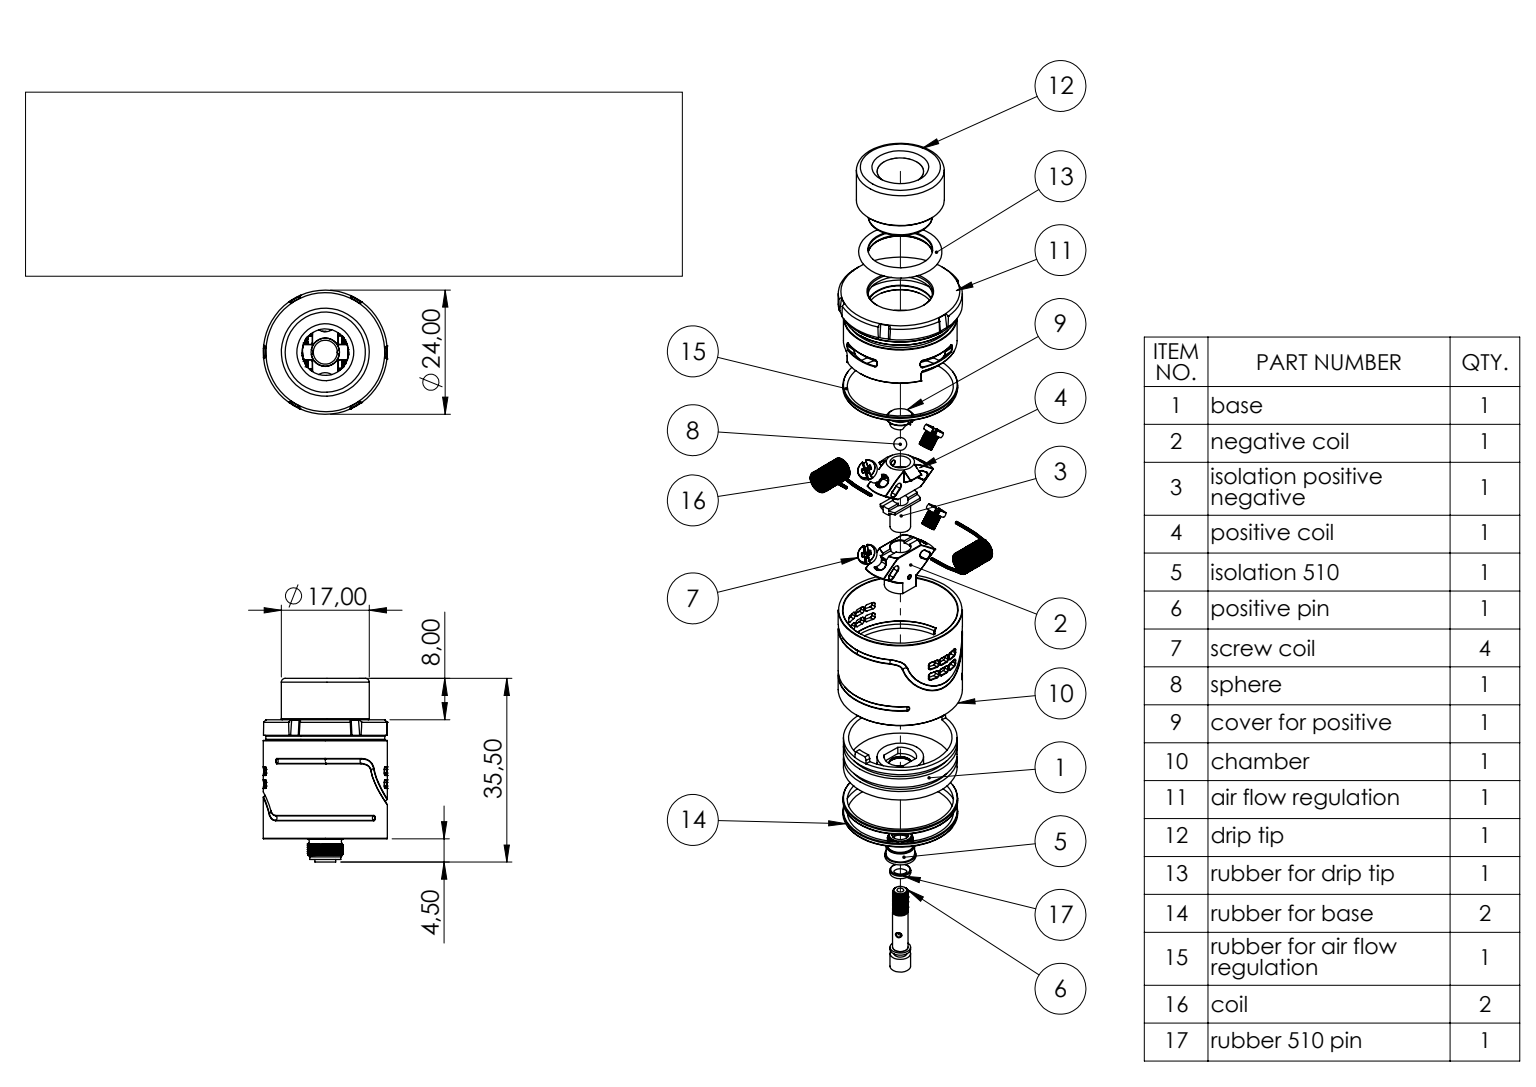
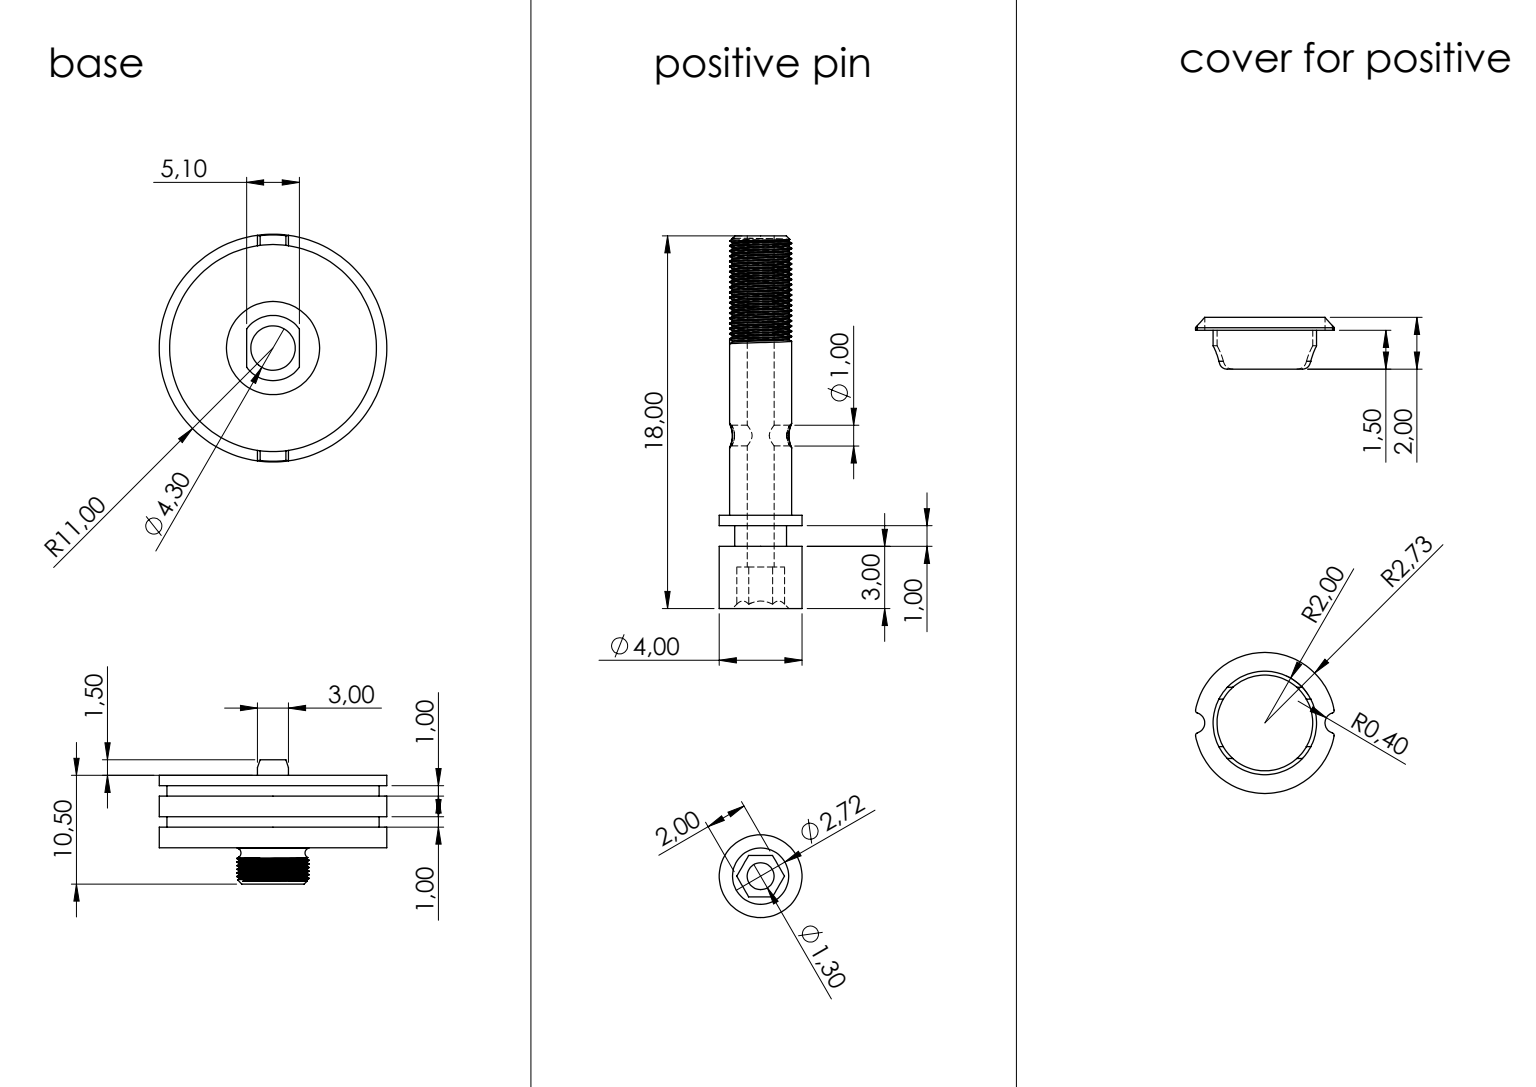
ISO-10303-21;
HEADER;
FILE_DESCRIPTION (('STEP AP214'),
    '1' );
FILE_NAME ('MAS-692',
    '2026-10-05T20:10:51',
    ( '' ),
    ( '' ),
    'SwSTEP 2.0',
    'SolidWorks 2020',
    '' );
FILE_SCHEMA (( 'AUTOMOTIVE_DESIGN' ));
ENDSEC;

DATA;
#1 = ORIENTED_EDGE ( 'NONE', *, *, #97562, .T. ) ;
#2 =( NAMED_UNIT ( * ) PLANE_ANGLE_UNIT ( ) SI_UNIT ( $, .RADIAN. ) );
#3 = ORIENTED_EDGE ( 'NONE', *, *, #96141, .T. ) ;
#4 = CARTESIAN_POINT ( 'NONE',  ( 5.963713532047742127, -0.4821895448718095945, 1.909345749545824367 ) ) ;
#5 = CARTESIAN_POINT ( 'NONE',  ( 1.311946287462633309, 1.302956792059128066, -1.440285294924074311 ) ) ;
#6 = CARTESIAN_POINT ( 'NONE',  ( 0.2454708137151571101, -1.954895187565863779, -0.4925657318226167591 ) ) ;
#8 = CARTESIAN_POINT ( 'NONE',  ( 4.311269015108330827, -1.545260327404588852, -1.036625270625696205 ) ) ;
#7 = CARTESIAN_POINT ( 'NONE',  ( -7.144220599758281054, 7.299621885998258897, 0.7998128361456341429 ) ) ;
#9 = CARTESIAN_POINT ( 'NONE',  ( 6.873057527484919937, 6.983264968346048818, 0.7998128361456352531 ) ) ;
#11 = ADVANCED_FACE ( 'NONE', ( #143939 ), #115364, .T. ) ;
#10 = CARTESIAN_POINT ( 'NONE',  ( 8.996750068618124985, 1.000000000000000888, 7.838941051145326355 ) ) ;
#12 = CYLINDRICAL_SURFACE ( 'NONE', #60912, 0.5000000000000000000 ) ;
#13 = CARTESIAN_POINT ( 'NONE',  ( -4.869349725602420520, 8.832658446511480577, 1.040834085586084257E-14 ) ) ;
#14 = CARTESIAN_POINT ( 'NONE',  ( -4.828112100242303306, 4.805421336470338645, -0.7216878364870338292 ) ) ;
#15 = CARTESIAN_POINT ( 'NONE',  ( 0.04676574305502099321, -1.756316032869180921, 1.310637071781264984 ) ) ;
#16 = CARTESIAN_POINT ( 'NONE',  ( 5.233084105194869551, 6.167981546557892436, -1.082531754730548412 ) ) ;
#17 = CARTESIAN_POINT ( 'NONE',  ( 11.89942855770814312, 9.799999999999998934, 0.6999999999999992895 ) ) ;
#18 = CARTESIAN_POINT ( 'NONE',  ( 1.833030277982334422, 2.531131934864056632, -2.500000000000000444 ) ) ;
#19 = CARTESIAN_POINT ( 'NONE',  ( 1.260069262837599791, 0.7379878962356714034, 1.670071910705408946 ) ) ;
#20 = CARTESIAN_POINT ( 'NONE',  ( -4.460796234096120472, 5.163016013655583158, 1.199719254218462483 ) ) ;
#21 = MECHANICAL_DESIGN_GEOMETRIC_PRESENTATION_REPRESENTATION (  '', ( #3437 ), #103815 ) ;
#22 = CARTESIAN_POINT ( 'NONE',  ( 3.515997504735939305, -1.600726479906929844, 0.6675610986628178756 ) ) ;
#23 = CARTESIAN_POINT ( 'NONE',  ( -0.4770184558378520734, 2.994739774722604331, -1.942553401570029203 ) ) ;
#24 = CARTESIAN_POINT ( 'NONE',  ( 6.609000000000019526, 4.695354556932705314, 2.562644781943986150 ) ) ;
#25 = CARTESIAN_POINT ( 'NONE',  ( 0.1331565106231329398, 0.7299000548664087429, -2.029785554894456556 ) ) ;
#26 = CARTESIAN_POINT ( 'NONE',  ( 6.445924739416000193, 0.6936395621829589686, -1.688995215704327313 ) ) ;
#27 = CARTESIAN_POINT ( 'NONE',  ( 4.504711789546460565, 0.5192035298374733099, 1.891763301562799260 ) ) ;
#28 = CARTESIAN_POINT ( 'NONE',  ( -8.474009703741204547, 9.845098394908269768, -1.199719254218446718 ) ) ;
#29 = CARTESIAN_POINT ( 'NONE',  ( 5.666418135507635512, 8.698239360479199433, 1.199719254218462483 ) ) ;
#30 = CARTESIAN_POINT ( 'NONE',  ( 4.389387035479824561, -0.001039498178659337352, -2.120667954306009406 ) ) ;
#31 = CARTESIAN_POINT ( 'NONE',  ( -9.158696461231359720, 10.64389961198009615, 1.199719254218462483 ) ) ;
#32 = ADVANCED_FACE ( 'NONE', ( #8553 ), #60499, .T. ) ;
#33 = CARTESIAN_POINT ( 'NONE',  ( 5.118366684358879759, 5.930181538962194132, 1.199719254218462483 ) ) ;
#34 = CARTESIAN_POINT ( 'NONE',  ( 3.274343992483694787, -1.016290647400164282, -1.803532422793553636 ) ) ;
#36 = CARTESIAN_POINT ( 'NONE',  ( 0.6823417656249882723, -0.5947916663252492686, 1.181850606188755259 ) ) ;
#35 = CARTESIAN_POINT ( 'NONE',  ( -0.4382560683119374190, -5.166862915010145052, -10.99126615174919408 ) ) ;
#37 = EDGE_LOOP ( 'NONE', ( #180346, #201044, #89611 ) ) ;
#38 = CARTESIAN_POINT ( 'NONE',  ( 2.549810578889585067, -1.582449011024213981, 1.667500336659861748 ) ) ;
#39 = CARTESIAN_POINT ( 'NONE',  ( 6.954969614130424027, 11.05795561655343384, 1.040834085586084257E-14 ) ) ;
#41 = CARTESIAN_POINT ( 'NONE',  ( 1.642778471875001811, -1.742708332855374298, 2.845375778867859751 ) ) ;
#40 = CARTESIAN_POINT ( 'NONE',  ( 4.719646871332936477, 8.520355426614829142, -0.7216878364870357165 ) ) ;
#42 = PRESENTATION_STYLE_ASSIGNMENT (( #185202 ) ) ;
#43 = CARTESIAN_POINT ( 'NONE',  ( 0.000000000000000000, 4.000000000000003553, 0.000000000000000000 ) ) ;
#44 = VERTEX_POINT ( 'NONE', #43221 ) ;
#45 = CARTESIAN_POINT ( 'NONE',  ( 10.37162432432990755, 11.20257592124748136, -0.7216878364870257245 ) ) ;
#46 = CARTESIAN_POINT ( 'NONE',  ( 3.568532368641282648, 0.6928216322696268969, 1.782650395559831180 ) ) ;
#47 = CARTESIAN_POINT ( 'NONE',  ( 4.928557879857294211, 1.651178231652555617, 0.4983569138605167814 ) ) ;
#48 = CARTESIAN_POINT ( 'NONE',  ( 3.608611488583326032, 1.916353073142588403, 0.6279913346786819561 ) ) ;
#49 =( BOUNDED_SURFACE ( )  B_SPLINE_SURFACE ( 3, 2, ( 
 ( #54801, #106802, #172831 ),
 ( #26553, #190122, #173916 ),
 ( #25490, #91596, #38551 ),
 ( #157648, #9245, #191177 ),
 ( #108952, #72088, #42845 ),
 ( #4939, #71015, #22263 ) ),
 .UNSPECIFIED., .F., .F., .T. ) 
 B_SPLINE_SURFACE_WITH_KNOTS ( ( 4, 2, 4 ),
 ( 3, 3 ),
 ( 0.0001465838689801548850, 0.0002810652682710442613, 0.0004155466675619336647 ),
 ( 0.000000000000000000, 1.000000000000000000 ),
 .UNSPECIFIED. ) 
 GEOMETRIC_REPRESENTATION_ITEM ( )  RATIONAL_B_SPLINE_SURFACE ( (
 ( 1.000000000000000000, 0.8789000212895399233, 1.000000000000000000),
 ( 1.000000000000000000, 0.9073166784884888481, 1.000000000000000000),
 ( 1.000000000000000000, 0.9160359019619195298, 1.000000000000000000),
 ( 1.000000000000000000, 0.8858134948703222378, 1.000000000000000000),
 ( 1.000000000000000000, 0.8506312074210943264, 1.000000000000000000),
 ( 1.000000000000000000, 0.8104931255412257673, 1.000000000000000000) ) ) 
 REPRESENTATION_ITEM ( '' )  SURFACE ( )  );
#50 = CARTESIAN_POINT ( 'NONE',  ( 5.063244923127927954, -1.278613472530117035, 1.910113253385301801 ) ) ;
#51 = CARTESIAN_POINT ( 'NONE',  ( -1.626862140677534470E-15, 1.125000000682806034, 1.224999999999975886 ) ) ;
#52 = CARTESIAN_POINT ( 'NONE',  ( 0.8388348947251201837, 2.174866457552121268, 0.3736606161612308630 ) ) ;
#53 = CARTESIAN_POINT ( 'NONE',  ( -3.797692425603673705, 6.484372692295976570, 1.082531754730549967 ) ) ;
#54 = CARTESIAN_POINT ( 'NONE',  ( 6.362547694819080668, -1.249765848162401438, 1.253281529121505589 ) ) ;
#56 = CARTESIAN_POINT ( 'NONE',  ( 1.851946410329910808, 2.285883199777267283, -0.1717553002464344836 ) ) ;
#55 = CARTESIAN_POINT ( 'NONE',  ( 6.710359684120930091, 6.793450817754725257, 0.7998128361456352531 ) ) ;
#57 = CARTESIAN_POINT ( 'NONE',  ( 6.228435704027582176, 0.1854037366294820077, 1.831779187086844729 ) ) ;
#58 = PRESENTATION_STYLE_ASSIGNMENT (( #85603 ) ) ;
#59 = CARTESIAN_POINT ( 'NONE',  ( -4.167152111353897403, 5.955039778036558040, 1.599625672291270506 ) ) ;
#60 = CARTESIAN_POINT ( 'NONE',  ( 1.360316468749959373, -0.4531249996586189654, -4.163336342344337027E-14 ) ) ;
#61 = FACE_OUTER_BOUND ( 'NONE', #36024, .T. ) ;
#62 = CARTESIAN_POINT ( 'NONE',  ( 0.3269468692386565678, -1.417551234153333395, 1.644607001386617418 ) ) ;
#63 = CARTESIAN_POINT ( 'NONE',  ( 1.973842561262352469, -0.8578407463649927456, 1.825077436249371354 ) ) ;
#64 = CARTESIAN_POINT ( 'NONE',  ( 1.499999999999989120, 0.05625000068281565957, 0.000000000000000000 ) ) ;
#65 = CARTESIAN_POINT ( 'NONE',  ( 5.479104952107777926, -0.04952074540257554031, -1.926025958231538882 ) ) ;
#66 = CARTESIAN_POINT ( 'NONE',  ( -8.012344526598182026E-15, 11.29687500034139980, -1.575800808251669460 ) ) ;
#67 = CARTESIAN_POINT ( 'NONE',  ( 1.898975720090949837, -2.179683001098455808, -0.4277757613022105110 ) ) ;
#68 = EDGE_LOOP ( 'NONE', ( #150530, #161755, #187821, #170704 ) ) ;
#69 = CARTESIAN_POINT ( 'NONE',  ( 6.731761806397376091, -7.792646766724933727, 6.779954559072931985 ) ) ;
#70 = LINE ( 'NONE', #134411, #196122 ) ;
#71 = CARTESIAN_POINT ( 'NONE',  ( 8.540746701604824409, 12.05162268759261224, -1.199719254218446718 ) ) ;
#72 = CARTESIAN_POINT ( 'NONE',  ( 6.658462837642789012, 9.821938173008357253, 1.082531754730549078 ) ) ;
#73 = CARTESIAN_POINT ( 'NONE',  ( 5.706559709869656771, 1.539012945689299139, 0.8127616963746787659 ) ) ;
#74 = CARTESIAN_POINT ( 'NONE',  ( 3.596105239937871456, 0.8843387906064968940, -1.751336483779348585 ) ) ;
#76 = CARTESIAN_POINT ( 'NONE',  ( -6.887178846062123938, 8.097758744236356776, -1.082531754730544860 ) ) ;
#75 = CARTESIAN_POINT ( 'NONE',  ( 4.253507506385319381, 5.985511395581417204, 1.599625672291267398 ) ) ;
#77 = CARTESIAN_POINT ( 'NONE',  ( -5.762141863986474100, 6.090740110424618159, 0.6348889758391648153 ) ) ;
#78 = CARTESIAN_POINT ( 'NONE',  ( 4.763087504681410955, -2.017952330160921015, -1.023110994099560411 ) ) ;
#79 = CARTESIAN_POINT ( 'NONE',  ( 1.135301032730736237, -0.04873925880971052838, -2.062252310772247910 ) ) ;
#80 = CARTESIAN_POINT ( 'NONE',  ( -8.830438121202295321, 9.196599317691152464, -0.7998128361456291469 ) ) ;
#81 = CARTESIAN_POINT ( 'NONE',  ( -4.460269348771590536, 5.266364330730674226, 1.082531754730558626 ) ) ;
#82 = CARTESIAN_POINT ( 'NONE',  ( 2.782378429719241986, -1.163933448739282062, 1.940043740367594305 ) ) ;
#83 = ORIENTED_EDGE ( 'NONE', *, *, #112082, .F. ) ;
#84 = CARTESIAN_POINT ( 'NONE',  ( -0.7500000000000006661, -0.6104166659838470288, -1.299038105676652011 ) ) ;
#85 = CARTESIAN_POINT ( 'NONE',  ( 2.301827437220682171, -1.870247568056710774, 0.04138213060620592881 ) ) ;
#86 = CARTESIAN_POINT ( 'NONE',  ( 1.441630353877725979, -1.487241779905050576, -0.8915045353455192112 ) ) ;
#87 = CARTESIAN_POINT ( 'NONE',  ( 5.495707582769355781, -2.191739722525353429, -0.0009102486706394352645 ) ) ;
#88 = CARTESIAN_POINT ( 'NONE',  ( 0.2533207856364183552, -1.770817270756098960, 1.316655756711228253 ) ) ;
#89 = CARTESIAN_POINT ( 'NONE',  ( 1.534131747024346737, 1.016495879925772616, -1.792692027746685346 ) ) ;
#90 = CARTESIAN_POINT ( 'NONE',  ( 4.013568362537369261, -0.9994162096361800529, -1.664904219174968114 ) ) ;
#91 = CARTESIAN_POINT ( 'NONE',  ( -3.592547517496929466, 7.135129837147637488, -0.7216878364870257245 ) ) ;
#92 = CARTESIAN_POINT ( 'NONE',  ( 6.928203230275524760, 15.51845925587262798, -9.797958971132702644 ) ) ;
#93 = CARTESIAN_POINT ( 'NONE',  ( 1.718750000000001554, -0.7852924748298989455, 1.895863743164124093 ) ) ;
#94 = CARTESIAN_POINT ( 'NONE',  ( 4.014365637759117256, 7.575528411784208771, 0.2883143100938356240 ) ) ;
#95 = CARTESIAN_POINT ( 'NONE',  ( 0.2800716429562755683, -1.702078881456047688, 0.3292984779095942116 ) ) ;
#96 = CARTESIAN_POINT ( 'NONE',  ( 11.88237951145550220, 12.34319347378715115, 0.9087114598430685586 ) ) ;
#97 = CARTESIAN_POINT ( 'NONE',  ( 0.6801582343749935644, 0.9739583336747514863, 1.178068619123805227 ) ) ;
#98 = CARTESIAN_POINT ( 'NONE',  ( 4.483046177357690176, -2.016033783801042034, -0.04667830911464498911 ) ) ;
#99 = CARTESIAN_POINT ( 'NONE',  ( -8.859363311525973117, 12.42334206583395328, -1.199719254218446718 ) ) ;
#100 = CARTESIAN_POINT ( 'NONE',  ( 8.308449207076147758, 8.587612251210650527, -0.7998128361456281477 ) ) ;
#101 = CARTESIAN_POINT ( 'NONE',  ( 4.553559489343365740, 6.405848385690952718, -1.599625672291269396 ) ) ;
#103 = CARTESIAN_POINT ( 'NONE',  ( 1.255262969126037044E-15, 0.4999999999999998890, -10.24999999999999822 ) ) ;
#102 = CARTESIAN_POINT ( 'NONE',  ( 2.068725586703868746, -1.668841220716179130, -0.7407507213199536755 ) ) ;
#104 = CARTESIAN_POINT ( 'NONE',  ( -0.7500000000000215383, 5.191666666666685082, 1.299038105676671107 ) ) ;
#105 = CARTESIAN_POINT ( 'NONE',  ( -9.333041836226904309, 15.44694763438996077, -7.472413793095822321 ) ) ;
#106 = VERTEX_POINT ( 'NONE', #173218 ) ;
#107 = CARTESIAN_POINT ( 'NONE',  ( -5.600926855776882540, 8.588146194164741232, -1.082531754730549967 ) ) ;
#108 = DIRECTION ( 'NONE',  ( 0.000000000000000000, 0.000000000000000000, -1.000000000000000000 ) ) ;
#109 = CARTESIAN_POINT ( 'NONE',  ( -8.565000355531095622, 11.01558638625153286, -1.599625672291263179 ) ) ;
#110 = CARTESIAN_POINT ( 'NONE',  ( 0.01783989211246589379, -0.5346760324982450241, 1.947684760809722304 ) ) ;
#111 = CARTESIAN_POINT ( 'NONE',  ( 6.551452540055466400, -1.985718062329771438, 0.9957849561875466993 ) ) ;
#112 = ORIENTED_EDGE ( 'NONE', *, *, #89227, .T. ) ;
#113 = CARTESIAN_POINT ( 'NONE',  ( -4.911796789900812144, 8.952456364851418158, 0.7998128361456291469 ) ) ;
#114 = CARTESIAN_POINT ( 'NONE',  ( 5.843727902690005749, 6.776436293681846301, -1.199719254218445830 ) ) ;
#115 = MECHANICAL_DESIGN_GEOMETRIC_PRESENTATION_REPRESENTATION (  '', ( #107520 ), #142122 ) ;
#116 = CARTESIAN_POINT ( 'NONE',  ( 6.666874348205719336, -1.883165374045802087, -0.8376701409097894180 ) ) ;
#117 = CARTESIAN_POINT ( 'NONE',  ( 4.869767617671093340, -0.2496050341583149201, -2.000857388266870984 ) ) ;
#118 = ORIENTED_EDGE ( 'NONE', *, *, #154536, .F. ) ;
#119 = ORIENTED_EDGE ( 'NONE', *, *, #79643, .F. ) ;
#120 = CARTESIAN_POINT ( 'NONE',  ( 10.50000000000000355, 11.00832445802304882, -3.600000000000000533 ) ) ;
#121 = CARTESIAN_POINT ( 'NONE',  ( -2.324088772396477673E-16, -1.093749999044084653, -3.475000000000000089 ) ) ;
#124 = VERTEX_POINT ( 'NONE', #206751 ) ;
#123 = CARTESIAN_POINT ( 'NONE',  ( -1.772826578343124959, 3.950000000000009059, -0.4500000000000423661 ) ) ;
#122 = CARTESIAN_POINT ( 'NONE',  ( -5.956828388357799042, 8.042995434541133193, 1.599625672291263179 ) ) ;
#125 = CARTESIAN_POINT ( 'NONE',  ( 5.720439131930858956, 7.397432110343761025, 1.315134405782365956 ) ) ;
#126 = CARTESIAN_POINT ( 'NONE',  ( 4.639999869408336863, 0.002810260262744306969, -2.016288307263448321 ) ) ;
#127 = CARTESIAN_POINT ( 'NONE',  ( 4.294743845541324490, 1.480121740587354573, 1.094796260939827404 ) ) ;
#128 = CARTESIAN_POINT ( 'NONE',  ( 2.969872605471105320, 6.605953636083950364, 7.500000000000000000 ) ) ;
#129 = CARTESIAN_POINT ( 'NONE',  ( 3.317284684000018746, 2.086097511483188338, 0.9870085806921449212 ) ) ;
#130 = CARTESIAN_POINT ( 'NONE',  ( 5.833751235630055376, 10.02806988486892514, 0.7998128361456331437 ) ) ;
#131 = CARTESIAN_POINT ( 'NONE',  ( 4.727887898869392203, -1.325758432718616042, -1.707240035374466114 ) ) ;
#132 = CARTESIAN_POINT ( 'NONE',  ( 6.286176778230493589, 10.48562334124426698, 0.7998128361456462443 ) ) ;
#133 = CARTESIAN_POINT ( 'NONE',  ( 1.030689935155226555, -1.755017395645932066, 0.8318847510124205424 ) ) ;
#134 = CARTESIAN_POINT ( 'NONE',  ( -5.434120640978981065, 5.234228924097238611, -0.7998128361456221525 ) ) ;
#135 = ORIENTED_EDGE ( 'NONE', *, *, #160637, .F. ) ;
#137 = ADVANCED_FACE ( 'NONE', ( #75695 ), #126301, .T. ) ;
#136 = AXIS2_PLACEMENT_3D ( 'NONE', #150027, #130648, #82874 ) ;
#138 = CARTESIAN_POINT ( 'NONE',  ( 6.446420058208158110, -6.527411821100059797, 7.058808231563617142 ) ) ;
#139 = CARTESIAN_POINT ( 'NONE',  ( -4.817943484809863008, 6.714296380401858499, 1.599625672291263179 ) ) ;
#140 = CARTESIAN_POINT ( 'NONE',  ( 3.783945140921864070, -0.9226758061156097313, 1.627204332209288395 ) ) ;
#143 = CARTESIAN_POINT ( 'NONE',  ( -5.586841817283045408, 8.675676665875643678, 1.199719254218454489 ) ) ;
#142 = CARTESIAN_POINT ( 'NONE',  ( -1.500000000000015099, -0.5479166659838513587, 0.8660254037844403729 ) ) ;
#141 = CARTESIAN_POINT ( 'NONE',  ( 1.828231037913151447, -0.9045423626323212396, -1.684975973026317408 ) ) ;
#144 = CARTESIAN_POINT ( 'NONE',  ( 3.018423772948013006, -1.088090592406821155, -1.919924466345590108 ) ) ;
#145 = CARTESIAN_POINT ( 'NONE',  ( 6.883263157960402445, 0.001763689368145578400, 1.846037217754380011 ) ) ;
#146 = CARTESIAN_POINT ( 'NONE',  ( 4.403700966340357681, 4.032072637018845107, -0.7998128361456211532 ) ) ;
#147 = CARTESIAN_POINT ( 'NONE',  ( 7.038091138825468107, 8.344099429118761790, -1.082531754730548412 ) ) ;
#148 = CARTESIAN_POINT ( 'NONE',  ( -3.216308754939891212, 4.775446185561722956, -1.599625672291262513 ) ) ;
#149 = CARTESIAN_POINT ( 'NONE',  ( -7.390603132780803719, 7.794994207765291172, -0.7216878364870338292 ) ) ;
#150 = CARTESIAN_POINT ( 'NONE',  ( 0.9484320465981105341, 0.5679970104440315026, 1.887783002132171539 ) ) ;
#151 = CARTESIAN_POINT ( 'NONE',  ( 0.3414292828918061296, 0.3991051782518301727, 2.272663865251875581 ) ) ;
#152 = CARTESIAN_POINT ( 'NONE',  ( 1.838261372102001800, -1.052240823716396267, 1.655630454418555830 ) ) ;
#153 = CARTESIAN_POINT ( 'NONE',  ( 5.032111728107424575, 1.183179145130999643, 1.689302184701612086 ) ) ;
#154 = CARTESIAN_POINT ( 'NONE',  ( 5.178851490740207453, 5.144340948726102702, 0.7216878364870317197 ) ) ;
#155 = CARTESIAN_POINT ( 'NONE',  ( 4.667750024854814050, 8.667735138964429709, -0.7998128361456381397 ) ) ;
#156 = VERTEX_POINT ( 'NONE', #175348 ) ;
#157 = CARTESIAN_POINT ( 'NONE',  ( -1.364683531250010295, 5.301041667008085767, -0.7879004041258300672 ) ) ;
#158 = CARTESIAN_POINT ( 'NONE',  ( -10.12724623727299900, 3.700526055228949840, -6.355430437403613020 ) ) ;
#159 = CARTESIAN_POINT ( 'NONE',  ( 4.541618270453549044, 5.361271406026338227, -1.082531754730548412 ) ) ;
#160 = CARTESIAN_POINT ( 'NONE',  ( 1.042111193480334430, 1.456518763772189695, 1.610191069602670000 ) ) ;
#162 = CARTESIAN_POINT ( 'NONE',  ( 6.251489360189885325, 1.835807759842246423, -0.1425652098738516838 ) ) ;
#161 = CARTESIAN_POINT ( 'NONE',  ( 1.224999999999948797, 0.4583333340161501734, -0.7072540797573277915 ) ) ;
#163 = CARTESIAN_POINT ( 'NONE',  ( 11.84668730067608244, 12.69999999999998153, 1.399999999999998357 ) ) ;
#164 = CARTESIAN_POINT ( 'NONE',  ( -11.92051736251532112, 12.44819756207321149, -1.381800029228967386 ) ) ;
#165 = CARTESIAN_POINT ( 'NONE',  ( 1.915107840602244593, -0.2339084544023955492, 1.855816807740391150 ) ) ;
#166 = CARTESIAN_POINT ( 'NONE',  ( 5.343121995983710626, -1.856993961526328007, 1.106124453333141577 ) ) ;
#167 = CARTESIAN_POINT ( 'NONE',  ( -6.137267537028628261, 5.996416355291856348, 0.05987573180751305790 ) ) ;
#168 = CARTESIAN_POINT ( 'NONE',  ( -0.02244404828160087226, 0.2256878572204877031, -2.222431841814066278 ) ) ;
#169 = CARTESIAN_POINT ( 'NONE',  ( 6.425920342564602983, 6.885296541689900351, -0.7293792964763821107 ) ) ;
#170 = CARTESIAN_POINT ( 'NONE',  ( 0.6823417656249899377, 5.738541667008087543, -1.181850606188754593 ) ) ;
#171 = CARTESIAN_POINT ( 'NONE',  ( 1.664566505720616929, 0.6010121217654046388, 1.815428919054395518 ) ) ;
#172 = CARTESIAN_POINT ( 'NONE',  ( 2.623613022005319984, -1.017049183177589855, -1.448221827668960238 ) ) ;
#173 = CARTESIAN_POINT ( 'NONE',  ( 0.2406774923011632261, 1.829974501424940891, 0.5550298453492612527 ) ) ;
#175 = CARTESIAN_POINT ( 'NONE',  ( 4.991753579581297728, -1.905966813954384387, 0.1920618708746626713 ) ) ;
#174 = CARTESIAN_POINT ( 'NONE',  ( 1.467871227757891193E-11, -3.138498625356828775, -3.379301813585260383 ) ) ;
#176 = CARTESIAN_POINT ( 'NONE',  ( 6.057084849134293236, 1.611049215779712940, -1.132701646639628246 ) ) ;
#177 = CARTESIAN_POINT ( 'NONE',  ( 1.499999999999990896, 4.275000000000021672, 1.214306433183764966E-14 ) ) ;
#178 = CARTESIAN_POINT ( 'NONE',  ( 0.7035762090183244055, 1.867434778015097940, -1.004864118554361863 ) ) ;
#179 = DIRECTION ( 'NONE',  ( 0.000000000000000000, 0.000000000000000000, -1.000000000000000000 ) ) ;
#180 = CARTESIAN_POINT ( 'NONE',  ( 3.959713429720784106, 1.856571849420919795, -0.2284545790810637578 ) ) ;
#182 = ORIENTED_EDGE ( 'NONE', *, *, #184994, .T. ) ;
#181 = CARTESIAN_POINT ( 'NONE',  ( 0.5569169099325711469, -1.540613122784354916, -0.9793164655157863274 ) ) ;
#184 = CARTESIAN_POINT ( 'NONE',  ( 4.649081266440608928, 8.305916344280937835, -0.4560373724170601606 ) ) ;
#183 = CARTESIAN_POINT ( 'NONE',  ( 5.074942902252104204, -2.077123540546990110, -0.7459609299403434646 ) ) ;
#185 = CARTESIAN_POINT ( 'NONE',  ( -1.201851678989727383E-14, 5.009375000341421469, -1.575800808251660134 ) ) ;
#186 = CARTESIAN_POINT ( 'NONE',  ( 2.189955769151647580, -1.345473201219016701, -1.563545076720110227 ) ) ;
#187 = CARTESIAN_POINT ( 'NONE',  ( 4.964256800898067645, 8.943383367689749619, 0.7998128361456462443 ) ) ;
#188 = CARTESIAN_POINT ( 'NONE',  ( -8.154339323615371171, 11.60081407993821045, 1.199719254218453823 ) ) ;
#189 = DIRECTION ( 'NONE',  ( 0.000000000000000000, 1.000000000000000000, 0.000000000000000000 ) ) ;
#190 = FACE_OUTER_BOUND ( 'NONE', #152846, .T. ) ;
#191 = CARTESIAN_POINT ( 'NONE',  ( 6.521744167503259249, -0.4122283346772101509, 1.874327247564554266 ) ) ;
#192 = ORIENTED_EDGE ( 'NONE', *, *, #191821, .F. ) ;
#193 = CARTESIAN_POINT ( 'NONE',  ( 3.912603064140641074, 0.7423916865902054907, 1.932869565047180549 ) ) ;
#194 = CARTESIAN_POINT ( 'NONE',  ( -1.402160292154681736E-14, -1.115624999658584082, 1.575800808251672791 ) ) ;
#195 = CARTESIAN_POINT ( 'NONE',  ( 2.003414267471514965, 1.795956895356983551, 1.202623776965026536 ) ) ;
#196 = CARTESIAN_POINT ( 'NONE',  ( -5.495582220874787538, 7.482514367559947033, -1.250084184017367539 ) ) ;
#197 = CARTESIAN_POINT ( 'NONE',  ( 1.647134723225437636, 0.2000593722277475561, 2.009751748981201569 ) ) ;
#198 = CARTESIAN_POINT ( 'NONE',  ( 3.823036128929238942, 7.404033217152015567, 1.040834085586084257E-14 ) ) ;
#199 = ORIENTED_EDGE ( 'NONE', *, *, #95230, .T. ) ;
#201 = CARTESIAN_POINT ( 'NONE',  ( 7.443063144222396232, 11.62739806832741785, 1.040834085586084257E-14 ) ) ;
#200 = CARTESIAN_POINT ( 'NONE',  ( 3.475000000000000533, -2.945833333333332416, -2.006292185433951047 ) ) ;
#202 = CARTESIAN_POINT ( 'NONE',  ( 0.3663205537283338309, -5.223179855899201307, 10.97093617010627220 ) ) ;
#203 = CARTESIAN_POINT ( 'NONE',  ( -0.2234322562767385167, -0.4468160588090731022, -1.973564571300358228 ) ) ;
#204 = CARTESIAN_POINT ( 'NONE',  ( 6.539320575229278454, 0.5749733277502915296, 2.156147827957733742 ) ) ;
#205 = CARTESIAN_POINT ( 'NONE',  ( 4.704715985517350596, 1.906866092115505840, 1.080010033982371498 ) ) ;
#206 = CARTESIAN_POINT ( 'NONE',  ( -1.500000000000011324, 3.702083334016152971, 0.8660254037844403729 ) ) ;
#207 = CARTESIAN_POINT ( 'NONE',  ( 3.287273477832891366, 0.04233216220104508987, -1.912079899511004433 ) ) ;
#208 = CARTESIAN_POINT ( 'NONE',  ( -3.554208825076827782, 7.298327395898266623, 0.7998128361456341429 ) ) ;
#209 = CARTESIAN_POINT ( 'NONE',  ( 5.300874872818843286, 5.286701561151180506, 0.7216878364870317197 ) ) ;
#211 = CARTESIAN_POINT ( 'NONE',  ( 1.880482680076976720, -0.5405129038237622696, -1.942536604102131026 ) ) ;
#210 = DIRECTION ( 'NONE',  ( 0.000000000000000000, 0.000000000000000000, 1.000000000000000000 ) ) ;
#212 = CARTESIAN_POINT ( 'NONE',  ( -0.6823417656250003738, 12.71354166700806942, 1.181850606188754593 ) ) ;
#214 = CARTESIAN_POINT ( 'NONE',  ( -3.644109427023046521, 7.473487774827342278, 0.000000000000000000 ) ) ;
#213 = CARTESIAN_POINT ( 'NONE',  ( 0.5566822826340491748, -1.655162342056889502, 1.586242259447123493 ) ) ;
#215 = CARTESIAN_POINT ( 'NONE',  ( 4.612129873793564094, -0.7390372460917455921, -1.558541145072767975 ) ) ;
#216 = CARTESIAN_POINT ( 'NONE',  ( 11.84668730067608244, 12.69999999999999929, -1.320000000000001616 ) ) ;
#217 = CARTESIAN_POINT ( 'NONE',  ( 3.011882680530176604, 6.665613560593854459, 0.7998128361456341429 ) ) ;
#218 = LINE ( 'NONE', #116204, #61046 ) ;
#219 = CARTESIAN_POINT ( 'NONE',  ( 0.8714495147512549833, -0.2914478312704605889, 1.939986204769503786 ) ) ;
#220 = CARTESIAN_POINT ( 'NONE',  ( 0.3033014811697418711, -0.5033704626738467747, 1.801585485020948729 ) ) ;
#221 = CARTESIAN_POINT ( 'NONE',  ( 2.706824224222692088, 6.309712028235118453, 0.7998128361456362523 ) ) ;
#222 = CARTESIAN_POINT ( 'NONE',  ( 0.1751657365761703222, 4.087554309226840488, -2.598743260590470783 ) ) ;
#223 = EDGE_LOOP ( 'NONE', ( #165565, #34083, #144999, #128787 ) ) ;
#224 = SURFACE_STYLE_USAGE ( .BOTH. , #31713 ) ;
#225 = ORIENTED_EDGE ( 'NONE', *, *, #185632, .T. ) ;
#226 = CARTESIAN_POINT ( 'NONE',  ( 5.039644362999008642, -1.718302384056184851, 0.5736564087924463928 ) ) ;
#227 = ORIENTED_EDGE ( 'NONE', *, *, #162616, .F. ) ;
#228 = CARTESIAN_POINT ( 'NONE',  ( 4.505052181490820651, 8.477920988373101707, -0.7998128361456381397 ) ) ;
#229 = CARTESIAN_POINT ( 'NONE',  ( -7.015401035077363900, 6.062865449010541141, 2.437084766375292144 ) ) ;
#230 = CARTESIAN_POINT ( 'NONE',  ( 5.514259914679787045, -1.811656974672648746, 0.006318095929410197376 ) ) ;
#231 = CARTESIAN_POINT ( 'NONE',  ( 5.790741006368192778, 8.809596036521288198, -1.082531754730548412 ) ) ;
#232 = CARTESIAN_POINT ( 'NONE',  ( 2.279325334093329936, 5.605928279738464859, -0.5932882675315593879 ) ) ;
#233 = CARTESIAN_POINT ( 'NONE',  ( 4.809732914444119878, 6.735689552132856583, -1.248430568442916888 ) ) ;
#234 = ORIENTED_EDGE ( 'NONE', *, *, #52222, .T. ) ;
#236 = CARTESIAN_POINT ( 'NONE',  ( 9.673906298550626559, 11.24497775551929557, 1.199719254218452047 ) ) ;
#235 = CARTESIAN_POINT ( 'NONE',  ( 6.215283151739675382, -1.596727646711604942, -0.9557930639402379969 ) ) ;
#237 = CARTESIAN_POINT ( 'NONE',  ( 3.480013654308728555, -1.913576260228011749, -0.09060460826773930609 ) ) ;
#238 = CARTESIAN_POINT ( 'NONE',  ( -6.451695228975252050, -8.176248043968191936, -7.005920419303019564 ) ) ;
#239 = STYLED_ITEM ( 'NONE', ( #58 ), #85152 ) ;
#240 = EDGE_CURVE ( 'NONE', #112800, #149263, #151353, .T. ) ;
#241 = CARTESIAN_POINT ( 'NONE',  ( -2.788906526875773208E-15, 11.93750000000000000, -1.499999999999998446 ) ) ;
#242 =( NAMED_UNIT ( * ) PLANE_ANGLE_UNIT ( ) SI_UNIT ( $, .RADIAN. ) );
#243 = CARTESIAN_POINT ( 'NONE',  ( 5.775410249741494972, 8.721433810464993996, -1.082531754730537088 ) ) ;
#245 = CARTESIAN_POINT ( 'NONE',  ( 6.016841150788749815, 0.2099786098018930069, 2.106937748889408546 ) ) ;
#244 = CARTESIAN_POINT ( 'NONE',  ( -10.49364770729726359, 11.34493653470939023, 0.7216878364870438212 ) ) ;
#246 = CARTESIAN_POINT ( 'NONE',  ( 0.3917762336288696523, 1.602822130585265015, 1.450656209987542855 ) ) ;
#247 = CARTESIAN_POINT ( 'NONE',  ( -6.771371375382467583, 6.864631124226471037, -0.7998128361456362523 ) ) ;
#248 = CARTESIAN_POINT ( 'NONE',  ( 4.146814880933355596, 5.931313009212638931, 1.599625672291261402 ) ) ;
#249 = CARTESIAN_POINT ( 'NONE',  ( 1.307329191252764922, -0.4475898743878243824, 1.769731943805815222 ) ) ;
#250 = CARTESIAN_POINT ( 'NONE',  ( -4.009460741339347045, 5.700790169694431420, -1.599625672291256295 ) ) ;
#251 = CARTESIAN_POINT ( 'NONE',  ( 3.680510133705969800, -1.759192178946006990, -0.4875382671739314500 ) ) ;
#252 = CARTESIAN_POINT ( 'NONE',  ( 9.376191831160928913, 12.67849274587929820, -8.895508691099047738 ) ) ;
#253 = CARTESIAN_POINT ( 'NONE',  ( 2.742330423940505302, 1.058908597569432120, -1.592262909973440888 ) ) ;
#254 = ORIENTED_EDGE ( 'NONE', *, *, #20526, .T. ) ;
#255 = CARTESIAN_POINT ( 'NONE',  ( 2.418351439525995961, 0.8393807748916733980, 1.781860320225916228 ) ) ;
#256 = CARTESIAN_POINT ( 'NONE',  ( 5.108904621496645149, -0.2812511558281989288, 1.921465535368711786 ) ) ;
#257 = CARTESIAN_POINT ( 'NONE',  ( -6.563028877466991595, 9.814561569423593923, 1.199719254218452935 ) ) ;
#259 = CARTESIAN_POINT ( 'NONE',  ( 4.974906307097914926, -1.534222593358970821, 1.464151343314526121 ) ) ;
#258 = CARTESIAN_POINT ( 'NONE',  ( 6.099189001301251523, 8.209082816308541197, 1.599625672291268286 ) ) ;
#261 = ADVANCED_FACE ( 'NONE', ( #76746 ), #62774, .T. ) ;
#260 = CARTESIAN_POINT ( 'NONE',  ( -6.387350227218078658, 6.552219065260997510, -2.500000000001207923 ) ) ;
#262 = CARTESIAN_POINT ( 'NONE',  ( 2.508343198132975349, -1.907285675847451234, -0.1387974571645037292 ) ) ;
#263 = CARTESIAN_POINT ( 'NONE',  ( 6.114015800945279189, 6.016301931502064271, 0.06476946160361742033 ) ) ;
#264 = CARTESIAN_POINT ( 'NONE',  ( 0.000000000000000000, 6.999999999999992006, 4.500000000000000000 ) ) ;
#265 = CARTESIAN_POINT ( 'NONE',  ( 5.391302360089590628, 6.318882837306503575, -1.199719254218452047 ) ) ;
#266 = AXIS2_PLACEMENT_3D ( 'NONE', #151063, #68698, #100160 ) ;
#267 = LINE ( 'NONE', #66337, #6225 ) ;
#268 = CARTESIAN_POINT ( 'NONE',  ( 4.600122369450095228, -1.825375079466069694, -0.04201004182294298950 ) ) ;
#269 = CARTESIAN_POINT ( 'NONE',  ( 0.9243811426856913815, 1.018911950503737174, 1.802186752163869699 ) ) ;
#270 = CARTESIAN_POINT ( 'NONE',  ( -7.537970219518066450, 11.73812298950569044, -0.7216878364870267237 ) ) ;
#271 = CARTESIAN_POINT ( 'NONE',  ( -6.579637281422358264, 6.781222396613637571, 0.3437121870633503828 ) ) ;
#272 = CARTESIAN_POINT ( 'NONE',  ( -0.3000000000000346279, 3.999999999999980904, -1.007084189318430356 ) ) ;
#273 = CARTESIAN_POINT ( 'NONE',  ( 5.172658500931742509, -1.761684834526537680, -0.6294727512598657926 ) ) ;
#274 = CARTESIAN_POINT ( 'NONE',  ( 6.805303039055573322, 10.02693841461847057, 1.199719254218460707 ) ) ;
#275 = CARTESIAN_POINT ( 'NONE',  ( -4.680589345215810049, 6.483773540883647435, -1.599625672291256517 ) ) ;
#276 = AXIS2_PLACEMENT_3D ( 'NONE', #147982, #164223, #79761 ) ;
#277 = CARTESIAN_POINT ( 'NONE',  ( 4.054051625686104998, 4.688480637177271149, -1.199719254218446718 ) ) ;
#278 = CARTESIAN_POINT ( 'NONE',  ( 0.6823417656249934904, 10.75520833367472839, 1.181850606188764807 ) ) ;
#279 = CARTESIAN_POINT ( 'NONE',  ( -5.063080299699540987, 7.994345218703034384, 1.199719254218464037 ) ) ;
#280 = CARTESIAN_POINT ( 'NONE',  ( 4.196412238629597447, 4.854568018944682706, -1.199719254218452047 ) ) ;
#281 = CARTESIAN_POINT ( 'NONE',  ( -7.391130018105325661, 8.652015104991543026, -1.199719254218452047 ) ) ;
#282 = CARTESIAN_POINT ( 'NONE',  ( -6.227272627378437342, 6.159572908229946187, -0.7998128361456291469 ) ) ;
#283 = CARTESIAN_POINT ( 'NONE',  ( 6.649308703871936288, 1.893188687436907047, -1.062577851937399620 ) ) ;
#284 = ADVANCED_FACE ( 'NONE', ( #194766 ), #46403, .F. ) ;
#285 = CARTESIAN_POINT ( 'NONE',  ( 2.882529129721671080, -0.6171794022716176054, -2.025259201532733755 ) ) ;
#286 = CARTESIAN_POINT ( 'NONE',  ( 8.809047120577066181, 11.30030761213851953, 1.599625672291281386 ) ) ;
#287 = CARTESIAN_POINT ( 'NONE',  ( 0.5718752940412629160, 6.816535892783741168, 3.722047857044940233 ) ) ;
#288 = CARTESIAN_POINT ( 'NONE',  ( 5.981320602565292965, -0.05662044862421274777, 2.069665677200482445 ) ) ;
#289 = CARTESIAN_POINT ( 'NONE',  ( 4.000033042702237474, 7.827758669039140749, -0.08873751906842038129 ) ) ;
#290 = CARTESIAN_POINT ( 'NONE',  ( 6.344852701515477200, 6.504675694630598137, -0.7216878364870257245 ) ) ;
#292 = CARTESIAN_POINT ( 'NONE',  ( 0.7500000000000006661, 9.614583334016129967, 1.299038105676657340 ) ) ;
#291 = CARTESIAN_POINT ( 'NONE',  ( 1.001543065824772753E-15, -3.762499999999999289, 4.012584370867899430 ) ) ;
#293 = CARTESIAN_POINT ( 'NONE',  ( 2.959215247630428536, 0.3357152255929369278, -2.267430770885081603 ) ) ;
#295 = CARTESIAN_POINT ( 'NONE',  ( 1.123270288254022198, 3.158552654332631882, -0.7749999999939810591 ) ) ;
#294 = CARTESIAN_POINT ( 'NONE',  ( 7.654042494670958593E-16, 3.079999999999999183, -6.250000000000000000 ) ) ;
#296 = CARTESIAN_POINT ( 'NONE',  ( 2.548957913124219044, 0.2380835140640499836, 1.897471792728817386 ) ) ;
#297 = CARTESIAN_POINT ( 'NONE',  ( 7.036318535368067728, 10.19249347702934294, -1.082531754730537976 ) ) ;
#298 = CARTESIAN_POINT ( 'NONE',  ( 0.7033859027741823366, 1.773467923640878796, -0.9528479892364212223 ) ) ;
#299 = CARTESIAN_POINT ( 'NONE',  ( 0.8835585337332927391, -1.864609544942645414, 0.6100022000963196689 ) ) ;
#300 = CARTESIAN_POINT ( 'NONE',  ( -8.597841969360544567, 13.18256606422934674, 0.7998128361456341429 ) ) ;
#301 = CARTESIAN_POINT ( 'NONE',  ( -8.389798128758148010, 8.682519326506312751, 0.7998128361456462443 ) ) ;
#302 = CARTESIAN_POINT ( 'NONE',  ( -3.285556943750000514, -0.5760416661887087786, -1.896917185911906500 ) ) ;
#304 = CARTESIAN_POINT ( 'NONE',  ( 2.500565701108145689, 1.422975883020457077, -1.052153950563482265 ) ) ;
#303 = CARTESIAN_POINT ( 'NONE',  ( 3.451197694293614671, 0.5077425806990677470, -2.027912974856157291 ) ) ;
#305 = CARTESIAN_POINT ( 'NONE',  ( 6.827182134110199030, 7.629137130509070275, 2.410944104600701188 ) ) ;
#307 = CARTESIAN_POINT ( 'NONE',  ( 5.789115795541526666, 1.732349586671273922, 1.501262892615047750 ) ) ;
#306 = DIRECTION ( 'NONE',  ( -5.578564026256490882E-16, -1.000000000000000000, -9.066213480720158442E-32 ) ) ;
#308 = CARTESIAN_POINT ( 'NONE',  ( 3.943067085940495264, 0.5840054040482050013, -1.639550319303827219 ) ) ;
#309 = CARTESIAN_POINT ( 'NONE',  ( 4.227444969362701421, 3.826440640544909400, 1.214306433183764966E-14 ) ) ;
#310 = CARTESIAN_POINT ( 'NONE',  ( 6.249382461256315580, 6.255644057745969988, -0.7998128361456481317 ) ) ;
#311 = CARTESIAN_POINT ( 'NONE',  ( 2.934579196337202323, 0.9245653808827180020, 1.466514439666162684 ) ) ;
#312 = CARTESIAN_POINT ( 'NONE',  ( 1.559489335033688251, -1.894147805384650995, -1.132260830144316888 ) ) ;
#313 = CARTESIAN_POINT ( 'NONE',  ( 5.248546085168739772, -2.154154806625402596, -0.2710006578958406576 ) ) ;
#314 = CARTESIAN_POINT ( 'NONE',  ( 5.034155109375821446, 4.767602470560229122, -0.7998128361456221525 ) ) ;
#315 = CARTESIAN_POINT ( 'NONE',  ( 5.682827415814322158, 1.645762192317705486, -1.164983060713747909 ) ) ;
#316 = CARTESIAN_POINT ( 'NONE',  ( 0.06249170576382599707, -1.450827213159947338, -1.451031289061120777 ) ) ;
#317 = VECTOR ( 'NONE', #161091, 1000.000000000000114 ) ;
#318 = CARTESIAN_POINT ( 'NONE',  ( -0.7500000000000215383, 3.722916667349487785, 1.299038105676671107 ) ) ;
#319 = CARTESIAN_POINT ( 'NONE',  ( 2.221590912301483645, -1.869112302256823011, 0.4658275329730912628 ) ) ;
#320 = CARTESIAN_POINT ( 'NONE',  ( -1.500000000000001110, 9.302083334016128191, 0.8660254037844419273 ) ) ;
#321 = CARTESIAN_POINT ( 'NONE',  ( 5.449557989901563815, -2.008192194917140849, 0.9499826718327757380 ) ) ;
#322 = VERTEX_POINT ( 'NONE', #162281 ) ;
#323 = CARTESIAN_POINT ( 'NONE',  ( 6.883263157960367806, 0.5819222519044697783, 1.998722019247618276 ) ) ;
#324 = CARTESIAN_POINT ( 'NONE',  ( -1.500000000000013101, 1.670833333333355153, 0.8660254037844403729 ) ) ;
#325 = CARTESIAN_POINT ( 'NONE',  ( 7.149227073107712549, 7.235186428247455837, -0.7998128361456281477 ) ) ;
#326 = CARTESIAN_POINT ( 'NONE',  ( 3.348500752450929596, 6.850408611260650815, 0.7216878364870317197 ) ) ;
#327 = CARTESIAN_POINT ( 'NONE',  ( 1.559560479473407701, -1.874198601735496794, 1.192037787016706485 ) ) ;
#328 = CARTESIAN_POINT ( 'NONE',  ( 6.373494408814909917, -0.2414686440028299685, 1.946897059556201848 ) ) ;
#329 = CARTESIAN_POINT ( 'NONE',  ( 8.758204044748010730, 9.320252261735261001, 0.7216878364870438212 ) ) ;
#330 = CARTESIAN_POINT ( 'NONE',  ( 4.797606254389322089, 6.690569611577942943, 1.599625672291268286 ) ) ;
#331 = CARTESIAN_POINT ( 'NONE',  ( -3.363831509966363598, 5.978201624052440266, -1.082531754730548412 ) ) ;
#332 = CARTESIAN_POINT ( 'NONE',  ( 4.211423687607918076, -1.713229066603161099, -1.148409633951211761 ) ) ;
#333 = CARTESIAN_POINT ( 'NONE',  ( -4.548924232584923288, 5.265832011892554121, -1.199719254218446718 ) ) ;
#334 = CARTESIAN_POINT ( 'NONE',  ( 1.499999999999990896, 5.306250000682820378, 1.214306433183764966E-14 ) ) ;
#335 = CARTESIAN_POINT ( 'NONE',  ( 1.364683531249986537, -0.8447916663252468261, -0.7879004041258309554 ) ) ;
#336 = CARTESIAN_POINT ( 'NONE',  ( 6.151601556293980977, 0.5431611868166182910, -1.789914130245950696 ) ) ;
#337 = CARTESIAN_POINT ( 'NONE',  ( 4.623498406067056088, 0.3027793956022621913, 1.707322668435699242 ) ) ;
#338 = CARTESIAN_POINT ( 'NONE',  ( 4.071615416877820692, -0.9979366678331093032, 1.425717084491331832 ) ) ;
#339 = CARTESIAN_POINT ( 'NONE',  ( 3.497113557321089861, 6.167384019261527683, -1.199719254218446718 ) ) ;
#340 = CARTESIAN_POINT ( 'NONE',  ( 1.453083402393087642, -1.969018001514400540, -1.173635730923931808 ) ) ;
#341 = CARTESIAN_POINT ( 'NONE',  ( -1.402160292154681736E-14, -1.178124999658576311, 1.575800808251672791 ) ) ;
#342 = CARTESIAN_POINT ( 'NONE',  ( 6.198786912940476235, 1.738631647849303130, 1.160874564816395615 ) ) ;
#343 = CARTESIAN_POINT ( 'NONE',  ( 0.6382991350510487383, -1.580419255802448575, 0.9442637585924051891 ) ) ;
#344 = CARTESIAN_POINT ( 'NONE',  ( -0.3817069231125022055, 3.999999999999974243, 1.007084182327149913 ) ) ;
#345 =( NAMED_UNIT ( * ) PLANE_ANGLE_UNIT ( ) SI_UNIT ( $, .RADIAN. ) );
#346 = CARTESIAN_POINT ( 'NONE',  ( 1.143204175302305670, 0.8197749522141674072, 1.842446510343001442 ) ) ;
#347 = CARTESIAN_POINT ( 'NONE',  ( 0.4280004979528989617, 1.123059939108238314, -1.881669248891951085 ) ) ;
#348 = CARTESIAN_POINT ( 'NONE',  ( 8.061225138011870683, 15.94050400400142564, -9.794890688158101710 ) ) ;
#349 = CARTESIAN_POINT ( 'NONE',  ( -7.039708073993679704, 9.236078724457858158, 1.599625672291283607 ) ) ;
#350 = CARTESIAN_POINT ( 'NONE',  ( 5.681030059326015014, 6.586622143090519188, -1.199719254218445830 ) ) ;
#351 = CARTESIAN_POINT ( 'NONE',  ( 1.360316468749973584, 2.786458333674735499, -0.7853790794159101196 ) ) ;
#352 = CARTESIAN_POINT ( 'NONE',  ( 3.018346832952636394, -2.117961878424143407, 0.1061830045200745365 ) ) ;
#353 = CARTESIAN_POINT ( 'NONE',  ( -1.364683531250000748, -0.4906249996585801409, 0.000000000000000000 ) ) ;
#354 = CARTESIAN_POINT ( 'NONE',  ( 5.707590141996651489, -0.4392596013848491521, 1.771934311310577659 ) ) ;
#355 = ORIENTED_EDGE ( 'NONE', *, *, #112300, .T. ) ;
#356 = CARTESIAN_POINT ( 'NONE',  ( -6.791708605802965870, 6.888357893050385705, -0.7998128361456362523 ) ) ;
#357 = PRESENTATION_STYLE_ASSIGNMENT (( #184467 ) ) ;
#358 = CARTESIAN_POINT ( 'NONE',  ( 5.194182247366861738, 9.073980031987776584, 0.7216878364870317197 ) ) ;
#359 = CARTESIAN_POINT ( 'NONE',  ( 3.475000000000000533, -3.631249999044082966, 0.000000000000000000 ) ) ;
#360 = CARTESIAN_POINT ( 'NONE',  ( -5.585069213825653023, 8.603332285183535433, -1.199719254218440723 ) ) ;
#361 = CARTESIAN_POINT ( 'NONE',  ( 3.674085990935217261, 2.004049791156937044, -0.2512726544132165563 ) ) ;
#362 = CARTESIAN_POINT ( 'NONE',  ( 6.458075443588827014, 2.201329523236052577, -0.1558686762383256763 ) ) ;
#363 = CARTESIAN_POINT ( 'NONE',  ( -5.336015975430226099, 8.383046517047350932, -1.199719254218453823 ) ) ;
#364 = CARTESIAN_POINT ( 'NONE',  ( 9.378489572351044856, 11.96465713920816043, -1.599625672291262513 ) ) ;
#365 = CARTESIAN_POINT ( 'NONE',  ( 4.698021595848828724, 0.7982989760673472324, -1.681190670221676120 ) ) ;
#366 = CARTESIAN_POINT ( 'NONE',  ( 9.413438726589914651, 9.876766690643398405, 0.000000000000000000 ) ) ;
#367 = CARTESIAN_POINT ( 'NONE',  ( 2.915646864528636417, 6.623614785250545367, 0.2169541561525832329 ) ) ;
#368 = CARTESIAN_POINT ( 'NONE',  ( -3.765413976293358278, 5.416068943807445635, 1.599625672291267398 ) ) ;
#369 = CARTESIAN_POINT ( 'NONE',  ( -8.532158741701643123, 8.848606708273724308, 0.7998128361456462443 ) ) ;
#370 = CARTESIAN_POINT ( 'NONE',  ( 0.3917762336288696523, 1.602822130585265015, 1.450656209987542855 ) ) ;
#372 = CARTESIAN_POINT ( 'NONE',  ( -4.265659997730736563, 7.487761795085347671, 1.069252549957976361 ) ) ;
#371 = CARTESIAN_POINT ( 'NONE',  ( -6.343235766347277149, 8.493804042195527870, -1.599625672291271394 ) ) ;
#373 = CARTESIAN_POINT ( 'NONE',  ( -1.364683531250014514, 0.4885416670080875434, -0.7879004041258289570 ) ) ;
#374 = CARTESIAN_POINT ( 'NONE',  ( 1.352469423652577607, -0.7852941029048329247, 1.545897522503926647 ) ) ;
#375 = CARTESIAN_POINT ( 'NONE',  ( 0.9545595967530025039, 0.3431710391763979073, -1.705965249089304470 ) ) ;
#377 = CARTESIAN_POINT ( 'NONE',  ( 9.083599731475992201, 9.699880562917908122, 0.7216878364870438212 ) ) ;
#376 = CARTESIAN_POINT ( 'NONE',  ( 0.2711454947614586608, -1.503558885491006247, 1.750568091222578282 ) ) ;
#378 = CARTESIAN_POINT ( 'NONE',  ( 2.905190055078214595, 6.611415174225076186, 0.7998128361456271485 ) ) ;
#379 = CARTESIAN_POINT ( 'NONE',  ( 2.091158219120598183, 1.794587730539594972, -1.012862355382545765 ) ) ;
#380 = CARTESIAN_POINT ( 'NONE',  ( 5.005985031943777308, 6.863401842066294556, -1.599625672291256295 ) ) ;
#381 = EDGE_CURVE ( 'NONE', #182271, #52415, #178195, .T. ) ;
#382 = CARTESIAN_POINT ( 'NONE',  ( 1.563827143785265328, 1.649830188709809686, -1.158509706484150970 ) ) ;
#383 = CARTESIAN_POINT ( 'NONE',  ( -0.6125000000000089262, 1.041666666666662966, 1.060881119635898040 ) ) ;
#384 = CARTESIAN_POINT ( 'NONE',  ( -4.610654757099099221, 7.536791762327691657, 1.199719254218452935 ) ) ;
#385 = AXIS2_PLACEMENT_3D ( 'NONE', #162717, #16422, #146480 ) ;
#386 = CARTESIAN_POINT ( 'NONE',  ( 6.420764531294745225, 1.746252128813120086, 0.6712297951826234899 ) ) ;
#388 = CARTESIAN_POINT ( 'NONE',  ( -6.834718835064852449, 8.106831741398025315, 1.082531754730549078 ) ) ;
#387 = CARTESIAN_POINT ( 'NONE',  ( 5.220932206144772714, 1.444093599275039885, -1.253800916539760113 ) ) ;
#389 = CARTESIAN_POINT ( 'NONE',  ( 6.656857027519620829, -1.708965229049699053, 1.396003577074665714 ) ) ;
#390 = CARTESIAN_POINT ( 'NONE',  ( -7.227905289416804102, 8.565549271475310533, -1.082531754730549967 ) ) ;
#391 = CARTESIAN_POINT ( 'NONE',  ( 7.201315867513990554, 8.430565262634994284, -1.199719254218452047 ) ) ;
#392 = EDGE_CURVE ( 'NONE', #179985, #120674, #60482, .T. ) ;
#393 = CARTESIAN_POINT ( 'NONE',  ( -4.977251789548269301, 4.979417640660637190, 0.7216878364870257245 ) ) ;
#394 = CARTESIAN_POINT ( 'NONE',  ( -0.09308815784560355022, -0.4424663830696302091, -1.977475021732390204 ) ) ;
#395 = CARTESIAN_POINT ( 'NONE',  ( -4.787437639401290745, 6.678706227425192488, 0.000000000000000000 ) ) ;
#396 = CARTESIAN_POINT ( 'NONE',  ( 4.085262347903253044, -0.2225469472450763153, -2.296823545465367822 ) ) ;
#397 = CARTESIAN_POINT ( 'NONE',  ( 5.090269282739749102, 1.010147525469132557, -1.681691772506640481 ) ) ;
#398 = CARTESIAN_POINT ( 'NONE',  ( 1.744895479173363517, -0.2825750800353257208, -1.941159045430330465 ) ) ;
#399 = CARTESIAN_POINT ( 'NONE',  ( 9.480175724453529185, 12.08329098332774265, 1.599625672291279388 ) ) ;
#400 = CARTESIAN_POINT ( 'NONE',  ( -3.511198596259299087, 6.271927390929313617, -7.499999999999997335 ) ) ;
#401 = VERTEX_POINT ( 'NONE', #180650 ) ;
#402 = CARTESIAN_POINT ( 'NONE',  ( -0.01227199510028028316, -0.5578357038005901103, 2.042509832261687475 ) ) ;
#403 = CARTESIAN_POINT ( 'NONE',  ( -3.899941742225307539, 7.701682465904834629, 0.7998128361456341429 ) ) ;
#404 = CARTESIAN_POINT ( 'NONE',  ( 0.6382991350510487383, -1.580419255802448575, 0.9442637585924050780 ) ) ;
#406 = CARTESIAN_POINT ( 'NONE',  ( 3.063685658700274761, 1.282989771343697294, 1.555699169480361022 ) ) ;
#405 = CARTESIAN_POINT ( 'NONE',  ( 4.399414683135016269, -1.891862197681973834, 1.064912953861403944 ) ) ;
#407 = CARTESIAN_POINT ( 'NONE',  ( 9.501800845313253419, 13.11895608245291101, -7.330069317485494729 ) ) ;
#408 = CARTESIAN_POINT ( 'NONE',  ( 1.494549364340029163, -1.129948290531690658, 1.794289463044356436 ) ) ;
#409 = CARTESIAN_POINT ( 'NONE',  ( -1.500000000000013101, 3.660416667349488673, -0.8660254037844313801 ) ) ;
#410 = CARTESIAN_POINT ( 'NONE',  ( 9.413438726589914651, 9.876766690643398405, 0.000000000000000000 ) ) ;
#411 = CARTESIAN_POINT ( 'NONE',  ( -1.886825320689270225, 2.480000000000016858, -2.459652456995881753 ) ) ;
#412 = CARTESIAN_POINT ( 'NONE',  ( 6.218145995260431214, 7.027935176161393294, 1.016989286988238206 ) ) ;
#413 = CARTESIAN_POINT ( 'NONE',  ( 2.407559617977403477, -0.4546984313768054342, 2.009812782922258734 ) ) ;
#414 = CIRCLE ( 'NONE', #87036, 11.09999999999999964 ) ;
#416 = DIRECTION ( 'NONE',  ( 0.000000000000000000, -1.000000000000000000, 0.000000000000000000 ) ) ;
#415 = CARTESIAN_POINT ( 'NONE',  ( -9.287498920561160887, 10.79416914786490089, -1.199719254218441611 ) ) ;
#417 = CARTESIAN_POINT ( 'NONE',  ( -0.6823417656250003738, 2.467708333674753618, -1.181850606188749264 ) ) ;
#418 = CARTESIAN_POINT ( 'NONE',  ( 0.07755575628183572490, 2.860544851022389867, -2.677061994759164065 ) ) ;
#419 = CARTESIAN_POINT ( 'NONE',  ( -5.738979324000901272, 5.917037536912919116, 2.440165351842437769 ) ) ;
#420 = CARTESIAN_POINT ( 'NONE',  ( 4.406835678522929456, -0.4222698756407486931, -1.864907683101609370 ) ) ;
#421 = CARTESIAN_POINT ( 'NONE',  ( 11.91826849282518275, 12.69999999999999929, -1.400000000000001465 ) ) ;
#422 = CARTESIAN_POINT ( 'NONE',  ( 1.669569175971203023, 0.1671416771932125456, -2.256311322606067371 ) ) ;
#423 = CARTESIAN_POINT ( 'NONE',  ( -4.464712657601869417, 4.103252943490596216, 0.7998128361456341429 ) ) ;
#425 = EDGE_CURVE ( 'NONE', #105059, #66250, #59241, .T. ) ;
#424 = CARTESIAN_POINT ( 'NONE',  ( 1.898416112216103624, -1.777124406008349533, -0.3506645682890742743 ) ) ;
#426 = CARTESIAN_POINT ( 'NONE',  ( 2.378032431427847371, -1.910899176573145342, -0.1362895805000780836 ) ) ;
#427 = CARTESIAN_POINT ( 'NONE',  ( 3.156751980976373329, -0.5984545454679365273, -1.982000093670479135 ) ) ;
#428 = CARTESIAN_POINT ( 'NONE',  ( 0.6823417656249882723, 1.238541667008083547, -1.181850606188749264 ) ) ;
#429 = AXIS2_PLACEMENT_3D ( 'NONE', #143118, #44524, #58621 ) ;
#430 = CARTESIAN_POINT ( 'NONE',  ( 0.3386658216258168763, 0.3346604457750371187, 1.942702894000091662 ) ) ;
#431 = CARTESIAN_POINT ( 'NONE',  ( 5.936148346467474468, 0.9475192508551170123, -1.677314091114836980 ) ) ;
#433 = CARTESIAN_POINT ( 'NONE',  ( 5.647444738788365726, 7.344714329438926548, -1.230740020431456028 ) ) ;
#432 = CARTESIAN_POINT ( 'NONE',  ( 0.6984242042700332664, -0.8252692633385866339, 2.155259511649917137 ) ) ;
#434 = CARTESIAN_POINT ( 'NONE',  ( -1.364683531250014514, 1.488541667008084435, -0.7879004041258289570 ) ) ;
#435 = CARTESIAN_POINT ( 'NONE',  ( 5.810998785189021909, -1.628375694745004321, 1.266036720739783128 ) ) ;
#436 = B_SPLINE_CURVE_WITH_KNOTS ( 'NONE', 3,
 ( #78019, #42351, #109537, #112728, #74835, #144144, #160344, #111660 ),
 .UNSPECIFIED., .F., .F.,
 ( 4, 2, 2, 4 ),
 ( 0.0006312381939941720749, 0.001000335483781913384, 0.001184884128675783984, 0.001369432773569654585 ),
 .UNSPECIFIED. ) ;
#437 = CARTESIAN_POINT ( 'NONE',  ( -5.575427483717760424, 7.527751369135936343, 1.599625672291269396 ) ) ;
#438 = CARTESIAN_POINT ( 'NONE',  ( 7.450369105909416589, 8.650851030771185890, -1.199719254218441611 ) ) ;
#439 = CARTESIAN_POINT ( 'NONE',  ( -0.9999999999999988898, 5.868705557303652398, -4.125226524755048807 ) ) ;
#441 = CARTESIAN_POINT ( 'NONE',  ( 0.7499999999999902300, 3.733333333333352488, 1.299038105676669330 ) ) ;
#440 = CARTESIAN_POINT ( 'NONE',  ( 5.139724016738759005, -1.487180916556319454, -1.491360876250556800 ) ) ;
#442 = EDGE_CURVE ( 'NONE', #108282, #170224, #25846, .T. ) ;
#443 = CARTESIAN_POINT ( 'NONE',  ( -1.364683531250012516, 2.301041667008087988, -0.7879004041258289570 ) ) ;
#444 = CARTESIAN_POINT ( 'NONE',  ( 5.044278900083454253, 2.155409826167026477, 0.1645634770654491874 ) ) ;
#445 = CARTESIAN_POINT ( 'NONE',  ( 4.916668454303085412, -0.6825918349771132876, -1.900952964002266210 ) ) ;
#446 = CARTESIAN_POINT ( 'NONE',  ( -3.795919822146315514, 7.372397525905186377, -0.7216878364870545903 ) ) ;
#447 = CARTESIAN_POINT ( 'NONE',  ( -3.931501358282937009, 7.530575984731317618, 0.7216878364870317197 ) ) ;
#450 = CARTESIAN_POINT ( 'NONE',  ( 5.422898255786183341, 7.349800603215774331, -1.443375672974051449 ) ) ;
#449 = CARTESIAN_POINT ( 'NONE',  ( 3.285556943750000070, -1.684374999522043836, 0.000000000000000000 ) ) ;
#448 = CARTESIAN_POINT ( 'NONE',  ( 6.339319342841494453, 9.553567112360518365, -1.199719254218452047 ) ) ;
#451 = CARTESIAN_POINT ( 'NONE',  ( -5.492988512192097161, 6.437516681426083132, 1.199719254218452935 ) ) ;
#452 = CARTESIAN_POINT ( 'NONE',  ( 3.274625289317079524, -0.3981104328964027994, -1.976669913042613747 ) ) ;
#453 = CARTESIAN_POINT ( 'NONE',  ( -8.045874094706015001, 11.47427131287732927, -1.199719254218446718 ) ) ;
#455 = CARTESIAN_POINT ( 'NONE',  ( -10.99896775280371486, -5.324706741106397523, 0.1653080603930973391 ) ) ;
#454 = CARTESIAN_POINT ( 'NONE',  ( -9.110716038703348119, 12.61262389758715408, 1.082531754730560403 ) ) ;
#456 = CARTESIAN_POINT ( 'NONE',  ( -0.6823417656249969321, 5.217708333674756283, -1.181850606188749264 ) ) ;
#458 = CARTESIAN_POINT ( 'NONE',  ( -1.364683531250014514, 8.588541667008065872, -0.7879004041258335089 ) ) ;
#457 = CARTESIAN_POINT ( 'NONE',  ( 4.979442225389012933, 2.018306902694905425, -0.7746836383674888804 ) ) ;
#459 = PRESENTATION_STYLE_ASSIGNMENT (( #53513 ) ) ;
#460 = CARTESIAN_POINT ( 'NONE',  ( -11.37874721094434527, 6.569860378138817403, -3.816774967323496082 ) ) ;
#462 = CARTESIAN_POINT ( 'NONE',  ( 5.360953910674266965, -0.05231296482399727665, -2.015913715532565043 ) ) ;
#461 = CARTESIAN_POINT ( 'NONE',  ( -5.856759170979136897, 9.776710099543576504, 0.000000000000000000 ) ) ;
#463 = CARTESIAN_POINT ( 'NONE',  ( 1.364683531249986537, -0.2822916663252520997, -0.7879004041258309554 ) ) ;
#464 = CARTESIAN_POINT ( 'NONE',  ( 0.3633288501447570207, 1.706897997983588322, -0.2475752363529682698 ) ) ;
#465 = CARTESIAN_POINT ( 'NONE',  ( 3.898851692381625877, 6.706354853490643642, -1.199719254218452047 ) ) ;
#467 = CARTESIAN_POINT ( 'NONE',  ( 5.332099551924443404, 9.442809587212341427, 0.000000000000000000 ) ) ;
#466 = CARTESIAN_POINT ( 'NONE',  ( 6.480434237652115570, 10.50433101066207442, 0.7216878364870438212 ) ) ;
#468 = DIRECTION ( 'NONE',  ( -0.1510067114093955887, -0.000000000000000000, -0.9885327375000383388 ) ) ;
#469 = CARTESIAN_POINT ( 'NONE',  ( 0.1921619543209041325, -0.3744425218715953796, -1.735604558297418443 ) ) ;
#470 =( BOUNDED_CURVE ( )  B_SPLINE_CURVE ( 3, ( #109998, #93702, #77422, #159743 ),
 .UNSPECIFIED., .F., .T. ) 
 B_SPLINE_CURVE_WITH_KNOTS ( ( 4, 4 ),
 ( 0.000000000000000000, 1.570796326794826836 ),
 .UNSPECIFIED. ) 
 CURVE ( )  GEOMETRIC_REPRESENTATION_ITEM ( )  RATIONAL_B_SPLINE_CURVE ( ( 1.000000000000000000, 0.8047378541243814798, 0.8047378541243814798, 1.000000000000000000 ) ) 
 REPRESENTATION_ITEM ( '' )  );
#471 = CARTESIAN_POINT ( 'NONE',  ( 1.313140557769366890, 1.644527964066449632, -1.160800818697106163 ) ) ;
#472 = CARTESIAN_POINT ( 'NONE',  ( -4.238987453163843178, 3.980249526191325771, 0.4947463914901452098 ) ) ;
#473 = AXIS2_PLACEMENT_3D ( 'NONE', #86071, #54636, #69791 ) ;
#474 = CARTESIAN_POINT ( 'NONE',  ( -6.902509602688821744, 8.185920970292658083, -1.082531754730549967 ) ) ;
#475 = EDGE_LOOP ( 'NONE', ( #184370, #199799, #47164, #11058, #211319, #194077, #40319, #83, #128481 ) ) ;
#476 = AXIS2_PLACEMENT_3D ( 'NONE', #130364, #209367, #32780 ) ;
#478 = CARTESIAN_POINT ( 'NONE',  ( 2.073842424929934314, -0.8596134062341630466, 1.824128527830502833 ) ) ;
#477 = CARTESIAN_POINT ( 'NONE',  ( 2.315225504062240702, 1.701464259299827919, -1.265282535349021575 ) ) ;
#479 = CARTESIAN_POINT ( 'NONE',  ( 2.724650786558381999, 1.309284593816659736, -1.252271045645783065 ) ) ;
#480 = CARTESIAN_POINT ( 'NONE',  ( 6.176621499477501054, 9.363752961769195693, -1.199719254218452047 ) ) ;
#481 = CARTESIAN_POINT ( 'NONE',  ( 6.754756207809571755, -1.674487575904315406, 1.366813541845832924 ) ) ;
#482 = ORIENTED_EDGE ( 'NONE', *, *, #180142, .T. ) ;
#483 = CARTESIAN_POINT ( 'NONE',  ( 7.474622759835693131, 7.614814729430110951, -0.7998128361456281477 ) ) ;
#485 = CARTESIAN_POINT ( 'NONE',  ( 0.6025738811294746311, 1.771267034891465642, 0.7302799438476501592 ) ) ;
#484 = CARTESIAN_POINT ( 'NONE',  ( -5.579343907223557331, 6.467988298970945849, 1.199719254218450271 ) ) ;
#486 = DIRECTION ( 'NONE',  ( 1.000000000000000000, -0.000000000000000000, -0.000000000000000000 ) ) ;
#487 = SURFACE_STYLE_USAGE ( .BOTH. , #166223 ) ;
#488 = CARTESIAN_POINT ( 'NONE',  ( 6.005898860729467437, 7.069598761348265370, -1.082531754730543083 ) ) ;
#489 = CARTESIAN_POINT ( 'NONE',  ( -1.402160292154681736E-14, 0.7593750003414168059, -1.575800808251659024 ) ) ;
#490 = CARTESIAN_POINT ( 'NONE',  ( 4.365362273920252889, 4.195270195769483124, 0.7216878364870317197 ) ) ;
#491 = CARTESIAN_POINT ( 'NONE',  ( -8.890396042259075315, 11.39521468743417998, -1.599625672291263179 ) ) ;
#492 = CARTESIAN_POINT ( 'NONE',  ( 4.100566281481184738, -0.6756360485904688851, -2.053482476349233643 ) ) ;
#493 = CARTESIAN_POINT ( 'NONE',  ( -5.722950238744243023, 7.770137593325314285, 1.443375672974058777 ) ) ;
#494 = CARTESIAN_POINT ( 'NONE',  ( 5.722950238744211937, 5.849399164722627553, 0.7216878364870328300 ) ) ;
#495 = CARTESIAN_POINT ( 'NONE',  ( 1.617596980227502756, 1.765956010477184535, 1.173731981927571555 ) ) ;
#496 = CARTESIAN_POINT ( 'NONE',  ( 6.422862827026682098, 1.704596635199370880, 0.6539724957527744964 ) ) ;
#497 = CARTESIAN_POINT ( 'NONE',  ( 3.339098322719173062, -1.740117145613935268, 0.9263661929081908886 ) ) ;
#498 = CARTESIAN_POINT ( 'NONE',  ( 5.642805672956042962, 1.844803604357934779, 0.5037821151940986564 ) ) ;
#499 = ORIENTED_EDGE ( 'NONE', *, *, #8528, .T. ) ;
#500 = DIRECTION ( 'NONE',  ( 0.000000000000000000, 0.000000000000000000, -1.000000000000000000 ) ) ;
#501 = CARTESIAN_POINT ( 'NONE',  ( 6.215292997425397203, -1.688482396400727170, -1.013753615619580106 ) ) ;
#502 = CARTESIAN_POINT ( 'NONE',  ( 1.201004818612857017, -0.4721336787944198643, 1.883569333377318245 ) ) ;
#503 = ORIENTED_EDGE ( 'NONE', *, *, #67371, .T. ) ;
#504 = CARTESIAN_POINT ( 'NONE',  ( -4.604929450496978660, 5.401447776115099408, -1.199719254218453823 ) ) ;
#505 = CARTESIAN_POINT ( 'NONE',  ( -6.455090533882201775, 8.624301270986276080, -1.443375672974066548 ) ) ;
#507 = CARTESIAN_POINT ( 'NONE',  ( 6.877010230629674759, 9.046264573866535486, 1.599625672291281386 ) ) ;
#506 = CARTESIAN_POINT ( 'NONE',  ( 2.449268230884271702, 0.5568478702235891697, -2.015041263885499756 ) ) ;
#510 = EDGE_CURVE ( 'NONE', #23152, #210434, #174637, .T. ) ;
#509 = CARTESIAN_POINT ( 'NONE',  ( 4.543390873910903238, 7.354354215321133204, 1.082531754730548412 ) ) ;
#508 = CARTESIAN_POINT ( 'NONE',  ( 6.174848896020108668, 9.291408581077091000, 1.199719254218460707 ) ) ;
#512 = VERTEX_POINT ( 'NONE', #98341 ) ;
#511 = CARTESIAN_POINT ( 'NONE',  ( 6.305323439471717251, 1.661359358424657318, -0.9468341723649562613 ) ) ;
#513 = CARTESIAN_POINT ( 'NONE',  ( 4.459734715955371520, 0.4851516707722826061, -2.152740496749529608 ) ) ;
#514 = CARTESIAN_POINT ( 'NONE',  ( 1.431021430919703574, 2.126993092707793132, 0.5877070120439558121 ) ) ;
#515 = CARTESIAN_POINT ( 'NONE',  ( 0.9614044138335111622, -1.507904615609249488, -1.175938229252027956 ) ) ;
#516 = CARTESIAN_POINT ( 'NONE',  ( -10.62873463776380234, 12.29999999999998295, 3.199999999999997957 ) ) ;
#517 = CARTESIAN_POINT ( 'NONE',  ( 8.886479618753304166, 12.45497775759917758, -1.199719254218446718 ) ) ;
#518 = CARTESIAN_POINT ( 'NONE',  ( 4.703616579153604427, -1.598285800263723688, -1.315984976451072708 ) ) ;
#519 = CARTESIAN_POINT ( 'NONE',  ( -6.087774667736030487, 7.061157519568837415, 1.199719254218450271 ) ) ;
#521 = CARTESIAN_POINT ( 'NONE',  ( 2.254944280175336324, -1.671361177491991201, 1.370965666894090385 ) ) ;
#520 = CARTESIAN_POINT ( 'NONE',  ( 1.123270288254022198, 2.908552654332631437, -0.7749999999939810591 ) ) ;
#522 = CARTESIAN_POINT ( 'NONE',  ( 3.966501855323391723, -2.045284974426237579, -0.7877190255709336508 ) ) ;
#523 = CARTESIAN_POINT ( 'NONE',  ( 10.39230484541318589, 3.447199233515649386, -6.000000000000107470 ) ) ;
#524 = CARTESIAN_POINT ( 'NONE',  ( -1.499999999999997780, 4.681250000682819490, 1.214306433183764966E-14 ) ) ;
#525 = CARTESIAN_POINT ( 'NONE',  ( 1.364683531249996529, 14.02604166700806942, 0.7879004041258405033 ) ) ;
#526 = CARTESIAN_POINT ( 'NONE',  ( -3.793249116773374396, 7.647484079536056356, 0.7998128361456352531 ) ) ;
#527 = PRODUCT_DEFINITION_CONTEXT ( 'detailed design', #188883, 'design' ) ;
#528 = CARTESIAN_POINT ( 'NONE',  ( 5.994686951402704800, -1.719894441074249158, 0.2214109503040090354 ) ) ;
#529 =( GEOMETRIC_REPRESENTATION_CONTEXT ( 3 ) GLOBAL_UNCERTAINTY_ASSIGNED_CONTEXT ( ( #23794 ) ) GLOBAL_UNIT_ASSIGNED_CONTEXT ( ( #120191, #135322, #18334 ) ) REPRESENTATION_CONTEXT ( 'NONE', 'WORKASPACE' ) );
#530 = CARTESIAN_POINT ( 'NONE',  ( -8.948018195339354719, 12.42280974699582607, 1.082531754730560403 ) ) ;
#531 = CARTESIAN_POINT ( 'NONE',  ( 3.731357587288412159, 0.05568397596692271218, -2.069689236595618542 ) ) ;
#532 = CARTESIAN_POINT ( 'NONE',  ( 5.343409318383084639, 0.4121200312635669993, -2.076573192147526115 ) ) ;
#533 = CARTESIAN_POINT ( 'NONE',  ( 5.666418135507635512, 8.698239360479199433, 1.199719254218462483 ) ) ;
#534 = CARTESIAN_POINT ( 'NONE',  ( 1.364683531249990311, 5.363541667008086655, 0.7879004041258499402 ) ) ;
#535 = CARTESIAN_POINT ( 'NONE',  ( 2.852355409199380798, -1.963852837454314271, -0.1495663577412101042 ) ) ;
#536 = CARTESIAN_POINT ( 'NONE',  ( 5.455124386806871506, 0.4517125544712205509, -2.247162937307800590 ) ) ;
#537 = CARTESIAN_POINT ( 'NONE',  ( 2.490611698265518648, -0.3118145247060916114, -1.798701865878708839 ) ) ;
#538 = ADVANCED_FACE ( 'NONE', ( #17059 ), #84921, .T. ) ;
#539 = CARTESIAN_POINT ( 'NONE',  ( 5.063044020060520900, 4.871582543017558109, 0.7998128361456352531 ) ) ;
#540 = CARTESIAN_POINT ( 'NONE',  ( 3.334942598837264960, 6.834590765378040444, 1.214306433183764966E-14 ) ) ;
#541 = CARTESIAN_POINT ( 'NONE',  ( -6.693975156845199059, 8.832723654451292816, 1.599625672291283607 ) ) ;
#542 = ORIENTED_EDGE ( 'NONE', *, *, #88694, .T. ) ;
#543 = ORIENTED_EDGE ( 'NONE', *, *, #68702, .T. ) ;
#544 = CARTESIAN_POINT ( 'NONE',  ( 4.183843882646627321, 1.951733592454238497, -0.4931575689418183917 ) ) ;
#545 = CARTESIAN_POINT ( 'NONE',  ( 4.223457129239616137, 0.2443821477370981265, -1.946437379933690481 ) ) ;
#546 = CARTESIAN_POINT ( 'NONE',  ( -7.802881099864745984, 9.062115023719057305, -1.199719254218446718 ) ) ;
#547 = CARTESIAN_POINT ( 'NONE',  ( -4.111146893441842920, 5.819424013814012753, 1.599625672291267398 ) ) ;
#548 = CARTESIAN_POINT ( 'NONE',  ( 0.1755611466353786954, 2.859968053823423784, -2.732108412375580109 ) ) ;
#550 = CARTESIAN_POINT ( 'NONE',  ( 5.858207189965921380, 0.7206212418228461480, 1.616676333947133504 ) ) ;
#549 = CARTESIAN_POINT ( 'NONE',  ( 0.3278234441896179518, 1.071198113070050972, -1.795324408978350439 ) ) ;
#551 = CARTESIAN_POINT ( 'NONE',  ( 10.99431798667268190, -5.199791778944933718, -0.3617173305618991974 ) ) ;
#552 = CARTESIAN_POINT ( 'NONE',  ( 2.343918204863020271, 2.190988169473460090, 0.05230688499441307066 ) ) ;
#553 = CARTESIAN_POINT ( 'NONE',  ( 0.6259951400321401849, 0.1256764613348868298, 1.735981902797034238 ) ) ;
#554 = VECTOR ( 'NONE', #28356, 1000.000000000000000 ) ;
#555 = CARTESIAN_POINT ( 'NONE',  ( 6.959412922516382771, 7.013736585890911535, 0.7998128361456341429 ) ) ;
#556 = CARTESIAN_POINT ( 'NONE',  ( 0.2335667940003048615, 2.868049447791064743, -2.641685461849890171 ) ) ;
#557 = CARTESIAN_POINT ( 'NONE',  ( 0.7676545703292583234, 0.8460830606174443158, 1.503042688352700829 ) ) ;
#558 = CARTESIAN_POINT ( 'NONE',  ( 0.6151802255017734256, 0.7180209600621060284, -2.183386540618210692 ) ) ;
#559 = CARTESIAN_POINT ( 'NONE',  ( 0.06437606466144081552, -1.426665095847098330, 1.663708609037084951 ) ) ;
#560 = CARTESIAN_POINT ( 'NONE',  ( 3.053566222061272040, -1.804402116661915967, -1.270350324234905903 ) ) ;
#561 = CARTESIAN_POINT ( 'NONE',  ( 1.112457285868488910, 2.168641027238225938, -0.1045176843600063021 ) ) ;
#562 = CARTESIAN_POINT ( 'NONE',  ( 0.3986991128735201673, 1.519733473351183362, -1.011397189243423700 ) ) ;
#563 = CARTESIAN_POINT ( 'NONE',  ( 2.694651208505644213, 1.530237149716510370, -1.463602791221560118 ) ) ;
#564 = CARTESIAN_POINT ( 'NONE',  ( 6.727182134110196721, 6.033756510516266935, 2.783943001041962795 ) ) ;
#565 = CARTESIAN_POINT ( 'NONE',  ( 5.913098435216375570, 1.699041482274340265, 0.9079036414736068039 ) ) ;
#566 = ORIENTED_EDGE ( 'NONE', *, *, #158591, .T. ) ;
#568 = CARTESIAN_POINT ( 'NONE',  ( -1.364683531250000748, 0.3218750003414205807, 0.000000000000000000 ) ) ;
#567 = CARTESIAN_POINT ( 'NONE',  ( 2.824086921994493071, 1.271197760638997254, -1.907441589200240983 ) ) ;
#569 = CARTESIAN_POINT ( 'NONE',  ( 2.496672843210871129, 6.064535417054653266, -0.7998128361456291469 ) ) ;
#570 = CARTESIAN_POINT ( 'NONE',  ( 5.681030059326015014, 6.586622143090519188, -1.199719254218445830 ) ) ;
#571 = AXIS2_PLACEMENT_3D ( 'NONE', #49828, #181943, #33573 ) ;
#572 = CARTESIAN_POINT ( 'NONE',  ( 4.987093027905733500, -2.091254775410257061, -0.7492775906185499268 ) ) ;
#573 = CARTESIAN_POINT ( 'NONE',  ( -7.754900677336769022, 9.110100880723427608, 1.082531754730558626 ) ) ;
#574 = EDGE_CURVE ( 'NONE', #72143, #200201, #108968, .T. ) ;
#575 = CYLINDRICAL_SURFACE ( 'NONE', #7911, 3.475000000000000089 ) ;
#576 = CARTESIAN_POINT ( 'NONE',  ( 6.656690234629796699, 6.868486149930637552, 1.040834085586084257E-14 ) ) ;
#577 = CARTESIAN_POINT ( 'NONE',  ( -7.659993601596720936, 8.999375959026737704, -1.082531754730543083 ) ) ;
#578 = CARTESIAN_POINT ( 'NONE',  ( 3.770576118376296471, 7.413106214832098750, 0.7216878364870257245 ) ) ;
#579 = ORIENTED_EDGE ( 'NONE', *, *, #182370, .T. ) ;
#580 = CARTESIAN_POINT ( 'NONE',  ( 2.672500184003968382, 1.427937546361924381, 1.423961308954827754 ) ) ;
#582 = CARTESIAN_POINT ( 'NONE',  ( 1.358340336993546726, -2.062741126468564890, -0.004002619933256982773 ) ) ;
#581 = CARTESIAN_POINT ( 'NONE',  ( 5.587931867126699537, 9.671004278289832001, -0.7998128361456291469 ) ) ;
#583 = CARTESIAN_POINT ( 'NONE',  ( 2.535847408461032609E-15, 11.09999999999999432, -0.2598076211376266764 ) ) ;
#584 = CARTESIAN_POINT ( 'NONE',  ( 3.702785349863636277, 7.334016984900627811, -0.7216878364870338292 ) ) ;
#585 = CARTESIAN_POINT ( 'NONE',  ( -6.905598574191406769, -7.287292132484036955, -6.905598574191375683 ) ) ;
#586 = CARTESIAN_POINT ( 'NONE',  ( -0.6823417656249969321, 3.217708333674754062, -1.181850606188749264 ) ) ;
#587 = CARTESIAN_POINT ( 'NONE',  ( 3.925867417771063739, 1.172880473742785812, -1.850976771919823793 ) ) ;
#588 = CARTESIAN_POINT ( 'NONE',  ( 1.020157974382044364, -1.821741137083273010, 0.8647263380179845971 ) ) ;
#589 = CARTESIAN_POINT ( 'NONE',  ( 0.7844012160764175512, 1.623964078452419857, -0.8677550623670119423 ) ) ;
#590 = CARTESIAN_POINT ( 'NONE',  ( 4.417794048288587128, 1.130693009273657124, -1.452954439256304520 ) ) ;
#591 = CARTESIAN_POINT ( 'NONE',  ( 7.202405917357655341, 9.425892875049191488, 1.599625672291281386 ) ) ;
#592 = SURFACE_STYLE_USAGE ( .BOTH. , #183645 ) ;
#593 = CARTESIAN_POINT ( 'NONE',  ( 5.508770632382115728, 1.381118045931900573, -1.193960910464037850 ) ) ;
#594 = CARTESIAN_POINT ( 'NONE',  ( 5.906875006520014182, -1.122496024291631755, -1.674889250513518446 ) ) ;
#595 = CARTESIAN_POINT ( 'NONE',  ( -8.015895134177625891, 10.37496362800581018, 1.599625672291295375 ) ) ;
#597 = CARTESIAN_POINT ( 'NONE',  ( -5.550083779947821760, 7.568460058062819407, -1.599625672291271394 ) ) ;
#596 = CARTESIAN_POINT ( 'NONE',  ( 4.153392199625399073, -1.879142691831453105, -1.259808711832038464 ) ) ;
#598 = CARTESIAN_POINT ( 'NONE',  ( 6.739294440770141392, -1.883009798889522024, 0.9431707147840006078 ) ) ;
#599 = CYLINDRICAL_SURFACE ( 'NONE', #53747, 0.3999999999999997446 ) ;
#600 = CARTESIAN_POINT ( 'NONE',  ( 5.090316257491098284, 1.067296284200716983, -1.773933887923849984 ) ) ;
#601 = CARTESIAN_POINT ( 'NONE',  ( 9.589694723567584234, 10.08239868711733855, -0.7998128361456281477 ) ) ;
#602 = APPLICATION_PROTOCOL_DEFINITION ( 'draft international standard', 'automotive_design', 1998, #188883 ) ;
#603 = B_SPLINE_CURVE_WITH_KNOTS ( 'NONE', 3,
 ( #59694, #174549, #207007, #60764, #12005, #143131 ),
 .UNSPECIFIED., .F., .F.,
 ( 4, 2, 4 ),
 ( 4.610090873601661862E-18, 9.933499788398740429E-05, 0.0001986699957679714476 ),
 .UNSPECIFIED. ) ;
#605 = CARTESIAN_POINT ( 'NONE',  ( 3.703666587441448943, -0.5581696590808477021, 1.843871709287647764 ) ) ;
#604 = CARTESIAN_POINT ( 'NONE',  ( -8.690940161559884913, 10.09818392903003748, 1.199719254218462483 ) ) ;
#606 = CARTESIAN_POINT ( 'NONE',  ( 6.556249800660121529, 9.806652646482286073, 1.199719254218452047 ) ) ;
#607 = CARTESIAN_POINT ( 'NONE',  ( 4.459584003380381745, 7.054591843250856975, -1.127873490090089748 ) ) ;
#608 = CARTESIAN_POINT ( 'NONE',  ( -4.288456660624211381, 3.897620947016656956, 1.214306433183764966E-14 ) ) ;
#610 = CARTESIAN_POINT ( 'NONE',  ( 1.231071286002645815, 1.486838745870424860, -1.650645422243676164 ) ) ;
#609 = CARTESIAN_POINT ( 'NONE',  ( 0.8969213510382867405, -2.070190491330957006, -0.4589741369691033857 ) ) ;
#611 = CARTESIAN_POINT ( 'NONE',  ( 3.399542317941701253, 1.658995184361473196, 1.297097526815289115 ) ) ;
#612 = CARTESIAN_POINT ( 'NONE',  ( -6.749980374757255319, 8.968339418673846097, 1.599625672291269396 ) ) ;
#613 = CARTESIAN_POINT ( 'NONE',  ( 5.289652487626049115, 9.323011668872403845, 0.7998128361456462443 ) ) ;
#614 = CARTESIAN_POINT ( 'NONE',  ( 2.822649888979886335, -1.354935067541668259, 1.419045635080482093 ) ) ;
#615 = CARTESIAN_POINT ( 'NONE',  ( 4.852928918687680948, 7.749168607522574526, 1.199719254218462483 ) ) ;
#616 = CARTESIAN_POINT ( 'NONE',  ( -4.047760499819613500, 7.578451897646762525, -0.3740945913360635977 ) ) ;
#617 = CARTESIAN_POINT ( 'NONE',  ( 5.508690485854129903, 5.321227076451600091, 1.040834085586084257E-14 ) ) ;
#618 = CARTESIAN_POINT ( 'NONE',  ( -6.617788377246204945, 6.893376992974917350, -0.7216878364870338292 ) ) ;
#619 = CARTESIAN_POINT ( 'NONE',  ( -7.754900677336769022, 9.110100880723427608, 1.082531754730558626 ) ) ;
#620 = CIRCLE ( 'NONE', #184019, 0.07999999999999951594 ) ;
#621 = CARTESIAN_POINT ( 'NONE',  ( 2.215225606797793567, 1.700350911433265555, -1.266953333846132512 ) ) ;
#622 = CARTESIAN_POINT ( 'NONE',  ( -6.720001414228860881, 7.869031733802326123, -1.199719254218452047 ) ) ;
#623 = CARTESIAN_POINT ( 'NONE',  ( 3.894932841003693191, 0.2855096342280309396, 1.940843471192068570 ) ) ;
#624 = CARTESIAN_POINT ( 'NONE',  ( 2.993221558690632556, 1.854768100113469265, -1.110066390340218367 ) ) ;
#625 = CARTESIAN_POINT ( 'NONE',  ( 3.034521004542716227, -1.622529355458858236, 0.8704296449140033198 ) ) ;
#626 = UNCERTAINTY_MEASURE_WITH_UNIT (LENGTH_MEASURE( 1.000000000000000082E-05 ), #100266, 'distance_accuracy_value', 'NONE');
#627 = AXIS2_PLACEMENT_3D ( 'NONE', #201676, #53323, #188656 ) ;
#628 = CARTESIAN_POINT ( 'NONE',  ( -4.379705010876359772, 7.173806194452361673, -1.050513582990858064 ) ) ;
#629 = CARTESIAN_POINT ( 'NONE',  ( -0.1007670162816230591, -8.052608368926286175, -9.499791922504428499 ) ) ;
#630 = ADVANCED_FACE ( 'NONE', ( #146201 ), #63852, .T. ) ;
#631 = CARTESIAN_POINT ( 'NONE',  ( 5.050617384047394687, -1.472844127453584839, -0.9267575401476387809 ) ) ;
#632 = DIRECTION ( 'NONE',  ( 1.207943261119674327E-30, 2.168404344971008079E-15, 1.000000000000000000 ) ) ;
#633 = CARTESIAN_POINT ( 'NONE',  ( 5.355107487717867265, 5.349972945200037522, 1.040834085586084257E-14 ) ) ;
#634 = CARTESIAN_POINT ( 'NONE',  ( -10.78402850230606447, 8.013881820625746499, 4.046242669647421408 ) ) ;
#635 = CARTESIAN_POINT ( 'NONE',  ( 2.377987466095924152, 1.329388817951412394, 1.704534938537699995 ) ) ;
#636 = CARTESIAN_POINT ( 'NONE',  ( 4.042342166264912606, 1.899327733865597168, -0.6766104081444989093 ) ) ;
#637 = CARTESIAN_POINT ( 'NONE',  ( -0.3978093821460775281, 3.011896635411767775, -0.3978093821461013424 ) ) ;
#638 = CARTESIAN_POINT ( 'NONE',  ( 0.9717996764858798375, 2.083101276202529384, -0.5774176476955604764 ) ) ;
#639 = CARTESIAN_POINT ( 'NONE',  ( 3.098462860235187133, -0.5706901479570201108, -1.887068881103808327 ) ) ;
#640 = CARTESIAN_POINT ( 'NONE',  ( 2.354701247847644119, -1.526412939949482128, 1.247560610424301109 ) ) ;
#641 = CARTESIAN_POINT ( 'NONE',  ( -1.237941840313982578, -1.374772708486751593, 1.500000000000001332 ) ) ;
#642 = CARTESIAN_POINT ( 'NONE',  ( 3.843253449720198667, 0.6512379428032251116, -1.829756300597375596 ) ) ;
#645 = ORIENTED_EDGE ( 'NONE', *, *, #104314, .F. ) ;
#644 = CARTESIAN_POINT ( 'NONE',  ( 10.91970695577495043, 0.000000000000000000, 5.204170427930421283E-15 ) ) ;
#643 = CARTESIAN_POINT ( 'NONE',  ( -8.134528978075012517, 12.43410820782212767, 1.040834085586084257E-14 ) ) ;
#646 = CARTESIAN_POINT ( 'NONE',  ( -7.228432174741334038, 8.462200954400218578, -1.199719254218452047 ) ) ;
#647 = CARTESIAN_POINT ( 'NONE',  ( 4.543917759235442944, 5.330267469643351852, 1.199719254218452935 ) ) ;
#648 = EDGE_CURVE ( 'NONE', #121570, #167726, #212215, .T. ) ;
#649 = CARTESIAN_POINT ( 'NONE',  ( -5.387385936583832802, 7.378645907471495846, -1.599625672291271394 ) ) ;
#650 = CARTESIAN_POINT ( 'NONE',  ( -8.148087131688679818, 12.44992605370473804, -0.7216878364870267237 ) ) ;
#651 = CARTESIAN_POINT ( 'NONE',  ( 0.9915960798324228165, 1.945464911009102460, -1.041603813667857370 ) ) ;
#652 = CARTESIAN_POINT ( 'NONE',  ( 3.285556943749998737, -3.755208332855373587, -1.896917185911906500 ) ) ;
#653 = CARTESIAN_POINT ( 'NONE',  ( 4.961744919065853132, -0.5270168765720646409, 1.889542207339139024 ) ) ;
#654 =( BOUNDED_CURVE ( )  B_SPLINE_CURVE ( 2, ( #165198, #117577, #152154, #180388, #116506, #83937, #35178, #199813, #213916 ),
 .UNSPECIFIED., .F., .T. ) 
 B_SPLINE_CURVE_WITH_KNOTS ( ( 3, 2, 2, 2, 3 ),
 ( 0.5468749999999997780, 0.5520833333333333703, 0.5625000000000000000, 0.5729166666666666297, 0.5781250000000001110 ),
 .UNSPECIFIED. ) 
 CURVE ( )  GEOMETRIC_REPRESENTATION_ITEM ( )  RATIONAL_B_SPLINE_CURVE ( ( 0.9330127018922194093, 0.9330127018922165227, 1.000000000000000000, 0.8660254037844387076, 1.000000000000000000, 0.8660254037844387076, 1.000000000000000000, 0.9330127018922178550, 0.9330127018922192983 ) ) 
 REPRESENTATION_ITEM ( '' )  );
#655 = ORIENTED_EDGE ( 'NONE', *, *, #150659, .T. ) ;
#656 = CARTESIAN_POINT ( 'NONE',  ( 3.151669946411875589, 2.064753251683769442, -0.4682690128248386818 ) ) ;
#657 = CARTESIAN_POINT ( 'NONE',  ( -0.7500000000000215383, 2.722916667349486897, 1.299038105676671107 ) ) ;
#659 = CARTESIAN_POINT ( 'NONE',  ( -5.850506979496850057, 6.784345216623154151, -1.199719254218446718 ) ) ;
#658 = CARTESIAN_POINT ( 'NONE',  ( 0.07479286986305544449, 2.046156589154801253, -2.272744413733415403 ) ) ;
#660 = CARTESIAN_POINT ( 'NONE',  ( 4.118977087773854961, -1.761250088754966692, 0.5364436722887636622 ) ) ;
#661 = ORIENTED_EDGE ( 'NONE', *, *, #178265, .T. ) ;
#662 = UNCERTAINTY_MEASURE_WITH_UNIT (LENGTH_MEASURE( 1.000000000000000082E-05 ), #182215, 'distance_accuracy_value', 'NONE');
#663 = CARTESIAN_POINT ( 'NONE',  ( -9.508345801885592863, 9.987491611821676329, 0.7998128361456462443 ) ) ;
#664 = DIRECTION ( 'NONE',  ( 1.000000000000000000, 0.000000000000000000, -1.465138070926357285E-17 ) ) ;
#665 = CARTESIAN_POINT ( 'NONE',  ( 5.519825572852568030, -0.5132647233585425628, 2.057443900658859182 ) ) ;
#666 = CARTESIAN_POINT ( 'NONE',  ( 0.000000000000000000, 0.6185895741317448682, 0.000000000000000000 ) ) ;
#667 = CARTESIAN_POINT ( 'NONE',  ( 6.311484202361478779, 7.322151976631905868, -1.199719254218446718 ) ) ;
#668 = ORIENTED_EDGE ( 'NONE', *, *, #118767, .F. ) ;
#669 = CARTESIAN_POINT ( 'NONE',  ( 5.554002131806472065, 2.058623415865985518, -0.09669752385456369115 ) ) ;
#670 = COLOUR_RGB ( '', 0.31764706, 0.68627451, 0.89019608) ;
#673 = CARTESIAN_POINT ( 'NONE',  ( 2.876309626556411203, -0.1380247437976732383, -1.836149222064882514 ) ) ;
#672 = CARTESIAN_POINT ( 'NONE',  ( 1.275590745840638363, -1.816738662498600165, 0.4029602180237248366 ) ) ;
#671 = DIRECTION ( 'NONE',  ( 1.000000000000000000, -0.000000000000000000, -0.000000000000000000 ) ) ;
#674 = CARTESIAN_POINT ( 'NONE',  ( 7.584896871841365851, 10.93646455286856956, -1.199719254218446718 ) ) ;
#675 = LINE ( 'NONE', #198886, #145063 ) ;
#676 = CARTESIAN_POINT ( 'NONE',  ( -6.583366107887490770, 9.838288338247510367, 1.199719254218452935 ) ) ;
#677 = DIRECTION ( 'NONE',  ( 0.000000000000000000, 1.000000000000000000, 0.000000000000000000 ) ) ;
#678 = CARTESIAN_POINT ( 'NONE',  ( 2.051678093609669240, -1.773579625386853875, -1.313098587465796774 ) ) ;
#679 = CARTESIAN_POINT ( 'NONE',  ( 5.448581927027607463, 0.6492139302081233465, 2.167288725150788409 ) ) ;
#680 = CARTESIAN_POINT ( 'NONE',  ( -6.317736394288148816, 8.393778431468064127, 1.443375672974078761 ) ) ;
#681 = CARTESIAN_POINT ( 'NONE',  ( 5.220911918456066836, 1.366450397884883428, -1.189473885788590035 ) ) ;
#682 = CARTESIAN_POINT ( 'NONE',  ( 5.612480213242726279, 1.848112342440700440, 0.5042863886801035589 ) ) ;
#683 = CARTESIAN_POINT ( 'NONE',  ( 1.284279953904121641, 3.077889714876734573, -0.7749999999999892530 ) ) ;
#684 = CARTESIAN_POINT ( 'NONE',  ( 5.172658500931742509, -1.761684834526537680, -0.6294727512598657926 ) ) ;
#685 = CARTESIAN_POINT ( 'NONE',  ( 4.527703488433511225, 1.805393378231552326, -0.4512502670087223944 ) ) ;
#686 = CARTESIAN_POINT ( 'NONE',  ( -1.364683531250010295, 5.488541667008087543, -0.7879004041258300672 ) ) ;
#687 = VECTOR ( 'NONE', #83277, 1000.000000000000000 ) ;
#688 = CARTESIAN_POINT ( 'NONE',  ( 6.561408083364261401, 0.2975169865880605835, -1.744492507556465011 ) ) ;
#689 = CARTESIAN_POINT ( 'NONE',  ( -0.1706859984542466180, -1.561801110730935971, -1.275320528755889526 ) ) ;
#691 = CARTESIAN_POINT ( 'NONE',  ( 2.649164382713434573, -1.750592827090621917, 1.170555837024005008 ) ) ;
#690 = CARTESIAN_POINT ( 'NONE',  ( -3.511198595814942980, 5.119484333249288532, 1.443375672974064550 ) ) ;
#692 = EDGE_CURVE ( 'NONE', #173454, #209728, #53694, .T. ) ;
#693 = CARTESIAN_POINT ( 'NONE',  ( 9.694243528971124846, 11.26870452434320491, 1.199719254218450271 ) ) ;
#695 = CARTESIAN_POINT ( 'NONE',  ( -9.398826802771548472, 11.98838390803207865, -1.599625672291263179 ) ) ;
#694 = DIRECTION ( 'NONE',  ( -1.276756478318932191E-15, 1.000000000000000000, -3.330669073875483426E-16 ) ) ;
#696 = DIRECTION ( 'NONE',  ( 0.000000000000000000, 0.000000000000000000, 1.000000000000000000 ) ) ;
#697 = CARTESIAN_POINT ( 'NONE',  ( 1.722921806169195547, 1.493705621373665915, -1.359711205623759023 ) ) ;
#698 = CARTESIAN_POINT ( 'NONE',  ( 0.6823417656249882723, 1.676041667008083769, -1.181850606188749264 ) ) ;
#699 = CARTESIAN_POINT ( 'NONE',  ( 6.620655732516645742, 3.706282450693794139, 2.340867613974298767 ) ) ;
#700 = ADVANCED_FACE ( 'NONE', ( #185046 ), #198533, .T. ) ;
#701 = CARTESIAN_POINT ( 'NONE',  ( 4.172158584703322681, 5.890604320285754980, -1.599625672291256295 ) ) ;
#702 = VERTEX_POINT ( 'NONE', #118001 ) ;
#703 = CARTESIAN_POINT ( 'NONE',  ( 1.827627302340195437, -2.036028831988645926, 0.7264203155534704193 ) ) ;
#704 = CARTESIAN_POINT ( 'NONE',  ( 6.889999999999967706, 3.707772630975701311, 2.234475054783117809 ) ) ;
#707 = DIRECTION ( 'NONE',  ( 0.6507913734559627184, 0.7592566023653016805, 0.000000000000000000 ) ) ;
#706 = FACE_OUTER_BOUND ( 'NONE', #213489, .T. ) ;
#705 = CARTESIAN_POINT ( 'NONE',  ( 3.413620815590684199, 7.204584394822967752, 0.7998128361456281477 ) ) ;
#708 = CARTESIAN_POINT ( 'NONE',  ( 9.856414487010592751, 10.60149777770828194, 0.7216878364870438212 ) ) ;
#709 = CARTESIAN_POINT ( 'NONE',  ( -1.201851678989727383E-14, 3.993750000682817713, 1.732050807568877637 ) ) ;
#710 = CARTESIAN_POINT ( 'NONE',  ( -7.619319141200077361, 9.912291636198670375, 1.443375672974090751 ) ) ;
#711 = CARTESIAN_POINT ( 'NONE',  ( 1.083813775577105565, -0.9808430935620198188, 1.959877696171570927 ) ) ;
#712 = CARTESIAN_POINT ( 'NONE',  ( 0.4301767877893971637, 8.007958762483859516, 1.954153227243374813 ) ) ;
#713 = CARTESIAN_POINT ( 'NONE',  ( 1.042281785820580176, 0.9147803334835495903, -2.069518175336809929 ) ) ;
#714 = CARTESIAN_POINT ( 'NONE',  ( -8.670602931139386627, 10.07445716020612103, 1.199719254218462483 ) ) ;
#715 = CARTESIAN_POINT ( 'NONE',  ( -3.592547517496929466, 7.135129837147637488, -0.7216878364870257245 ) ) ;
#716 = CARTESIAN_POINT ( 'NONE',  ( -0.6823417656250212460, 3.363541667008085323, 1.181850606188767472 ) ) ;
#717 = CARTESIAN_POINT ( 'NONE',  ( 4.763071791759735163, 8.170823326046956936, 0.7639991172946744014 ) ) ;
#718 = VECTOR ( 'NONE', #62707, 1000.000000000000000 ) ;
#719 = CARTESIAN_POINT ( 'NONE',  ( 1.499999999999993117, 11.35416666666667140, 0.8660254037844409281 ) ) ;
#720 = CARTESIAN_POINT ( 'NONE',  ( 4.848976215542928792, 5.686169002002086970, 1.199719254218452047 ) ) ;
#721 = CARTESIAN_POINT ( 'NONE',  ( 2.811481186154769496, -1.751065702721636308, 0.2553572387639922447 ) ) ;
#722 = CARTESIAN_POINT ( 'NONE',  ( 5.965903178300210108, 2.175115270774199416, -0.3715683035191638117 ) ) ;
#723 = CARTESIAN_POINT ( 'NONE',  ( -8.012344526598182026E-15, 15.35937500034140513, -1.575800808251669460 ) ) ;
#724 = ORIENTED_EDGE ( 'NONE', *, *, #115096, .T. ) ;
#725 = CARTESIAN_POINT ( 'NONE',  ( -5.448397627845328550, 7.449826213943242514, 1.599625672291263179 ) ) ;
#726 = CARTESIAN_POINT ( 'NONE',  ( 5.114861317887108072, 0.1511565883688982259, 2.010826320608386730 ) ) ;
#727 = ORIENTED_EDGE ( 'NONE', *, *, #105154, .T. ) ;
#728 = CARTESIAN_POINT ( 'NONE',  ( 2.219420098953532428, -1.815089452277141691, 0.4520615115926190919 ) ) ;
#729 = CARTESIAN_POINT ( 'NONE',  ( 3.854399998794607374, -2.067664388167046674, -0.1065051105964970740 ) ) ;
#730 = CARTESIAN_POINT ( 'NONE',  ( -0.5773502691896261751, -4.295408888568413630, -0.9999999999999991118 ) ) ;
#731 = CARTESIAN_POINT ( 'NONE',  ( 2.109489925670060551, 1.480643174185194200, 1.210387159491378650 ) ) ;
#732 = CARTESIAN_POINT ( 'NONE',  ( -1.436838838544753694, 7.449283400311743186, 4.203727439823589762 ) ) ;
#733 = CARTESIAN_POINT ( 'NONE',  ( -9.399770542442999144, 4.999985930147239799, -6.933469103752857521 ) ) ;
#734 = CARTESIAN_POINT ( 'NONE',  ( -7.235142258280575334, -6.594478602024302027, 7.235142258280601091 ) ) ;
#735 = CARTESIAN_POINT ( 'NONE',  ( 0.6823417656249899377, 3.988541667008085767, -1.181850606188754593 ) ) ;
#736 = CARTESIAN_POINT ( 'NONE',  ( 0.7559434568639654684, 0.7726834774516875282, -1.749509110286852742 ) ) ;
#737 = CARTESIAN_POINT ( 'NONE',  ( 6.590672070018850803, 7.822110515511036866, -1.082531754730548412 ) ) ;
#738 = CARTESIAN_POINT ( 'NONE',  ( 2.752341281506097470, -1.956419249932477955, -0.1471676765215298721 ) ) ;
#739 = CARTESIAN_POINT ( 'NONE',  ( 1.790313668900414878, -0.4735605917218765892, 0.7140520948302738757 ) ) ;
#740 = CARTESIAN_POINT ( 'NONE',  ( -5.822300622425855110, 5.757381912443740646, 0.7998128361456281477 ) ) ;
#741 = CARTESIAN_POINT ( 'NONE',  ( 5.185831674374465905, 2.043064739972153543, -0.5678235988075125418 ) ) ;
#743 = CARTESIAN_POINT ( 'NONE',  ( -11.96215121607992593, 13.82833553780824154, -0.9565349792967606790 ) ) ;
#742 = CARTESIAN_POINT ( 'NONE',  ( 10.08456733046637765, 10.65975006183261087, 0.000000000000000000 ) ) ;
#744 = CARTESIAN_POINT ( 'NONE',  ( 6.292255012522757873, -1.961630990407544406, -0.1958228842163112771 ) ) ;
#745 = CARTESIAN_POINT ( 'NONE',  ( -1.201851678989727383E-14, 2.321875000341416584, 1.575800808251672791 ) ) ;
#746 = CARTESIAN_POINT ( 'NONE',  ( 1.775641216270260170, 0.3400756789797795832, -1.984116031292797677 ) ) ;
#748 = CARTESIAN_POINT ( 'NONE',  ( 0.7204975843347528608, 2.086673352822054461, 0.3575386888887230885 ) ) ;
#747 = CARTESIAN_POINT ( 'NONE',  ( -7.592202833972775622, 8.920286730132099606, 1.082531754730558626 ) ) ;
#749 = CARTESIAN_POINT ( 'NONE',  ( 11.53069314862830552, 7.261250335387300581, -3.355468136185856487 ) ) ;
#750 = CARTESIAN_POINT ( 'NONE',  ( 2.225130849662222410, -1.891980959128433781, -0.8411517639917851508 ) ) ;
#751 = CARTESIAN_POINT ( 'NONE',  ( 4.041212305325117882, 6.872442235258051646, -1.199719254218448494 ) ) ;
#752 = CARTESIAN_POINT ( 'NONE',  ( 4.248501033035879004, 6.049946853332221153, -1.599625672291273171 ) ) ;
#753 = ORIENTED_EDGE ( 'NONE', *, *, #46793, .F. ) ;
#755 = CARTESIAN_POINT ( 'NONE',  ( 5.054492339796319733, 4.791329239384148231, -0.7998128361456211532 ) ) ;
#754 = CARTESIAN_POINT ( 'NONE',  ( 6.298786922650962516, 1.737427944715240091, 1.162477542130130548 ) ) ;
#758 = VERTEX_POINT ( 'NONE', #154712 ) ;
#757 = CARTESIAN_POINT ( 'NONE',  ( 2.789504176380937395, 1.719411750852325449, -0.5702826837221984801 ) ) ;
#756 = CARTESIAN_POINT ( 'NONE',  ( 3.873894609034499670, 1.013791609252197690, 1.518000939925366000 ) ) ;
#759 = CARTESIAN_POINT ( 'NONE',  ( 10.38962578677386084, 11.01565159419135043, 0.000000000000000000 ) ) ;
#760 = CARTESIAN_POINT ( 'NONE',  ( 10.67997715883384657, 8.352520031436601045, -3.105267373736821046 ) ) ;
#761 = CARTESIAN_POINT ( 'NONE',  ( 5.438574045396407541, 2.173287242562565780, 0.3821286992964008089 ) ) ;
#762 = CARTESIAN_POINT ( 'NONE',  ( -1.364683531250010740, 11.19270833367473550, 0.7879004041258445001 ) ) ;
#763 = ORIENTED_EDGE ( 'NONE', *, *, #8087, .T. ) ;
#764 = CARTESIAN_POINT ( 'NONE',  ( 3.615784255950851289, -0.5524401208748200842, 1.830756043982272097 ) ) ;
#765 = CARTESIAN_POINT ( 'NONE',  ( -8.123306592882240551, 12.62894145833798376, 0.000000000000000000 ) ) ;
#766 = CIRCLE ( 'NONE', #108191, 0.07999999999999998779 ) ;
#767 = CARTESIAN_POINT ( 'NONE',  ( 5.784525094524856748, 9.900363043587685041, 1.040834085586084257E-14 ) ) ;
#768 = CARTESIAN_POINT ( 'NONE',  ( 0.6801582343749952297, 2.088541667008066316, -1.178068619123855409 ) ) ;
#769 = CARTESIAN_POINT ( 'NONE',  ( 5.327991180046175224, 5.318337252916401248, -0.7216878364870207285 ) ) ;
#770 = CARTESIAN_POINT ( 'NONE',  ( -5.570361349191150779, 5.866663122702686195, 0.5491554309224304653 ) ) ;
#771 = DIRECTION ( 'NONE',  ( 8.638326563840814399E-31, -0.000000000000000000, 1.000000000000000000 ) ) ;
#772 = CARTESIAN_POINT ( 'NONE',  ( -0.1121326479804653220, -0.4008509640632436088, -1.803546454093779561 ) ) ;
#773 = EDGE_LOOP ( 'NONE', ( #1049, #99023, #98681, #151558, #138881, #82301, #133035, #37995, #73322, #97682, #96732, #136112, #8265, #74514, #72858, #38949, #164337, #200453 ) ) ;
#774 = CARTESIAN_POINT ( 'NONE',  ( 0.000000000000000000, 0.000000000000000000, 0.000000000000000000 ) ) ;
#775 = CARTESIAN_POINT ( 'NONE',  ( 4.885944009213345929, -0.8832235454491498272, 1.648918812636574804 ) ) ;
#776 = CARTESIAN_POINT ( 'NONE',  ( 6.481679955784983349, 9.719654494127929922, -1.199719254218452047 ) ) ;
#777 = CARTESIAN_POINT ( 'NONE',  ( 0.08053691275167890185, 14.48153890507870223, 11.99972973886013961 ) ) ;
#778 = CARTESIAN_POINT ( 'NONE',  ( -5.409340102172518705, 9.254721185935849803, 0.000000000000000000 ) ) ;
#779 = CARTESIAN_POINT ( 'NONE',  ( 4.310602774141044868, 7.116454772218158809, -1.199719254218452047 ) ) ;
#780 = CARTESIAN_POINT ( 'NONE',  ( 1.252720943002823883, -0.4733663544725670302, -1.911600023467324716 ) ) ;
#781 = CARTESIAN_POINT ( 'NONE',  ( 2.530875249677287719, -1.674875632724934338, 1.122518345125958383 ) ) ;
#782 = CARTESIAN_POINT ( 'NONE',  ( -7.537443334193545397, 10.88110209227943770, -1.199719254218446718 ) ) ;
#783 = CARTESIAN_POINT ( 'NONE',  ( 6.204791576909545192, 7.267953590263130259, -1.199719254218452047 ) ) ;
#784 = CARTESIAN_POINT ( 'NONE',  ( -1.115562610750309283E-14, 11.31249999999999822, 1.500000000000001554 ) ) ;
#785 = CARTESIAN_POINT ( 'NONE',  ( 2.273600812266802773, 1.349468827467028120, 1.726581335083368085 ) ) ;
#786 = CARTESIAN_POINT ( 'NONE',  ( 6.024025069106937913, -1.018266858664597763, -1.515143308444939274 ) ) ;
#787 = CARTESIAN_POINT ( 'NONE',  ( -4.620631424159025613, 4.285158171140619032, -0.7998128361456221525 ) ) ;
#788 = CARTESIAN_POINT ( 'NONE',  ( 6.717278222822382183, -7.473374494058216300, -6.830415307812249814 ) ) ;
#789 = CARTESIAN_POINT ( 'NONE',  ( 1.922735082439555487, -0.6236244280033541587, -0.2879360613984097150 ) ) ;
#790 = CARTESIAN_POINT ( 'NONE',  ( 3.757017964762656703, 7.397288368949487491, -1.734723475976807094E-15 ) ) ;
#791 = CARTESIAN_POINT ( 'NONE',  ( 8.235688245297327015, 11.69572115523387268, -1.199719254218446718 ) ) ;
#792 = DIRECTION ( 'NONE',  ( -0.5265943820737358783, 0.4485553919928856326, 0.7221470882600643515 ) ) ;
#793 = CARTESIAN_POINT ( 'NONE',  ( 5.709392085130549077, 9.675058176045386205, 0.000000000000000000 ) ) ;
#794 = EDGE_LOOP ( 'NONE', ( #170295, #136868, #121989, #212162, #31787, #181573, #75016, #98751 ) ) ;
#796 = CARTESIAN_POINT ( 'NONE',  ( 0.9264321329857813092, -0.9072109017984790746, -1.797169606962043309 ) ) ;
#795 = CARTESIAN_POINT ( 'NONE',  ( 4.036529152626888717, -1.599951230533543267, 0.9111318136766360931 ) ) ;
#797 = CARTESIAN_POINT ( 'NONE',  ( 2.724286267170890952, -1.998689782195923081, -1.134749220811093418 ) ) ;
#799 = CARTESIAN_POINT ( 'NONE',  ( 0.7603355536747276044, -0.6198598984368717257, -1.754846704163029125 ) ) ;
#798 = CARTESIAN_POINT ( 'NONE',  ( 3.145128448690309053, 4.692402494937224056, -1.443375672974057666 ) ) ;
#800 = CARTESIAN_POINT ( 'NONE',  ( 0.000000000000000000, -0.08749999999999961975, -4.012584370867899430 ) ) ;
#801 = CARTESIAN_POINT ( 'NONE',  ( -2.740719608256871442, 6.349256642941639051, 0.7998128361456341429 ) ) ;
#802 = CYLINDRICAL_SURFACE ( 'NONE', #123024, 1.250000000000000000 ) ;
#803 = CARTESIAN_POINT ( 'NONE',  ( 4.218947473185084007, 1.474887410857337100, -1.217315437338606365 ) ) ;
#804 = CARTESIAN_POINT ( 'NONE',  ( -9.332089804907933939, 9.781859615347734405, 1.040834085586084257E-14 ) ) ;
#805 = CARTESIAN_POINT ( 'NONE',  ( -6.292392690518209264, 8.434487120394948079, -1.443375672974066548 ) ) ;
#807 = CARTESIAN_POINT ( 'NONE',  ( 2.553401164250346245, 0.5009360343536627402, -1.802255699741683870 ) ) ;
#806 = CARTESIAN_POINT ( 'NONE',  ( 4.159774813393120496, 0.9870934738810345221, 1.843074783240926884 ) ) ;
#808 = CARTESIAN_POINT ( 'NONE',  ( 7.131225611108085616, 10.30321839872603462, 1.082531754730558626 ) ) ;
#809 = CARTESIAN_POINT ( 'NONE',  ( -1.001543065824772872E-14, 5.634375000341417028, 1.575800808251672791 ) ) ;
#810 = CARTESIAN_POINT ( 'NONE',  ( 5.601068772352080671, -0.4412860211496574814, 1.787476196608045464 ) ) ;
#811 = CIRCLE ( 'NONE', #45881, 2.725000000000000089 ) ;
#812 = CARTESIAN_POINT ( 'NONE',  ( 4.518945272056516416, 4.166524327021037699, 0.7998128361456341429 ) ) ;
#813 = CARTESIAN_POINT ( 'NONE',  ( 5.928835565505618632, 6.052265235248638575, -0.5446974197955555264 ) ) ;
#814 = CARTESIAN_POINT ( 'NONE',  ( 5.127475435434773132, -1.636205250265274191, 0.5461684234016728201 ) ) ;
#815 = CARTESIAN_POINT ( 'NONE',  ( -5.377780486114890124, 9.425827667109372143, 0.000000000000000000 ) ) ;
#816 = CARTESIAN_POINT ( 'NONE',  ( 0.2637851986186890429, 1.619078963417280859, -0.6216347861247341067 ) ) ;
#817 = CARTESIAN_POINT ( 'NONE',  ( 6.340462157465731607, 2.182225300935904055, 0.3281612982340698093 ) ) ;
#818 = CARTESIAN_POINT ( 'NONE',  ( 1.123270288250311610, 3.110197346350006331, 0.7749999999993734123 ) ) ;
#819 = CARTESIAN_POINT ( 'NONE',  ( 1.743066579297358008E-15, 0.7500000006828128063, -1.225000000000021849 ) ) ;
#820 = CARTESIAN_POINT ( 'NONE',  ( 4.979425714853139340, -0.1133551455631234828, 2.168255935233906584 ) ) ;
#821 = CARTESIAN_POINT ( 'NONE',  ( 3.387140609607977026, 1.650079954178599539, -0.7815607168924765258 ) ) ;
#822 = CARTESIAN_POINT ( 'NONE',  ( 0.9538670997781794059, -0.7113550649951918547, 1.828410001767373450 ) ) ;
#823 = CARTESIAN_POINT ( 'NONE',  ( 5.278551870535488355, -0.5171574069430958653, -2.053072726559619365 ) ) ;
#824 = VERTEX_POINT ( 'NONE', #187194 ) ;
#825 = ADVANCED_FACE ( 'NONE', ( #183991 ), #39943, .T. ) ;
#827 = CARTESIAN_POINT ( 'NONE',  ( -1.364683531250012516, 3.592708333674750509, 0.7879004041258379498 ) ) ;
#826 = CARTESIAN_POINT ( 'NONE',  ( 5.566080547264319556, -1.456586111465259403, 1.770153815000871989 ) ) ;
#828 = CARTESIAN_POINT ( 'NONE',  ( 8.971744963941056028, 11.49012176272984931, 1.599625672291281386 ) ) ;
#829 = CARTESIAN_POINT ( 'NONE',  ( 1.576976220782677185, -1.497206391897941913, 1.501870991332490135 ) ) ;
#830 = CARTESIAN_POINT ( 'NONE',  ( -5.938108093105513241, 6.030140318152288792, 0.7216878364870317197 ) ) ;
#831 = EDGE_CURVE ( 'NONE', #191521, #28791, #95318, .T. ) ;
#832 = CYLINDRICAL_SURFACE ( 'NONE', #156750, 1.250000000000000000 ) ;
#833 = VECTOR ( 'NONE', #207710, 1000.000000000000000 ) ;
#834 = B_SPLINE_CURVE_WITH_KNOTS ( 'NONE', 3,
 ( #91115, #202684, #5534, #157174, #88976, #21785, #39148 ),
 .UNSPECIFIED., .F., .F.,
 ( 4, 3, 4 ),
 ( 0.002201685690204611880, 0.002395020826490580276, 0.002952547457960625829 ),
 .UNSPECIFIED. ) ;
#835 = CARTESIAN_POINT ( 'NONE',  ( -4.080641047588907888, 6.744203074620265248, -1.082531754730548412 ) ) ;
#836 =( GEOMETRIC_REPRESENTATION_CONTEXT ( 3 ) GLOBAL_UNCERTAINTY_ASSIGNED_CONTEXT ( ( #213503 ) ) GLOBAL_UNIT_ASSIGNED_CONTEXT ( ( #89871, #123512, #158065 ) ) REPRESENTATION_CONTEXT ( 'NONE', 'WORKASPACE' ) );
#837 = CARTESIAN_POINT ( 'NONE',  ( 6.561400879130542485, 1.800260439488234443, 1.213256210689506176 ) ) ;
#839 = CARTESIAN_POINT ( 'NONE',  ( 0.7500000000000006661, 12.44791666734946389, -1.299038105676657340 ) ) ;
#838 = CARTESIAN_POINT ( 'NONE',  ( 6.983263157960362122, 6.035089925019382129, 2.648702789725385198 ) ) ;
#840 = ORIENTED_EDGE ( 'NONE', *, *, #141283, .F. ) ;
#842 = ORIENTED_EDGE ( 'NONE', *, *, #62981, .F. ) ;
#841 = CARTESIAN_POINT ( 'NONE',  ( 2.051734446849303506, -1.982521776546506853, 1.002060208660388474 ) ) ;
#843 = CARTESIAN_POINT ( 'NONE',  ( 6.135388727473008785, 0.6351960432287793168, 1.913804721665197883 ) ) ;
#845 = CARTESIAN_POINT ( 'NONE',  ( 4.012594160722949610, 0.7376926799337081286, 1.926325278971857236 ) ) ;
#844 = CARTESIAN_POINT ( 'NONE',  ( 2.849184837166184536, 6.475799410002530898, 0.7998128361456362523 ) ) ;
#847 = CARTESIAN_POINT ( 'NONE',  ( -3.475000000000000533, -3.849999999999999201, 0.000000000000000000 ) ) ;
#846 = CARTESIAN_POINT ( 'NONE',  ( 6.964048179274811012, 8.153752959689313684, 1.199719254218452047 ) ) ;
#848 = CARTESIAN_POINT ( 'NONE',  ( 6.225128807330042591, 7.291680359087043151, -1.199719254218452047 ) ) ;
#849 = CARTESIAN_POINT ( 'NONE',  ( -1.642778471874998480, -3.288541666188707246, 2.845375778867863303 ) ) ;
#850 = DIRECTION ( 'NONE',  ( -2.103352214621884660E-13, 0.000000000000000000, 1.000000000000000000 ) ) ;
#851 = CARTESIAN_POINT ( 'NONE',  ( 0.7793769126323678575, 1.405529721366456597, 1.547827308177295746 ) ) ;
#852 = CARTESIAN_POINT ( 'NONE',  ( 4.219375079941334761, 1.978050461189932552, 0.3905991720301109082 ) ) ;
#853 = CARTESIAN_POINT ( 'NONE',  ( 4.528748383445759806, -1.681502307688139908, 0.7506017836093890061 ) ) ;
#855 = ORIENTED_EDGE ( 'NONE', *, *, #55426, .T. ) ;
#854 = CARTESIAN_POINT ( 'NONE',  ( 3.832150974156964818, 7.622593236491780999, 1.040834085586084257E-14 ) ) ;
#856 = CARTESIAN_POINT ( 'NONE',  ( 1.834533585138716782, 0.1645414454686990324, 1.716894335133994698 ) ) ;
#857 = CARTESIAN_POINT ( 'NONE',  ( 0.04025042243083893495, 0.7762349914572730381, 1.861342399428978389 ) ) ;
#858 = CARTESIAN_POINT ( 'NONE',  ( 1.424907242902058613, -1.669187457468356950, -1.580674740522235888 ) ) ;
#859 = CARTESIAN_POINT ( 'NONE',  ( -6.144869935491728441, 8.192100896205577243, -1.599625672291263179 ) ) ;
#860 = CARTESIAN_POINT ( 'NONE',  ( 1.230147817042701375, -1.435374304221140651, -1.748800500726248153 ) ) ;
#861 = CARTESIAN_POINT ( 'NONE',  ( 3.774133669461790852, 1.169908569812891264, 1.751025317131530423 ) ) ;
#862 = CARTESIAN_POINT ( 'NONE',  ( -5.483346782084204563, 5.361935765378481378, 0.000000000000000000 ) ) ;
#863 = CARTESIAN_POINT ( 'NONE',  ( 7.637320603199683866, 7.804628880021436288, -0.7998128361456281477 ) ) ;
#864 = CARTESIAN_POINT ( 'NONE',  ( 6.360183458142179447, 6.592837920686898556, -0.7216878364870458196 ) ) ;
#865 = CARTESIAN_POINT ( 'NONE',  ( 6.687508294236179651, -1.450827213159664675, 1.451031289061379681 ) ) ;
#866 = CARTESIAN_POINT ( 'NONE',  ( -4.791917227426195858, 7.677988301050826969, -1.199719254218452047 ) ) ;
#867 = CARTESIAN_POINT ( 'NONE',  ( 5.463572716182819811, 8.357623354646536384, 1.082531754730558626 ) ) ;
#868 = CARTESIAN_POINT ( 'NONE',  ( -1.402160292154681736E-14, 1.837500000000019895, -1.732050807568863648 ) ) ;
#869 = AXIS2_PLACEMENT_3D ( 'NONE', #75473, #189221, #172990 ) ;
#870 = CARTESIAN_POINT ( 'NONE',  ( -2.761056838677368397, 6.372983411765559048, 0.7998128361456341429 ) ) ;
#871 = CARTESIAN_POINT ( 'NONE',  ( 5.607756438734910809, 1.682095628590657643, 1.451081198120441229 ) ) ;
#872 = CARTESIAN_POINT ( 'NONE',  ( 3.398540877415173966, 1.727514402264049620, -1.348270469230819391 ) ) ;
#873 = CARTESIAN_POINT ( 'NONE',  ( -6.261168011412601153, 6.199117522936475666, 1.040834085586084257E-14 ) ) ;
#874 = CARTESIAN_POINT ( 'NONE',  ( -5.496904935697871863, 5.377753611261092637, 0.7998128361456281477 ) ) ;
#875 = CARTESIAN_POINT ( 'NONE',  ( 6.111998723603361938, -0.7147493727725148238, 1.996541221815250733 ) ) ;
#876 = CARTESIAN_POINT ( 'NONE',  ( 1.364683531249988535, 3.905208333674751842, -0.7879004041258239610 ) ) ;
#877 = CARTESIAN_POINT ( 'NONE',  ( 6.610000000000006537, 0.002781820520842553934, 2.000159646111852929 ) ) ;
#878 = CARTESIAN_POINT ( 'NONE',  ( -5.260200412422208593, 7.159986452624450770, -1.443375672974053447 ) ) ;
#879 = CARTESIAN_POINT ( 'NONE',  ( 5.590118541908202232, 1.264772504208915072, 1.701965355810124203 ) ) ;
#880 = CARTESIAN_POINT ( 'NONE',  ( -7.105881907338169157, 8.423188659050232729, -1.082531754730549967 ) ) ;
#881 = ORIENTED_EDGE ( 'NONE', *, *, #139074, .T. ) ;
#883 = CARTESIAN_POINT ( 'NONE',  ( 6.438358464623771482, 2.137424745569570295, 0.3223339197731683869 ) ) ;
#882 = CARTESIAN_POINT ( 'NONE',  ( -5.478903473698268023, 5.564677938835638216, -0.7216878364870338292 ) ) ;
#884 = CARTESIAN_POINT ( 'NONE',  ( 5.005985031943777308, 6.863401842066294556, -1.599625672291256295 ) ) ;
#885 = CARTESIAN_POINT ( 'NONE',  ( 11.84668730067608600, 13.40000000000000036, -1.400000000000001910 ) ) ;
#886 = UNCERTAINTY_MEASURE_WITH_UNIT (LENGTH_MEASURE( 1.000000000000000082E-05 ), #29913, 'distance_accuracy_value', 'NONE');
#887 = CARTESIAN_POINT ( 'NONE',  ( 1.364683531249988535, 2.176041667008087543, 0.7879004041258500513 ) ) ;
#888 = CARTESIAN_POINT ( 'NONE',  ( 1.628031597684251208, 0.1703553616784689029, 1.732092769550299227 ) ) ;
#889 = CARTESIAN_POINT ( 'NONE',  ( 2.737856954955798727, 5.281584649835344258, 1.199719254218452047 ) ) ;
#890 = FACE_OUTER_BOUND ( 'NONE', #59511, .T. ) ;
#891 = CARTESIAN_POINT ( 'NONE',  ( -1.402160292154681736E-14, 0.5093750003414236893, -1.575800808251659024 ) ) ;
#892 = CARTESIAN_POINT ( 'NONE',  ( -0.3000000000000117573, 3.322650755865466543, -0.5865692111442739609 ) ) ;
#893 = CARTESIAN_POINT ( 'NONE',  ( 4.891577088959510711, 1.599438101461609918, 1.454397306527709155 ) ) ;
#894 = CARTESIAN_POINT ( 'NONE',  ( -4.081167932913447594, 4.720116328942494555, -1.199719254218452047 ) ) ;
#895 = CARTESIAN_POINT ( 'NONE',  ( -6.439759776366783761, 8.536139043893143707, 1.443375672974078761 ) ) ;
#896 = CARTESIAN_POINT ( 'NONE',  ( 5.084929678302336775, -0.2608814864752464491, -2.145832476913120068 ) ) ;
#897 = VERTEX_POINT ( 'NONE', #202354 ) ;
#898 = CARTESIAN_POINT ( 'NONE',  ( -1.364683531250012516, 3.530208333674758059, 0.7879004041258379498 ) ) ;
#899 = CARTESIAN_POINT ( 'NONE',  ( 6.292255012522757873, -1.961630990407544406, -0.1958228842163112771 ) ) ;
#900 = CARTESIAN_POINT ( 'NONE',  ( 4.956219290344169970, 1.285291309562084816, 1.163873732738918587 ) ) ;
#902 = CARTESIAN_POINT ( 'NONE',  ( 1.558417602779540889, -1.546676288433556756, 1.552911753681482487 ) ) ;
#901 = CARTESIAN_POINT ( 'NONE',  ( 1.360316468750001784, -0.7552083329919376808, 0.7853790794158941324 ) ) ;
#903 = CARTESIAN_POINT ( 'NONE',  ( 2.151827808644761308, -1.853761708218491178, -1.374033529217959515 ) ) ;
#904 = CARTESIAN_POINT ( 'NONE',  ( 4.780574613336814771, -1.997868641178605298, -0.5047315492533087644 ) ) ;
#905 = CARTESIAN_POINT ( 'NONE',  ( 6.515186996419942034, -1.882659881547473546, 0.4762376372081030262 ) ) ;
#906 = CARTESIAN_POINT ( 'NONE',  ( -6.141480396866151992, 9.148515648777049591, 1.082531754730548412 ) ) ;
#907 = B_SPLINE_CURVE_WITH_KNOTS ( 'NONE', 3,
 ( #57698, #90211, #123855, #54496 ),
 .UNSPECIFIED., .F., .F.,
 ( 4, 4 ),
 ( 0.000000000000000000, 2.032232339064896589E-05 ),
 .UNSPECIFIED. ) ;
#908 = CARTESIAN_POINT ( 'NONE',  ( -5.517242166118370150, 5.401480380085008193, 0.7998128361456281477 ) ) ;
#909 = CARTESIAN_POINT ( 'NONE',  ( 4.758470758277942636, 5.183766117661583017, 0.9120521451414279612 ) ) ;
#910 = EDGE_CURVE ( 'NONE', #102469, #190223, #25470, .T. ) ;
#911 = CARTESIAN_POINT ( 'NONE',  ( 3.287459871768631636, 0.04819156399121089784, -2.120204644799832394 ) ) ;
#912 = CARTESIAN_POINT ( 'NONE',  ( -1.499999999999997780, 5.150000000000022560, 1.214306433183764966E-14 ) ) ;
#913 = CARTESIAN_POINT ( 'NONE',  ( 1.547500230860882287, -1.423960469535384465, 1.427938386157491246 ) ) ;
#914 = CARTESIAN_POINT ( 'NONE',  ( -6.765155463094763455, 8.915767345075790828, 1.443375672974078761 ) ) ;
#915 = CARTESIAN_POINT ( 'NONE',  ( 4.735508036034060453, -2.019198892066270457, 0.8907332283012432406 ) ) ;
#916 = CARTESIAN_POINT ( 'NONE',  ( -1.642778471875000035, -1.655208332855377051, -2.845375778867859751 ) ) ;
#917 = CARTESIAN_POINT ( 'NONE',  ( 2.307254945994464457, -1.491077236629720248, -1.113220461199310618 ) ) ;
#918 = CARTESIAN_POINT ( 'NONE',  ( -7.986233326679965216, -6.863455982311493564, 7.564733433744408764 ) ) ;
#919 = DIRECTION ( 'NONE',  ( 8.638326563840814399E-31, 0.000000000000000000, 1.000000000000000000 ) ) ;
#921 = CARTESIAN_POINT ( 'NONE',  ( 6.825078400183582694, 7.051583320515966591, 2.842498375355909435 ) ) ;
#920 = CARTESIAN_POINT ( 'NONE',  ( -5.476171693740270463, 7.594609835490887306, -1.347918582746489902 ) ) ;
#922 = FACE_OUTER_BOUND ( 'NONE', #13196, .T. ) ;
#923 = ORIENTED_EDGE ( 'NONE', *, *, #66878, .F. ) ;
#924 = CARTESIAN_POINT ( 'NONE',  ( 3.080987681966301572, -0.1499786273361273514, -2.055480798767507444 ) ) ;
#925 = CARTESIAN_POINT ( 'NONE',  ( 1.360316468749992236, 2.015625000341400685, -1.040834085586084257E-14 ) ) ;
#926 = UNCERTAINTY_MEASURE_WITH_UNIT (LENGTH_MEASURE( 1.000000000000000082E-05 ), #6639, 'distance_accuracy_value', 'NONE');
#927 = CARTESIAN_POINT ( 'NONE',  ( -5.961834861707238531, 7.978559976790334574, -1.599625672291263179 ) ) ;
#928 = CARTESIAN_POINT ( 'NONE',  ( 3.158857784513937617, 0.4929582698031101939, 1.958447305144744410 ) ) ;
#929 = CARTESIAN_POINT ( 'NONE',  ( -0.7500000000000006661, -0.8916666666666448471, -1.299038105676652011 ) ) ;
#930 = CARTESIAN_POINT ( 'NONE',  ( 9.571693261567954636, 12.19006144329456731, 1.443375672974076540 ) ) ;
#931 = CARTESIAN_POINT ( 'NONE',  ( 1.692332502075646783, -2.050886281836623581, -0.2028688129896583647 ) ) ;
#932 = EDGE_CURVE ( 'NONE', #104450, #135613, #77272, .T. ) ;
#934 = CARTESIAN_POINT ( 'NONE',  ( -8.012344526598182026E-15, 13.04687500034139980, -1.575800808251669460 ) ) ;
#933 = DIRECTION ( 'NONE',  ( 0.000000000000000000, 1.000000000000000000, 0.000000000000000000 ) ) ;
#935 = CARTESIAN_POINT ( 'NONE',  ( 4.008406971134620633, 7.828225232965717595, 0.7998128361456321445 ) ) ;
#936 = VECTOR ( 'NONE', #86539, 1000.000000000000000 ) ;
#937 = CARTESIAN_POINT ( 'NONE',  ( -0.1409997244345879974, 2.021982482314553131, -2.415666835770650778 ) ) ;
#938 = CARTESIAN_POINT ( 'NONE',  ( 1.394213304513430174, 1.506067903837378097, -1.058747118707924262 ) ) ;
#939 = AXIS2_PLACEMENT_3D ( 'NONE', #116182, #182168, #33798 ) ;
#940 = CARTESIAN_POINT ( 'NONE',  ( 6.270183524512255246, 1.130759168108757873, 1.895055401287759178 ) ) ;
#941 = CARTESIAN_POINT ( 'NONE',  ( 7.062871678076271920, 7.204714810702593120, -0.7998128361456341429 ) ) ;
#942 = CARTESIAN_POINT ( 'NONE',  ( 1.845224345143604561, -1.827161268409679407, 1.154667503900350445 ) ) ;
#943 = CARTESIAN_POINT ( 'NONE',  ( -3.633221978782299910, 5.261844946711204507, -1.443375672974053447 ) ) ;
#944 = CARTESIAN_POINT ( 'NONE',  ( 2.307827663788959871, -1.164988201124015577, -1.645758576239789051 ) ) ;
#945 = CARTESIAN_POINT ( 'NONE',  ( -1.499999999999964029, 8.500000000000000000, 9.886859966642596476 ) ) ;
#946 = CARTESIAN_POINT ( 'NONE',  ( -0.02418498125556165293, 7.070485378046342362, 4.060647170728404198 ) ) ;
#947 = CARTESIAN_POINT ( 'NONE',  ( 3.159844690031233583, 6.439914444440794306, -0.7080165339683067716 ) ) ;
#948 = CARTESIAN_POINT ( 'NONE',  ( 4.205908039233514195, -1.966248567454803364, 0.1440612947745979200 ) ) ;
#949 = CARTESIAN_POINT ( 'NONE',  ( 3.010954138651841916, 0.05432569772663429358, 2.015980714967258614 ) ) ;
#951 = CARTESIAN_POINT ( 'NONE',  ( 9.151390499099949949, 12.66007743471656788, -1.082531754730543971 ) ) ;
#950 = CARTESIAN_POINT ( 'NONE',  ( 1.364683531249988535, 2.113541667008087099, 0.7879004041258500513 ) ) ;
#953 = CARTESIAN_POINT ( 'NONE',  ( -0.02244404828157658613, -0.004869073801674199918, -2.189079685368473527 ) ) ;
#952 = CARTESIAN_POINT ( 'NONE',  ( -7.283754839039664475, 9.520799950344851936, -1.599625672291263179 ) ) ;
#954 = EDGE_CURVE ( 'NONE', #82527, #56186, #181684, .T. ) ;
#955 = CARTESIAN_POINT ( 'NONE',  ( 5.512195382060368409, 2.068158883198469855, -0.09793725168850964113 ) ) ;
#956 = CARTESIAN_POINT ( 'NONE',  ( 7.494959990256193194, 7.638541498254023843, -0.7998128361456281477 ) ) ;
#957 = CARTESIAN_POINT ( 'NONE',  ( -7.874588291438845644, 8.081441182967111558, -0.7998128361456291469 ) ) ;
#958 = CARTESIAN_POINT ( 'NONE',  ( 6.539320575229233157, 0.001224430076711413356, 2.103502572931112091 ) ) ;
#959 = CARTESIAN_POINT ( 'NONE',  ( 4.851822172175670467, -1.431287984025449100, -1.425384875499214443 ) ) ;
#960 = CARTESIAN_POINT ( 'NONE',  ( -1.402160292154681736E-14, -0.5062499993171791779, 1.732050807568877637 ) ) ;
#961 = EDGE_CURVE ( 'NONE', #137116, #194727, #203846, .T. ) ;
#962 = CARTESIAN_POINT ( 'NONE',  ( 0.8310137546357538874, -1.940837517380919808, -0.6983779148895614686 ) ) ;
#963 = CARTESIAN_POINT ( 'NONE',  ( 8.920901888111997025, 10.47043562662792304, 1.082531754730549967 ) ) ;
#964 = CARTESIAN_POINT ( 'NONE',  ( 5.155843554946782703, 9.237177590738404831, -0.7998128361456481317 ) ) ;
#965 = CARTESIAN_POINT ( 'NONE',  ( 6.249382461256315580, 6.255644057745969988, -0.7998128361456481317 ) ) ;
#966 = CARTESIAN_POINT ( 'NONE',  ( -1.364683531250012516, 1.342708333674755616, 0.7879004041258379498 ) ) ;
#968 = CARTESIAN_POINT ( 'NONE',  ( 3.404766800216717737, 6.348112014766642552, 1.069586989871921467 ) ) ;
#967 = CARTESIAN_POINT ( 'NONE',  ( 4.716257332707354699, 6.595662536282280719, -1.599625672291269396 ) ) ;
#969 = CARTESIAN_POINT ( 'NONE',  ( 5.897433631820129918, 8.863794422890064695, -1.082531754730537976 ) ) ;
#971 = CARTESIAN_POINT ( 'NONE',  ( 11.33772463945037146, 12.69999999999998153, 3.599999999999999201 ) ) ;
#970 = CARTESIAN_POINT ( 'NONE',  ( 3.367796644333774569, -0.4264072692300807099, 2.128736309618290079 ) ) ;
#973 = CARTESIAN_POINT ( 'NONE',  ( 2.823586671956069605, 1.020774559177588081, -1.532180179759069283 ) ) ;
#972 = CARTESIAN_POINT ( 'NONE',  ( -3.280709984826970516, 6.771319382366015383, 0.7216878364870317197 ) ) ;
#974 = CARTESIAN_POINT ( 'NONE',  ( -1.364683531250010295, 5.238541667008086655, -0.7879004041258300672 ) ) ;
#975 = CARTESIAN_POINT ( 'NONE',  ( 3.896163805485418852, -0.6886730243073329039, -2.080591098665984795 ) ) ;
#976 = CARTESIAN_POINT ( 'NONE',  ( 3.834746474454188013E-15, 8.812500000000000000, 1.500000000000001554 ) ) ;
#977 = CARTESIAN_POINT ( 'NONE',  ( 4.768612610038791111, -1.481304060603398032, 1.710260256980479898 ) ) ;
#978 = FACE_OUTER_BOUND ( 'NONE', #59802, .T. ) ;
#979 = CARTESIAN_POINT ( 'NONE',  ( 5.819104682239041537, 7.212836251160942957, -1.171789181936284896 ) ) ;
#980 = VECTOR ( 'NONE', #108007, 1000.000000000000000 ) ;
#981 = CARTESIAN_POINT ( 'NONE',  ( -6.414416072596849538, 7.616478518518682073, -1.082531754730549967 ) ) ;
#982 = CARTESIAN_POINT ( 'NONE',  ( 3.757017964762656703, 7.397288368949487491, -1.734723475976807094E-15 ) ) ;
#983 = CARTESIAN_POINT ( 'NONE',  ( 6.678955280633751102, -0.08981333502068940267, -1.767555964166868998 ) ) ;
#984 = CARTESIAN_POINT ( 'NONE',  ( 4.266274873615797603, 2.012593780953766842, -0.05172614775082911426 ) ) ;
#985 = CARTESIAN_POINT ( 'NONE',  ( 7.416473721875251890, 8.611306416064660851, 1.199719254218462483 ) ) ;
#986 = CARTESIAN_POINT ( 'NONE',  ( 2.714012760861806317, -2.083235677042583944, 0.3076118897425133003 ) ) ;
#987 = CARTESIAN_POINT ( 'NONE',  ( 1.300237133077002394, 1.285435684207901774, -1.420472988465313557 ) ) ;
#989 = CARTESIAN_POINT ( 'NONE',  ( 4.304877467538922531, 4.981110786005563007, 1.199719254218464037 ) ) ;
#988 = CARTESIAN_POINT ( 'NONE',  ( -1.364683531250014514, 12.08854166700806765, -0.7879004041258335089 ) ) ;
#990 = B_SPLINE_CURVE_WITH_KNOTS ( 'NONE', 3,
 ( #112463, #131886, #64702, #162226, #79885, #212006 ),
 .UNSPECIFIED., .F., .F.,
 ( 4, 2, 4 ),
 ( 0.001889712630306643673, 0.002203932548491402497, 0.002518152466676161320 ),
 .UNSPECIFIED. ) ;
#991 = CARTESIAN_POINT ( 'NONE',  ( 1.803111746996020948, -1.665554870236161333, 1.050892442246372349 ) ) ;
#992 = CARTESIAN_POINT ( 'NONE',  ( 0.4087956859853311142, 1.625333209436867321, 0.9259686016569528277 ) ) ;
#993 = CARTESIAN_POINT ( 'NONE',  ( 0.5550359226569913096, 1.633180182981083028, -1.086726831054436682 ) ) ;
#995 = ORIENTED_EDGE ( 'NONE', *, *, #65741, .T. ) ;
#994 = CARTESIAN_POINT ( 'NONE',  ( -0.1054227091227821350, -1.855472971956134920, -0.4628026090111520552 ) ) ;
#996 = CARTESIAN_POINT ( 'NONE',  ( 4.528060117284222308, 8.226561203566173930, 0.7216878364870438212 ) ) ;
#997 = CARTESIAN_POINT ( 'NONE',  ( -1.402160292154681736E-14, 0.7593750003414168059, -1.575800808251659024 ) ) ;
#998 = CARTESIAN_POINT ( 'NONE',  ( 6.350466393003619814, 0.5888352225367661230, 1.775644890098279749 ) ) ;
#999 = CARTESIAN_POINT ( 'NONE',  ( 9.459838494033030898, 12.05956421450382088, 1.599625672291281386 ) ) ;
#1000 = DIRECTION ( 'NONE',  ( 1.207943261119674327E-30, 2.168404344971008079E-15, 1.000000000000000000 ) ) ;
#1001 = AXIS2_PLACEMENT_3D ( 'NONE', #80650, #164042, #112153 ) ;
#1002 = DIRECTION ( 'NONE',  ( 0.000000000000000000, 0.7999999999999973799, -0.6000000000000034195 ) ) ;
#1003 = CARTESIAN_POINT ( 'NONE',  ( 0.4146172280090759665, 0.7909515328246279342, 1.913518691844050323 ) ) ;
#1004 = CARTESIAN_POINT ( 'NONE',  ( -0.7500000000000006661, -0.1416666666666441254, -1.299038105676652011 ) ) ;
#1005 = CARTESIAN_POINT ( 'NONE',  ( 8.111855979677986994, 8.358253485912799263, 1.040834085586084257E-14 ) ) ;
#1006 = CARTESIAN_POINT ( 'NONE',  ( -8.636707547105197946, 10.03491254549959777, -1.199719254218446718 ) ) ;
#1007 = CARTESIAN_POINT ( 'NONE',  ( 5.529746549527311039, 7.544733289238903851, -1.599625672291281386 ) ) ;
#1008 = CARTESIAN_POINT ( 'NONE',  ( 3.549202351727371862, 7.362762853649070571, -0.7998128361456362523 ) ) ;
#1009 = CARTESIAN_POINT ( 'NONE',  ( -1.201851678989727383E-14, 1.321875000341419248, 1.575800808251672791 ) ) ;
#1010 = CARTESIAN_POINT ( 'NONE',  ( -0.7500000000000215383, 2.191666666666689078, 1.299038105676671107 ) ) ;
#1012 = CARTESIAN_POINT ( 'NONE',  ( 5.007038802148489509, 4.735966778795008381, 0.7998128361456341429 ) ) ;
#1011 = CARTESIAN_POINT ( 'NONE',  ( 5.793401095800717826, -1.774274828963496198, 0.8374297333502839225 ) ) ;
#1013 = CARTESIAN_POINT ( 'NONE',  ( 2.741564358335503382, -1.928455994415989139, -0.5879317209081732498 ) ) ;
#1014 = CARTESIAN_POINT ( 'NONE',  ( 3.116317603207694464, 1.870113986138211670, 0.4147879586954768549 ) ) ;
#1015 = CARTESIAN_POINT ( 'NONE',  ( -6.966220764712169000, 6.002124920821316323, -2.420000000000000373 ) ) ;
#1016 = AXIS2_PLACEMENT_3D ( 'NONE', #89451, #186921, #6019 ) ;
#1017 = CARTESIAN_POINT ( 'NONE',  ( 2.103317784989285677, -0.4765762082987561321, 2.138964651187735821 ) ) ;
#1018 = CARTESIAN_POINT ( 'NONE',  ( 0.2335667940002320309, 7.629137130509054288, -2.753349444758381281 ) ) ;
#1019 = CARTESIAN_POINT ( 'NONE',  ( 3.004993591039197831, 1.578202713744047303, 1.003818400984110681 ) ) ;
#1020 = CARTESIAN_POINT ( 'NONE',  ( 0.7499999999999867883, -0.9020833326505162120, -1.299038105676652011 ) ) ;
#1021 = CARTESIAN_POINT ( 'NONE',  ( -6.482770005628665011, 10.71498210654212002, 0.7998128361456481317 ) ) ;
#1023 = CARTESIAN_POINT ( 'NONE',  ( 4.341493734318905950, 0.4621530863439751724, -2.066033417628045932 ) ) ;
#1022 = CARTESIAN_POINT ( 'NONE',  ( -5.599154252763867134, 5.634694171087028636, 0.000000000000000000 ) ) ;
#1024 = DIRECTION ( 'NONE',  ( -1.000000000000000000, 0.000000000000000000, 0.000000000000000000 ) ) ;
#1025 = CARTESIAN_POINT ( 'NONE',  ( 6.180147188013234150, -1.146869210499700920, -1.723488058659912392 ) ) ;
#1027 = CARTESIAN_POINT ( 'NONE',  ( -5.030511086842778923, 7.205508557346677279, -1.253558018337496582 ) ) ;
#1026 = CARTESIAN_POINT ( 'NONE',  ( 2.454727380131729753, -1.820530515947630379, -1.027877103350574250 ) ) ;
#1029 = ORIENTED_EDGE ( 'NONE', *, *, #159807, .F. ) ;
#1028 = CARTESIAN_POINT ( 'NONE',  ( 1.061059408578250318, 0.3424711756105159877, -1.690240703899626107 ) ) ;
#1030 = CARTESIAN_POINT ( 'NONE',  ( 6.425674737872927089, 9.584038729905381970, -1.199719254218440723 ) ) ;
#1031 = MECHANICAL_DESIGN_GEOMETRIC_PRESENTATION_REPRESENTATION (  '', ( #101406 ), #122221 ) ;
#1032 = DIRECTION ( 'NONE',  ( -5.176899690512889973E-31, 0.6299249119529756191, -0.7766560405359864694 ) ) ;
#1033 = FACE_OUTER_BOUND ( 'NONE', #150305, .T. ) ;
#1034 = CARTESIAN_POINT ( 'NONE',  ( -10.32660017610915837, 5.019824769181640889, 7.354833152352289183 ) ) ;
#1035 = CARTESIAN_POINT ( 'NONE',  ( 5.300874872818821082, 9.128178418356554857, 0.7216878364870438212 ) ) ;
#1036 = CARTESIAN_POINT ( 'NONE',  ( -0.7500000000000179856, 9.541666666666671404, 1.299038105676658228 ) ) ;
#1037 = ADVANCED_FACE ( 'NONE', ( #178914 ), #183155, .F. ) ;
#1039 = CARTESIAN_POINT ( 'NONE',  ( 1.066738840199648042, -1.428349636637029407, 1.113955053652333493 ) ) ;
#1038 = CARTESIAN_POINT ( 'NONE',  ( 7.679767667498067496, 7.924426798361372093, 0.000000000000000000 ) ) ;
#1040 = CARTESIAN_POINT ( 'NONE',  ( -5.859094939400033120, 9.987361195942037639, -0.7998128361456231517 ) ) ;
#1041 = CARTESIAN_POINT ( 'NONE',  ( 4.813308228051395687, 5.574280006603454574, 1.199719254218462483 ) ) ;
#1042 = CARTESIAN_POINT ( 'NONE',  ( -6.466610638350029916, 6.780223854948245865, 0.3187201834274414058 ) ) ;
#1043 = CARTESIAN_POINT ( 'NONE',  ( 7.225569521440261767, 7.394528961293920233, -0.7998128361456341429 ) ) ;
#1044 = DIRECTION ( 'NONE',  ( 0.000000000000000000, 1.000000000000000000, 0.000000000000000000 ) ) ;
#1045 = LINE ( 'NONE', #164649, #45487 ) ;
#1046 = CARTESIAN_POINT ( 'NONE',  ( -11.45842088241054491, 11.09306470877032069, 3.566211699757684261 ) ) ;
#1047 = CARTESIAN_POINT ( 'NONE',  ( 8.839552966430002101, 11.33589776563360019, -1.443375672974052559 ) ) ;
#1048 = ORIENTED_EDGE ( 'NONE', *, *, #68958, .F. ) ;
#1049 = ORIENTED_EDGE ( 'NONE', *, *, #67497, .T. ) ;
#1050 = CARTESIAN_POINT ( 'NONE',  ( 2.576407586095734725, 1.218277932339612901, -1.406949740073556887 ) ) ;
#1051 = CARTESIAN_POINT ( 'NONE',  ( 0.3334082175802362547, 0.6002418569295930872, -1.819223357073847636 ) ) ;
#1052 = CARTESIAN_POINT ( 'NONE',  ( 0.4695848928168535608, -1.793611485386744420, -1.130822890709509254 ) ) ;
#1053 = CARTESIAN_POINT ( 'NONE',  ( -15.75000000000000000, 10.19999999999998153, 3.599999999999999201 ) ) ;
#1054 = FACE_OUTER_BOUND ( 'NONE', #104348, .T. ) ;
#1055 = CARTESIAN_POINT ( 'NONE',  ( 7.721398836998391246, -5.907420853759296264, 7.721398836998372595 ) ) ;
#1056 =( BOUNDED_CURVE ( )  B_SPLINE_CURVE ( 2, ( #102050, #170239, #187553, #185416, #85797, #37034, #69520 ),
 .UNSPECIFIED., .F., .T. ) 
 B_SPLINE_CURVE_WITH_KNOTS ( ( 3, 2, 2, 3 ),
 ( 0.000000000000000000, 0.005952380952380876590, 0.01190476190476175318, 0.01785714285714263064 ),
 .UNSPECIFIED. ) 
 CURVE ( )  GEOMETRIC_REPRESENTATION_ITEM ( )  RATIONAL_B_SPLINE_CURVE ( ( 1.000000000000000000, 0.8660254037844387076, 1.000000000000000000, 0.8660254037844387076, 1.000000000000000000, 0.8660254037844438146, 0.9999999999999948930 ) ) 
 REPRESENTATION_ITEM ( '' )  );
#1057 = CARTESIAN_POINT ( 'NONE',  ( -4.039966587192274083, 5.736380323189513852, 1.443375672974064550 ) ) ;
#1058 = CARTESIAN_POINT ( 'NONE',  ( 9.273413882067330860, 9.921330405274451536, -0.7216878364870257245 ) ) ;
#1059 = CARTESIAN_POINT ( 'NONE',  ( 4.698083300297758669, 0.8457734583860087030, -1.778757171186759134 ) ) ;
#1060 = CARTESIAN_POINT ( 'NONE',  ( 1.067215373428985092, -1.669322716927954753, 1.307481345630675529 ) ) ;
#1061 = CARTESIAN_POINT ( 'NONE',  ( -5.311043488251275591, 7.219303374425030562, -1.599625672291256295 ) ) ;
#1062 = CARTESIAN_POINT ( 'NONE',  ( -11.37613258624509349, 7.826217927974032484, 3.683897043248439029 ) ) ;
#1063 = CARTESIAN_POINT ( 'NONE',  ( 11.78331023100045627, 12.29999999999998295, 1.799999999999999600 ) ) ;
#1064 = CARTESIAN_POINT ( 'NONE',  ( 6.035146784841348477, -1.584849238314169240, -1.513754250258770639 ) ) ;
#1065 = CARTESIAN_POINT ( 'NONE',  ( 0.000000000000000000, -9.063431457505059186, 0.000000000000000000 ) ) ;
#1066 = CARTESIAN_POINT ( 'NONE',  ( 3.803666480526507687, -0.5600534170543782775, 1.843171563392527856 ) ) ;
#1067 = CARTESIAN_POINT ( 'NONE',  ( -5.181187258716735577, 9.196468901811520880, 0.7998128361456481317 ) ) ;
#1068 = CARTESIAN_POINT ( 'NONE',  ( -1.284279953904132077, 2.878360285806111474, -0.7749999999999935829 ) ) ;
#1069 = CARTESIAN_POINT ( 'NONE',  ( 0.9442952520863318044, 0.8911936224933308948, -2.019119535841918278 ) ) ;
#1070 = CARTESIAN_POINT ( 'NONE',  ( 5.447384925931444855, 6.422658924545643799, -1.238017914293283228 ) ) ;
#1071 = VERTEX_POINT ( 'NONE', #103 ) ;
#1072 =( BOUNDED_SURFACE ( )  B_SPLINE_SURFACE ( 3, 3, ( 
 ( #98633, #161515, #128031, #95467, #162577, #66087, #46700, #14151, #212356, #17347, #180936 ),
 ( #13097, #131196, #197184, #132230, #163643, #16279, #15224, #195062, #81314, #83429, #112817 ),
 ( #177756, #63996, #147390, #61866, #193985, #48821, #130148, #164693, #213417, #82365, #79177 ),
 ( #148454, #145293, #181989, #24, #80245, #198239, #211298, #49877, #33621, #146343, #62922 ),
 ( #47778, #99692, #129090, #178830, #30444, #113891, #54142, #20550, #137536, #171077, #168948 ),
 ( #103965, #38957, #120278, #170007, #117067, #2151, #186252, #187328, #153773, #37887, #183065 ),
 ( #203554, #68228, #85563, #34679, #201424, #102889, #67156, #71425, #3222, #21595, #118138 ) ),
 .UNSPECIFIED., .T., .F., .F. ) 
 B_SPLINE_SURFACE_WITH_KNOTS ( ( 4, 3, 4 ),
 ( 4, 1, 1, 1, 1, 1, 1, 1, 4 ),
 ( 0.000000000000000000, 0.5000000000000000000, 1.000000000000000000 ),
 ( 0.000000000000000000, 0.2256085737580844630, 0.3975982043691296264, 0.5251069566405043298, 0.6172860083021659561, 0.6832860984239963464, 0.7321959383537668398, 0.7728624839797392232, 1.000000000000000000 ),
 .UNSPECIFIED. ) 
 GEOMETRIC_REPRESENTATION_ITEM ( )  RATIONAL_B_SPLINE_SURFACE ( (
 ( 1.000000000000000222, 1.000000000000000222, 1.000000000000000444, 0.9999999999999996669, 1.000000000000000444, 0.9999999999999997780, 1.000000000000000222, 1.000000000000000222, 0.9999999999999996669, 1.000000000000000000, 1.000000000000000000),
 ( 0.3333333333333334259, 0.3333333333333334259, 0.3333333333333334259, 0.3333333333333333703, 0.3333333333333334259, 0.3333333333333333148, 0.3333333333333334814, 0.3333333333333334259, 0.3333333333333331483, 0.3333333333333334259, 0.3333333333333333703),
 ( 0.3333333333333334259, 0.3333333333333334259, 0.3333333333333334259, 0.3333333333333333703, 0.3333333333333334259, 0.3333333333333333148, 0.3333333333333334814, 0.3333333333333334259, 0.3333333333333331483, 0.3333333333333334259, 0.3333333333333333703),
 ( 1.000000000000000222, 1.000000000000000222, 1.000000000000000444, 0.9999999999999996669, 1.000000000000000444, 0.9999999999999997780, 1.000000000000000222, 1.000000000000000222, 0.9999999999999996669, 1.000000000000000000, 1.000000000000000000),
 ( 0.3333333333333334259, 0.3333333333333334259, 0.3333333333333334259, 0.3333333333333333703, 0.3333333333333334259, 0.3333333333333333148, 0.3333333333333334814, 0.3333333333333334259, 0.3333333333333331483, 0.3333333333333334259, 0.3333333333333333703),
 ( 0.3333333333333334259, 0.3333333333333334259, 0.3333333333333334259, 0.3333333333333333703, 0.3333333333333334259, 0.3333333333333333148, 0.3333333333333334814, 0.3333333333333334259, 0.3333333333333331483, 0.3333333333333334259, 0.3333333333333333703),
 ( 1.000000000000000222, 1.000000000000000222, 1.000000000000000444, 0.9999999999999996669, 1.000000000000000444, 0.9999999999999997780, 1.000000000000000222, 1.000000000000000222, 0.9999999999999996669, 1.000000000000000000, 1.000000000000000000) ) ) 
 REPRESENTATION_ITEM ( '' )  SURFACE ( )  );
#1073 = ORIENTED_EDGE ( 'NONE', *, *, #78717, .T. ) ;
#1074 = CARTESIAN_POINT ( 'NONE',  ( 6.543809977506837683, 1.355650292293397507, 1.428865145875155340 ) ) ;
#1075 = CARTESIAN_POINT ( 'NONE',  ( 1.505311199525250831, -1.927169978453403321, 0.2396651170105366657 ) ) ;
#1076 = CARTESIAN_POINT ( 'NONE',  ( 6.766976407292540685, -2.298085592349991213, 0.04593636341931536110 ) ) ;
#1078 = CARTESIAN_POINT ( 'NONE',  ( 4.381604285809827637, -1.781765127997904763, 0.5371461504297748712 ) ) ;
#1077 = CARTESIAN_POINT ( 'NONE',  ( -6.794571259104023930, 7.956029886156682274, 1.199719254218452047 ) ) ;
#1079 = CARTESIAN_POINT ( 'NONE',  ( 7.686546744304875389, 7.932335721302671949, 0.7998128361456291469 ) ) ;
#1080 = CARTESIAN_POINT ( 'NONE',  ( 9.000007961041747606, 1.000000000000000888, 7.937244906211794238 ) ) ;
#1081 = CARTESIAN_POINT ( 'NONE',  ( 11.89942855770813956, 12.22000000000000064, 0.6999999999999992895 ) ) ;
#1082 = CARTESIAN_POINT ( 'NONE',  ( -5.473741331615264549, 7.409117525016355010, -1.599625672291256295 ) ) ;
#1083 = CARTESIAN_POINT ( 'NONE',  ( -3.277990255609289694, -0.8976961690679158279, 0.3594898028441471105 ) ) ;
#1084 = CARTESIAN_POINT ( 'NONE',  ( 0.6092356648998223934, -0.3158941238240610128, 2.168550393043596536 ) ) ;
#1085 = CARTESIAN_POINT ( 'NONE',  ( 4.365362273920244007, 6.116008624372160973, 1.443375672974062551 ) ) ;
#1086 = EDGE_CURVE ( 'NONE', #188607, #206477, #202400, .T. ) ;
#1087 = CARTESIAN_POINT ( 'NONE',  ( 0.000000000000000000, 4.000000000000003553, 0.000000000000000000 ) ) ;
#1089 =( BOUNDED_CURVE ( )  B_SPLINE_CURVE ( 3, ( #195966, #64881, #99529, #165589 ),
 .UNSPECIFIED., .F., .T. ) 
 B_SPLINE_CURVE_WITH_KNOTS ( ( 4, 4 ),
 ( 0.4999999999999963918, 1.000000000000000000 ),
 .UNSPECIFIED. ) 
 CURVE ( )  GEOMETRIC_REPRESENTATION_ITEM ( )  RATIONAL_B_SPLINE_CURVE ( ( 1.000000000000004663, 0.3333333333333333703, 0.3333333333333285409, 1.000000000000000000 ) ) 
 REPRESENTATION_ITEM ( '' )  );
#1088 = CARTESIAN_POINT ( 'NONE',  ( -3.563261906135796409, 6.332667919118538435, 2.500000000000011102 ) ) ;
#1090 = CARTESIAN_POINT ( 'NONE',  ( 1.717148762710469789, -0.2249250470785572054, 1.811706739299999924 ) ) ;
#1091 = CARTESIAN_POINT ( 'NONE',  ( -3.598799709423620374, 6.286017863381107240, 1.199719254218464037 ) ) ;
#1092 = VECTOR ( 'NONE', #206274, 1000.000000000000000 ) ;
#1093 = CARTESIAN_POINT ( 'NONE',  ( 4.113671241589770489, 0.09026135180613574505, 1.731944212183807341 ) ) ;
#1094 = CARTESIAN_POINT ( 'NONE',  ( 0.001041342783940506700, 2.586899276670884262, -2.002406093249768926 ) ) ;
#1095 = CARTESIAN_POINT ( 'NONE',  ( -1.975475456537005874E-15, 2.812500000000000888, 1.224999999999953904 ) ) ;
#1096 = CARTESIAN_POINT ( 'NONE',  ( 0.1331565106231571705, 2.881392620029461504, -2.434650611646618223 ) ) ;
#1097 = CIRCLE ( 'NONE', #56491, 11.92000000000000171 ) ;
#1098 = CARTESIAN_POINT ( 'NONE',  ( 0.2934164811014350893, 1.426665091747752356, 1.294802382297273180 ) ) ;
#1099 = CARTESIAN_POINT ( 'NONE',  ( 4.135565103414404753, 1.848670044762780407, -0.6568835154602686854 ) ) ;
#1100 = EDGE_CURVE ( 'NONE', #39859, #170847, #133352, .T. ) ;
#1101 = CARTESIAN_POINT ( 'NONE',  ( -8.688077508258798431, 9.030511935923748013, -0.7998128361456291469 ) ) ;
#1102 = CARTESIAN_POINT ( 'NONE',  ( 5.124091990960999432, 8.065525525174782828, -1.199719254218452047 ) ) ;
#1103 = CARTESIAN_POINT ( 'NONE',  ( 5.180389117862056914, 1.045492054797515946, 1.844774357600783121 ) ) ;
#1104 = CARTESIAN_POINT ( 'NONE',  ( 5.643937085038755797, 9.806620042512378177, -0.7998128361456481317 ) ) ;
#1105 = CARTESIAN_POINT ( 'NONE',  ( -7.472515219426274946, 11.86968485597268064, 0.000000000000000000 ) ) ;
#1106 = CARTESIAN_POINT ( 'NONE',  ( 4.310602774141044868, 7.116454772218158809, -1.199719254218452047 ) ) ;
#1107 = CARTESIAN_POINT ( 'NONE',  ( 3.397389602098393802, -1.828008730618407851, 0.9717071122367711977 ) ) ;
#1109 = CARTESIAN_POINT ( 'NONE',  ( -1.402160292154681736E-14, 0.5093750003414236893, -1.575800808251659024 ) ) ;
#1108 = SURFACE_SIDE_STYLE ('',( #195073 ) ) ;
#1110 = VERTEX_POINT ( 'NONE', #18511 ) ;
#1111 = CARTESIAN_POINT ( 'NONE',  ( 3.446149177467156655, -2.027825264502993718, -1.082511230532481106 ) ) ;
#1112 = CARTESIAN_POINT ( 'NONE',  ( 8.771762198361678031, 9.336070107617867819, 1.040834085586084257E-14 ) ) ;
#1114 = CARTESIAN_POINT ( 'NONE',  ( -1.642778471875000035, -3.317708332855374476, -2.845375778867859751 ) ) ;
#1113 = CARTESIAN_POINT ( 'NONE',  ( 6.129694847154206983, 8.244672969803623630, -1.443375672974078761 ) ) ;
#1115 = DIRECTION ( 'NONE',  ( 0.000000000000000000, 1.000000000000000000, 0.000000000000000000 ) ) ;
#1116 = CARTESIAN_POINT ( 'NONE',  ( 0.000000000000000000, 12.22000000000000064, 0.000000000000000000 ) ) ;
#1117 = VERTEX_POINT ( 'NONE', #82446 ) ;
#1118 = CARTESIAN_POINT ( 'NONE',  ( -5.204170427930421283E-15, -5.907420853759282053, 10.91970695577496997 ) ) ;
#1119 = CARTESIAN_POINT ( 'NONE',  ( 3.761887187967042134, 0.6396200178584460216, -1.802413552503052463 ) ) ;
#1120 = CARTESIAN_POINT ( 'NONE',  ( -0.08058608058609216529, -9.999999999999994671, -10.99970480893080271 ) ) ;
#1121 = CARTESIAN_POINT ( 'NONE',  ( 5.297747862459361912, -0.6177129893134482019, 1.610538751920454592 ) ) ;
#1122 = CARTESIAN_POINT ( 'NONE',  ( 3.362517798112668821, -1.944730434982215650, -0.5331690889110105580 ) ) ;
#1123 = CARTESIAN_POINT ( 'NONE',  ( 5.537770794106480210, -1.814135573521371780, 1.411581493584870728 ) ) ;
#1124 = CARTESIAN_POINT ( 'NONE',  ( 11.55950211276791251, 11.37999999999998302, 3.221476510067114329 ) ) ;
#1125 = CARTESIAN_POINT ( 'NONE',  ( 1.260703874955213744, 0.8971468365699288849, 2.016480257658866737 ) ) ;
#1126 = CARTESIAN_POINT ( 'NONE',  ( -4.258669648468323743, 6.061810238003387141, 1.443375672974065660 ) ) ;
#1127 = CARTESIAN_POINT ( 'NONE',  ( 5.852768638770064591, -1.394116391329143667, 1.090054309861036241 ) ) ;
#1129 = CARTESIAN_POINT ( 'NONE',  ( 1.728911070687192186, 0.2280534122649588435, 2.280891765651926750 ) ) ;
#1128 = CARTESIAN_POINT ( 'NONE',  ( 6.384963997392946844, 6.413822516572072807, 0.7998128361456352531 ) ) ;
#1130 = CARTESIAN_POINT ( 'NONE',  ( 0.04040834310030903126, -1.341606091951352164, -1.108378290077848494 ) ) ;
#1131 = CARTESIAN_POINT ( 'NONE',  ( -3.297657676621885692, 4.870353260857385180, 1.599625672291267398 ) ) ;
#1132 = CARTESIAN_POINT ( 'NONE',  ( 11.86239285000045918, 11.37999999999999901, -1.812080536912753059 ) ) ;
#1133 = CARTESIAN_POINT ( 'NONE',  ( -5.191846479390389568, 5.021852078902356631, 0.7998128361456281477 ) ) ;
#1134 = CYLINDRICAL_SURFACE ( 'NONE', #80203, 1.500000000000000222 ) ;
#1135 = CARTESIAN_POINT ( 'NONE',  ( 6.707487347292075519, -1.660346423639452951, -1.236579608897829363 ) ) ;
#1136 = CARTESIAN_POINT ( 'NONE',  ( 1.305875433988498813, -1.124247956386617009, -1.673852571057245830 ) ) ;
#1137 =( BOUNDED_CURVE ( )  B_SPLINE_CURVE ( 2, ( #18392, #113862, #32530, #15194, #48792, #82334, #130120 ),
 .UNSPECIFIED., .F., .T. ) 
 B_SPLINE_CURVE_WITH_KNOTS ( ( 3, 2, 2, 3 ),
 ( 0.3749999999999998890, 0.3833333333333333592, 0.3916666666666668295, 0.4000000000000002998 ),
 .UNSPECIFIED. ) 
 CURVE ( )  GEOMETRIC_REPRESENTATION_ITEM ( )  RATIONAL_B_SPLINE_CURVE ( ( 1.000000000000001776, 0.8660254037844369313, 1.000000000000000000, 0.8660254037844387076, 1.000000000000000000, 0.8660254037844342667, 1.000000000000004441 ) ) 
 REPRESENTATION_ITEM ( '' )  );
#1138 = CARTESIAN_POINT ( 'NONE',  ( -1.402160292154681736E-14, -0.2562499993171780122, 1.732050807568877637 ) ) ;
#1139 = CARTESIAN_POINT ( 'NONE',  ( 5.197847267195914611, -0.6914886683457229788, 1.798296804713859220 ) ) ;
#1140 = CARTESIAN_POINT ( 'NONE',  ( -0.6823417656250003738, 11.40104166700806765, 1.181850606188754593 ) ) ;
#1141 = CARTESIAN_POINT ( 'NONE',  ( 1.863841412593499003, -1.787636906239049805, -1.318573911375673369 ) ) ;
#1142 = VERTEX_POINT ( 'NONE', #84590 ) ;
#1144 = CARTESIAN_POINT ( 'NONE',  ( -1.270904146967337889, 3.209693569853256268, 0.7750000000000083489 ) ) ;
#1143 = CARTESIAN_POINT ( 'NONE',  ( -1.500000000000001110, 5.379166666666693075, -0.8660254037844372643 ) ) ;
#1145 = CARTESIAN_POINT ( 'NONE',  ( 6.902720183911290164, 14.55305236562705318, -9.761920501353818835 ) ) ;
#1146 = CARTESIAN_POINT ( 'NONE',  ( 8.269583629331492602, 11.73526576994040482, 1.199719254218450271 ) ) ;
#1147 = DIRECTION ( 'NONE',  ( 0.000000000000000000, 0.000000000000000000, 1.000000000000000000 ) ) ;
#1148 = CARTESIAN_POINT ( 'NONE',  ( 3.948569229637605815, -1.449640539659799776, -0.9628182713226125511 ) ) ;
#1149 = CARTESIAN_POINT ( 'NONE',  ( 2.611707774152134842, 0.5260268489151799232, -1.889944157703125072 ) ) ;
#1151 = CARTESIAN_POINT ( 'NONE',  ( -5.558479791922849245, 9.428717490644563881, 0.7216878364870458196 ) ) ;
#1150 = CARTESIAN_POINT ( 'NONE',  ( 3.662674053986138656, 7.424870162959149589, 0.7998128361456321445 ) ) ;
#1152 = CARTESIAN_POINT ( 'NONE',  ( -5.907986510169434879, 6.002582827494773454, 0.1128355114666315662 ) ) ;
#1153 = CARTESIAN_POINT ( 'NONE',  ( 10.56588178375152864, 11.22128359066528169, -0.7998128361456281477 ) ) ;
#1154 = CIRCLE ( 'NONE', #42813, 0.07999999999999994615 ) ;
#1155 = CARTESIAN_POINT ( 'NONE',  ( 0.6255240776356413290, 0.2040786869749251498, -2.052575575099666150 ) ) ;
#1156 = CARTESIAN_POINT ( 'NONE',  ( -6.995117189646935962, 10.24838825697502109, 1.199719254218453823 ) ) ;
#1157 = CARTESIAN_POINT ( 'NONE',  ( -3.090895833791289071, 6.549869539491048442, 1.040834085586084257E-14 ) ) ;
#1158 = CARTESIAN_POINT ( 'NONE',  ( 1.516897200560879178, 1.518302048914378588, -1.677564506150258206 ) ) ;
#1159 = ORIENTED_EDGE ( 'NONE', *, *, #134668, .F. ) ;
#1160 = CARTESIAN_POINT ( 'NONE',  ( 1.499999999999987121, 0.03541666734948738238, 0.8660254037844524744 ) ) ;
#1161 = CARTESIAN_POINT ( 'NONE',  ( 2.442468673064964957, 0.4055347385497136137, 1.825902681341363021 ) ) ;
#1162 = CARTESIAN_POINT ( 'NONE',  ( 1.177864744846460754, 1.312336027064511690, 1.133722492108141244 ) ) ;
#1163 = CARTESIAN_POINT ( 'NONE',  ( 5.214472588068230330, 2.024700573814151028, 0.8392323156421463981 ) ) ;
#1164 = CARTESIAN_POINT ( 'NONE',  ( 5.438606028847273066, 2.272309368472532398, 0.4011960609803484901 ) ) ;
#1165 = CARTESIAN_POINT ( 'NONE',  ( 0.9013288230189763217, 1.684346374898238352, 1.187240197102001904 ) ) ;
#1166 = CARTESIAN_POINT ( 'NONE',  ( 3.503789773231671845, -0.7878879028691202491, -1.775113385239434072 ) ) ;
#1167 = CARTESIAN_POINT ( 'NONE',  ( -4.568734577680887199, 6.353276312092901890, -1.443375672974051449 ) ) ;
#1168 = CARTESIAN_POINT ( 'NONE',  ( 6.169203917683822702, 0.1378038699498609632, -1.865550841118966297 ) ) ;
#1169 = CARTESIAN_POINT ( 'NONE',  ( 1.468750000000000888, 0.7852924748299092705, -1.895863743164120097 ) ) ;
#1170 = CARTESIAN_POINT ( 'NONE',  ( 4.010558181858147719, 7.580895019428740333, -0.2605091080661054437 ) ) ;
#1171 = CARTESIAN_POINT ( 'NONE',  ( 0.4734851067992265627, 1.504414441068102404, 0.8618086654073161545 ) ) ;
#1172 = ADVANCED_FACE ( 'NONE', ( #46789 ), #131277, .T. ) ;
#1173 = CARTESIAN_POINT ( 'NONE',  ( 0.6801582343749831283, 1.223958333674737720, 1.178068619123822547 ) ) ;
#1175 = CARTESIAN_POINT ( 'NONE',  ( 4.729138786257041538, 2.011204126674607462, 0.1455352507326590494 ) ) ;
#1174 = AXIS2_PLACEMENT_3D ( 'NONE', #114767, #111570, #194880 ) ;
#1176 = CARTESIAN_POINT ( 'NONE',  ( -4.243338890952904841, 5.973648010910253880, -1.443375672974051449 ) ) ;
#1177 = CARTESIAN_POINT ( 'NONE',  ( 8.127223016387999266, 11.56917838817298616, 1.199719254218460707 ) ) ;
#1178 = CARTESIAN_POINT ( 'NONE',  ( 3.217027588192558074, 6.975225629525113824, -1.734723475976807094E-15 ) ) ;
#1179 = CARTESIAN_POINT ( 'NONE',  ( 2.156629195875509719, -1.411784796728832392, 1.157573153174975111 ) ) ;
#1180 = CARTESIAN_POINT ( 'NONE',  ( -5.472651281771599763, 6.413789912602166687, 1.199719254218452935 ) ) ;
#1181 = CARTESIAN_POINT ( 'NONE',  ( 0.07999999999999327094, -8.407420853759283830, 10.91970695577496286 ) ) ;
#1182 = CARTESIAN_POINT ( 'NONE',  ( -0.6125000000000383471, 1.854166667349464781, 1.060881119635894487 ) ) ;
#1183 = EDGE_LOOP ( 'NONE', ( #24674, #45547, #19701, #34320, #64094 ) ) ;
#1184 = CARTESIAN_POINT ( 'NONE',  ( -6.251718229232857915, 7.426664367927358512, -1.082531754730549967 ) ) ;
#1185 = CARTESIAN_POINT ( 'NONE',  ( -2.252626078164912560, 5.779814191167667481, 0.7998128361456341429 ) ) ;
#1186 = CARTESIAN_POINT ( 'NONE',  ( -7.458957065812611198, 11.85386701009007204, 0.7998128361456481317 ) ) ;
#1187 = CARTESIAN_POINT ( 'NONE',  ( 6.481118763745143063, -1.847444428138062422, -0.8165197575118980922 ) ) ;
#1188 = CARTESIAN_POINT ( 'NONE',  ( 6.621772978582266767, -0.4938884631311352691, 2.173981893038397839 ) ) ;
#1189 = CARTESIAN_POINT ( 'NONE',  ( -6.505933609711270549, 8.683618192786854095, -1.599625672291271394 ) ) ;
#1190 = CARTESIAN_POINT ( 'NONE',  ( 5.626797444871351139, 6.523350759560078593, 1.199719254218462483 ) ) ;
#1191 = CARTESIAN_POINT ( 'NONE',  ( 5.858293207932864455, 0.8329246649354884457, 1.885258002110825615 ) ) ;
#1192 = CARTESIAN_POINT ( 'NONE',  ( 5.502577337681268332, -1.966645332631598908, 0.4444998760482973821 ) ) ;
#1193 = EDGE_LOOP ( 'NONE', ( #146802, #196436, #20921, #16035 ) ) ;
#1194 = ORIENTED_EDGE ( 'NONE', *, *, #33879, .F. ) ;
#1195 = CARTESIAN_POINT ( 'NONE',  ( -1.284279953904156280, 2.921639714193936754, 0.7750000000000117906 ) ) ;
#1196 = CARTESIAN_POINT ( 'NONE',  ( -0.2108831679770946654, 7.629137130509072939, -2.497154329497498715 ) ) ;
#1199 = VERTEX_POINT ( 'NONE', #148536 ) ;
#1198 = DIRECTION ( 'NONE',  ( 0.000000000000000000, 8.546850786086437571E-32, 1.000000000000000000 ) ) ;
#1197 = CARTESIAN_POINT ( 'NONE',  ( -6.200875153403786477, 8.327716660428123419, -1.599625672291271394 ) ) ;
#1200 = CARTESIAN_POINT ( 'NONE',  ( 5.098657496608274720, 7.938328561423579011, 1.202842226815619142 ) ) ;
#1201 = CARTESIAN_POINT ( 'NONE',  ( 5.448592227559037049, 1.351948914259465173, 1.495821383734573073 ) ) ;
#1202 = CARTESIAN_POINT ( 'NONE',  ( 4.663899394030392997, -1.200468288914667614, 1.396033019000951336 ) ) ;
#1203 = CARTESIAN_POINT ( 'NONE',  ( -0.02319159430947541692, 2.051704324979522820, -2.228571760951563618 ) ) ;
#1204 = CARTESIAN_POINT ( 'NONE',  ( 3.405163318333865874, 1.819529416799025912, -1.419322092190724138 ) ) ;
#1205 = CARTESIAN_POINT ( 'NONE',  ( 5.345657705538078730, 9.458627433094950021, 0.7998128361456331437 ) ) ;
#1206 = CARTESIAN_POINT ( 'NONE',  ( 5.237646302014136168, -1.524508687941978469, -1.532700278705993790 ) ) ;
#1207 = CARTESIAN_POINT ( 'NONE',  ( 8.633844893804129228, 8.967240552393299424, -0.7998128361456211532 ) ) ;
#1208 = CARTESIAN_POINT ( 'NONE',  ( 0.1693407553623625106, 1.118952433510589817, 1.587118285914286941 ) ) ;
#1209 = CARTESIAN_POINT ( 'NONE',  ( -3.438964519360665051, 7.163875705896082913, -0.7998128361456281477 ) ) ;
#1210 = CARTESIAN_POINT ( 'NONE',  ( 4.025041230705061146, 2.281562605710918845, -0.2770438755856743929 ) ) ;
#1211 = DIRECTION ( 'NONE',  ( 0.000000000000000000, 0.000000000000000000, 1.000000000000000000 ) ) ;
#1212 = CARTESIAN_POINT ( 'NONE',  ( -3.983063267364693960, 7.868933921892603323, -0.7998128361456481317 ) ) ;
#1213 = CARTESIAN_POINT ( 'NONE',  ( 3.432352559540859271, 1.824792983844251371, 0.4109263881779609551 ) ) ;
#1216 = CARTESIAN_POINT ( 'NONE',  ( -5.749539660647037032, 8.865490816466966351, 1.199719254218454489 ) ) ;
#1215 = CARTESIAN_POINT ( 'NONE',  ( -1.402160292154681736E-14, -1.256249999317182953, 1.732050807568877637 ) ) ;
#1214 = CARTESIAN_POINT ( 'NONE',  ( 0.9844543725016400293, -1.211084316286781037, 1.480072698922259455 ) ) ;
#1217 = CARTESIAN_POINT ( 'NONE',  ( 2.912931060594741162, 1.598032330669514778, -1.522282275181946032 ) ) ;
#1218 = EDGE_CURVE ( 'NONE', #40908, #89432, #43359, .T. ) ;
#1219 = CARTESIAN_POINT ( 'NONE',  ( 4.856179778084614540, 5.010200168423447842, 0.6077543439236311462 ) ) ;
#1220 = CARTESIAN_POINT ( 'NONE',  ( 4.976006071415387311, 5.764094157194782575, 1.199719254218462483 ) ) ;
#1221 = CYLINDRICAL_SURFACE ( 'NONE', #40355, 1.500000000000000222 ) ;
#1222 = CARTESIAN_POINT ( 'NONE',  ( -4.810445574750349174, 4.506608013497163334, 0.7998128361456341429 ) ) ;
#1223 = CARTESIAN_POINT ( 'NONE',  ( -7.878696662872776812, 8.364436659539265406, -0.7216878364870338292 ) ) ;
#1224 = CARTESIAN_POINT ( 'NONE',  ( 0.3331948752925878998, -1.804169345717737238, 0.7948754592718260126 ) ) ;
#1225 = CARTESIAN_POINT ( 'NONE',  ( 0.08353690965077953390, -0.1615750995121113531, -2.271551823106517709 ) ) ;
#1226 = CARTESIAN_POINT ( 'NONE',  ( 1.662477996687723669, -0.7030478115006146833, -1.831755296705489977 ) ) ;
#1227 = CARTESIAN_POINT ( 'NONE',  ( 4.487212223095434105, 0.09620561770018636050, 2.060423205476647812 ) ) ;
#1228 = CARTESIAN_POINT ( 'NONE',  ( 4.365362273920230685, 8.036747052974847705, 0.7216878364870298324 ) ) ;
#1229 = CARTESIAN_POINT ( 'NONE',  ( 6.717138760927786834, 6.801359740696030443, -0.7998128361456481317 ) ) ;
#1230 = ORIENTED_EDGE ( 'NONE', *, *, #175281, .T. ) ;
#1231 = CARTESIAN_POINT ( 'NONE',  ( 7.659993601596707613, 9.959745173328078849, -1.443375672974058777 ) ) ;
#1232 = CARTESIAN_POINT ( 'NONE',  ( 0.6823417656249917140, 4.405208333674755394, 1.181850606188765695 ) ) ;
#1233 = CARTESIAN_POINT ( 'NONE',  ( -10.89183333199790482, 4.909323612238607915, -5.036858318171161919 ) ) ;
#1234 = CARTESIAN_POINT ( 'NONE',  ( 3.131570294632282092, 5.636953862837537521, -1.082531754730543971 ) ) ;
#1235 = CARTESIAN_POINT ( 'NONE',  ( 6.877413710614480813, -0.1567828624706164298, 2.136824976188213654 ) ) ;
#1237 = CARTESIAN_POINT ( 'NONE',  ( 6.567912610837368881, -1.126952994821692533, 1.456688911285822119 ) ) ;
#1236 = CARTESIAN_POINT ( 'NONE',  ( 9.606148981167590861, -6.583980363595129504, -0.4355862708379804604 ) ) ;
#1238 = EDGE_CURVE ( 'NONE', #81519, #74569, #198321, .T. ) ;
#1239 = CARTESIAN_POINT ( 'NONE',  ( -2.467126471220350226, 3.603011019375347068, 11.63837686854861886 ) ) ;
#1240 = LINE ( 'NONE', #117214, #18483 ) ;
#1241 = CARTESIAN_POINT ( 'NONE',  ( 1.475632603725419267, 1.109822327618605442, 1.505604422130282449 ) ) ;
#1242 = CARTESIAN_POINT ( 'NONE',  ( -6.137326611691442224, 5.996379759157309586, -0.05818935505210766357 ) ) ;
#1243 = CARTESIAN_POINT ( 'NONE',  ( 5.763319317650291040, 7.363698819737331647, -1.304181885133362195 ) ) ;
#1244 = CARTESIAN_POINT ( 'NONE',  ( -1.364683531250010295, 5.342708333674750953, 0.7879004041258379498 ) ) ;
#1245 = CARTESIAN_POINT ( 'NONE',  ( 0.6977377480232997975, 1.284608138224270002, 1.416691289136004395 ) ) ;
#1246 = PRESENTATION_LAYER_ASSIGNMENT (  '', '', ( #94684 ) ) ;
#1247 = CARTESIAN_POINT ( 'NONE',  ( 2.957584522866180343, 1.761491525812574510, -0.1715649573520404425 ) ) ;
#1248 = CARTESIAN_POINT ( 'NONE',  ( 1.031728963041964153, -1.865498905729731316, 0.4196304693004496156 ) ) ;
#1249 =( GEOMETRIC_REPRESENTATION_CONTEXT ( 3 ) GLOBAL_UNCERTAINTY_ASSIGNED_CONTEXT ( ( #40635 ) ) GLOBAL_UNIT_ASSIGNED_CONTEXT ( ( #90258, #110825, #176833 ) ) REPRESENTATION_CONTEXT ( 'NONE', 'WORKASPACE' ) );
#1251 = CARTESIAN_POINT ( 'NONE',  ( 4.235878408818731344, 1.915113449751761010, -0.05082400106456300831 ) ) ;
#1250 = CARTESIAN_POINT ( 'NONE',  ( 2.691539545140940959, -3.171237134043524808, -1.997224515217858487 ) ) ;
#1252 = CARTESIAN_POINT ( 'NONE',  ( -0.7500000000000249800, -1.058333333333314030, 1.299038105676659116 ) ) ;
#1253 = CARTESIAN_POINT ( 'NONE',  ( 5.107841235723004303, 0.6198312778436664283, -1.869525964861347589 ) ) ;
#1254 = CARTESIAN_POINT ( 'NONE',  ( 1.002369745560643510, -0.9483682245385971488, 1.896766750748935415 ) ) ;
#1255 = DIRECTION ( 'NONE',  ( 0.000000000000000000, 0.000000000000000000, -1.000000000000000000 ) ) ;
#1256 = CARTESIAN_POINT ( 'NONE',  ( 3.449935675575486638, 1.870836310073907827, 0.001118452434160921221 ) ) ;
#1258 = ORIENTED_EDGE ( 'NONE', *, *, #48325, .T. ) ;
#1257 = CARTESIAN_POINT ( 'NONE',  ( 1.101864800459760207, -1.825872481749410525, -0.002338443969775172437 ) ) ;
#1260 = CARTESIAN_POINT ( 'NONE',  ( -1.777638883463123598, -0.9165151389911724289, 1.199999999999999734 ) ) ;
#1259 = CARTESIAN_POINT ( 'NONE',  ( 3.985166894971280183, -0.2153072539897090687, -2.196357064762343825 ) ) ;
#1261 = CARTESIAN_POINT ( 'NONE',  ( 1.364683531249990311, 4.446875000341417028, 1.214306433183764966E-14 ) ) ;
#1262 = CARTESIAN_POINT ( 'NONE',  ( 2.383324636069758640, -0.002395321609373335381, 2.062851379284504461 ) ) ;
#1263 = CARTESIAN_POINT ( 'NONE',  ( 6.100279051144945619, 9.204410428722734849, -1.199719254218440723 ) ) ;
#1264 = CARTESIAN_POINT ( 'NONE',  ( -7.991641480251377772, 11.41099992934688956, 1.199719254218453823 ) ) ;
#1265 = CARTESIAN_POINT ( 'NONE',  ( -1.785627835867960034, 15.44799008577503585, -11.82984269095817353 ) ) ;
#1266 = CARTESIAN_POINT ( 'NONE',  ( 11.78331023100045627, 11.29999999999999893, -1.800000000000001155 ) ) ;
#1267 = ADVANCED_FACE ( 'NONE', ( #96609 ), #117015, .T. ) ;
#1268 = CIRCLE ( 'NONE', #122445, 12.00000000000000178 ) ;
#1269 = DIRECTION ( 'NONE',  ( -3.491481338843133750E-15, -0.000000000000000000, -1.000000000000000000 ) ) ;
#1270 = ORIENTED_EDGE ( 'NONE', *, *, #25737, .T. ) ;
#1271 = CARTESIAN_POINT ( 'NONE',  ( 4.738769824615551407, -2.007376682328159134, -0.5062664373569197851 ) ) ;
#1272 = CARTESIAN_POINT ( 'NONE',  ( -1.500000000000011324, 4.420833333333352044, 0.8660254037844403729 ) ) ;
#1273 = CARTESIAN_POINT ( 'NONE',  ( 1.563986776035675819, 2.129895014553784272, -0.3678597298803277793 ) ) ;
#1274 = CARTESIAN_POINT ( 'NONE',  ( -5.386282318077409315, 7.574627448853999745, -1.244059264865501557 ) ) ;
#1275 = CARTESIAN_POINT ( 'NONE',  ( 2.033858944562048965, -1.958440182618191416, 0.4929867953931149627 ) ) ;
#1276 = CARTESIAN_POINT ( 'NONE',  ( -3.285556943750000070, -0.1112512837626866702, -0.04025571921194345121 ) ) ;
#1278 = CARTESIAN_POINT ( 'NONE',  ( 8.514157279702022407, 10.95626946445095307, -1.443375672974063439 ) ) ;
#1277 = CARTESIAN_POINT ( 'NONE',  ( 3.475000000000000533, -3.645833333333333037, -2.006292185433951047 ) ) ;
#1279 = CARTESIAN_POINT ( 'NONE',  ( 6.380232485702068246, -0.2495653932444163448, 2.000551205290925783 ) ) ;
#1280 = CARTESIAN_POINT ( 'NONE',  ( -0.04763828917917976857, -1.313539345393003321, 1.530161206715647149 ) ) ;
#1281 = CARTESIAN_POINT ( 'NONE',  ( 6.639320575229256782, 2.033582276073117701, 2.408309898857839304 ) ) ;
#1282 = CARTESIAN_POINT ( 'NONE',  ( 4.792620198997869174, 1.822056328612733145, -1.217503271791681163 ) ) ;
#1283 = CARTESIAN_POINT ( 'NONE',  ( 1.499999999999987121, 3.327083334016150751, -0.8660254037844262731 ) ) ;
#1284 = CARTESIAN_POINT ( 'NONE',  ( 3.902528505893249733, -1.892296425594198750, -0.2755589300712790735 ) ) ;
#1285 = CARTESIAN_POINT ( 'NONE',  ( -5.576481253922474401, 5.400316305864651056, -0.7998128361456221525 ) ) ;
#1286 = CARTESIAN_POINT ( 'NONE',  ( 4.378920427089557421, 5.171457255435017331, -1.082531754730548412 ) ) ;
#1288 = CARTESIAN_POINT ( 'NONE',  ( 1.722280025409760329, 1.994874335020242695, 0.2930476355553628953 ) ) ;
#1287 = CARTESIAN_POINT ( 'NONE',  ( -1.420000000000001039, 6.280000000000042881, -2.899999999999995470 ) ) ;
#1289 = CARTESIAN_POINT ( 'NONE',  ( -8.012344526598182026E-15, 11.85937500034140157, -1.575800808251669460 ) ) ;
#1291 = CARTESIAN_POINT ( 'NONE',  ( -4.980641328173854632, 6.904110530993182948, 1.599625672291263179 ) ) ;
#1290 = CARTESIAN_POINT ( 'NONE',  ( 0.2227793574855509162, 2.196107815404338748, 0.6574155683778097892 ) ) ;
#1292 = CARTESIAN_POINT ( 'NONE',  ( 4.401177694619070380, 1.385992036768167068, 1.026327495003590551 ) ) ;
#1293 = CARTESIAN_POINT ( 'NONE',  ( 0.1399997263886038068, 0.2431072571701595186, -2.034387401959360187 ) ) ;
#1294 = CARTESIAN_POINT ( 'NONE',  ( 4.172158584703322681, 5.890604320285754980, -1.599625672291256295 ) ) ;
#1295 = CARTESIAN_POINT ( 'NONE',  ( 11.86145016429273191, 10.90000000000000036, 1.099999999999996758 ) ) ;
#1296 = CARTESIAN_POINT ( 'NONE',  ( 1.310910670669521272, -1.548711629584406113, 1.204245502051364936 ) ) ;
#1297 = CARTESIAN_POINT ( 'NONE',  ( 4.924636110261782385, 6.768494766770632332, 1.599625672291267398 ) ) ;
#1298 = CARTESIAN_POINT ( 'NONE',  ( 0.1755611466353447780, 1.308645672766622914, -2.493865953706751792 ) ) ;
#1299 = VERTEX_POINT ( 'NONE', #59288 ) ;
#1300 =( LENGTH_UNIT ( ) NAMED_UNIT ( * ) SI_UNIT ( .MILLI., .METRE. ) );
#1301 = VERTEX_POINT ( 'NONE', #170096 ) ;
#1302 = CARTESIAN_POINT ( 'NONE',  ( 3.773895570499671503, 1.797357569013877887, -0.2251608728849313346 ) ) ;
#1303 = ORIENTED_EDGE ( 'NONE', *, *, #173163, .T. ) ;
#1304 = CARTESIAN_POINT ( 'NONE',  ( 6.866278450678116485, 6.975356045404744521, 0.000000000000000000 ) ) ;
#1305 = CARTESIAN_POINT ( 'NONE',  ( 0.000000000000000000, 10.00000000000000888, 0.000000000000000000 ) ) ;
#1306 = CARTESIAN_POINT ( 'NONE',  ( 4.406777823604307365, -0.4013596350818599556, -1.766266891646672166 ) ) ;
#1307 = CARTESIAN_POINT ( 'NONE',  ( 5.763624699140868834, 7.817591130454727200, -1.443375672974078761 ) ) ;
#1308 = FILL_AREA_STYLE ('',( #117284 ) ) ;
#1309 = CARTESIAN_POINT ( 'NONE',  ( 5.762717851902044330, 6.056246448182416309, -0.5943541797442238872 ) ) ;
#1311 = CARTESIAN_POINT ( 'NONE',  ( 9.999301985278609806, 11.62460605670194447, 1.199719254218452047 ) ) ;
#1310 = CARTESIAN_POINT ( 'NONE',  ( 6.039480578167179203, 1.719269793624801590, -0.7129749698730929452 ) ) ;
#1312 = CARTESIAN_POINT ( 'NONE',  ( 3.550306043379815257, -1.284141074626928392, 1.421643848488469031 ) ) ;
#1313 = AXIS2_PLACEMENT_3D ( 'NONE', #163918, #211566, #65305 ) ;
#1314 = DIRECTION ( 'NONE',  ( -5.421010862427534989E-16, 0.5005768354468326242, 0.8656921114426506803 ) ) ;
#1315 = CARTESIAN_POINT ( 'NONE',  ( -11.43653507270588499, 5.655220009861049668, 5.468867579827167980 ) ) ;
#1316 = CARTESIAN_POINT ( 'NONE',  ( 9.499633409936901529, -9.910600865424404660, -0.08345703571627054174 ) ) ;
#1317 = CARTESIAN_POINT ( 'NONE',  ( -1.364683531250014514, -1.219791666325248602, 0.7879004041258379498 ) ) ;
#1318 = AXIS2_PLACEMENT_3D ( 'NONE', #155804, #120166, #185069 ) ;
#1319 = CARTESIAN_POINT ( 'NONE',  ( 6.399085315970131305, 8.488685506763726352, -1.443375672974057666 ) ) ;
#1321 = CARTESIAN_POINT ( 'NONE',  ( 5.260995011843273339, -0.05493784808423751720, -2.116803055475650730 ) ) ;
#1320 = CARTESIAN_POINT ( 'NONE',  ( -9.653042183249970876, 11.32459930428888306, -1.082531754730539753 ) ) ;
#1322 = CARTESIAN_POINT ( 'NONE',  ( 0.9894095316701528864, 1.906041449620498707, -1.019753361306941386 ) ) ;
#1323 = CARTESIAN_POINT ( 'NONE',  ( -5.692444392891315097, 7.734547439830227411, -1.599625672291271394 ) ) ;
#1324 = CARTESIAN_POINT ( 'NONE',  ( 6.703580607314123085, 6.785541894813420072, 0.000000000000000000 ) ) ;
#1325 = CARTESIAN_POINT ( 'NONE',  ( 0.7799652524137989928, -1.018268764971082430, 1.515009401286564694 ) ) ;
#1326 = CARTESIAN_POINT ( 'NONE',  ( -4.939248034080176097, 4.656877549381960080, 1.214306433183764966E-14 ) ) ;
#1327 = CARTESIAN_POINT ( 'NONE',  ( 3.258640109524315154, -1.383274205585843797, 1.191454006006509303 ) ) ;
#1328 = CARTESIAN_POINT ( 'NONE',  ( 9.578206935409037115, -9.746166700193986898, -0.1671882239534273895 ) ) ;
#1329 = CARTESIAN_POINT ( 'NONE',  ( 1.757924209179074770, 0.7287868685415777037, -1.768279316124596878 ) ) ;
#1330 = EDGE_LOOP ( 'NONE', ( #91029, #12999, #122001, #37714, #25958, #53087 ) ) ;
#1331 = CARTESIAN_POINT ( 'NONE',  ( 2.963290904843593587, 1.662405373943407261, 1.055889934586044188 ) ) ;
#1332 = CARTESIAN_POINT ( 'NONE',  ( 4.739756017840593749, 1.937102985688110568, 0.1393878014490906314 ) ) ;
#1333 = CARTESIAN_POINT ( 'NONE',  ( -5.887983850084758330, 10.09134126839936840, 0.7998128361456291469 ) ) ;
#1335 = CARTESIAN_POINT ( 'NONE',  ( 4.096021571020786567, 1.387573888390711385, 1.603661410755026440 ) ) ;
#1334 = CARTESIAN_POINT ( 'NONE',  ( 5.996449078994045223, 10.21788403546024782, 0.7998128361456331437 ) ) ;
#1336 = DIRECTION ( 'NONE',  ( 0.7592566023653004592, -0.6507913734559639396, 0.000000000000000000 ) ) ;
#1337 = CARTESIAN_POINT ( 'NONE',  ( 2.789602095257078584, 1.815147277589121533, -0.6018686165152677958 ) ) ;
#1338 = CARTESIAN_POINT ( 'NONE',  ( 6.115167699822185554, 6.015585554489271125, 0.01814796302670486361 ) ) ;
#1339 = CARTESIAN_POINT ( 'NONE',  ( -4.281104764355953662, 5.612007818275039917, -1.265243560071245055 ) ) ;
#1340 = CARTESIAN_POINT ( 'NONE',  ( 0.000000000000000000, 9.999999999999998224, -2.000000000000000000 ) ) ;
#1341 = CARTESIAN_POINT ( 'NONE',  ( 3.718679271898170491, 7.560485927181699317, 0.7998128361456271485 ) ) ;
#1342 = DIRECTION ( 'NONE',  ( -3.330669073875479482E-16, 3.330669073875479482E-16, 1.000000000000000000 ) ) ;
#1343 = CARTESIAN_POINT ( 'NONE',  ( 5.268108045213575785, 0.9031548532531764595, 1.586571422427636824 ) ) ;
#1344 = CYLINDRICAL_SURFACE ( 'NONE', #14413, 0.6500000000000000222 ) ;
#1345 = CARTESIAN_POINT ( 'NONE',  ( -8.839552966430012759, 10.37552855133225904, -1.082531754730543971 ) ) ;
#1346 = CARTESIAN_POINT ( 'NONE',  ( -6.458928793950097891, 6.861006557743732692, 0.6885227102202008398 ) ) ;
#1347 = CARTESIAN_POINT ( 'NONE',  ( -0.3000000000000289102, 3.999999999999980904, -0.9782388782689288576 ) ) ;
#1348 = CARTESIAN_POINT ( 'NONE',  ( 5.787941465827733722, -0.8397648285632768328, 1.671655200917811168 ) ) ;
#1349 = CARTESIAN_POINT ( 'NONE',  ( 8.111855979677986994, 8.358253485912799263, 1.040834085586084257E-14 ) ) ;
#1350 = CARTESIAN_POINT ( 'NONE',  ( -3.922452899745962451, 7.727945483012266692, -0.5281491603440056082 ) ) ;
#1351 = EDGE_CURVE ( 'NONE', #113572, #84297, #191408, .T. ) ;
#1352 = CARTESIAN_POINT ( 'NONE',  ( 4.813308228051395687, 5.574280006603454574, 1.199719254218462483 ) ) ;
#1353 = CARTESIAN_POINT ( 'NONE',  ( -0.6823417656250039265, 9.880208333674728394, -1.181850606188755259 ) ) ;
#1354 = CARTESIAN_POINT ( 'NONE',  ( -4.629219384062206011, 7.488174150459498968, -1.199719254218452047 ) ) ;
#1355 = CARTESIAN_POINT ( 'NONE',  ( -4.516274566683622815, 5.401980094953223066, 1.082531754730549078 ) ) ;
#1356 = CARTESIAN_POINT ( 'NONE',  ( -6.742482464697739708, 6.760651051769146491, 0.7998128361456341429 ) ) ;
#1357 = CARTESIAN_POINT ( 'NONE',  ( 6.877770952621925282, -2.108145516380425910, 0.5186976372570563099 ) ) ;
#1358 = CARTESIAN_POINT ( 'NONE',  ( 0.8259615556985228091, 0.8540520341687988237, -1.937501654548081875 ) ) ;
#1359 = CARTESIAN_POINT ( 'NONE',  ( 10.06423010004587759, 10.63602329300870153, 0.000000000000000000 ) ) ;
#1360 = CARTESIAN_POINT ( 'NONE',  ( 0.4934552264687537271, 6.857579847919138771, 3.660192259447391461 ) ) ;
#1361 = CARTESIAN_POINT ( 'NONE',  ( 6.807487347360918761, -1.659057770219806160, -1.238116672595261480 ) ) ;
#1363 = CARTESIAN_POINT ( 'NONE',  ( 4.033840454514115770, 7.781623563118116316, -0.4120627063678127255 ) ) ;
#1362 = CARTESIAN_POINT ( 'NONE',  ( 1.733694375844633706, 1.821329977863223926, 0.2691589665217360983 ) ) ;
#1364 = CARTESIAN_POINT ( 'NONE',  ( 6.182154858151487353, 6.314861544039274577, -0.7216878364870257245 ) ) ;
#1366 = CARTESIAN_POINT ( 'NONE',  ( -2.081668171172168513E-14, 6.487495393664096888, 3.100011470320013451 ) ) ;
#1365 = CARTESIAN_POINT ( 'NONE',  ( 3.475000000000000533, -3.675000000000001155, 0.000000000000000000 ) ) ;
#1367 = CARTESIAN_POINT ( 'NONE',  ( 1.939794425703120995, 0.8746495868690505882, -2.119022276272637839 ) ) ;
#1369 = CARTESIAN_POINT ( 'NONE',  ( 1.123270288250309834, 3.221052654332833054, -0.7749999999993620881 ) ) ;
#1368 = CARTESIAN_POINT ( 'NONE',  ( -1.198337723683057465, 3.300000000000024691, 0.6661986840810731891 ) ) ;
#1370 = CARTESIAN_POINT ( 'NONE',  ( 2.197387184563174944, 1.746976956643018442, -0.7784620831182070821 ) ) ;
#1371 = ORIENTED_EDGE ( 'NONE', *, *, #22519, .F. ) ;
#1372 = CARTESIAN_POINT ( 'NONE',  ( 8.893785580440313865, 9.478430720042945623, 1.040834085586084257E-14 ) ) ;
#1373 = EDGE_CURVE ( 'NONE', #149611, #126977, #18598, .T. ) ;
#1374 = CARTESIAN_POINT ( 'NONE',  ( 0.6330651387380836770, 1.861715503769780566, 0.7666268175344230773 ) ) ;
#1375 = CARTESIAN_POINT ( 'NONE',  ( 0.9187138386215136787, -1.424830647414500051, 1.348730089142296418 ) ) ;
#1376 = CARTESIAN_POINT ( 'NONE',  ( -0.3282377607281257714, 2.761164550367435133, -1.225000000000007638 ) ) ;
#1378 = CARTESIAN_POINT ( 'NONE',  ( -10.43233925736708301, 5.066585305077033752, -5.254699789447807134 ) ) ;
#1377 = CARTESIAN_POINT ( 'NONE',  ( -7.527801604085656351, 9.805521176231838609, 1.599625672291295375 ) ) ;
#1379 = CARTESIAN_POINT ( 'NONE',  ( -9.348561386651960348, 4.000000000000000888, 7.001914024036570261 ) ) ;
#1381 = CARTESIAN_POINT ( 'NONE',  ( 2.693947877954734338, -1.764960265255947736, -0.1323486908471616652 ) ) ;
#1380 = CARTESIAN_POINT ( 'NONE',  ( 4.312501488504257630, 1.911392599577836693, 0.8473735431044140398 ) ) ;
#1382 = CARTESIAN_POINT ( 'NONE',  ( 7.752014238602739730E-16, 1.000000000000002665, -6.329999999999995630 ) ) ;
#1384 = CARTESIAN_POINT ( 'NONE',  ( 5.736350775408121550, 0.4420370857395071740, 2.249087507758650517 ) ) ;
#1383 = CARTESIAN_POINT ( 'NONE',  ( 2.672702088255949078E-15, 1.937500000000013323, -1.225000000000018074 ) ) ;
#1385 = CARTESIAN_POINT ( 'NONE',  ( 3.327794560494615084, 1.698141246764593770, 0.3800555388253792355 ) ) ;
#1386 = CARTESIAN_POINT ( 'NONE',  ( 9.541187415715040032, 12.15447128979948310, -1.599625672291262513 ) ) ;
#1387 = CARTESIAN_POINT ( 'NONE',  ( 2.864235035935404738, -0.5475380835847867278, 1.645162456946830831 ) ) ;
#1388 = CARTESIAN_POINT ( 'NONE',  ( 3.772083221923136609, -2.139637338432040181, 0.3678540365955537128 ) ) ;
#1389 = CARTESIAN_POINT ( 'NONE',  ( 5.522248639467795428, 5.337044922334209573, -0.7998128361456231517 ) ) ;
#1390 = CARTESIAN_POINT ( 'NONE',  ( 5.753138727196851043, 0.1435251449807967150, -2.011451301405759118 ) ) ;
#1391 = CARTESIAN_POINT ( 'NONE',  ( 0.6250000000000001110, -2.052068128417942283, 3.751950811937565850E-14 ) ) ;
#1392 = CARTESIAN_POINT ( 'NONE',  ( 1.499999999999989120, 4.535416667349484676, 0.8660254037844524744 ) ) ;
#1393 = CARTESIAN_POINT ( 'NONE',  ( 2.010648722831087198, 1.429088002864507212, -1.291968487218410511 ) ) ;
#1394 = CARTESIAN_POINT ( 'NONE',  ( 1.499999999999997113, 8.927083334016126415, -0.8660254037844378194 ) ) ;
#1395 = CARTESIAN_POINT ( 'NONE',  ( 5.414381242519362480, -2.221583670654456721, 0.0001252536179462138133 ) ) ;
#1396 = EDGE_LOOP ( 'NONE', ( #3690, #54781, #30008, #199049 ) ) ;
#1397 = CARTESIAN_POINT ( 'NONE',  ( -0.1106856583841242386, 7.629137130509040965, -2.596956429031356262 ) ) ;
#1398 = CARTESIAN_POINT ( 'NONE',  ( 0.7499999999999902300, 1.983333333333357817, 1.299038105676669330 ) ) ;
#1399 = CARTESIAN_POINT ( 'NONE',  ( 5.612185521052973414, 8.634967976948757951, -1.199719254218440723 ) ) ;
#1400 = CARTESIAN_POINT ( 'NONE',  ( 4.406036734316882253, 6.163462161501577441, -1.443375672974051449 ) ) ;
#1401 = CARTESIAN_POINT ( 'NONE',  ( -3.285556943750000070, -1.859374999522041882, 0.000000000000000000 ) ) ;
#1402 = CARTESIAN_POINT ( 'NONE',  ( 1.418920233055203761, -0.8037200727962053870, -2.070967414838392084 ) ) ;
#1403 = CARTESIAN_POINT ( 'NONE',  ( 2.494940289813108780, 3.499999999999989342, -11.73777120880564695 ) ) ;
#1404 = CARTESIAN_POINT ( 'NONE',  ( 8.771762198361678031, 9.336070107617867819, 1.040834085586084257E-14 ) ) ;
#1405 = FACE_OUTER_BOUND ( 'NONE', #99903, .T. ) ;
#1406 = CARTESIAN_POINT ( 'NONE',  ( 6.802048716365778347, -2.262122309816359422, 0.04523717395405778968 ) ) ;
#1407 = PRESENTATION_LAYER_ASSIGNMENT (  '', '', ( #67119 ) ) ;
#1408 = CARTESIAN_POINT ( 'NONE',  ( 4.716257332707354699, 6.595662536282280719, -1.599625672291269396 ) ) ;
#1409 = CARTESIAN_POINT ( 'NONE',  ( -4.394251184604987870, 5.259619482528146150, 1.082531754730549078 ) ) ;
#1410 = CARTESIAN_POINT ( 'NONE',  ( 4.018078825213769356, 2.047437054436978876, -0.2496575186523365686 ) ) ;
#1411 = CARTESIAN_POINT ( 'NONE',  ( -5.752737250900127997, 5.605948302338584099, 0.000000000000000000 ) ) ;
#1412 = CARTESIAN_POINT ( 'NONE',  ( 1.499999999999989120, 4.285416667349482900, 0.8660254037844524744 ) ) ;
#1413 = CARTESIAN_POINT ( 'NONE',  ( -0.6823417656250246877, -0.1989583329919109023, 1.181850606188755259 ) ) ;
#1414 = CARTESIAN_POINT ( 'NONE',  ( 5.413307058180727438, -0.2754873708227522644, 1.850039175317084617 ) ) ;
#1415 = CARTESIAN_POINT ( 'NONE',  ( 4.729033670188855787, 1.730023327335796113, 0.1204123811070593880 ) ) ;
#1416 = CARTESIAN_POINT ( 'NONE',  ( 4.247407853763897734, 1.739958666061100390, -0.04810691789801542495 ) ) ;
#1417 = CARTESIAN_POINT ( 'NONE',  ( 5.020596955762157698, 4.751784624677624080, 1.040834085586084257E-14 ) ) ;
#1418 = CARTESIAN_POINT ( 'NONE',  ( 1.664052950329899971, 1.182993008014191938, 1.963431667052175422 ) ) ;
#1419 = CARTESIAN_POINT ( 'NONE',  ( -1.001543065824772872E-14, 4.884375000341420581, 1.575800808251672791 ) ) ;
#1420 = CARTESIAN_POINT ( 'NONE',  ( 5.847236579984706140, 0.6061975457797988964, -2.000951093856804253 ) ) ;
#1421 = CARTESIAN_POINT ( 'NONE',  ( 6.456980378258257325, 0.3295113258894696862, -1.913641714292084073 ) ) ;
#1422 = CARTESIAN_POINT ( 'NONE',  ( -0.2887529476172396303, 1.000000000000000888, 11.89119375935166012 ) ) ;
#1423 = CARTESIAN_POINT ( 'NONE',  ( 1.090470458312575053, -0.4872005951904456733, 1.956561897242928172 ) ) ;
#1424 = CARTESIAN_POINT ( 'NONE',  ( -3.755245360860945958, 7.324943987738942397, -0.7216878364870454865 ) ) ;
#1425 = CARTESIAN_POINT ( 'NONE',  ( 7.320801413324473650, 14.00000000000000000, -10.35317664616355771 ) ) ;
#1426 = CARTESIAN_POINT ( 'NONE',  ( -7.714753101375940503, 8.959299025482085455, 1.199719254218462483 ) ) ;
#1427 = CARTESIAN_POINT ( 'NONE',  ( 6.114890974963323345, 7.092793211334054604, 1.199719254218462483 ) ) ;
#1428 = CARTESIAN_POINT ( 'NONE',  ( -3.755786496842897795E-14, 1.453125000341440876, 1.570758158831776052 ) ) ;
#1429 = CARTESIAN_POINT ( 'NONE',  ( 3.405043383231837417, -0.4154483767263848493, -2.079220720149973278 ) ) ;
#1430 = CARTESIAN_POINT ( 'NONE',  ( -0.6823417656250003738, -0.5322916663252491576, -1.181850606188749264 ) ) ;
#1431 = CARTESIAN_POINT ( 'NONE',  ( 5.654876981934024549, -1.436564326775534806, 1.126588154728463742 ) ) ;
#1432 = VERTEX_POINT ( 'NONE', #200449 ) ;
#1433 = CARTESIAN_POINT ( 'NONE',  ( -5.769876891067536206, 8.889217585290882795, 1.199719254218454489 ) ) ;
#1434 =( LENGTH_UNIT ( ) NAMED_UNIT ( * ) SI_UNIT ( .MILLI., .METRE. ) );
#1435 = CARTESIAN_POINT ( 'NONE',  ( -1.737500000000000266, -2.814583332377419644, -3.009438278150923907 ) ) ;
#1436 = CARTESIAN_POINT ( 'NONE',  ( -5.181187258716735577, 9.196468901811520880, 0.7998128361456481317 ) ) ;
#1437 = CARTESIAN_POINT ( 'NONE',  ( 3.744402900219420793, 1.076886947916893211, -1.708549110318995368 ) ) ;
#1438 = CARTESIAN_POINT ( 'NONE',  ( 0.5343771797220103759, 1.082321145649869587, -1.806417116151628477 ) ) ;
#1439 = CARTESIAN_POINT ( 'NONE',  ( -4.995253251992230581, 4.792493313604505367, 0.000000000000000000 ) ) ;
#1440 = CARTESIAN_POINT ( 'NONE',  ( 3.572968443166994579, 1.680613686130405515, 0.7995154651666557255 ) ) ;
#1441 = CARTESIAN_POINT ( 'NONE',  ( 10.22692794340986921, 10.82583744360002243, 0.000000000000000000 ) ) ;
#1442 = CARTESIAN_POINT ( 'NONE',  ( 10.62873463776380056, 12.30000000000000071, -3.200000000000001510 ) ) ;
#1443 = CARTESIAN_POINT ( 'NONE',  ( -2.981903720001798597, 5.566305875722335372, -1.199719254218446718 ) ) ;
#1444 = CARTESIAN_POINT ( 'NONE',  ( -7.670162217029145246, 9.971608557999250166, 1.599625672291295375 ) ) ;
#1445 = CARTESIAN_POINT ( 'NONE',  ( 6.332896556214961947, 0.1992470125839322093, 2.051223679500746133 ) ) ;
#1447 = CARTESIAN_POINT ( 'NONE',  ( -5.011569529345123897, 6.785514760743092566, 1.449221747052743092 ) ) ;
#1446 = CARTESIAN_POINT ( 'NONE',  ( -5.738844160334429567, 9.917344963690652548, 0.000000000000000000 ) ) ;
#1448 = CARTESIAN_POINT ( 'NONE',  ( 5.011754246625688580, 8.023990808224052529, -1.135194352273690255 ) ) ;
#1449 = CARTESIAN_POINT ( 'NONE',  ( 2.073226780758777643, 1.288078611216292302, -1.160843940205048774 ) ) ;
#1450 = CARTESIAN_POINT ( 'NONE',  ( 1.481926975991064710, -0.2526488567047910361, -1.721760536436983680 ) ) ;
#1452 = CARTESIAN_POINT ( 'NONE',  ( 8.622622508611357262, 9.162073802909148412, -0.7216878364870197293 ) ) ;
#1451 = CARTESIAN_POINT ( 'NONE',  ( 0.3941752559601471306, 1.712991706939146486, 1.546321376980333007 ) ) ;
#1453 = CARTESIAN_POINT ( 'NONE',  ( 3.203469434578891661, 6.959407783642502565, -0.7998128361456362523 ) ) ;
#1454 = CARTESIAN_POINT ( 'NONE',  ( 1.774756598535260466, -1.955815263226182932, -0.6494449766335576024 ) ) ;
#1455 = CARTESIAN_POINT ( 'NONE',  ( 3.832150974156964818, 7.622593236491780999, 1.040834085586084257E-14 ) ) ;
#1456 = CARTESIAN_POINT ( 'NONE',  ( 6.309976275596433481, -1.946771231211348319, 1.221538734657970693 ) ) ;
#1457 = FACE_OUTER_BOUND ( 'NONE', #169413, .T. ) ;
#1459 = CIRCLE ( 'NONE', #122659, 10.99999999999738698 ) ;
#1458 = CARTESIAN_POINT ( 'NONE',  ( -5.041653019435350380, 6.975290837464928728, -1.599625672291271394 ) ) ;
#1460 = CARTESIAN_POINT ( 'NONE',  ( 0.6023365795125863453, -0.6618663087945526602, -1.857178468014776263 ) ) ;
#1461 = VECTOR ( 'NONE', #26119, 1000.000000000000000 ) ;
#1463 = CARTESIAN_POINT ( 'NONE',  ( -6.997416678428844072, 8.296645891989347987, 1.082531754730549078 ) ) ;
#1462 = CARTESIAN_POINT ( 'NONE',  ( 4.359561026920276916, -1.481784043772149229, -1.208992945495937610 ) ) ;
#1464 = CARTESIAN_POINT ( 'NONE',  ( 6.375609195709820654, 2.113139023092651225, -0.6363509056886568205 ) ) ;
#1465 = CARTESIAN_POINT ( 'NONE',  ( -6.766604819867150233, -7.256397064628574256, -6.766604819867120035 ) ) ;
#1466 = CARTESIAN_POINT ( 'NONE',  ( 6.068156270568149324, 9.237210194708310951, 1.199719254218452047 ) ) ;
#1467 = CARTESIAN_POINT ( 'NONE',  ( -3.919715807682309094, 6.626733304721049933, 1.082531754730549967 ) ) ;
#1468 = CARTESIAN_POINT ( 'NONE',  ( -0.02277885239688070759, -1.805142470748948513, -0.9059449988992168690 ) ) ;
#1469 = CARTESIAN_POINT ( 'NONE',  ( 3.329449612262088021, 0.05463889213834548231, 2.307092628889866326 ) ) ;
#1470 = CARTESIAN_POINT ( 'NONE',  ( 5.195737816846159873, -1.386088135442983260, -1.388664821390848347 ) ) ;
#1471 = CARTESIAN_POINT ( 'NONE',  ( 1.235121763443976395, -0.04261391538399812023, -1.961451400788959631 ) ) ;
#1472 = DIRECTION ( 'NONE',  ( 0.000000000000000000, -1.000000000000000000, 0.000000000000000000 ) ) ;
#1473 = FACE_OUTER_BOUND ( 'NONE', #175970, .T. ) ;
#1474 = ORIENTED_EDGE ( 'NONE', *, *, #92359, .T. ) ;
#1475 = CARTESIAN_POINT ( 'NONE',  ( -0.2349522205629230309, -0.1529240981989663239, -2.083514258294770105 ) ) ;
#1477 = CARTESIAN_POINT ( 'NONE',  ( -7.133561379084627063, 11.47423870890741782, 0.7998128361456481317 ) ) ;
#1476 = CARTESIAN_POINT ( 'NONE',  ( -3.411848212133334446, 7.132240014130862171, 0.7998128361456341429 ) ) ;
#1478 = FACE_OUTER_BOUND ( 'NONE', #174070, .T. ) ;
#1479 = CARTESIAN_POINT ( 'NONE',  ( 3.924824802941798030, -1.462044496099848212, 1.605114832664520153 ) ) ;
#1480 = CARTESIAN_POINT ( 'NONE',  ( 1.448815997565377156, 7.903552007303750848, -10.65195286442484601 ) ) ;
#1482 = EDGE_CURVE ( 'NONE', #30243, #96092, #98102, .T. ) ;
#1481 = CARTESIAN_POINT ( 'NONE',  ( 1.652743449602233072, 2.098267697663995790, 0.3060111223712052020 ) ) ;
#1483 = CARTESIAN_POINT ( 'NONE',  ( -1.500000000000013101, 2.410416667349482456, -0.8660254037844313801 ) ) ;
#1484 = CARTESIAN_POINT ( 'NONE',  ( 10.71502147350184231, 11.39527989537399755, 0.000000000000000000 ) ) ;
#1485 = CARTESIAN_POINT ( 'NONE',  ( -3.011287625495571607, 6.360174617139689346, -0.7852620323503290978 ) ) ;
#1486 = CARTESIAN_POINT ( 'NONE',  ( 6.598740849494261873, 6.770918179921630475, -0.1579934589533253664 ) ) ;
#1487 = CARTESIAN_POINT ( 'NONE',  ( 2.179047869568909945, -0.09785464545388269930, -2.058565441667548068 ) ) ;
#1489 = CARTESIAN_POINT ( 'NONE',  ( 1.438880590755393429, 3.300000000000025135, 0.4368907704009279414 ) ) ;
#1488 = CARTESIAN_POINT ( 'NONE',  ( -9.179033691651859783, 10.66762638080401260, 1.199719254218462483 ) ) ;
#1490 = CARTESIAN_POINT ( 'NONE',  ( -0.6823417656250212460, 2.551041667008084435, 1.181850606188767472 ) ) ;
#1491 = CARTESIAN_POINT ( 'NONE',  ( -0.02244404828157658613, 5.719765766439059540, -2.783169749654360814 ) ) ;
#1492 = FACE_OUTER_BOUND ( 'NONE', #13832, .T. ) ;
#1493 = EDGE_LOOP ( 'NONE', ( #199835, #152427, #123597, #122648, #51346 ) ) ;
#1494 = CARTESIAN_POINT ( 'NONE',  ( 4.512308969215598431, -1.911949174345693336, -0.04343532550177275214 ) ) ;
#1495 = CARTESIAN_POINT ( 'NONE',  ( 4.542476715900265916, 4.951051008190067826, -0.8264431066547142102 ) ) ;
#1496 = CARTESIAN_POINT ( 'NONE',  ( 1.616897013105462522, 1.519709519468028791, -1.676125853178417113 ) ) ;
#1497 = CARTESIAN_POINT ( 'NONE',  ( -10.49364770729726359, 11.34493653470939023, 0.7216878364870438212 ) ) ;
#1498 = CARTESIAN_POINT ( 'NONE',  ( 1.265540092975623088, 0.5243090560775253151, -1.734071359953066382 ) ) ;
#1499 = CARTESIAN_POINT ( 'NONE',  ( 2.290125521308879808, -0.7372973962519657753, -1.768360312244516841 ) ) ;
#1500 = CARTESIAN_POINT ( 'NONE',  ( 2.734898984476673789, -1.980466496001157317, -0.6033880717724803278 ) ) ;
#1501 = CARTESIAN_POINT ( 'NONE',  ( -1.201851678989727383E-14, 2.134375000341423689, 1.575800808251672791 ) ) ;
#1502 = CARTESIAN_POINT ( 'NONE',  ( 0.3210827503922530357, -0.09932373348091848297, 1.969089571372897085 ) ) ;
#1503 = CARTESIAN_POINT ( 'NONE',  ( 5.672470344399177300, -1.220246509433765558, 1.490775554449337070 ) ) ;
#1505 = CARTESIAN_POINT ( 'NONE',  ( 5.910429572389825026, 7.145202977605201511, -1.123150837922413547 ) ) ;
#1504 = CARTESIAN_POINT ( 'NONE',  ( 6.586557750117827403, -2.163372447211810989, -0.4352210726449382006 ) ) ;
#1506 = CARTESIAN_POINT ( 'NONE',  ( -0.6823417656250212460, 1.301041667008083547, 1.181850606188755259 ) ) ;
#1507 = CARTESIAN_POINT ( 'NONE',  ( 5.318824396150737321, -1.496427615725079097, 1.419873077484270496 ) ) ;
#1508 = CARTESIAN_POINT ( 'NONE',  ( -5.819474248763749635, 7.812472595022922128, -1.599625672291256295 ) ) ;
#1509 = CARTESIAN_POINT ( 'NONE',  ( 8.076906825439115423, 10.44614393447756129, -1.599625672291262513 ) ) ;
#1510 = CARTESIAN_POINT ( 'NONE',  ( 5.217190183160311356, 4.981143389975473568, -0.7998128361456211532 ) ) ;
#1511 = EDGE_CURVE ( 'NONE', #26662, #152681, #56567, .T. ) ;
#1514 = CARTESIAN_POINT ( 'NONE',  ( -0.7499999999999972244, 3.858333333333359594, -1.299038105676652011 ) ) ;
#1513 = CARTESIAN_POINT ( 'NONE',  ( 4.735441112814092079, -1.926550399551892001, 0.8509862954892956077 ) ) ;
#1512 = CIRCLE ( 'NONE', #164066, 0.7499999999999997780 ) ;
#1515 = CARTESIAN_POINT ( 'NONE',  ( 1.346384888165049754, -0.9767783691352300846, 1.939140577548441380 ) ) ;
#1516 = CARTESIAN_POINT ( 'NONE',  ( -1.201851678989727383E-14, 3.009375000341419248, -1.575800808251660134 ) ) ;
#1517 = CARTESIAN_POINT ( 'NONE',  ( 5.237646302014136168, -1.524508687941978469, -1.532700278705993790 ) ) ;
#1518 = CARTESIAN_POINT ( 'NONE',  ( 5.074870355641393438, -1.461326316769593348, 1.394373881654621394 ) ) ;
#1519 = CARTESIAN_POINT ( 'NONE',  ( 0.000000000000000000, 6.999999999999992006, 0.000000000000000000 ) ) ;
#1520 = AXIS2_PLACEMENT_3D ( 'NONE', #146817, #128498, #131651 ) ;
#1523 = CARTESIAN_POINT ( 'NONE',  ( 5.178851490740193242, 8.025448591630130579, 1.082531754730558626 ) ) ;
#1522 = CARTESIAN_POINT ( 'NONE',  ( 3.285556943750000070, -0.9843749995220412163, 0.000000000000000000 ) ) ;
#1521 = CARTESIAN_POINT ( 'NONE',  ( -9.333041836230696831, 14.55305236563169302, -7.472413793098840351 ) ) ;
#1524 = CARTESIAN_POINT ( 'NONE',  ( -6.656127069666307072, 6.730179434224282886, 0.7998128361456341429 ) ) ;
#1525 = CARTESIAN_POINT ( 'NONE',  ( 3.749232653202066778, 0.2420323627391370025, -2.001857840249580800 ) ) ;
#1526 = CARTESIAN_POINT ( 'NONE',  ( -9.352427035328430449, 9.805586384171650849, 1.040834085586084257E-14 ) ) ;
#1528 = CARTESIAN_POINT ( 'NONE',  ( -10.96107445065241315, -5.401429653175735979, 0.1376292675369562291 ) ) ;
#1527 = CARTESIAN_POINT ( 'NONE',  ( -9.978437869977950569, 11.70422760547153906, -1.082531754730539753 ) ) ;
#1529 = CARTESIAN_POINT ( 'NONE',  ( 1.364683531249990311, 4.384375000341417028, 1.214306433183764966E-14 ) ) ;
#1531 = CARTESIAN_POINT ( 'NONE',  ( 1.364683531249996529, 8.463541667008065872, 0.7879004041258403923 ) ) ;
#1530 = CARTESIAN_POINT ( 'NONE',  ( 5.401312781148373432, 1.764888628567516049, 1.247983453017486699 ) ) ;
#1532 =( NAMED_UNIT ( * ) SI_UNIT ( $, .STERADIAN. ) SOLID_ANGLE_UNIT ( ) );
#1533 = DIRECTION ( 'NONE',  ( 1.000000000000000000, -5.578564026256504688E-16, -1.232595164407830946E-31 ) ) ;
#1535 = CARTESIAN_POINT ( 'NONE',  ( 5.132435489663482286, 0.5880379476735001498, 1.928747580961232444 ) ) ;
#1534 = CARTESIAN_POINT ( 'NONE',  ( -7.673551755210395342, 8.054824590608001600, 1.040834085586084257E-14 ) ) ;
#1536 = CARTESIAN_POINT ( 'NONE',  ( 1.499999999999990896, 5.025000000000022560, 1.214306433183764966E-14 ) ) ;
#1537 = CARTESIAN_POINT ( 'NONE',  ( 0.08204731311520391257, -1.671590265245853413, -0.4250796685295650246 ) ) ;
#1538 = CARTESIAN_POINT ( 'NONE',  ( 5.571474780572990504, 5.464751763615448787, 0.7998128361456352531 ) ) ;
#1540 = CARTESIAN_POINT ( 'NONE',  ( 5.643937085038755797, 9.806620042512378177, -0.7998128361456481317 ) ) ;
#1539 = CARTESIAN_POINT ( 'NONE',  ( 7.565086526745395723, 10.80938946696957004, -1.082531754730543083 ) ) ;
#1541 = CARTESIAN_POINT ( 'NONE',  ( -5.346851039111055748, 6.199209027673978412, -2.420000000000000373 ) ) ;
#1542 = CARTESIAN_POINT ( 'NONE',  ( 5.606678975738343951, 1.416997745663551633, -1.221222563005261774 ) ) ;
#1543 = CARTESIAN_POINT ( 'NONE',  ( 0.1881394758670457412, 1.160778376788082378, 1.644543748126830796 ) ) ;
#1544 = CARTESIAN_POINT ( 'NONE',  ( 6.539320575229254473, 0.5926322452488984593, 1.950287522085321301 ) ) ;
#1545 = CARTESIAN_POINT ( 'NONE',  ( 3.511198595814932766, 5.119484333249288532, 1.443375672974066548 ) ) ;
#1546 = CARTESIAN_POINT ( 'NONE',  ( -7.743115126736118015, 8.206258200713163475, 0.7216878364870317197 ) ) ;
#1547 = ORIENTED_EDGE ( 'NONE', *, *, #172795, .T. ) ;
#1548 = CARTESIAN_POINT ( 'NONE',  ( 8.690413276235306128, 13.08263988900915109, -0.7216878364870267237 ) ) ;
#1550 = CARTESIAN_POINT ( 'NONE',  ( 1.247672978039487734, 1.986097573956084439, -0.3474914183895366215 ) ) ;
#1549 = CARTESIAN_POINT ( 'NONE',  ( 1.770341816056511863, 2.114587264445011883, -0.1591180397043714667 ) ) ;
#1551 = CARTESIAN_POINT ( 'NONE',  ( 2.355456482938292240, -1.344675202547132464, -1.214172642412311598 ) ) ;
#1552 = CARTESIAN_POINT ( 'NONE',  ( 6.016786309414542622, 10.24161080428416426, 0.7998128361456341429 ) ) ;
#1553 = CARTESIAN_POINT ( 'NONE',  ( 5.981359018292747187, 1.999130597612966964, -0.8229454869796914984 ) ) ;
#1554 = ORIENTED_EDGE ( 'NONE', *, *, #33991, .T. ) ;
#1555 = CARTESIAN_POINT ( 'NONE',  ( 7.287671262545424966, 8.461036880179857889, -1.199719254218451159 ) ) ;
#1556 = CLOSED_SHELL ( 'NONE', ( #107918, #9042, #10227, #38719, #9976, #149647, #133397, #214326 ) ) ;
#1558 = CARTESIAN_POINT ( 'NONE',  ( -0.01269188720853537365, -0.5084903737302053361, 1.846954624685708923 ) ) ;
#1557 = CARTESIAN_POINT ( 'NONE',  ( -4.880045225915050189, 7.780804299287790826, 1.199719254218464037 ) ) ;
#1559 = LINE ( 'NONE', #22067, #152655 ) ;
#1560 = CYLINDRICAL_SURFACE ( 'NONE', #93873, 0.4000000000000010214 ) ;
#1561 = CARTESIAN_POINT ( 'NONE',  ( 5.951666246274803562, 7.006327377817825663, 1.082531754730558626 ) ) ;
#1562 = CARTESIAN_POINT ( 'NONE',  ( -1.201851678989727383E-14, 0.8843750003414173610, 1.575800808251672791 ) ) ;
#1563 = CARTESIAN_POINT ( 'NONE',  ( -3.164938793786285842, 5.779846795137578930, -1.199719254218452935 ) ) ;
#1564 = CARTESIAN_POINT ( 'NONE',  ( 4.540002997438313592, 0.9271085556134452954, -1.952944755896801610 ) ) ;
#1565 = CARTESIAN_POINT ( 'NONE',  ( -6.211043768836215229, 8.339580045099285854, 1.443375672974064550 ) ) ;
#1566 = CARTESIAN_POINT ( 'NONE',  ( 3.933273961740286317, 7.602920365423422311, 0.7216878364870257245 ) ) ;
#1567 = CARTESIAN_POINT ( 'NONE',  ( 1.793382672576701919, -0.1090974814243403090, -2.117938670719583527 ) ) ;
#1568 = CARTESIAN_POINT ( 'NONE',  ( 6.809597967592865508, -0.3964169337347979161, 1.788522171948719874 ) ) ;
#1569 = CARTESIAN_POINT ( 'NONE',  ( 2.776590643643538581, -1.885432240069355503, -0.5755950866291289492 ) ) ;
#1570 = CARTESIAN_POINT ( 'NONE',  ( 5.414289803398987466, -1.912571729023364364, 0.006307610287324683096 ) ) ;
#1571 = EDGE_LOOP ( 'NONE', ( #141077, #205442 ) ) ;
#1572 = CARTESIAN_POINT ( 'NONE',  ( 9.611540586923190688, -6.723650695528643695, -0.1589091098076216013 ) ) ;
#1573 = CARTESIAN_POINT ( 'NONE',  ( 6.373500198570408060, -0.2424619166165129514, 1.954513512140013676 ) ) ;
#1574 = CARTESIAN_POINT ( 'NONE',  ( 1.728360517318433542, 0.1903740514868361433, 1.932600189055997619 ) ) ;
#1575 = ORIENTED_EDGE ( 'NONE', *, *, #16285, .F. ) ;
#1576 = CARTESIAN_POINT ( 'NONE',  ( -3.298376509874564988, 7.070132704820777825, 0.000000000000000000 ) ) ;
#1578 = CARTESIAN_POINT ( 'NONE',  ( -4.480158349507305421E-13, -7.034525084948354490, 10.67552547708289268 ) ) ;
#1577 = CARTESIAN_POINT ( 'NONE',  ( -6.956742217587851052, 7.288823140040177506, 0.000000000000000000 ) ) ;
#1579 = CARTESIAN_POINT ( 'NONE',  ( 7.633404179693907388, 8.864391950186421454, -1.199719254218441611 ) ) ;
#1581 = CARTESIAN_POINT ( 'NONE',  ( 5.112833325684902341, 7.058334528089426740, -1.443375672974078761 ) ) ;
#1580 = CARTESIAN_POINT ( 'NONE',  ( 5.445571254183207088, 9.504916896522420444, -0.7998128361456281477 ) ) ;
#1583 = ORIENTED_EDGE ( 'NONE', *, *, #204878, .F. ) ;
#1582 = CARTESIAN_POINT ( 'NONE',  ( 5.602191078447533279, -0.8559053986842229955, 1.710104642658970997 ) ) ;
#1584 = CARTESIAN_POINT ( 'NONE',  ( 2.842613246588860942, 2.190307313262893185, 0.2694104812042824038 ) ) ;
#1585 = CARTESIAN_POINT ( 'NONE',  ( 2.292262453775519404, -0.9438808975747980945, 1.994871701834355804 ) ) ;
#1586 = CARTESIAN_POINT ( 'NONE',  ( 1.492681600543877440, 8.694743381153815065, 2.590460435319994481 ) ) ;
#1587 = CARTESIAN_POINT ( 'NONE',  ( 0.4516295384478058450, -1.352486712789633172, -1.352142238705160704 ) ) ;
#1588 = CARTESIAN_POINT ( 'NONE',  ( 0.000000000000000000, 13.49999999999999822, -1.500000000000000222 ) ) ;
#1589 = CARTESIAN_POINT ( 'NONE',  ( -6.756361134959188774, -6.891066458783145166, -6.828399852920279400 ) ) ;
#1590 = CARTESIAN_POINT ( 'NONE',  ( 3.385274849524767316, 0.04804411014160993310, 2.069964801482151895 ) ) ;
#1591 = CARTESIAN_POINT ( 'NONE',  ( -4.791917227426195858, 7.677988301050826969, -1.199719254218452047 ) ) ;
#1592 = CARTESIAN_POINT ( 'NONE',  ( -5.757633847399098670, 7.274473465504208036, 1.200491007486852002 ) ) ;
#1594 = CARTESIAN_POINT ( 'NONE',  ( 2.219795081190904629, -2.096929600374438429, 0.5247480557022954351 ) ) ;
#1593 = CARTESIAN_POINT ( 'NONE',  ( -4.009460741339347045, 5.700790169694431420, -1.599625672291256295 ) ) ;
#1595 = CARTESIAN_POINT ( 'NONE',  ( 3.720431430916489646, 2.081484170424623859, 0.6860852429351402826 ) ) ;
#1596 = CARTESIAN_POINT ( 'NONE',  ( 0.000000000000000000, 8.920000000000001705, -2.000000000000000000 ) ) ;
#1597 = CARTESIAN_POINT ( 'NONE',  ( 5.085717018901939390, 5.105960408239938353, 0.000000000000000000 ) ) ;
#1598 = CARTESIAN_POINT ( 'NONE',  ( -1.001543065824772872E-14, 4.743750000682821266, 1.732050807568877637 ) ) ;
#1599 = EDGE_CURVE ( 'NONE', #159704, #117563, #86721, .T. ) ;
#1600 = CARTESIAN_POINT ( 'NONE',  ( -1.402160292154681736E-14, 14.73437500034139980, 1.575800808251682339 ) ) ;
#1601 = CARTESIAN_POINT ( 'NONE',  ( -4.281342646865346602, 8.216926531310035031, 0.7998128361456352531 ) ) ;
#1603 = CARTESIAN_POINT ( 'NONE',  ( 5.660742353926829118, 1.040242247344788762, 1.387327330804826619 ) ) ;
#1602 = AXIS2_PLACEMENT_3D ( 'NONE', #73848, #139942, #205969 ) ;
#1604 = CARTESIAN_POINT ( 'NONE',  ( -8.351459436338023679, 12.68719374246231624, -0.7216878364870267237 ) ) ;
#1605 = CARTESIAN_POINT ( 'NONE',  ( 3.784089331405198209, -1.229265877060268242, -1.665672133652921660 ) ) ;
#1606 = CARTESIAN_POINT ( 'NONE',  ( 5.484029812627264633, -2.117403151077674739, 0.0008096548943584136460 ) ) ;
#1607 = AXIS2_PLACEMENT_3D ( 'NONE', #102862, #87673, #121322 ) ;
#1608 = CARTESIAN_POINT ( 'NONE',  ( 6.796715079152391148, 6.823922435299587974, 0.7998128361456341429 ) ) ;
#1609 = CARTESIAN_POINT ( 'NONE',  ( 1.364683531249990311, 4.634375000341417916, 1.214306433183764966E-14 ) ) ;
#1610 = CARTESIAN_POINT ( 'NONE',  ( 2.799605281554286229, -1.456005023894543893, -1.326338995474019011 ) ) ;
#1611 = CARTESIAN_POINT ( 'NONE',  ( 1.037202349414727109, -0.04413313863061394532, 1.912034500058952036 ) ) ;
#1612 = CARTESIAN_POINT ( 'NONE',  ( 6.035170563425642953, -1.656272789430097703, -1.584931405618497990 ) ) ;
#1613 = CARTESIAN_POINT ( 'NONE',  ( 3.351995281737112364, 1.825872481133209657, -0.0009662468829912955644 ) ) ;
#1614 = CARTESIAN_POINT ( 'NONE',  ( 4.903208829997618423, 5.749440385532527564, -1.199719254218450271 ) ) ;
#1615 = CARTESIAN_POINT ( 'NONE',  ( 3.999292125906894313, 7.609665213625947722, 0.7216878364870317197 ) ) ;
#1616 = CARTESIAN_POINT ( 'NONE',  ( -6.021792782764022078, 10.17717534653336209, -0.7998128361456291469 ) ) ;
#1617 = ORIENTED_EDGE ( 'NONE', *, *, #48198, .T. ) ;
#1618 = ORIENTED_EDGE ( 'NONE', *, *, #202081, .T. ) ;
#1619 = CARTESIAN_POINT ( 'NONE',  ( 3.656497369231588745, 2.003880934342232578, 0.1932520657266077191 ) ) ;
#1620 = CIRCLE ( 'NONE', #57014, 0.07999999999999998779 ) ;
#1621 = CARTESIAN_POINT ( 'NONE',  ( 4.750807836863311095, -0.4258335417525476729, -1.914832529679215023 ) ) ;
#1622 = CARTESIAN_POINT ( 'NONE',  ( -8.694856585065634746, 9.038420858865048757, 0.7998128361456462443 ) ) ;
#1623 = CARTESIAN_POINT ( 'NONE',  ( -5.250031796989778066, 7.148123067953287446, 1.599625672291267398 ) ) ;
#1624 = CARTESIAN_POINT ( 'NONE',  ( -3.947104627881522720, 8.980740528188976057, -0.7749999999999979128 ) ) ;
#1626 = CARTESIAN_POINT ( 'NONE',  ( 6.262547730648324595, -1.248425448203832611, 1.254777848270997254 ) ) ;
#1625 = CARTESIAN_POINT ( 'NONE',  ( 0.8727377898805768197, -0.05501089605610678251, -2.090203850258448792 ) ) ;
#1627 = CARTESIAN_POINT ( 'NONE',  ( 2.993041990875914493, 6.420974562437304911, 0.3677586026352899218 ) ) ;
#1628 = CARTESIAN_POINT ( 'NONE',  ( 1.588088344156918907, -2.181139600106785092, -0.2122876309011075546 ) ) ;
#1629 = CARTESIAN_POINT ( 'NONE',  ( 0.02830193721903468546, -1.592744100209501967, 0.7021035195741828216 ) ) ;
#1630 = CARTESIAN_POINT ( 'NONE',  ( 6.693975156845185737, 8.832723654451292816, 1.599625672291281386 ) ) ;
#1631 = CARTESIAN_POINT ( 'NONE',  ( 0.1333692844072559003, 2.872395615372814515, -2.542035612928101873 ) ) ;
#1632 = CARTESIAN_POINT ( 'NONE',  ( 0.2051046121598932848, -0.4657588872633237065, 1.660747436093058083 ) ) ;
#1633 = CARTESIAN_POINT ( 'NONE',  ( 0.8085102987360716087, -1.969961327451934086, 1.183767188307288221 ) ) ;
#1634 = CARTESIAN_POINT ( 'NONE',  ( 0.4861908890553789941, -2.175720422541329580, -0.2624175912114696252 ) ) ;
#1635 = CARTESIAN_POINT ( 'NONE',  ( 3.106307083854151774, -2.204334110825040494, 0.1085914373066959593 ) ) ;
#1636 = CARTESIAN_POINT ( 'NONE',  ( 0.3214382364499007161, -1.938747691508705184, -0.9774007134471692781 ) ) ;
#1637 = PLANE ( 'NONE',  #210177 ) ;
#1638 = CARTESIAN_POINT ( 'NONE',  ( 2.659486872612493613, 2.008994876937011398, -0.6687478447182227947 ) ) ;
#1639 = AXIS2_PLACEMENT_3D ( 'NONE', #182712, #2874, #135066 ) ;
#1640 = CARTESIAN_POINT ( 'NONE',  ( 6.827182134110199030, 1.215541611938670608, 2.400477883804314150 ) ) ;
#1641 = CARTESIAN_POINT ( 'NONE',  ( 5.245112492223927170, -1.652184091924509879, 0.9903546681122497031 ) ) ;
#1642 = VERTEX_POINT ( 'NONE', #153866 ) ;
#1644 = CARTESIAN_POINT ( 'NONE',  ( -1.001543065824772872E-14, 5.712500000000021672, 1.732050807568877637 ) ) ;
#1643 = CARTESIAN_POINT ( 'NONE',  ( 2.033172958078794501, -2.045629734292064850, 1.034765616053961557 ) ) ;
#1645 = CARTESIAN_POINT ( 'NONE',  ( 3.521367211247359741, 5.131347717920458962, -1.599625672291262513 ) ) ;
#1646 = CARTESIAN_POINT ( 'NONE',  ( 4.981731378017507872, 7.899438143407371271, -1.199719254218452047 ) ) ;
#1647 = CARTESIAN_POINT ( 'NONE',  ( 4.424628119981884211, -0.9497243516023866627, -2.008178830631357492 ) ) ;
#1648 = CARTESIAN_POINT ( 'NONE',  ( -7.456621297836087514, 9.722477485607340597, 1.443375672974090751 ) ) ;
#1649 = CARTESIAN_POINT ( 'NONE',  ( -2.493766133720152212, 8.265889183060426859, -2.456386456769293236 ) ) ;
#1650 = CARTESIAN_POINT ( 'NONE',  ( 6.317736394288140822, 7.433409217166723870, 1.082531754730558626 ) ) ;
#1651 = CARTESIAN_POINT ( 'NONE',  ( -8.365017589507372620, 9.821903944922480534, 1.082531754730558626 ) ) ;
#1652 = CARTESIAN_POINT ( 'NONE',  ( 5.316205630334249754, 7.295602216847000498, -1.443375672974078761 ) ) ;
#1653 = VECTOR ( 'NONE', #11849, 1000.000000000000000 ) ;
#1654 = ORIENTED_EDGE ( 'NONE', *, *, #41993, .T. ) ;
#1655 = CARTESIAN_POINT ( 'NONE',  ( 3.094375128876575065, -0.3905979561782264575, 1.978050703236901686 ) ) ;
#1657 = CARTESIAN_POINT ( 'NONE',  ( 0.5497677191402570163, 1.525909772416549126, 1.387868932477815065 ) ) ;
#1656 = CARTESIAN_POINT ( 'NONE',  ( 6.642605195691581699, 9.837124264027149678, 1.199719254218462483 ) ) ;
#1658 = CARTESIAN_POINT ( 'NONE',  ( -11.00029519899100450, -6.134628647623513231, 8.483881999699072196E-15 ) ) ;
#1659 = ADVANCED_FACE ( 'NONE', ( #152790 ), #205507, .T. ) ;
#1660 = CARTESIAN_POINT ( 'NONE',  ( 5.628043163004202931, 8.619781885929965526, -1.082531754730548412 ) ) ;
#1661 = CARTESIAN_POINT ( 'NONE',  ( -2.305169766234572926, 5.485456815665096464, -0.7666753726264395885 ) ) ;
#1662 = CARTESIAN_POINT ( 'NONE',  ( -1.201851678989727383E-14, 3.446875000341421469, -1.575800808251660134 ) ) ;
#1663 = CARTESIAN_POINT ( 'NONE',  ( 4.418054252288761141, 1.349281245414082342, -1.726737887558588591 ) ) ;
#1664 = CARTESIAN_POINT ( 'NONE',  ( 1.002577532868035526, -1.966644254196001196, 0.4445047019146358691 ) ) ;
#1665 = CARTESIAN_POINT ( 'NONE',  ( 1.311775528174640604, 1.236260529797410301, -1.364685630449238740 ) ) ;
#1666 = CARTESIAN_POINT ( 'NONE',  ( 5.513300880735551246, -2.237181406077014323, 0.4993042908148867531 ) ) ;
#1667 = CARTESIAN_POINT ( 'NONE',  ( 3.960763856159645879, 0.2235175650571289141, -1.827449369368571386 ) ) ;
#1668 = AXIS2_PLACEMENT_3D ( 'NONE', #81303, #62908, #211285 ) ;
#1669 = CARTESIAN_POINT ( 'NONE',  ( 8.392660782059197189, 9.750191319612612872, 1.199719254218462483 ) ) ;
#1670 =( NAMED_UNIT ( * ) SI_UNIT ( $, .STERADIAN. ) SOLID_ANGLE_UNIT ( ) );
#1671 = CARTESIAN_POINT ( 'NONE',  ( 3.996943106591983597, 1.542326501817241180, -0.9764022233923685956 ) ) ;
#1672 = CARTESIAN_POINT ( 'NONE',  ( 5.256482491209823138, 1.942542154241846397, -0.5404887192124520068 ) ) ;
#1673 = CARTESIAN_POINT ( 'NONE',  ( -9.040589502214116280, 9.441775928871617651, 0.7998128361456462443 ) ) ;
#1675 = CARTESIAN_POINT ( 'NONE',  ( -7.442499979258930587, 7.647614495415686164, -0.7998128361456362523 ) ) ;
#1674 = CARTESIAN_POINT ( 'NONE',  ( 4.997079013686112958, 1.883918014071528146, -1.252661935414706162 ) ) ;
#1676 = CARTESIAN_POINT ( 'NONE',  ( 6.282269041519704444, -1.129704631681987204, 1.777121156631493726 ) ) ;
#1677 = CARTESIAN_POINT ( 'NONE',  ( 1.499999999999990896, 4.306250000682819490, 1.214306433183764966E-14 ) ) ;
#1678 = CARTESIAN_POINT ( 'NONE',  ( 4.650872726564402981, -0.4503784926754761386, -2.020631409805350387 ) ) ;
#1679 = CARTESIAN_POINT ( 'NONE',  ( 9.728138913005292210, 11.30824913904973705, -1.199719254218440723 ) ) ;
#1680 = CARTESIAN_POINT ( 'NONE',  ( -2.754243431018125239E-14, 1.984375000341467299, 1.570758158831788265 ) ) ;
#1681 = APPLICATION_PROTOCOL_DEFINITION ( 'draft international standard', 'automotive_design', 1998, #110207 ) ;
#1683 = CARTESIAN_POINT ( 'NONE',  ( 2.191906549581578822, -0.8239416835312768361, 1.741544141456285555 ) ) ;
#1682 = CARTESIAN_POINT ( 'NONE',  ( -6.692921386640485082, 10.96015871772258521, -0.7998128361456291469 ) ) ;
#1684 = UNCERTAINTY_MEASURE_WITH_UNIT (LENGTH_MEASURE( 1.000000000000000082E-05 ), #105985, 'distance_accuracy_value', 'NONE');
#1685 = CARTESIAN_POINT ( 'NONE',  ( -5.029148636026397945, 4.832037928311032182, 0.7998128361456281477 ) ) ;
#1686 = CARTESIAN_POINT ( 'NONE',  ( 6.455907338579963017, -0.6669464233056993097, 1.853184144328771543 ) ) ;
#1687 = CARTESIAN_POINT ( 'NONE',  ( 5.194182247366881278, 5.232503174782402233, 0.7216878364870328300 ) ) ;
#1688 = CARTESIAN_POINT ( 'NONE',  ( 5.859090863903361424, 5.997168572722006097, -0.3086645125121977862 ) ) ;
#1689 = CARTESIAN_POINT ( 'NONE',  ( -3.898132859128961236, 4.506575409527250997, -1.199719254218452047 ) ) ;
#1691 = CARTESIAN_POINT ( 'NONE',  ( 2.268119307372215676, 0.5874642799142595351, -2.142291314107084954 ) ) ;
#1690 = CARTESIAN_POINT ( 'NONE',  ( 0.4398875993102538962, -2.011672884243600024, 0.6710486789910232730 ) ) ;
#1692 = CARTESIAN_POINT ( 'NONE',  ( 3.715936783694527179, -2.075135040979354528, 0.3580079364009710052 ) ) ;
#1693 = CARTESIAN_POINT ( 'NONE',  ( -7.449279056065764237, 7.655523418356991350, 0.7998128361456341429 ) ) ;
#1694 = CARTESIAN_POINT ( 'NONE',  ( 7.637320603199683866, 7.804628880021436288, -0.7998128361456281477 ) ) ;
#1695 = CARTESIAN_POINT ( 'NONE',  ( 0.6075646283644918766, 0.5893627863808469369, -1.765331146162614662 ) ) ;
#1696 = CARTESIAN_POINT ( 'NONE',  ( 7.623762449586013901, 7.788811034138823253, 1.040834085586084257E-14 ) ) ;
#1697 = CARTESIAN_POINT ( 'NONE',  ( -4.209440762792112878, 7.367024337791516331, -0.8326445619948764643 ) ) ;
#1698 = CARTESIAN_POINT ( 'NONE',  ( 3.662674053986138656, 7.424870162959149589, 0.7998128361456321445 ) ) ;
#1699 = CARTESIAN_POINT ( 'NONE',  ( -4.326460416536637155, 8.061637896019123062, 0.000000000000000000 ) ) ;
#1700 = CARTESIAN_POINT ( 'NONE',  ( -8.026063749610061748, 9.426457798375635022, -1.082531754730543971 ) ) ;
#1701 = CARTESIAN_POINT ( 'NONE',  ( 0.8441712343106638761, -1.349783269286155774, -1.635521010841307410 ) ) ;
#1702 = CARTESIAN_POINT ( 'NONE',  ( -4.938913097128142304, 8.984092056616635347, -0.7998128361456362523 ) ) ;
#1704 = CARTESIAN_POINT ( 'NONE',  ( 4.949637131784443866, 1.452432516441283905, 1.319008059494260143 ) ) ;
#1703 = CARTESIAN_POINT ( 'NONE',  ( 1.224999999999959233, 0.8541666666667160346, 0.7072540797572558491 ) ) ;
#1705 = CARTESIAN_POINT ( 'NONE',  ( 3.204151765443470357, -2.159293047372488950, 0.1044485798024074874 ) ) ;
#1706 = CARTESIAN_POINT ( 'NONE',  ( 1.311775528174640604, 1.236260529797410301, -1.364685630449238740 ) ) ;
#1707 = CARTESIAN_POINT ( 'NONE',  ( -4.018125071768071876, 7.621166010707856486, 0.1319346992594405132 ) ) ;
#1708 = CARTESIAN_POINT ( 'NONE',  ( -0.4644097342743139234, -8.233137084989849086, -9.488641820551089623 ) ) ;
#1709 = CARTESIAN_POINT ( 'NONE',  ( 4.277133665768851678, 1.139379310349198260, 1.315593229251702523 ) ) ;
#1710 = CARTESIAN_POINT ( 'NONE',  ( 0.3263184169966619752, 15.00000000000058265, -11.67999999558625213 ) ) ;
#1711 = CARTESIAN_POINT ( 'NONE',  ( 5.178851490740193242, 8.025448591630130579, 1.082531754730558626 ) ) ;
#1712 = CARTESIAN_POINT ( 'NONE',  ( -10.44369633504468631, 5.112959841837462882, -5.232137017608344820 ) ) ;
#1713 = CARTESIAN_POINT ( 'NONE',  ( 1.463986924769441478, 2.129665692569195024, -0.3698555562515608020 ) ) ;
#1714 = CARTESIAN_POINT ( 'NONE',  ( 3.796249832574852601, -1.863883295361246084, 0.7690029265580224926 ) ) ;
#1715 = CARTESIAN_POINT ( 'NONE',  ( -9.775065565328603157, 11.46695991671396087, -1.082531754730537976 ) ) ;
#1716 = CARTESIAN_POINT ( 'NONE',  ( 1.305796196612364124, -0.5247483525172502716, 2.096912610238470975 ) ) ;
#1717 = CARTESIAN_POINT ( 'NONE',  ( 3.660970522598467891, -1.737989841360635834, -0.9306492429120606369 ) ) ;
#1718 = CARTESIAN_POINT ( 'NONE',  ( 6.609000000000047947, 7.629137130509099585, 2.699999999999993516 ) ) ;
#1719 = CARTESIAN_POINT ( 'NONE',  ( 3.069799403425711226, -1.154559939549955949, 1.561474065217777207 ) ) ;
#1722 = ORIENTED_EDGE ( 'NONE', *, *, #196542, .T. ) ;
#1721 = CARTESIAN_POINT ( 'NONE',  ( -3.038435823238377687, 6.558942537171132514, -0.7216878364870458196 ) ) ;
#1720 = CARTESIAN_POINT ( 'NONE',  ( -9.124274191872636663, 11.66807252865000244, -1.443375672974058777 ) ) ;
#1723 = CARTESIAN_POINT ( 'NONE',  ( -5.289089322662584358, 5.343228095960675716, 0.000000000000000000 ) ) ;
#1724 = CARTESIAN_POINT ( 'NONE',  ( 3.923105346307896202, 5.670318552149568703, -1.599625672291269396 ) ) ;
#1725 = CARTESIAN_POINT ( 'NONE',  ( -4.142898457427624415, 6.991076079377632091, 1.199719254218452935 ) ) ;
#1726 = CARTESIAN_POINT ( 'NONE',  ( -6.791708605802965870, 6.888357893050385705, -0.7998128361456362523 ) ) ;
#1727 = CARTESIAN_POINT ( 'NONE',  ( -10.26315909542058336, 11.07603315418659840, -0.7216878364870267237 ) ) ;
#1728 = CARTESIAN_POINT ( 'NONE',  ( 6.299901696735699552, -0.7855725015378700604, 2.169893659913350259 ) ) ;
#1729 = CARTESIAN_POINT ( 'NONE',  ( 1.001543065824772753E-15, -3.521874999522041083, 3.793834371823811669 ) ) ;
#1730 = CARTESIAN_POINT ( 'NONE',  ( 4.873855640358407904, -1.924671727690111966, 0.3787619532854279436 ) ) ;
#1731 = CARTESIAN_POINT ( 'NONE',  ( 1.828750219146151323, 0.7691198443132395424, -1.864169014999479623 ) ) ;
#1732 = EDGE_LOOP ( 'NONE', ( #72750, #180023, #184227, #175031, #33412, #31755 ) ) ;
#1733 = CARTESIAN_POINT ( 'NONE',  ( 3.415340404243884187, -1.954662906411578804, 0.8143554997327147049 ) ) ;
#1734 = CARTESIAN_POINT ( 'NONE',  ( -0.7500000000000215383, 3.222916667349487341, 1.299038105676671107 ) ) ;
#1736 = CARTESIAN_POINT ( 'NONE',  ( -5.042743069279040036, 7.970618449879118828, 1.199719254218464037 ) ) ;
#1735 = DIRECTION ( 'NONE',  ( 0.000000000000000000, 1.000000000000000000, 0.000000000000000000 ) ) ;
#1737 = CARTESIAN_POINT ( 'NONE',  ( 3.908013947242465314, 1.300727540704300633, -1.303293010247716488 ) ) ;
#1738 = VERTEX_POINT ( 'NONE', #78731 ) ;
#1739 = CARTESIAN_POINT ( 'NONE',  ( -8.402302512167102222, 10.82577223566020841, -1.599625672291263179 ) ) ;
#1740 = CARTESIAN_POINT ( 'NONE',  ( 7.084367489069545069E-14, 8.210952333604106812, 2.038660652713624177 ) ) ;
#1742 = ADVANCED_FACE ( 'NONE', ( #112379 ), #212158, .T. ) ;
#1741 = CARTESIAN_POINT ( 'NONE',  ( 4.974906307097914926, -1.534222593358970821, 1.464151343314526121 ) ) ;
#1743 = DIRECTION ( 'NONE',  ( 0.000000000000000000, 0.000000000000000000, 1.000000000000000000 ) ) ;
#1744 = CARTESIAN_POINT ( 'NONE',  ( 5.438792177376376991, 9.497007973581119700, 1.040834085586084257E-14 ) ) ;
#1745 = CARTESIAN_POINT ( 'NONE',  ( 5.589157960464589792, 1.819533713976368094, -0.9674792931896135650 ) ) ;
#1748 = CARTESIAN_POINT ( 'NONE',  ( 2.718100415690410721, 1.734538518968967935, 0.6181264464550640936 ) ) ;
#1747 = CARTESIAN_POINT ( 'NONE',  ( 1.047037934171668905, 1.643801913826014482, -0.8725737860223039544 ) ) ;
#1746 = DIRECTION ( 'NONE',  ( 0.03984146075563027578, 0.000000000000000000, 0.9992060137953822085 ) ) ;
#1749 = CARTESIAN_POINT ( 'NONE',  ( 7.750457368506414646, 12.19395069656619945, 0.7998128361456462443 ) ) ;
#1750 = CARTESIAN_POINT ( 'NONE',  ( 1.082249783303695034, -6.507923190189534549E-15, 0.8432277037082082094 ) ) ;
#1751 =( BOUNDED_CURVE ( )  B_SPLINE_CURVE ( 3, ( #164109, #28773, #94855, #113290 ),
 .UNSPECIFIED., .F., .T. ) 
 B_SPLINE_CURVE_WITH_KNOTS ( ( 4, 4 ),
 ( 0.4999999999999988898, 1.000000000000000000 ),
 .UNSPECIFIED. ) 
 CURVE ( )  GEOMETRIC_REPRESENTATION_ITEM ( )  RATIONAL_B_SPLINE_CURVE ( ( 1.000000000000001998, 0.3333333333333334814, 0.3333333333333319826, 1.000000000000000444 ) ) 
 REPRESENTATION_ITEM ( '' )  );
#1752 = DIRECTION ( 'NONE',  ( 0.000000000000000000, 0.000000000000000000, 1.000000000000000000 ) ) ;
#1753 = DIRECTION ( 'NONE',  ( 0.000000000000000000, -1.084202172485501594E-14, -1.000000000000000000 ) ) ;
#1754 = CARTESIAN_POINT ( 'NONE',  ( 2.649284799151204073, -1.834272514977531632, 1.226802785254533568 ) ) ;
#1755 = CARTESIAN_POINT ( 'NONE',  ( 4.640055761359395348, 0.9730784542925293712, -2.042606338686814738 ) ) ;
#1756 = CARTESIAN_POINT ( 'NONE',  ( -6.724481002698120768, 9.828683022247721723, -1.082531754730538864 ) ) ;
#1757 = CARTESIAN_POINT ( 'NONE',  ( 4.658376882426285448, 1.807244876408566681, 0.1260263862136162261 ) ) ;
#1758 = CARTESIAN_POINT ( 'NONE',  ( 5.032410968829077014, 0.5625187028349203366, 1.831241071522809127 ) ) ;
#1759 = CARTESIAN_POINT ( 'NONE',  ( -1.201851678989727383E-14, 5.009375000341421469, -1.575800808251660134 ) ) ;
#1760 = CARTESIAN_POINT ( 'NONE',  ( 3.696128747971284323, -1.969148060776576337, -0.09815990810512796594 ) ) ;
#1761 = CARTESIAN_POINT ( 'NONE',  ( 5.330866702616011921, 0.1386157390740362649, 1.865562100978317206 ) ) ;
#1762 = CARTESIAN_POINT ( 'NONE',  ( 4.844130899818556379, -0.8777628995196519179, 1.641066814073613767 ) ) ;
#1763 = CARTESIAN_POINT ( 'NONE',  ( -6.735629246274043785E-15, -9.954379061088852509, 9.579665937614933569 ) ) ;
#1764 = AXIS2_PLACEMENT_3D ( 'NONE', #37629, #151395, #118947 ) ;
#1765 = CARTESIAN_POINT ( 'NONE',  ( 4.891328792415849058, 1.312644105602623457, 1.187316208720709421 ) ) ;
#1766 = CARTESIAN_POINT ( 'NONE',  ( 0.05782782957228919940, 1.164991625563294386, 1.645756161228327130 ) ) ;
#1768 = CARTESIAN_POINT ( 'NONE',  ( 1.489043601129129701, -0.3103829872296200443, -2.082944856911663312 ) ) ;
#1767 = CARTESIAN_POINT ( 'NONE',  ( -2.765500147063310266, 6.170241238308400433, 1.040834085586084257E-14 ) ) ;
#1769 = CIRCLE ( 'NONE', #174839, 0.5000000000000016653 ) ;
#1770 = CARTESIAN_POINT ( 'NONE',  ( 8.374132434735052755, 12.92157160716627295, -0.7998128361456352531 ) ) ;
#1772 = CARTESIAN_POINT ( 'NONE',  ( -1.127943160727153060, 2.800000000000024691, -0.7749999999999935829 ) ) ;
#1771 = CARTESIAN_POINT ( 'NONE',  ( -7.721398836998370818, -5.907420853759296264, 7.721398836998400128 ) ) ;
#1773 = CARTESIAN_POINT ( 'NONE',  ( 3.181995841446764839, 2.068044944583770306, -0.4684364081647199307 ) ) ;
#1774 =( NAMED_UNIT ( * ) PLANE_ANGLE_UNIT ( ) SI_UNIT ( $, .RADIAN. ) );
#1775 = CARTESIAN_POINT ( 'NONE',  ( 1.511979465466501527, -0.6765842426028411127, 1.903255196800458071 ) ) ;
#1776 = CARTESIAN_POINT ( 'NONE',  ( 1.364683531249988535, 2.113541667008087099, 0.7879004041258500513 ) ) ;
#1777 = CARTESIAN_POINT ( 'NONE',  ( 6.720655732516641834, 2.102516797890502165, 2.037305422295607293 ) ) ;
#1778 = CARTESIAN_POINT ( 'NONE',  ( 5.508690485854129903, 5.321227076451600091, 1.040834085586084257E-14 ) ) ;
#1779 = EDGE_LOOP ( 'NONE', ( #104681, #212819 ) ) ;
#1780 = CARTESIAN_POINT ( 'NONE',  ( 2.548304106926166490, 2.161049004374314464, 0.05582717182670697553 ) ) ;
#1781 = CARTESIAN_POINT ( 'NONE',  ( 6.620655732516649294, 0.5971256128398574337, 1.879834161342401666 ) ) ;
#1784 = DIRECTION ( 'NONE',  ( -1.665334536937734811E-16, 0.000000000000000000, -1.000000000000000000 ) ) ;
#1783 = CARTESIAN_POINT ( 'NONE',  ( 11.95359438121989726, 9.995781002913002311, -1.059536798430469107 ) ) ;
#1782 = CARTESIAN_POINT ( 'NONE',  ( 5.435893244436359240, 5.306573304789342416, -0.7998128361456481317 ) ) ;
#1785 = DIRECTION ( 'NONE',  ( 0.9999455182791219254, 0.000000000000000000, -0.01043841336116897722 ) ) ;
#1786 = DIRECTION ( 'NONE',  ( -5.578564026256490882E-16, -1.000000000000000000, -9.066213480720158442E-32 ) ) ;
#1787 = CARTESIAN_POINT ( 'NONE',  ( -5.897433632264490910, 9.824163637709826702, 0.000000000000000000 ) ) ;
#1788 = CARTESIAN_POINT ( 'NONE',  ( 0.6795420635867071013, 1.475991390215245058, 1.620154534501851096 ) ) ;
#1789 = CARTESIAN_POINT ( 'NONE',  ( -0.004619473214107579565, 7.151453204069600389, 1.999995854215794511 ) ) ;
#1791 = CARTESIAN_POINT ( 'NONE',  ( -1.364683531250000748, 11.85937500034139802, 0.000000000000000000 ) ) ;
#1790 = CARTESIAN_POINT ( 'NONE',  ( 1.692605830730309791, -2.251738780704269249, -0.2206997258237669290 ) ) ;
#1792 = CARTESIAN_POINT ( 'NONE',  ( -8.320953590485107298, 10.73086516036454618, 1.599625672291269396 ) ) ;
#1793 = CARTESIAN_POINT ( 'NONE',  ( -3.565431210269599749, 7.103494145382415859, 0.7216878364870317197 ) ) ;
#1794 = CARTESIAN_POINT ( 'NONE',  ( 0.6823417656249899377, 2.655208333674753618, 1.181850606188767472 ) ) ;
#1795 = CARTESIAN_POINT ( 'NONE',  ( 4.599920620972065777, 8.367456947080912144, 0.1478172174028801744 ) ) ;
#1796 = CARTESIAN_POINT ( 'NONE',  ( 1.499999999999993117, 10.60416666666666607, 0.8660254037844409281 ) ) ;
#1797 = CARTESIAN_POINT ( 'NONE',  ( 4.125434265850294047, -1.649698657028845883, 0.5036723037128154612 ) ) ;
#1798 = CARTESIAN_POINT ( 'NONE',  ( 6.536439455564150514, 9.679577560583279450, 1.082531754730549078 ) ) ;
#1799 = CARTESIAN_POINT ( 'NONE',  ( 2.706023412207391843, -0.6731984680253579878, -1.636901589742848051 ) ) ;
#1800 = CARTESIAN_POINT ( 'NONE',  ( 5.579209114504255496, -0.04897750150410771358, -2.206396493298476980 ) ) ;
#1801 = VERTEX_POINT ( 'NONE', #63560 ) ;
#1802 = CARTESIAN_POINT ( 'NONE',  ( -6.608673532018475960, 6.674816973635147477, -0.7998128361456362523 ) ) ;
#1803 = CARTESIAN_POINT ( 'NONE',  ( 5.554314605481814660, -1.277030258849481736, 1.560512323070535112 ) ) ;
#1804 = ORIENTED_EDGE ( 'NONE', *, *, #177588, .F. ) ;
#1805 = CARTESIAN_POINT ( 'NONE',  ( 2.412791964582483129, 1.669947582624079274, 0.8431454209596804805 ) ) ;
#1806 = CARTESIAN_POINT ( 'NONE',  ( 2.166927730644189420, 1.536898783757352005, -1.387270004372019416 ) ) ;
#1807 = CARTESIAN_POINT ( 'NONE',  ( -7.878696662872776812, 8.364436659539265406, -0.7216878364870338292 ) ) ;
#1808 = CARTESIAN_POINT ( 'NONE',  ( 1.951281838316549777, -1.706683157587106425, 0.8630329916254894096 ) ) ;
#1809 = CARTESIAN_POINT ( 'NONE',  ( 1.499999999999996891, 9.645833333333333925, -0.8660254037844378194 ) ) ;
#1810 = CARTESIAN_POINT ( 'NONE',  ( -11.75342398721120141, 4.618418902329548992, -5.022351803590792585 ) ) ;
#1811 = CARTESIAN_POINT ( 'NONE',  ( -7.636191794455529092, -6.027819618361862197, 7.636191794455553961 ) ) ;
#1812 = CARTESIAN_POINT ( 'NONE',  ( 0.6823417656249917140, 4.655208333674755394, 1.181850606188765695 ) ) ;
#1813 = CARTESIAN_POINT ( 'NONE',  ( 6.411931881972196610E-05, -0.8997486769052507327, 1.687471195204979457 ) ) ;
#1814 = AXIS2_PLACEMENT_3D ( 'NONE', #77579, #34949, #33893 ) ;
#1815 = CARTESIAN_POINT ( 'NONE',  ( 6.102578539926878598, 7.252668063737060855, -1.082531754730548412 ) ) ;
#1816 = CARTESIAN_POINT ( 'NONE',  ( 1.398799877119625501, 0.3793605821263335565, 1.924665094374561791 ) ) ;
#1817 = CARTESIAN_POINT ( 'NONE',  ( 0.3333609138582178111, -1.319029705771988858, 1.524807370920200356 ) ) ;
#1818 = CARTESIAN_POINT ( 'NONE',  ( -6.296835998904160014, 6.311006518335105397, 0.000000000000000000 ) ) ;
#1819 = CARTESIAN_POINT ( 'NONE',  ( 5.783468009189684622, 0.1541500780414573613, -2.115021274163720211 ) ) ;
#1821 =( NAMED_UNIT ( * ) PLANE_ANGLE_UNIT ( ) SI_UNIT ( $, .RADIAN. ) );
#1820 = CARTESIAN_POINT ( 'NONE',  ( 9.260382613333817403, 10.76253345609967660, -1.199719254218446718 ) ) ;
#1822 = CARTESIAN_POINT ( 'NONE',  ( 6.134049847598044281, 0.9739642658876453973, -1.713909437456696105 ) ) ;
#1823 = CARTESIAN_POINT ( 'NONE',  ( 0.6823417656249899377, 2.092708333674753174, 1.181850606188767472 ) ) ;
#1824 = CARTESIAN_POINT ( 'NONE',  ( 1.459241111239812705, -1.698469834904120290, 1.080578982646386743 ) ) ;
#1825 = ORIENTED_EDGE ( 'NONE', *, *, #25480, .F. ) ;
#1827 = CARTESIAN_POINT ( 'NONE',  ( 1.318125747981816698, 1.040119728068724880, -1.844044674895953806 ) ) ;
#1826 = CARTESIAN_POINT ( 'NONE',  ( -8.541273586929371220, 9.067166727613487964, 0.7216878364870438212 ) ) ;
#1828 = CARTESIAN_POINT ( 'NONE',  ( 11.09870862492791233, 7.996335997987229049, -4.583701278145491109 ) ) ;
#1829 = CARTESIAN_POINT ( 'NONE',  ( 2.137250951388528275, -0.09934309608320915363, -2.068088366144354318 ) ) ;
#1830 = CARTESIAN_POINT ( 'NONE',  ( 3.705121118284530279, 7.544668081299086282, -1.734723475976807094E-15 ) ) ;
#1831 = CARTESIAN_POINT ( 'NONE',  ( 3.549202351727371862, 7.362762853649070571, -0.7998128361456362523 ) ) ;
#1832 = ORIENTED_EDGE ( 'NONE', *, *, #152899, .F. ) ;
#1834 = CARTESIAN_POINT ( 'NONE',  ( 5.138703914779377158, 5.953908307786102583, 1.199719254218462483 ) ) ;
#1833 = CARTESIAN_POINT ( 'NONE',  ( 4.189459526602421491, -0.8002100119003925371, 1.931633446273020693 ) ) ;
#1837 = ORIENTED_EDGE ( 'NONE', *, *, #166482, .F. ) ;
#1836 = CARTESIAN_POINT ( 'NONE',  ( 2.314858244453772862, 1.454059926310177220, -1.080092325806664144 ) ) ;
#1835 = CARTESIAN_POINT ( 'NONE',  ( 3.786012796616508247, -0.9002957760516903107, 1.588078298607284111 ) ) ;
#1838 = CARTESIAN_POINT ( 'NONE',  ( 9.490416961614043245, -9.037429132956701139, -0.4317745627846678591 ) ) ;
#1839 = CARTESIAN_POINT ( 'NONE',  ( -0.7500000000000006661, 2.858333333333358706, -1.299038105676652011 ) ) ;
#1840 = CARTESIAN_POINT ( 'NONE',  ( 10.48872307347595090, 11.88768493876267485, 6.438521854865753014 ) ) ;
#1841 = CARTESIAN_POINT ( 'NONE',  ( 5.614374367772542840, -0.9875226594672005254, -1.973556357105679337 ) ) ;
#1842 = CARTESIAN_POINT ( 'NONE',  ( -0.6823417656250039265, 8.880208333674733723, -1.181850606188755259 ) ) ;
#1843 = ORIENTED_EDGE ( 'NONE', *, *, #58178, .F. ) ;
#1844 = CARTESIAN_POINT ( 'NONE',  ( 3.633378786761193968, -0.1378984027537045187, 1.907353237798288470 ) ) ;
#1845 = CARTESIAN_POINT ( 'NONE',  ( -3.490334480514268645, 6.159475096320226939, -1.199719254218452935 ) ) ;
#1846 = CARTESIAN_POINT ( 'NONE',  ( 8.132193210098487057, 8.381980254736715708, 1.040834085586084257E-14 ) ) ;
#1847 = CARTESIAN_POINT ( 'NONE',  ( -5.558564015327488080E-14, 0.6093750003414449834, -1.570758158831798257 ) ) ;
#1848 = CARTESIAN_POINT ( 'NONE',  ( 5.151735183068521629, 5.112705256442466428, 1.040834085586084257E-14 ) ) ;
#1849 = CARTESIAN_POINT ( 'NONE',  ( -11.88235317400313917, 12.34335760226970358, 0.9089793033029930358 ) ) ;
#1850 = CARTESIAN_POINT ( 'NONE',  ( 0.8371598888798935656, 0.7463826720714298313, -1.683355135116318069 ) ) ;
#1851 = LINE ( 'NONE', #51717, #123874 ) ;
#1852 = EDGE_CURVE ( 'NONE', #197886, #149924, #212986, .T. ) ;
#1853 = CARTESIAN_POINT ( 'NONE',  ( 3.954256261376987602, 0.6707706173689140794, 1.746330409709492937 ) ) ;
#1854 = CARTESIAN_POINT ( 'NONE',  ( 8.018721507839716267, 8.319872945426633137, -0.7998128361456341429 ) ) ;
#1855 = CARTESIAN_POINT ( 'NONE',  ( -1.500000000000015099, 12.51041666734946389, -0.8660254037844309360 ) ) ;
#1856 = STYLED_ITEM ( 'NONE', ( #32642 ), #1037 ) ;
#1857 = CARTESIAN_POINT ( 'NONE',  ( -6.209271165378811297, 10.18797409300986878, 0.7216878364870458196 ) ) ;
#1858 = CARTESIAN_POINT ( 'NONE',  ( 4.635998460869027227, 7.496083073400806818, -1.199719254218452047 ) ) ;
#1859 = CARTESIAN_POINT ( 'NONE',  ( 6.385608392048681026, -1.951384585020640383, 0.6918703269920488674 ) ) ;
#1860 = CARTESIAN_POINT ( 'NONE',  ( 2.583611426500437069, -0.6298568260672477992, 1.915607262459443794 ) ) ;
#1861 = CARTESIAN_POINT ( 'NONE',  ( -6.984421689334302741, 11.30024240419870374, 0.000000000000000000 ) ) ;
#1862 = CARTESIAN_POINT ( 'NONE',  ( 6.313256805818848960, 7.394496357324014113, 1.199719254218452047 ) ) ;
#1863 = CARTESIAN_POINT ( 'NONE',  ( 2.343918204863020271, 2.190988169473460090, 0.05230688499441307066 ) ) ;
#1864 = CARTESIAN_POINT ( 'NONE',  ( 6.094357461763900474, -1.817385979143220087, -0.1739998769475573914 ) ) ;
#1865 = CARTESIAN_POINT ( 'NONE',  ( -2.937312835655025101, 6.578615408239493867, 1.040834085586084257E-14 ) ) ;
#1866 = EDGE_CURVE ( 'NONE', #136049, #106, #60036, .T. ) ;
#1867 = CARTESIAN_POINT ( 'NONE',  ( 3.906157654512984134, 7.571284673658201569, -0.7216878364870338292 ) ) ;
#1868 = CARTESIAN_POINT ( 'NONE',  ( 8.829384350997564468, 11.32403438096243775, 1.599625672291281386 ) ) ;
#1869 = CARTESIAN_POINT ( 'NONE',  ( 3.246287715468270108, 5.874753870433235825, 1.199719254218450271 ) ) ;
#1870 = CARTESIAN_POINT ( 'NONE',  ( 6.292392690518195941, 8.434487120394948079, -1.443375672974078761 ) ) ;
#1871 = VERTEX_POINT ( 'NONE', #114513 ) ;
#1873 = CARTESIAN_POINT ( 'NONE',  ( 1.172521868268823875, 0.8179054604866965450, 1.839630344048637678 ) ) ;
#1872 = CARTESIAN_POINT ( 'NONE',  ( 3.579498943475650563, -0.9044721095569520086, 1.603693017070174864 ) ) ;
#1874 = CARTESIAN_POINT ( 'NONE',  ( 2.618911895557019420, 0.6142130902007210125, -2.214721005821191024 ) ) ;
#1876 = CARTESIAN_POINT ( 'NONE',  ( 1.481066496106745234, -0.05241980694788496431, 1.860401082089859770 ) ) ;
#1875 = DIRECTION ( 'NONE',  ( -0.000000000000000000, 1.000000000000000000, -0.000000000000000000 ) ) ;
#1877 = CARTESIAN_POINT ( 'NONE',  ( 3.285556943750000514, -3.813541666188710710, 1.896917185911906500 ) ) ;
#1878 = CARTESIAN_POINT ( 'NONE',  ( -5.766295404513795297, 5.621766148221195358, 0.7998128361456341429 ) ) ;
#1879 = CARTESIAN_POINT ( 'NONE',  ( -1.364683531249997417, 5.759375000341418804, 1.214306433183764966E-14 ) ) ;
#1880 = CARTESIAN_POINT ( 'NONE',  ( 4.552931727387078631, 0.3324577288378940954, 1.883125075537089854 ) ) ;
#1881 = CARTESIAN_POINT ( 'NONE',  ( -8.402302512167102222, 10.82577223566020841, -1.599625672291263179 ) ) ;
#1882 = CARTESIAN_POINT ( 'NONE',  ( 6.157602363183391603, 6.969851231138187941, -0.9158007892692658913 ) ) ;
#1883 = CARTESIAN_POINT ( 'NONE',  ( -7.621091744657483069, 8.063897588288083895, 0.7216878364870317197 ) ) ;
#1885 = CARTESIAN_POINT ( 'NONE',  ( 2.201827603038747139, -1.870314503716500099, 0.04339327950253490246 ) ) ;
#1884 = CARTESIAN_POINT ( 'NONE',  ( 3.667594231577479658, 1.163246697351211223, 1.737046641446901463 ) ) ;
#1886 = CARTESIAN_POINT ( 'NONE',  ( 8.432808358020029260, 8.940623960552603222, 0.7216878364870438212 ) ) ;
#1887 = CARTESIAN_POINT ( 'NONE',  ( 9.797921721691059460, 3.956598013261175772, 6.103348209225848642 ) ) ;
#1888 = CARTESIAN_POINT ( 'NONE',  ( 3.069568678616676927, -1.034394858748697743, 1.399543075413912430 ) ) ;
#1889 = CARTESIAN_POINT ( 'NONE',  ( 3.499976210622149253, 7.235056012367825140, 0.7998128361456321445 ) ) ;
#1891 = CARTESIAN_POINT ( 'NONE',  ( 5.691725559638619814, 5.534767995866836543, 1.040834085586084257E-14 ) ) ;
#1890 = CARTESIAN_POINT ( 'NONE',  ( 5.969672231941198781, 6.017005441543672895, -0.3686804784870336693 ) ) ;
#1892 = CARTESIAN_POINT ( 'NONE',  ( 4.142953665201137170, -1.499297852604332348, 0.8526725997853346062 ) ) ;
#1893 = CARTESIAN_POINT ( 'NONE',  ( -5.540478329478883524, 9.615641817700700145, 0.000000000000000000 ) ) ;
#1894 = CARTESIAN_POINT ( 'NONE',  ( 6.498651167236064730, -0.5841124237929047336, -2.128106146270396071 ) ) ;
#1895 = CARTESIAN_POINT ( 'NONE',  ( 0.000000000000000000, 3.553052365627050513, 0.000000000000000000 ) ) ;
#1896 = SURFACE_STYLE_FILL_AREA ( #165491 ) ;
#1897 = CARTESIAN_POINT ( 'NONE',  ( 3.116274269780743733, 2.161009848182334991, -0.2084346501036362376 ) ) ;
#1898 = CARTESIAN_POINT ( 'NONE',  ( 3.773894676421325478, 1.015518775504126614, 1.516979517045339509 ) ) ;
#1899 = CARTESIAN_POINT ( 'NONE',  ( 0.2682999959267086676, -0.8333247372044672030, -1.774235371720728649 ) ) ;
#1900 = CARTESIAN_POINT ( 'NONE',  ( 5.665271214873143890, 1.955333520279872506, -0.8127364881663766694 ) ) ;
#1901 = EDGE_CURVE ( 'NONE', #91287, #146442, #53074, .T. ) ;
#1902 = ORIENTED_EDGE ( 'NONE', *, *, #91274, .F. ) ;
#1904 = CARTESIAN_POINT ( 'NONE',  ( -1.402160292154681736E-14, 2.009375000341422801, -1.575800808251660134 ) ) ;
#1903 = CARTESIAN_POINT ( 'NONE',  ( 5.671479170183292950, 1.362789248821870025, 1.843150307845689229 ) ) ;
#1905 = CARTESIAN_POINT ( 'NONE',  ( 7.879259827836241570, 12.34422023245099176, 1.040834085586084257E-14 ) ) ;
#1906 = CARTESIAN_POINT ( 'NONE',  ( 1.084817099560590803, -1.342388549496125627, 1.641497191572589776 ) ) ;
#1907 = CARTESIAN_POINT ( 'NONE',  ( -5.436456409399874623, 5.444880020495701523, 0.000000000000000000 ) ) ;
#1908 =( GEOMETRIC_REPRESENTATION_CONTEXT ( 3 ) GLOBAL_UNCERTAINTY_ASSIGNED_CONTEXT ( ( #209237 ) ) GLOBAL_UNIT_ASSIGNED_CONTEXT ( ( #94356, #65005, #80205 ) ) REPRESENTATION_CONTEXT ( 'NONE', 'WORKASPACE' ) );
#1909 = CARTESIAN_POINT ( 'NONE',  ( 4.202664430556261266, 4.005456045178151570, 0.7216878364870317197 ) ) ;
#1910 = CARTESIAN_POINT ( 'NONE',  ( -5.463572716182839351, 7.397254140345190798, 1.443375672974064550 ) ) ;
#1911 = CARTESIAN_POINT ( 'NONE',  ( 6.174718801439761151, 1.464035886807094844, -1.603313688547292726 ) ) ;
#1913 = CARTESIAN_POINT ( 'NONE',  ( -6.009258394948636914E-15, 13.21875000068279427, -1.732050807568875195 ) ) ;
#1912 = FACE_OUTER_BOUND ( 'NONE', #168026, .T. ) ;
#1916 = ORIENTED_EDGE ( 'NONE', *, *, #31157, .F. ) ;
#1915 = CARTESIAN_POINT ( 'NONE',  ( 1.155278206730834256, 0.4382352071879510036, 2.177490050429623736 ) ) ;
#1914 = AXIS2_PLACEMENT_3D ( 'NONE', #35016, #51290, #50222 ) ;
#1917 = CARTESIAN_POINT ( 'NONE',  ( 5.924453975591452703, -1.462443569488897754, -1.388487997949397368 ) ) ;
#1919 = CARTESIAN_POINT ( 'NONE',  ( 3.995030872118944032, 0.2978362323166737213, 2.040820773513659425 ) ) ;
#1918 = CARTESIAN_POINT ( 'NONE',  ( 5.671388329218120639, 5.511041227042920099, 1.040834085586084257E-14 ) ) ;
#1921 = CARTESIAN_POINT ( 'NONE',  ( -3.475000000000000533, -3.879166666666665986, -2.006292185433948827 ) ) ;
#1920 = CARTESIAN_POINT ( 'NONE',  ( 6.638652492546827766, 7.774124658506663010, 1.199719254218452047 ) ) ;
#1922 = EDGE_CURVE ( 'NONE', #174777, #97759, #198409, .T. ) ;
#1923 = CARTESIAN_POINT ( 'NONE',  ( 6.526270840131753737, 8.707344961610770540, -1.599625672291283607 ) ) ;
#1924 = CARTESIAN_POINT ( 'NONE',  ( 1.642778471875001811, -1.392708332855374653, 2.845375778867859751 ) ) ;
#1925 = CARTESIAN_POINT ( 'NONE',  ( 0.5157159539815784344, -1.120044586405210207, -1.765097889335610404 ) ) ;
#1926 = CARTESIAN_POINT ( 'NONE',  ( 4.342422763466713853, 0.4390309838058319425, -1.967887491402267486 ) ) ;
#1927 = CARTESIAN_POINT ( 'NONE',  ( 3.931074656914943954, -1.272613488525012659, -1.330884258478791438 ) ) ;
#1928 = EDGE_CURVE ( 'NONE', #32900, #45587, #28933, .T. ) ;
#1929 = CARTESIAN_POINT ( 'NONE',  ( 3.683011284406639607, 7.448596931783069586, 0.7998128361456321445 ) ) ;
#1930 = CARTESIAN_POINT ( 'NONE',  ( 0.3930057192131968802, 1.272852841813755687, 1.164116782529129868 ) ) ;
#1931 = CARTESIAN_POINT ( 'NONE',  ( 0.3618152180564599973, -5.223163831703878657, 10.97113184882214298 ) ) ;
#1932 =( BOUNDED_CURVE ( )  B_SPLINE_CURVE ( 2, ( #75134, #139079, #40511, #104435, #26365, #138007, #141242 ),
 .UNSPECIFIED., .F., .T. ) 
 B_SPLINE_CURVE_WITH_KNOTS ( ( 3, 2, 2, 3 ),
 ( 0.1874999999999999722, 0.1916666666666665964, 0.1958333333333332205, 0.1999999999999998446 ),
 .UNSPECIFIED. ) 
 CURVE ( )  GEOMETRIC_REPRESENTATION_ITEM ( )  RATIONAL_B_SPLINE_CURVE ( ( 1.000000000000000888, 0.8660254037844378194, 1.000000000000000000, 0.8660254037844387076, 1.000000000000000000, 0.8660254037844440367, 0.9999999999999946709 ) ) 
 REPRESENTATION_ITEM ( '' )  );
#1933 = CARTESIAN_POINT ( 'NONE',  ( -5.494078562035765501, 7.432844293840273231, -1.599625672291256295 ) ) ;
#1934 = CARTESIAN_POINT ( 'NONE',  ( 0.8610526709191126393, -1.638059776709074322, 1.560773681941391100 ) ) ;
#1935 = CARTESIAN_POINT ( 'NONE',  ( 3.141344390434357869, -1.857286833677756599, 0.9929794709265575836 ) ) ;
#1936 = CARTESIAN_POINT ( 'NONE',  ( -5.093022980588950865, 5.970890227889075419, -1.199719254218453823 ) ) ;
#1937 = CARTESIAN_POINT ( 'NONE',  ( 6.908042961362778733, 8.018137195466769285, 1.199719254218462483 ) ) ;
#1938 = CARTESIAN_POINT ( 'NONE',  ( 4.868786560638885597, 7.733982516503781213, 1.082531754730548412 ) ) ;
#1939 = CARTESIAN_POINT ( 'NONE',  ( 6.093750000000004441, -1.895863743164213355, -0.7852924748296624680 ) ) ;
#1940 = CARTESIAN_POINT ( 'NONE',  ( -5.925076824372040640, 6.871343368977510302, 1.199719254218450271 ) ) ;
#1941 = CARTESIAN_POINT ( 'NONE',  ( -1.201851678989727383E-14, 2.837500000000024780, -1.732050807568863648 ) ) ;
#1942 = CARTESIAN_POINT ( 'NONE',  ( -3.276266675996675204, 6.974061555304760240, -0.7998128361456281477 ) ) ;
#1943 = CARTESIAN_POINT ( 'NONE',  ( 5.221006152755099272, 1.681885564164938840, -1.451226649161361015 ) ) ;
#1944 = CARTESIAN_POINT ( 'NONE',  ( 3.732539452256115275, 0.3211115598316104935, 2.167677955659273348 ) ) ;
#1945 = CARTESIAN_POINT ( 'NONE',  ( -4.574986769607567894, 7.424902766929059261, 1.199719254218464037 ) ) ;
#1946 = CARTESIAN_POINT ( 'NONE',  ( -4.496464221587651799, 5.274905009054215554, 1.199719254218452935 ) ) ;
#1947 = CARTESIAN_POINT ( 'NONE',  ( -1.364683531250012516, 2.780208333674754506, 0.7879004041258379498 ) ) ;
#1948 = CARTESIAN_POINT ( 'NONE',  ( 6.609999999999985221, 3.681232580627872952, 2.794007784547379192 ) ) ;
#1950 = CARTESIAN_POINT ( 'NONE',  ( -6.236387472606166327, 6.378132927569716060, -0.7216878364870278340 ) ) ;
#1949 = VECTOR ( 'NONE', #166204, 1000.000000000000000 ) ;
#1951 = CARTESIAN_POINT ( 'NONE',  ( 4.887034483293543730, -1.997634423138573867, -0.7120497732875651353 ) ) ;
#1952 = CARTESIAN_POINT ( 'NONE',  ( -7.770231434407805615, 8.237893892996801526, 0.000000000000000000 ) ) ;
#1953 = EDGE_LOOP ( 'NONE', ( #157859, #138577, #171255, #137292, #164830, #143916, #204873, #56553, #39831, #143622, #110813, #20199, #67902, #39672 ) ) ;
#1955 = CARTESIAN_POINT ( 'NONE',  ( 6.121977807712331909, -1.196819783530624015, -1.799967629666970881 ) ) ;
#1954 = CARTESIAN_POINT ( 'NONE',  ( -4.665414256878287702, 8.457084043084382330, -0.7216878364870338292 ) ) ;
#1956 = CARTESIAN_POINT ( 'NONE',  ( 3.818592820543298405, 7.606775390609172405, -0.7998128361456221525 ) ) ;
#1957 = CARTESIAN_POINT ( 'NONE',  ( 6.321814700078944860, 1.054209175812788502, -1.509406368332133930 ) ) ;
#1958 = CARTESIAN_POINT ( 'NONE',  ( 0.6823417656249899377, 2.655208333674753618, 1.181850606188767472 ) ) ;
#1959 = CARTESIAN_POINT ( 'NONE',  ( 1.030331162470259354, -1.574104619921200765, 0.7428470239391560259 ) ) ;
#1960 = CARTESIAN_POINT ( 'NONE',  ( -0.4153311931458959494, 3.850000000000006306, 0.5000000000000064393 ) ) ;
#1961 = CARTESIAN_POINT ( 'NONE',  ( 0.6823417656249864960, -1.011458332991911568, -1.181850606188749264 ) ) ;
#1962 = CYLINDRICAL_SURFACE ( 'NONE', #101371, 2.000000000000000000 ) ;
#1963 = CARTESIAN_POINT ( 'NONE',  ( 5.049776242366147194, 0.6816224847111511664, -2.051488706027407183 ) ) ;
#1964 = CARTESIAN_POINT ( 'NONE',  ( -4.406563619641430840, 5.099744630125142564, -1.199719254218446718 ) ) ;
#1965 = CARTESIAN_POINT ( 'NONE',  ( -7.551528372687420720, 8.872833191965849409, 1.082531754730558626 ) ) ;
#1966 = CARTESIAN_POINT ( 'NONE',  ( 4.557600102482579629, 0.4766696971462945909, -2.108333899287537339 ) ) ;
#1967 = CARTESIAN_POINT ( 'NONE',  ( -1.364683531250012516, 2.488541667008088876, -0.7879004041258289570 ) ) ;
#1968 = CARTESIAN_POINT ( 'NONE',  ( 6.485619883616900339, 1.357675630217811014, 1.429558606944077326 ) ) ;
#1969 = CARTESIAN_POINT ( 'NONE',  ( 4.604694260812782325, 0.7408162341489711311, -1.567766963475358599 ) ) ;
#1971 = CARTESIAN_POINT ( 'NONE',  ( 1.575987392057216940, -1.168677030305173004, 1.853764812240476623 ) ) ;
#1970 = CARTESIAN_POINT ( 'NONE',  ( 0.6801582343749952297, -0.1927083329918907739, -1.178068619123876282 ) ) ;
#1972 = CARTESIAN_POINT ( 'NONE',  ( 2.345130104517737291, 0.5056967325399002178, 2.251352274652190122 ) ) ;
#1973 = CARTESIAN_POINT ( 'NONE',  ( 4.323548078123999439, -1.973147536489193499, 0.5946332991794788247 ) ) ;
#1974 = CARTESIAN_POINT ( 'NONE',  ( 6.480031042553710208, -1.905489079494159910, -0.3742900760800580984 ) ) ;
#1975 = CARTESIAN_POINT ( 'NONE',  ( -7.009202228140751778, 9.200488570962775725, -1.443375672974058777 ) ) ;
#1976 = CIRCLE ( 'NONE', #22858, 0.07999999999999946043 ) ;
#1977 = CARTESIAN_POINT ( 'NONE',  ( -3.630551273409382329, 7.457669928944732796, 0.7998128361456352531 ) ) ;
#1978 = DIRECTION ( 'NONE',  ( -0.9988044021632737079, 2.913101175831703182E-16, 0.04888523518676889112 ) ) ;
#1979 = DIRECTION ( 'NONE',  ( 0.7592566023653005702, -0.6507913734559639396, 0.000000000000000000 ) ) ;
#1980 = CARTESIAN_POINT ( 'NONE',  ( 1.776017750421728270, 1.753029812786778940, -0.9963028777105964462 ) ) ;
#1981 = CARTESIAN_POINT ( 'NONE',  ( -5.192409643909507544, 9.001635651295671892, 0.7216878364870458196 ) ) ;
#1982 = CARTESIAN_POINT ( 'NONE',  ( 3.926972183325681875, 2.094573593246536802, 0.6948772193901550098 ) ) ;
#1983 = CARTESIAN_POINT ( 'NONE',  ( 1.642778471875001811, -1.130208332855375808, 2.845375778867859751 ) ) ;
#1984 = CARTESIAN_POINT ( 'NONE',  ( 1.815070623055618615, -1.592837743320011601, -0.9620759905232498799 ) ) ;
#1985 = FACE_OUTER_BOUND ( 'NONE', #56986, .T. ) ;
#1986 = CARTESIAN_POINT ( 'NONE',  ( 1.836970198721030181E-16, 7.500000000000000000, 1.500000000000000222 ) ) ;
#1987 = DIRECTION ( 'NONE',  ( 0.000000000000000000, 0.000000000000000000, -1.000000000000000000 ) ) ;
#1989 = CARTESIAN_POINT ( 'NONE',  ( 6.925078400183531713, 7.629137130509035636, 2.644348168701659674 ) ) ;
#1988 = CARTESIAN_POINT ( 'NONE',  ( -4.839158742459761520, 8.201312040681516535, -0.9517655008395020655 ) ) ;
#1990 = CYLINDRICAL_SURFACE ( 'NONE', #71546, 1.250000000000000000 ) ;
#1991 = ORIENTED_EDGE ( 'NONE', *, *, #214118, .F. ) ;
#1992 = CARTESIAN_POINT ( 'NONE',  ( 3.836836124264888959, 0.3005266716369097701, 2.038723765318616099 ) ) ;
#1993 = CARTESIAN_POINT ( 'NONE',  ( 1.360316468749985575, 2.036458333674739940, -0.7853790794159022370 ) ) ;
#1994 = CARTESIAN_POINT ( 'NONE',  ( -5.904739593951539689, 6.847616600153594746, 1.199719254218450271 ) ) ;
#1995 = CARTESIAN_POINT ( 'NONE',  ( 2.244791279253912197, 1.959548689066059168, 0.4886446307589187854 ) ) ;
#1996 = CARTESIAN_POINT ( 'NONE',  ( -1.500000000000001332, -0.5999999999999755529, 0.000000000000000000 ) ) ;
#1997 = CARTESIAN_POINT ( 'NONE',  ( 2.523789150438203510, 6.096171108819874007, 0.7998128361456462443 ) ) ;
#1998 = CARTESIAN_POINT ( 'NONE',  ( 1.991158371866567967, 1.793705239296649045, -1.014668517943543513 ) ) ;
#2000 = CARTESIAN_POINT ( 'NONE',  ( 1.364683531249996529, 13.71354166700806765, 0.7879004041258405033 ) ) ;
#1999 = DIRECTION ( 'NONE',  ( 0.000000000000000000, 1.000000000000000000, 0.000000000000000000 ) ) ;
#2001 = CARTESIAN_POINT ( 'NONE',  ( 6.765682348419287173, 7.852049813699357728, 1.199719254218462483 ) ) ;
#2002 = CARTESIAN_POINT ( 'NONE',  ( -0.1409997244345879974, 6.947781918643359589, -2.595319453918026653 ) ) ;
#2003 = CARTESIAN_POINT ( 'NONE',  ( 0.3218710511002781383, 1.760991339961643920, 0.5373333866721883290 ) ) ;
#2004 = CARTESIAN_POINT ( 'NONE',  ( 5.725267921653402148, -0.05769419298589681389, 2.206291853148376170 ) ) ;
#2005 = CARTESIAN_POINT ( 'NONE',  ( 6.873057527484919937, 6.983264968346048818, 0.7998128361456352531 ) ) ;
#2006 = CARTESIAN_POINT ( 'NONE',  ( 1.616726252867954683, 1.452999108549270169, -1.600537328674697779 ) ) ;
#2007 = CARTESIAN_POINT ( 'NONE',  ( -3.443407828190963915, 6.961133532957338943, 0.7216878364870317197 ) ) ;
#2008 = CARTESIAN_POINT ( 'NONE',  ( 2.272673044126482189, -0.3494851828299732621, -1.985868527484459634 ) ) ;
#2009 = CARTESIAN_POINT ( 'NONE',  ( 2.302535375473542700, -2.053259096611260937, 1.032894330136547856 ) ) ;
#2010 = CARTESIAN_POINT ( 'NONE',  ( 0.000000000000000000, 18.91999999999999815, 0.000000000000000000 ) ) ;
#2011 = CARTESIAN_POINT ( 'NONE',  ( 0.4966798268824790252, 1.557709316500059726, -1.035497600327957235 ) ) ;
#2012 = CARTESIAN_POINT ( 'NONE',  ( 4.715676653857135747, -1.933614719187324082, 0.3836508851736331605 ) ) ;
#2013 = CARTESIAN_POINT ( 'NONE',  ( 3.837125247982266174, -1.679222704393277921, -1.116210984008485507 ) ) ;
#2015 = CARTESIAN_POINT ( 'NONE',  ( 9.368320956918608999, 11.95279375453699622, 1.443375672974076540 ) ) ;
#2014 = CARTESIAN_POINT ( 'NONE',  ( 0.6823417656249899377, 2.592708333674753618, 1.181850606188767472 ) ) ;
#2017 = CARTESIAN_POINT ( 'NONE',  ( 4.723321587070372196, -0.1039652108096918437, 2.103624988570974352 ) ) ;
#2016 = CARTESIAN_POINT ( 'NONE',  ( -7.015454420067433361, 10.27211502579893754, 1.199719254218453823 ) ) ;
#2018 = CARTESIAN_POINT ( 'NONE',  ( 5.846161131210033446, -0.9342735719010831774, 1.847668428805064655 ) ) ;
#2019 = CARTESIAN_POINT ( 'NONE',  ( 7.308008492965924141, 8.484763649003774333, -1.199719254218451159 ) ) ;
#2020 = CARTESIAN_POINT ( 'NONE',  ( -5.703176172842872482, 9.805455968292021041, 0.000000000000000000 ) ) ;
#2021 = CARTESIAN_POINT ( 'NONE',  ( -1.445184293213162663, 8.696352241143832984, 2.614796098495217436 ) ) ;
#2022 = CARTESIAN_POINT ( 'NONE',  ( 5.273696820376614802, 0.3899264243738297941, -1.981607871481812833 ) ) ;
#2023 = CARTESIAN_POINT ( 'NONE',  ( 0.7499999999999885647, -1.235416665983847473, 1.299038105676657340 ) ) ;
#2024 = CARTESIAN_POINT ( 'NONE',  ( 0.7431262955939599291, -0.2488486719821168813, -2.047412193126110225 ) ) ;
#2025 = CARTESIAN_POINT ( 'NONE',  ( 6.792271770766432404, 10.86814146596211472, 1.040834085586084257E-14 ) ) ;
#2026 = CARTESIAN_POINT ( 'NONE',  ( 7.191674137406095291, 7.354984346587396082, 0.000000000000000000 ) ) ;
#2027 = CARTESIAN_POINT ( 'NONE',  ( 4.037295881819344956, 7.932205305423046582, -0.7998128361456362523 ) ) ;
#2028 = CARTESIAN_POINT ( 'NONE',  ( 1.364683531249986537, 0.4260416670080872659, 0.7879004041258500513 ) ) ;
#2030 =( LENGTH_UNIT ( ) NAMED_UNIT ( * ) SI_UNIT ( .MILLI., .METRE. ) );
#2029 = CARTESIAN_POINT ( 'NONE',  ( 4.420840606507738357, 7.315341919971147355, 1.199719254218451159 ) ) ;
#2031 = CARTESIAN_POINT ( 'NONE',  ( 7.741342523278707866, 8.133913820021057006, 0.7216878364870458196 ) ) ;
#2032 = CARTESIAN_POINT ( 'NONE',  ( 3.192005314569335894, -1.456082124923337995, -1.610717807342199048 ) ) ;
#2034 = CARTESIAN_POINT ( 'NONE',  ( 3.491602800004707241, -1.839307750763185645, -0.08696504193297231733 ) ) ;
#2033 = CARTESIAN_POINT ( 'NONE',  ( -5.924549939491850381, 6.014322472269677533, 0.000000000000000000 ) ) ;
#2035 = CARTESIAN_POINT ( 'NONE',  ( -0.6823417656250212460, 3.301041667008085323, 1.181850606188767472 ) ) ;
#2036 = CARTESIAN_POINT ( 'NONE',  ( 4.159861740090546434, 1.033864333764370702, 1.932389678422803181 ) ) ;
#2037 = CARTESIAN_POINT ( 'NONE',  ( 8.748033642589533088, 13.52645069410513479, 8.214566069811549909 ) ) ;
#2038 = CARTESIAN_POINT ( 'NONE',  ( 4.750980993940300046, -1.819980134924009452, 1.343945550547174239 ) ) ;
#2039 = CARTESIAN_POINT ( 'NONE',  ( -4.985647801523292344, 6.839675073242382553, -1.599625672291256295 ) ) ;
#2040 = CARTESIAN_POINT ( 'NONE',  ( -4.662544117754887196, 7.086110115384146368, -1.393066284953614620 ) ) ;
#2041 = CARTESIAN_POINT ( 'NONE',  ( 5.228576739797318851, 7.698598165248225378, -1.206158463488806953 ) ) ;
#2042 = CARTESIAN_POINT ( 'NONE',  ( -6.278834536460198734, 6.497930845391236332, 0.7216878364870257245 ) ) ;
#2043 = CARTESIAN_POINT ( 'NONE',  ( 5.451787166470912993, 6.493411461371761284, -1.082531754730548412 ) ) ;
#2044 = CARTESIAN_POINT ( 'NONE',  ( 6.415310830085463323, -0.2139434178000785558, 1.756706237510232915 ) ) ;
#2045 = CARTESIAN_POINT ( 'NONE',  ( 4.424480750451430744, -0.8629065238535367222, -1.818916818396177026 ) ) ;
#2046 = CARTESIAN_POINT ( 'NONE',  ( 6.174848896020108668, 9.291408581077091000, 1.199719254218460707 ) ) ;
#2047 = CARTESIAN_POINT ( 'NONE',  ( 3.012826026228847098, 1.526343371991075948, -1.451234828553144673 ) ) ;
#2048 = CARTESIAN_POINT ( 'NONE',  ( 0.9135317552573400945, -1.216341065326152160, -1.479849217926126004 ) ) ;
#2050 = CARTESIAN_POINT ( 'NONE',  ( -0.7500000000000006661, 2.858333333333358706, -1.299038105676652011 ) ) ;
#2049 = CARTESIAN_POINT ( 'NONE',  ( 1.364683531249997417, 12.23437500034139980, 2.602085213965210642E-15 ) ) ;
#2051 = CARTESIAN_POINT ( 'NONE',  ( 2.594150448275188481, 0.9308562254837976502, -1.735710503097695145 ) ) ;
#2052 = CARTESIAN_POINT ( 'NONE',  ( 0.4263524580605422276, 1.788790299270696993, 0.5473224044415525569 ) ) ;
#2053 = CARTESIAN_POINT ( 'NONE',  ( 1.117545225965112188, 0.3861695934333775337, -1.923310697798483293 ) ) ;
#2055 = ORIENTED_EDGE ( 'NONE', *, *, #133829, .T. ) ;
#2054 = CARTESIAN_POINT ( 'NONE',  ( 0.1231139863388103495, 1.664874722635242277, 0.9407772870168448209 ) ) ;
#2056 = CARTESIAN_POINT ( 'NONE',  ( 6.209271165378815738, 7.306866450105836464, -1.082531754730543083 ) ) ;
#2057 = CARTESIAN_POINT ( 'NONE',  ( -1.402160292154681736E-14, 0.5093750003414236893, -1.575800808251659024 ) ) ;
#2058 = EDGE_CURVE ( 'NONE', #144530, #7256, #60351, .T. ) ;
#2060 = CARTESIAN_POINT ( 'NONE',  ( 5.752782329262379868, -1.473788443143897453, 1.151991621687727507 ) ) ;
#2059 = CIRCLE ( 'NONE', #123265, 0.08000000000000020983 ) ;
#2061 = CARTESIAN_POINT ( 'NONE',  ( 9.378489572351044856, 11.96465713920816043, -1.599625672291262513 ) ) ;
#2062 = CARTESIAN_POINT ( 'NONE',  ( -1.201851678989727383E-14, 2.821875000341418360, 1.575800808251672791 ) ) ;
#2063 = CARTESIAN_POINT ( 'NONE',  ( 5.735237735067807208, -0.04509738862551111033, -2.069921269439451539 ) ) ;
#2064 = CARTESIAN_POINT ( 'NONE',  ( 0.6125000000000019318, 2.666666666666678509, -1.060881119635941339 ) ) ;
#2065 = CARTESIAN_POINT ( 'NONE',  ( -4.082413651046300274, 6.816547455312373494, 1.082531754730549967 ) ) ;
#2066 = CARTESIAN_POINT ( 'NONE',  ( 0.3267351109269465148, -1.353470794461093973, 1.566751113397255812 ) ) ;
#2068 = CARTESIAN_POINT ( 'NONE',  ( -1.500000000000013101, 0.1708333333333560411, 0.8660254037844403729 ) ) ;
#2067 = VECTOR ( 'NONE', #106947, 1000.000000000000114 ) ;
#2069 = CARTESIAN_POINT ( 'NONE',  ( 5.750629710490689384, 9.860818428881154674, -0.7998128361456291469 ) ) ;
#2070 = CARTESIAN_POINT ( 'NONE',  ( -7.991641480251377772, 11.41099992934688956, 1.199719254218453823 ) ) ;
#2071 = CARTESIAN_POINT ( 'NONE',  ( 6.690022453700429139, 6.769724048930809701, 0.7998128361456331437 ) ) ;
#2072 = CARTESIAN_POINT ( 'NONE',  ( 1.364683531249986537, 0.6135416670080880985, 0.7879004041258500513 ) ) ;
#2073 = CARTESIAN_POINT ( 'NONE',  ( -1.500000000000011324, 2.920833333333352932, 0.8660254037844403729 ) ) ;
#2075 = CARTESIAN_POINT ( 'NONE',  ( 3.928111819657337911, 5.605883094398769195, 1.599625672291267398 ) ) ;
#2074 = CARTESIAN_POINT ( 'NONE',  ( 5.635196431686764207, -0.04651148872366302894, -1.961470878453225763 ) ) ;
#2076 = CARTESIAN_POINT ( 'NONE',  ( 2.794295885581669747, -1.882186412485300719, 0.7230279869864173481 ) ) ;
#2077 = CARTESIAN_POINT ( 'NONE',  ( 2.114329361022151854, 1.859220375642420819, 0.4613663794279678765 ) ) ;
#2078 = CARTESIAN_POINT ( 'NONE',  ( -1.899436509991837552, 3.291494839451070131, -0.4074537448170277854 ) ) ;
#2079 = CARTESIAN_POINT ( 'NONE',  ( 0.1170720436180875679, -0.1011795954627830590, 2.189343785608413917 ) ) ;
#2080 = CARTESIAN_POINT ( 'NONE',  ( 0.2331713839410576583, 0.005725554726919174046, -1.953566683266183102 ) ) ;
#2081 = CARTESIAN_POINT ( 'NONE',  ( 2.794054307841778328, -1.865266697571520194, -0.1415833504254116748 ) ) ;
#2082 = CARTESIAN_POINT ( 'NONE',  ( -1.402160292154681736E-14, -0.1312499993171854229, -1.732050807568870754 ) ) ;
#2083 = CARTESIAN_POINT ( 'NONE',  ( -8.342344591110322227, 8.627156865917170236, -0.7998128361456291469 ) ) ;
#2085 = CARTESIAN_POINT ( 'NONE',  ( 4.780926590999498238, 1.759528625808198354, -1.177310133890494548 ) ) ;
#2084 = CARTESIAN_POINT ( 'NONE',  ( -4.772106882330241717, 5.630174786549132726, -1.082531754730544860 ) ) ;
#2086 = CARTESIAN_POINT ( 'NONE',  ( 6.938893903907228378E-15, 10.64264068711930733, 1.214306433183764966E-14 ) ) ;
#2087 = CARTESIAN_POINT ( 'NONE',  ( 6.039524589772497620, 1.914416561877980261, -0.7887839105886890190 ) ) ;
#2089 = CARTESIAN_POINT ( 'NONE',  ( 6.620655732516651071, 4.689394895873098434, 2.736297475404291024 ) ) ;
#2088 = CARTESIAN_POINT ( 'NONE',  ( 1.997712292880989837, -2.090220067774691159, 0.05436529341687650757 ) ) ;
#2091 = VERTEX_POINT ( 'NONE', #146970 ) ;
#2090 = CARTESIAN_POINT ( 'NONE',  ( 0.7797844759148920835, -0.9637546898726162548, 1.430169641563599159 ) ) ;
#2092 = EDGE_CURVE ( 'NONE', #108467, #7144, #178391, .T. ) ;
#2093 = CARTESIAN_POINT ( 'NONE',  ( 6.938021921891177612, 9.117444880338284818, -1.599625672291262513 ) ) ;
#2094 = FILL_AREA_STYLE_COLOUR ( '', #209766 ) ;
#2095 = CARTESIAN_POINT ( 'NONE',  ( -6.966220764712148572, 6.002124920821316323, 2.420000000000000373 ) ) ;
#2096 = CARTESIAN_POINT ( 'NONE',  ( -9.928151704202875294, 5.423124072284297270, 6.082134274749043001 ) ) ;
#2097 = CARTESIAN_POINT ( 'NONE',  ( 5.599154252319471503, 9.476171027773981237, -0.7216878364870267237 ) ) ;
#2098 = LINE ( 'NONE', #81258, #144593 ) ;
#2100 = CARTESIAN_POINT ( 'NONE',  ( 0.2932429122153769052, 1.690905606409907058, -0.6502662643994570058 ) ) ;
#2099 = CARTESIAN_POINT ( 'NONE',  ( 5.182959862174088883, 9.268813282503625572, 0.7998128361456331437 ) ) ;
#2102 = CARTESIAN_POINT ( 'NONE',  ( -8.345207244411405156, 9.694828859023472134, 1.199719254218462483 ) ) ;
#2101 = AXIS2_PLACEMENT_3D ( 'NONE', #159302, #14090, #63931 ) ;
#2103 = CARTESIAN_POINT ( 'NONE',  ( 5.678167406024951624, 5.518950149984223508, 0.7998128361456341429 ) ) ;
#2104 = CARTESIAN_POINT ( 'NONE',  ( -5.349061533644712263, 7.606979636585072591, 1.237473162191610188 ) ) ;
#2105 = CARTESIAN_POINT ( 'NONE',  ( 5.515134625708930649, 9.656350506627580543, 0.000000000000000000 ) ) ;
#2106 = DIRECTION ( 'NONE',  ( 0.000000000000000000, 1.000000000000000000, 0.000000000000000000 ) ) ;
#2107 = CARTESIAN_POINT ( 'NONE',  ( 3.995705304526904200, 7.602062626508213405, -0.07732544726959944548 ) ) ;
#2108 = CARTESIAN_POINT ( 'NONE',  ( 8.107412671292022921, 12.40247251657532956, 0.7216878364870438212 ) ) ;
#2109 = VERTEX_POINT ( 'NONE', #48401 ) ;
#2110 = CARTESIAN_POINT ( 'NONE',  ( 0.7025736824820059123, 1.770395976773591284, 0.7320947492839694482 ) ) ;
#2111 = CARTESIAN_POINT ( 'NONE',  ( 0.2410938523699951708, 2.030451451530786766, 0.6113826261911478044 ) ) ;
#2112 = DIRECTION ( 'NONE',  ( 0.000000000000000000, 1.000000000000000000, 0.000000000000000000 ) ) ;
#2113 = CARTESIAN_POINT ( 'NONE',  ( -0.1399997263889594112, -0.002789056014654289761, -2.000146600338557956 ) ) ;
#2114 = CARTESIAN_POINT ( 'NONE',  ( -0.4500000000000389244, 3.999999999999948042, 0.4999999999999779066 ) ) ;
#2115 = CARTESIAN_POINT ( 'NONE',  ( -5.287316719649550301, 5.270883715786984780, 0.7216878364870317197 ) ) ;
#2116 = CARTESIAN_POINT ( 'NONE',  ( 9.408995418203971894, 11.03987807840189816, 1.082531754730549967 ) ) ;
#2117 = CARTESIAN_POINT ( 'NONE',  ( 3.045709290742618425, 1.389371873615535602, 1.396104611999344769 ) ) ;
#2118 = CARTESIAN_POINT ( 'NONE',  ( 0.9969211937387794098, -2.069638562867767373, -0.4609060192823294932 ) ) ;
#2119 = CARTESIAN_POINT ( 'NONE',  ( -6.566226467720086113, 6.555019055295208119, 1.040834085586084257E-14 ) ) ;
#2120 = CARTESIAN_POINT ( 'NONE',  ( -10.63115277548007498, 5.888090174969209833, -5.475543521278559922 ) ) ;
#2121 = DIRECTION ( 'NONE',  ( 1.000000000000000000, 6.532318089225149424E-16, -4.440892098500620245E-16 ) ) ;
#2122 = CARTESIAN_POINT ( 'NONE',  ( 6.421842908546859796, 1.265077015623069512, -1.789241164368003290 ) ) ;
#2123 = FACE_OUTER_BOUND ( 'NONE', #176365, .T. ) ;
#2124 = CARTESIAN_POINT ( 'NONE',  ( 3.768508550381458821, -1.294476758928708060, 1.426794059921440594 ) ) ;
#2125 = CARTESIAN_POINT ( 'NONE',  ( -7.832860060393135093, 10.16142270859057462, 1.599625672291295375 ) ) ;
#2126 = CARTESIAN_POINT ( 'NONE',  ( -0.2411972340275866378, -0.002466136893032525382, -1.900252416837118874 ) ) ;
#2127 = CARTESIAN_POINT ( 'NONE',  ( 0.7157882511714327434, -0.3199875008889854766, 2.183444778895065941 ) ) ;
#2128 = EDGE_CURVE ( 'NONE', #10132, #104455, #80771, .T. ) ;
#2129 = FACE_OUTER_BOUND ( 'NONE', #90690, .T. ) ;
#2130 = ORIENTED_EDGE ( 'NONE', *, *, #75894, .F. ) ;
#2131 = CARTESIAN_POINT ( 'NONE',  ( 1.500000000000001332, 10.65625000068279249, 0.000000000000000000 ) ) ;
#2132 = CARTESIAN_POINT ( 'NONE',  ( 6.332857179708399009, -1.868906791504289844, -0.6213115537570863545 ) ) ;
#2133 = CARTESIAN_POINT ( 'NONE',  ( 6.614805131849967879, -0.1256686391097518729, 1.812046779126045726 ) ) ;
#2134 = CARTESIAN_POINT ( 'NONE',  ( 6.257181701683109942, -2.286357481388684221, -0.2351346485395827413 ) ) ;
#2136 = CARTESIAN_POINT ( 'NONE',  ( 4.416758307032777608, -1.381121683685157642, 1.247472197611438016 ) ) ;
#2135 = CARTESIAN_POINT ( 'NONE',  ( -6.257970421159510188, 9.458660037064859694, 1.199719254218452047 ) ) ;
#2137 = CARTESIAN_POINT ( 'NONE',  ( 5.365994935958575240, 9.482354201918870018, 0.7998128361456341429 ) ) ;
#2138 = CARTESIAN_POINT ( 'NONE',  ( 2.972033609136344623, 6.549060441754430251, -0.4946758370507741698 ) ) ;
#2139 =( NAMED_UNIT ( * ) SI_UNIT ( $, .STERADIAN. ) SOLID_ANGLE_UNIT ( ) );
#2140 = CARTESIAN_POINT ( 'NONE',  ( -4.530395885260773525, 8.437212299446219532, 0.7998128361456481317 ) ) ;
#2141 = CARTESIAN_POINT ( 'NONE',  ( -3.367283612523017666, -0.9434115528611304313, 0.1057662437326452737 ) ) ;
#2142 = CARTESIAN_POINT ( 'NONE',  ( -0.1232117409455633916, -0.1621322592461546530, -2.156395338765437764 ) ) ;
#2143 = CARTESIAN_POINT ( 'NONE',  ( 3.863710590214593399, 7.451486755318259547, 1.040834085586084257E-14 ) ) ;
#2144 = ORIENTED_EDGE ( 'NONE', *, *, #54770, .T. ) ;
#2145 = CARTESIAN_POINT ( 'NONE',  ( -0.5368768833858145184, 13.37576698399828246, -1.254641125003840507 ) ) ;
#2146 = FACE_OUTER_BOUND ( 'NONE', #82357, .T. ) ;
#2148 = EDGE_CURVE ( 'NONE', #31723, #61426, #1268, .T. ) ;
#2147 = CARTESIAN_POINT ( 'NONE',  ( 0.2932112110246976044, 1.350478442433366677, 1.228755397233910696 ) ) ;
#2149 = CARTESIAN_POINT ( 'NONE',  ( -4.517891501851816649, 6.293959390292322986, -1.599625672291256295 ) ) ;
#2150 = CARTESIAN_POINT ( 'NONE',  ( 2.865509578329272777, -0.1299577181766899403, -1.729349861900606022 ) ) ;
#2151 = CARTESIAN_POINT ( 'NONE',  ( 6.508999999999982577, 2.977730662443831111, 2.353651457310241835 ) ) ;
#2152 = CARTESIAN_POINT ( 'NONE',  ( 3.946537740505243974, 2.817530495244580102, -0.7749999999999935829 ) ) ;
#2153 = CARTESIAN_POINT ( 'NONE',  ( 0.01214912391013078102, -0.8215866570660257384, -1.740624652096602221 ) ) ;
#2154 = CARTESIAN_POINT ( 'NONE',  ( 3.994932754639446859, 0.2835094185691371393, 1.941019531709553103 ) ) ;
#2155 = CARTESIAN_POINT ( 'NONE',  ( -10.15235809853472126, 10.73883929124566983, -0.7998128361456291469 ) ) ;
#2156 = CARTESIAN_POINT ( 'NONE',  ( 7.461064606222022277, 7.598996883547496139, 1.040834085586084257E-14 ) ) ;
#2157 = CARTESIAN_POINT ( 'NONE',  ( 5.285831659486547984, 2.043504495962459977, -0.5658664308652374686 ) ) ;
#2158 = CARTESIAN_POINT ( 'NONE',  ( 7.666209513884374438, 7.908608952478760834, 0.7998128361456281477 ) ) ;
#2159 = CARTESIAN_POINT ( 'NONE',  ( -7.797910906154257304, 12.24931315715533486, 0.000000000000000000 ) ) ;
#2160 = CARTESIAN_POINT ( 'NONE',  ( 5.443762371086860341, 6.309809840144842141, 1.199719254218462483 ) ) ;
#2161 = CARTESIAN_POINT ( 'NONE',  ( 3.239188805615275335, -0.1476314317495740769, -2.065021578984991724 ) ) ;
#2162 = CARTESIAN_POINT ( 'NONE',  ( -1.364683531250000748, -0.1781249996585798634, 0.000000000000000000 ) ) ;
#2164 = EDGE_LOOP ( 'NONE', ( #182900, #30650 ) ) ;
#2163 = CARTESIAN_POINT ( 'NONE',  ( 5.145291483242067088, 0.1622298597842904699, 2.215448774714718461 ) ) ;
#2165 = CARTESIAN_POINT ( 'NONE',  ( 2.954051123917677213, -2.124883583899921824, -0.8772644825643919342 ) ) ;
#2166 = CARTESIAN_POINT ( 'NONE',  ( 7.402388683381404988, 10.61957531637824204, -1.082531754730537976 ) ) ;
#2168 = CARTESIAN_POINT ( 'NONE',  ( 1.642778471875000035, -2.676041666188708756, -2.845375778867859751 ) ) ;
#2167 = CARTESIAN_POINT ( 'NONE',  ( 6.156811154381533591, 9.236677875870187293, -1.082531754730548412 ) ) ;
#2169 = EDGE_CURVE ( 'NONE', #89957, #26009, #98210, .T. ) ;
#2170 = CARTESIAN_POINT ( 'NONE',  ( 0.6124999999999932720, 1.666666666666712038, -1.060881119635983083 ) ) ;
#2171 = CARTESIAN_POINT ( 'NONE',  ( -3.179715765502671321, 5.975770656120749535, -2.419999999999998597 ) ) ;
#2172 = ORIENTED_EDGE ( 'NONE', *, *, #47152, .T. ) ;
#2173 = CARTESIAN_POINT ( 'NONE',  ( -0.3459972005395436367, -9.006862989983622114, 9.494064636159285087 ) ) ;
#2174 = EDGE_CURVE ( 'NONE', #22696, #43310, #35303, .T. ) ;
#2175 = CARTESIAN_POINT ( 'NONE',  ( 4.429883728109570207, -1.874397765517330061, 0.3784635845696313061 ) ) ;
#2176 = CARTESIAN_POINT ( 'NONE',  ( -0.03975248801529755738, 6.418311689316416491, -3.191082252424501498 ) ) ;
#2177 = CARTESIAN_POINT ( 'NONE',  ( 4.875862107049974803, 0.9950566627994448243, 1.408581599115072747 ) ) ;
#2178 = CARTESIAN_POINT ( 'NONE',  ( 3.925017756809038527, -1.752140073516525565, 0.9981236898717813499 ) ) ;
#2179 = CARTESIAN_POINT ( 'NONE',  ( 5.485083606918717436, -2.298851034700015727, -0.002838145216723860897 ) ) ;
#2180 = DIRECTION ( 'NONE',  ( 0.000000000000000000, -1.000000000000000000, -9.023263958591317418E-17 ) ) ;
#2181 = CARTESIAN_POINT ( 'NONE',  ( 6.375619162920919791, 2.015872221316476143, -0.6097100970045774559 ) ) ;
#2182 = CARTESIAN_POINT ( 'NONE',  ( -4.150204419558982671, 7.856005899545188242, 0.7216878364870338292 ) ) ;
#2183 = CARTESIAN_POINT ( 'NONE',  ( 6.327411112729964593, -1.665570200489007169, 0.5986406977509810545 ) ) ;
#2184 = PRESENTATION_LAYER_ASSIGNMENT (  '', '', ( #154368 ) ) ;
#2186 = CARTESIAN_POINT ( 'NONE',  ( 2.062813984423640612, -2.096776522422974409, -0.9266714075790563054 ) ) ;
#2185 = CARTESIAN_POINT ( 'NONE',  ( 5.550083779947807550, 7.568460058062819407, -1.599625672291283607 ) ) ;
#2187 = CARTESIAN_POINT ( 'NONE',  ( 6.597600327481837112, -1.840612352326329804, 0.05063316525460298534 ) ) ;
#2188 = CARTESIAN_POINT ( 'NONE',  ( -7.095713291905736853, 9.371694488680407886, 1.599625672291269396 ) ) ;
#2189 = DIRECTION ( 'NONE',  ( -0.8660254037844387076, 0.000000000000000000, -0.4999999999999999445 ) ) ;
#2190 = CARTESIAN_POINT ( 'NONE',  ( -2.844178363816758814, 6.540234867753325076, -0.7998128361456481317 ) ) ;
#2191 = CARTESIAN_POINT ( 'NONE',  ( -3.355169270512988773E-14, -0.6406249996585449136, -1.570758158831794260 ) ) ;
#2192 = DIRECTION ( 'NONE',  ( 0.000000000000000000, 0.000000000000000000, -1.000000000000000000 ) ) ;
#2193 = CARTESIAN_POINT ( 'NONE',  ( 6.865700769154306826, -0.4580177224273937475, 2.026514595051785772 ) ) ;
#2194 = CARTESIAN_POINT ( 'NONE',  ( 1.762908039156896978, -0.1037823317905466058, -2.014007988105172231 ) ) ;
#2195 = CARTESIAN_POINT ( 'NONE',  ( -0.7500000000000006661, -0.3604166659838467512, -1.299038105676652011 ) ) ;
#2196 = CARTESIAN_POINT ( 'NONE',  ( 5.004483369110711344, -0.6506757832731756563, -1.813419023564779353 ) ) ;
#2197 = CARTESIAN_POINT ( 'NONE',  ( 0.6823417656249969321, 11.02604166700806765, -1.181850606188757036 ) ) ;
#2198 = CARTESIAN_POINT ( 'NONE',  ( 1.951734608585634190, -1.981729029064113856, 1.003908989668365948 ) ) ;
#2199 = ORIENTED_EDGE ( 'NONE', *, *, #9864, .T. ) ;
#2201 = CARTESIAN_POINT ( 'NONE',  ( 4.175548122884573665, 3.973820352894515295, 1.214306433183764966E-14 ) ) ;
#2200 = CARTESIAN_POINT ( 'NONE',  ( 1.230761180058546289, 3.021116465842660581, -0.7749999999999874767 ) ) ;
#2202 = CARTESIAN_POINT ( 'NONE',  ( -0.3254290916866059979, 3.359077955639389046, -1.974305197405200163 ) ) ;
#2203 = CARTESIAN_POINT ( 'NONE',  ( 9.240045382913317340, 10.73880668727576015, -1.199719254218446718 ) ) ;
#2204 = CARTESIAN_POINT ( 'NONE',  ( 3.469446951953614189E-15, 5.227586206896610577, 1.214306433183764966E-14 ) ) ;
#2205 = DIRECTION ( 'NONE',  ( 1.000000000000000000, -0.000000000000000000, -0.000000000000000000 ) ) ;
#2206 = CARTESIAN_POINT ( 'NONE',  ( 4.036439982160089812, -1.511860617216064684, 0.8620873645008280128 ) ) ;
#2207 = CARTESIAN_POINT ( 'NONE',  ( 2.541395235131336694, 1.794889867694851260, -0.7924082849640816661 ) ) ;
#2209 = CARTESIAN_POINT ( 'NONE',  ( -7.266807147244793263, 8.540658428949452485, 1.082531754730549967 ) ) ;
#2208 = CARTESIAN_POINT ( 'NONE',  ( 3.472859903394816872, 7.203420320602605287, -0.7998128361456291469 ) ) ;
#2210 = CARTESIAN_POINT ( 'NONE',  ( -5.912397865540070185, 5.999963284693008880, 0.01096864257240509621 ) ) ;
#2211 = CARTESIAN_POINT ( 'NONE',  ( 11.29689844398643395, -5.530538574611989056, 9.269928574751062911E-15 ) ) ;
#2212 = CIRCLE ( 'NONE', #109479, 10.99999999999999112 ) ;
#2213 = CARTESIAN_POINT ( 'NONE',  ( 1.469262158920743966, 1.818092299969736425, 0.9742969159239748267 ) ) ;
#2214 = CARTESIAN_POINT ( 'NONE',  ( -6.496328159242330536, 10.73079995242472862, 0.000000000000000000 ) ) ;
#2215 = CARTESIAN_POINT ( 'NONE',  ( -4.650083499362882122, 6.448183387388563226, 1.443375672974064550 ) ) ;
#2216 = VECTOR ( 'NONE', #157528, 1000.000000000000000 ) ;
#2217 = CARTESIAN_POINT ( 'NONE',  ( 1.481717434351536244, 2.089849803356018221, -0.8673477522002839279 ) ) ;
#2218 = ORIENTED_EDGE ( 'NONE', *, *, #126729, .T. ) ;
#2219 = CARTESIAN_POINT ( 'NONE',  ( 1.499999999999987121, 0.07708333401615156955, -0.8660254037844323793 ) ) ;
#2220 = CARTESIAN_POINT ( 'NONE',  ( 3.022558680773678397, 1.760047114015901526, 0.6337009143728977723 ) ) ;
#2221 = CARTESIAN_POINT ( 'NONE',  ( 0.8790820841908916217, -0.4200629052855206491, -1.682323782590444461 ) ) ;
#2222 = CARTESIAN_POINT ( 'NONE',  ( 5.741772062182810998, 2.188963553168365994, 0.1087695542012837302 ) ) ;
#2223 = CARTESIAN_POINT ( 'NONE',  ( 5.772612788190349953, -1.469667252935745960, 1.779063562929294129 ) ) ;
#2224 = CARTESIAN_POINT ( 'NONE',  ( 1.780222679459046997, -1.103320402871512673, 1.740482491890801287 ) ) ;
#2225 = CARTESIAN_POINT ( 'NONE',  ( 3.697155016903285407, -0.5626119583077812125, 1.858668453590556213 ) ) ;
#2226 = CARTESIAN_POINT ( 'NONE',  ( -5.233084104750526322, 5.207612331738130429, 0.000000000000000000 ) ) ;
#2227 = CARTESIAN_POINT ( 'NONE',  ( 5.782452155351484713, -1.824793809246130438, -0.4103911052399379367 ) ) ;
#2228 = CARTESIAN_POINT ( 'NONE',  ( 1.937500000000002220, 1.451031289061040841, -1.451031289061198049 ) ) ;
#2229 = CARTESIAN_POINT ( 'NONE',  ( 3.995022045461748217, 7.603044914155053569, 0.06581304817247432548 ) ) ;
#2230 = CARTESIAN_POINT ( 'NONE',  ( 0.2625146791020065984, -1.733275965524210482, -0.05152637578398518159 ) ) ;
#2231 = CARTESIAN_POINT ( 'NONE',  ( 3.879041347285658414, 6.579279767591636130, -1.082531754730548412 ) ) ;
#2232 = CARTESIAN_POINT ( 'NONE',  ( -0.6801582343750299797, 0.9322916670080338974, 1.178068619123803451 ) ) ;
#2233 = CARTESIAN_POINT ( 'NONE',  ( 4.500625067706437221, -1.976956227568788638, 0.3961002554062897918 ) ) ;
#2234 = CARTESIAN_POINT ( 'NONE',  ( -4.582292731294565158, 4.448355729372827305, 1.214306433183764966E-14 ) ) ;
#2235 = CARTESIAN_POINT ( 'NONE',  ( 9.284636267260101050, 9.726497154758602548, -0.7998128361456281477 ) ) ;
#2236 = CARTESIAN_POINT ( 'NONE',  ( 5.174371902270911150, 6.065797303184739420, 1.199719254218452047 ) ) ;
#2238 = CARTESIAN_POINT ( 'NONE',  ( -6.717278222822391953, 7.849261790823902629, 6.830415307812263137 ) ) ;
#2237 = CARTESIAN_POINT ( 'NONE',  ( 1.769861954154128725, 0.9373860217288846330, 1.566528536362868707 ) ) ;
#2239 = CARTESIAN_POINT ( 'NONE',  ( -5.795184315198522285, 5.725746220678519904, -0.7998128361456362523 ) ) ;
#2240 = CARTESIAN_POINT ( 'NONE',  ( -5.842637852846352509, 5.781108681267656202, 0.7998128361456282587 ) ) ;
#2241 = CARTESIAN_POINT ( 'NONE',  ( -10.51596412982177853, 9.986590817315772028, -3.553961965504329967 ) ) ;
#2242 = ORIENTED_EDGE ( 'NONE', *, *, #150221, .T. ) ;
#2243 = CARTESIAN_POINT ( 'NONE',  ( -6.427974226210522168, 6.671927150099951298, 0.000000000000000000 ) ) ;
#2244 = CARTESIAN_POINT ( 'NONE',  ( -3.952365473583647315, 4.569846793057691592, 1.199719254218462483 ) ) ;
#2246 = CARTESIAN_POINT ( 'NONE',  ( -8.727698198895085469, 11.20540053684285553, -1.599625672291263179 ) ) ;
#2245 = B_SPLINE_CURVE_WITH_KNOTS ( 'NONE', 3,
 ( #47719, #113835, #179833, #97531, #32504, #164640, #184071, #102839, #103912, #101766, #186200, #7444, #23703, #122383, #54089, #37835, #169957, #185128, #204571, #168895, #20498, #134303 ),
 .UNSPECIFIED., .F., .F.,
 ( 4, 3, 3, 3, 3, 3, 3, 4 ),
 ( 0.000000000000000000, 1.209865308640946775E-05, 2.418763075658931773E-05, 3.626888754244386227E-05, 5.481069466193077340E-05, 8.058589917397381919E-05, 0.0001081451638904062126, 0.0001095998438940776838 ),
 .UNSPECIFIED. ) ;
#2247 = CARTESIAN_POINT ( 'NONE',  ( 5.303380940763749329, 1.780254367526274972, -0.9538449857209270188 ) ) ;
#2249 = VERTEX_POINT ( 'NONE', #52631 ) ;
#2248 = CARTESIAN_POINT ( 'NONE',  ( 0.3465379015402513252, 1.086389676674501148, -1.820904993421072371 ) ) ;
#2250 = CARTESIAN_POINT ( 'NONE',  ( -7.273023059088104425, 7.449891421883056530, 0.000000000000000000 ) ) ;
#2251 = CARTESIAN_POINT ( 'NONE',  ( 5.705283713252285338, 5.550585841749444249, -0.7998128361456211532 ) ) ;
#2252 = CARTESIAN_POINT ( 'NONE',  ( 4.873930702218094879, 1.184903577025652188, 1.686001177547257424 ) ) ;
#2253 = CARTESIAN_POINT ( 'NONE',  ( 5.027970288326707227, -1.728003250605243180, 1.038991650911202713 ) ) ;
#2254 = ORIENTED_EDGE ( 'NONE', *, *, #31074, .T. ) ;
#2255 = CARTESIAN_POINT ( 'NONE',  ( 3.598535064101026748, 7.346084821328116909, 0.3627869759331026622 ) ) ;
#2256 = CARTESIAN_POINT ( 'NONE',  ( 6.535912570239620578, 9.782925877658371405, 1.199719254218452047 ) ) ;
#2257 = CIRCLE ( 'NONE', #26555, 12.00000000000000178 ) ;
#2259 = ORIENTED_EDGE ( 'NONE', *, *, #27400, .F. ) ;
#2258 = CARTESIAN_POINT ( 'NONE',  ( -6.466312919074983512, 6.508729591867735031, -0.7998128361456362523 ) ) ;
#2260 = CARTESIAN_POINT ( 'NONE',  ( 5.017113787211129328, 8.018716392533608683, 1.139262206072016559 ) ) ;
#2261 = CARTESIAN_POINT ( 'NONE',  ( 4.833361152654930493, -1.319026006086077230, 1.524810761284051575 ) ) ;
#2262 = CARTESIAN_POINT ( 'NONE',  ( 4.329911453333429527, 1.806054511993939515, 0.3568155486674411958 ) ) ;
#2263 = CARTESIAN_POINT ( 'NONE',  ( 10.54982673430220252, -8.131911363926706215, -0.6210660986541617357 ) ) ;
#2264 = CARTESIAN_POINT ( 'NONE',  ( 1.823324434984688214, 2.154351390505971686, 0.8276274939288345012 ) ) ;
#2265 = CARTESIAN_POINT ( 'NONE',  ( 7.018280793729500644, 8.217024343219755167, -1.199719254218452047 ) ) ;
#2266 = CARTESIAN_POINT ( 'NONE',  ( 5.307972821619873827, -2.151738229465068653, 0.2060058040841972193 ) ) ;
#2267 = CARTESIAN_POINT ( 'NONE',  ( 8.959240580532112475, 9.346868853575953651, -0.7998128361456221525 ) ) ;
#2268 = CARTESIAN_POINT ( 'NONE',  ( 0.3802858058059845336, -0.2390265653847540028, -1.927249604900363122 ) ) ;
#2269 = CARTESIAN_POINT ( 'NONE',  ( -3.601662362724658895, 7.353689856487406473, -0.7998128361456281477 ) ) ;
#2270 = AXIS2_PLACEMENT_3D ( 'NONE', #97155, #179457, #182625 ) ;
#2271 = CARTESIAN_POINT ( 'NONE',  ( 2.671705178897700428, 0.4353224022266768967, -0.1180795802420642887 ) ) ;
#2272 = CARTESIAN_POINT ( 'NONE',  ( -3.467853430045390706, 7.267855778353407459, 0.7998128361456352531 ) ) ;
#2273 = CARTESIAN_POINT ( 'NONE',  ( 3.590566789841375339, -0.3639703897368729568, -1.834726254853453087 ) ) ;
#2276 = CARTESIAN_POINT ( 'NONE',  ( -6.557303570864871034, 7.679217583210999010, -1.199719254218452047 ) ) ;
#2275 = CARTESIAN_POINT ( 'NONE',  ( -0.7500000000000006661, -1.110416665983847473, -1.299038105676652011 ) ) ;
#2274 = CARTESIAN_POINT ( 'NONE',  ( 0.08795244648929222142, 1.102731429460445334, 1.562230693318837238 ) ) ;
#2277 = CARTESIAN_POINT ( 'NONE',  ( 2.403190426070573871, 1.771669130372434564, -1.315670724662293178 ) ) ;
#2278 = CARTESIAN_POINT ( 'NONE',  ( 6.720655732516647163, -0.001531948155462499201, 2.073773125298985054 ) ) ;
#2279 = CARTESIAN_POINT ( 'NONE',  ( 5.040934186182656873, 4.775511393501539636, 1.040834085586084257E-14 ) ) ;
#2280 = CARTESIAN_POINT ( 'NONE',  ( 6.902509602688803980, 9.146290184594002781, -1.443375672974064550 ) ) ;
#2281 = CARTESIAN_POINT ( 'NONE',  ( -5.610376637956639101, 5.439860920571172542, 0.000000000000000000 ) ) ;
#2282 = CARTESIAN_POINT ( 'NONE',  ( -7.417719440008134768, 7.826629899530511025, 0.7216878364870317197 ) ) ;
#2283 = CARTESIAN_POINT ( 'NONE',  ( 0.3683541893860732275, -1.290952873633111953, 1.489922359098810878 ) ) ;
#2284 = CARTESIAN_POINT ( 'NONE',  ( 0.1129635547038260190, -0.9897495874401724958, -2.082026327295583012 ) ) ;
#2285 = CARTESIAN_POINT ( 'NONE',  ( 1.961309178647975715, 1.629323162926434199, 1.092499269706406428 ) ) ;
#2286 = CARTESIAN_POINT ( 'NONE',  ( 3.801677422522796945, -1.558724286948458548, -1.350822056805228266 ) ) ;
#2287 = CARTESIAN_POINT ( 'NONE',  ( 6.832946231607457399, 7.074118146404578589, -0.7216878364870257245 ) ) ;
#2288 = CARTESIAN_POINT ( 'NONE',  ( 5.773793314573267388, 7.829454515125894964, 1.599625672291268286 ) ) ;
#2289 = VERTEX_POINT ( 'NONE', #198859 ) ;
#2290 = CARTESIAN_POINT ( 'NONE',  ( 8.446366511189332016, 9.916811020218137429, -1.082531754730543083 ) ) ;
#2291 = CARTESIAN_POINT ( 'NONE',  ( -1.001543065824772872E-14, 5.134375000341421469, 1.575800808251672791 ) ) ;
#2292 = CARTESIAN_POINT ( 'NONE',  ( -10.84253909858433218, 4.919570308430901484, -5.035411995924089723 ) ) ;
#2293 = CARTESIAN_POINT ( 'NONE',  ( 3.321384445223597659, 6.818772919495430074, -0.7216878364870267237 ) ) ;
#2294 = CARTESIAN_POINT ( 'NONE',  ( 0.2511275705787468504, -0.4786951167374750571, -2.125832126681607370 ) ) ;
#2296 = CARTESIAN_POINT ( 'NONE',  ( 6.497600353373155002, -1.840680978339729545, 0.05264081064878384231 ) ) ;
#2295 = DIRECTION ( 'NONE',  ( -0.000000000000000000, -1.000000000000000000, -0.000000000000000000 ) ) ;
#2297 = CARTESIAN_POINT ( 'NONE',  ( 5.358717427693826529, 6.320109463822404905, -1.084804798701855422 ) ) ;
#2299 = DIRECTION ( 'NONE',  ( 3.330669073875478989E-16, -4.632576442341012461E-16, -1.000000000000000000 ) ) ;
#2298 = B_SPLINE_CURVE_WITH_KNOTS ( 'NONE', 3,
 ( #197808, #82989, #212983, #98207, #49441, #15846 ),
 .UNSPECIFIED., .F., .F.,
 ( 4, 2, 4 ),
 ( 0.000000000000000000, 0.001226111284895915667, 0.002452222569791831768 ),
 .UNSPECIFIED. ) ;
#2300 = CARTESIAN_POINT ( 'NONE',  ( 0.9482695043977107385, 0.5371953702461745861, 1.791772314883005146 ) ) ;
#2302 = EDGE_CURVE ( 'NONE', #64997, #36604, #30885, .T. ) ;
#2301 = CARTESIAN_POINT ( 'NONE',  ( -5.796211742468360129, 6.069872997065163922, -0.5622600474686073602 ) ) ;
#2303 = DIRECTION ( 'NONE',  ( -0.6483454320283789096, 0.000000000000000000, 0.7613463080411795314 ) ) ;
#2304 = CARTESIAN_POINT ( 'NONE',  ( 5.862225131719664972, 7.287605523280396902, -1.268052015211480033 ) ) ;
#2305 = CARTESIAN_POINT ( 'NONE',  ( -1.364683531250010295, 5.092708333674757171, 0.7879004041258379498 ) ) ;
#2306 = CARTESIAN_POINT ( 'NONE',  ( 0.7504700684401002242, 1.884043224930329385, 0.3264296256808990049 ) ) ;
#2307 = CARTESIAN_POINT ( 'NONE',  ( 2.817004693338585941, -0.1753839976894235320, 1.761133515796961868 ) ) ;
#2308 = CARTESIAN_POINT ( 'NONE',  ( 0.2055213853429035953, 1.417038256915002181, 1.284265443176696442 ) ) ;
#2310 = CARTESIAN_POINT ( 'NONE',  ( 4.710494965788769584, 1.834319554003289721, 0.5521488281355608763 ) ) ;
#2309 = CARTESIAN_POINT ( 'NONE',  ( -9.834497819152506537, 3.956598013261176217, -6.044631300485411529 ) ) ;
#2311 = CARTESIAN_POINT ( 'NONE',  ( -0.1409997244346075651, 7.629137130509101361, -2.600278764091648487 ) ) ;
#2312 = CARTESIAN_POINT ( 'NONE',  ( 5.371531009330141160, -0.2907324665500017891, 1.947856185699713638 ) ) ;
#2314 = EDGE_CURVE ( 'NONE', #158402, #95365, #73964, .T. ) ;
#2313 = CARTESIAN_POINT ( 'NONE',  ( 0.5277791401020451856, -0.3051165123582540994, 2.098401203810342786 ) ) ;
#2315 = CARTESIAN_POINT ( 'NONE',  ( 0.4373225248172820656, -7.723431457505077979, -10.96785329849813273 ) ) ;
#2316 = CARTESIAN_POINT ( 'NONE',  ( 4.223419137798128276, -1.790188510885984297, 0.5427707113358354318 ) ) ;
#2318 = VERTEX_POINT ( 'NONE', #66709 ) ;
#2317 = CARTESIAN_POINT ( 'NONE',  ( 0.7151340513122245168, -0.2707656271505008982, 1.805370379145049275 ) ) ;
#2320 = CARTESIAN_POINT ( 'NONE',  ( 0.000000000000000000, -3.600000000000005862, 0.000000000000000000 ) ) ;
#2319 = CARTESIAN_POINT ( 'NONE',  ( 3.053566222061272040, -1.804402116661915967, -1.270350324234905903 ) ) ;
#2321 = CARTESIAN_POINT ( 'NONE',  ( -0.6823417656249969321, 5.280208333674756283, -1.181850606188749264 ) ) ;
#2322 = CARTESIAN_POINT ( 'NONE',  ( 1.100133984900531825, 0.8377775336174065890, -1.885062252648894265 ) ) ;
#2324 = ADVANCED_FACE ( 'NONE', ( #36371 ), #212046, .T. ) ;
#2323 = CARTESIAN_POINT ( 'NONE',  ( 5.438792177376376991, 9.497007973581119700, 1.040834085586084257E-14 ) ) ;
#2325 = CARTESIAN_POINT ( 'NONE',  ( -7.669108446824431269, 12.09904362127053545, -0.7998128361456291469 ) ) ;
#2326 = CARTESIAN_POINT ( 'NONE',  ( 1.931788062848141441E-13, 7.054063922337705073, -3.955400951015614730 ) ) ;
#2327 = LINE ( 'NONE', #34843, #100006 ) ;
#2328 = DIRECTION ( 'NONE',  ( 0.7071067811865489050, -0.7071067811865462405, -6.410781031902101009E-32 ) ) ;
#2329 = ORIENTED_EDGE ( 'NONE', *, *, #181317, .T. ) ;
#2330 = CARTESIAN_POINT ( 'NONE',  ( 3.578635096964689843, 1.315621898185691974, -1.598582974826658010 ) ) ;
#2331 = CARTESIAN_POINT ( 'NONE',  ( 1.499999999999990896, 4.775000000000022560, 1.214306433183764966E-14 ) ) ;
#2332 = CARTESIAN_POINT ( 'NONE',  ( 1.388190569347878212, -0.9732202972718406730, 1.930209198840258100 ) ) ;
#2333 = CARTESIAN_POINT ( 'NONE',  ( -6.444026653998019327, 6.794751805161505231, -0.4079633569072909638 ) ) ;
#2334 = CARTESIAN_POINT ( 'NONE',  ( 1.049479869930733944, -1.824965358647975489, 0.8655331567536515003 ) ) ;
#2335 = DIRECTION ( 'NONE',  ( 1.000000000000000000, 0.000000000000000000, 0.000000000000000000 ) ) ;
#2336 = ORIENTED_EDGE ( 'NONE', *, *, #208712, .T. ) ;
#2338 = CARTESIAN_POINT ( 'NONE',  ( 8.351459436338029008, 10.76645531385962862, -1.443375672974063439 ) ) ;
#2337 = CARTESIAN_POINT ( 'NONE',  ( 3.130865642711470276, -4.000192543527539613, -1.507748429708645199 ) ) ;
#2339 = CARTESIAN_POINT ( 'NONE',  ( 6.749375321999433908, -1.976647572034227140, -0.3960365597561604778 ) ) ;
#2340 = CARTESIAN_POINT ( 'NONE',  ( 0.3918150239524306189, -2.006371095615328226, 0.2024682584410575914 ) ) ;
#2341 = CARTESIAN_POINT ( 'NONE',  ( 6.539320575229230492, 2.428701779328062749, 2.485127258459709054 ) ) ;
#2342 = CARTESIAN_POINT ( 'NONE',  ( 4.669572502782517454, 1.262004115398765780, 1.791526714441132873 ) ) ;
#2343 =( BOUNDED_SURFACE ( )  B_SPLINE_SURFACE ( 3, 2, ( 
 ( #205237, #55808, #154383 ),
 ( #105661, #204153, #141381 ),
 ( #56878, #5960, #187929 ),
 ( #41724, #157600, #207391 ),
 ( #73106, #125168, #189007 ),
 ( #158656, #171688, #191127 ) ),
 .UNSPECIFIED., .F., .F., .T. ) 
 B_SPLINE_SURFACE_WITH_KNOTS ( ( 4, 2, 4 ),
 ( 3, 3 ),
 ( 0.000000000000000000, 0.0003754689591423960443, 0.0007509379182847920886 ),
 ( 0.000000000000000000, 1.000000000000000000 ),
 .UNSPECIFIED. ) 
 GEOMETRIC_REPRESENTATION_ITEM ( )  RATIONAL_B_SPLINE_SURFACE ( (
 ( 1.000000000000000000, 0.7071067811865551223, 1.000000000000000000),
 ( 1.000000000000000000, 0.7018599272024059754, 1.000000000000000000),
 ( 1.000000000000000000, 0.6927733177260235742, 1.000000000000000000),
 ( 1.000000000000000000, 0.6772007068873748814, 1.000000000000000000),
 ( 1.000000000000000000, 0.6709974581637072610, 1.000000000000000000),
 ( 1.000000000000000000, 0.6711954675835395401, 1.000000000000000000) ) ) 
 REPRESENTATION_ITEM ( '' )  SURFACE ( )  );
#2344 = CARTESIAN_POINT ( 'NONE',  ( -0.7500000000000006661, 2.889583334016148974, -1.299038105676652011 ) ) ;
#2345 = CARTESIAN_POINT ( 'NONE',  ( 3.146637304467227558, 1.866760668956708447, 0.4145885930168375921 ) ) ;
#2346 = CARTESIAN_POINT ( 'NONE',  ( -5.199715606040888005, 6.025088614257851027, -1.199719254218446718 ) ) ;
#2347 = CARTESIAN_POINT ( 'NONE',  ( 2.670593071767634719, 6.059516317130127838, -0.7216878364870267237 ) ) ;
#2349 = CARTESIAN_POINT ( 'NONE',  ( 1.528922965942226986, -1.701935853630029083, 1.081086586856384590 ) ) ;
#2348 = CARTESIAN_POINT ( 'NONE',  ( -8.771762197917311710, 13.17754696430482042, 0.7216878364870317197 ) ) ;
#2350 = CARTESIAN_POINT ( 'NONE',  ( -1.364683531250010295, 10.94270833367473372, 0.7879004041258445001 ) ) ;
#2352 = CARTESIAN_POINT ( 'NONE',  ( -3.820365424000704557, 7.679119771301277098, -0.7998128361456481317 ) ) ;
#2351 = CARTESIAN_POINT ( 'NONE',  ( 0.5391474206018737059, -1.962199071191613964, 1.185045521927590162 ) ) ;
#2353 = CARTESIAN_POINT ( 'NONE',  ( 3.627714610788032701, -1.027129601966117134, -1.385419451709940519 ) ) ;
#2354 = CARTESIAN_POINT ( 'NONE',  ( 0.1399997263885795207, 2.876830203203218694, -2.488333633689450597 ) ) ;
#2355 = CARTESIAN_POINT ( 'NONE',  ( 2.998324526916512411, 6.649795714711241423, 0.000000000000000000 ) ) ;
#2356 = CARTESIAN_POINT ( 'NONE',  ( -1.203941962966158297, 2.947768152887754400, -0.7749999999999944711 ) ) ;
#2357 = CARTESIAN_POINT ( 'NONE',  ( 1.767943819387544968, -1.947426213878332035, 0.2369139692007388165 ) ) ;
#2358 =( BOUNDED_CURVE ( )  B_SPLINE_CURVE ( 2, ( #63130, #78303, #129294, #209348, #192038, #177957, #128227 ),
 .UNSPECIFIED., .F., .T. ) 
 B_SPLINE_CURVE_WITH_KNOTS ( ( 3, 2, 2, 3 ),
 ( 0.1607142857142856152, 0.1666666666666666297, 0.1726190476190476719, 0.1785714285714287142 ),
 .UNSPECIFIED. ) 
 CURVE ( )  GEOMETRIC_REPRESENTATION_ITEM ( )  RATIONAL_B_SPLINE_CURVE ( ( 1.000000000000002442, 0.8660254037844361541, 1.000000000000000000, 0.8660254037844387076, 1.000000000000000000, 0.8660254037844355990, 1.000000000000003109 ) ) 
 REPRESENTATION_ITEM ( '' )  );
#2359 = LINE ( 'NONE', #202702, #32917 ) ;
#2360 = CARTESIAN_POINT ( 'NONE',  ( 3.194917754314666514, 6.879154480009089134, 0.7998128361456321445 ) ) ;
#2361 = CARTESIAN_POINT ( 'NONE',  ( 0.1753634416057498202, 0.7014533214223102053, -2.226873008360684913 ) ) ;
#2362 = ORIENTED_EDGE ( 'NONE', *, *, #105101, .T. ) ;
#2363 = CARTESIAN_POINT ( 'NONE',  ( -1.499999999999963141, 7.750000000000000000, 10.86128356754324820 ) ) ;
#2364 = ORIENTED_EDGE ( 'NONE', *, *, #150402, .T. ) ;
#2365 = CARTESIAN_POINT ( 'NONE',  ( 3.457467740999135231, -1.373635607365558453, -1.181027286383716124 ) ) ;
#2366 = VERTEX_POINT ( 'NONE', #89981 ) ;
#2367 = CARTESIAN_POINT ( 'NONE',  ( 7.367930134383754215, 7.560616343061329125, -0.7998128361456341429 ) ) ;
#2368 = CARTESIAN_POINT ( 'NONE',  ( 3.464990776744291345, 6.200183785247111778, 1.199719254218452047 ) ) ;
#2369 = CARTESIAN_POINT ( 'NONE',  ( 4.986864056229866726, -1.707513420791425540, -0.6052512474536574372 ) ) ;
#2370 = CARTESIAN_POINT ( 'NONE',  ( 7.485510208076452621, 7.905719128943566432, 0.000000000000000000 ) ) ;
#2371 = CARTESIAN_POINT ( 'NONE',  ( 5.000138648025401977, 6.582195279309941860, -1.237349059142704988 ) ) ;
#2372 = AXIS2_PLACEMENT_3D ( 'NONE', #8636, #206834, #154907 ) ;
#2374 = CARTESIAN_POINT ( 'NONE',  ( 8.218213668177886788, 12.73966637951625813, 0.7998128361456462443 ) ) ;
#2373 = CARTESIAN_POINT ( 'NONE',  ( 5.810971417242416948, -1.466730511752023958, 1.145431029696217573 ) ) ;
#2375 = CARTESIAN_POINT ( 'NONE',  ( 4.306187113567048641, 1.175507255964372222, -1.512451795395561405 ) ) ;
#2376 = DIRECTION ( 'NONE',  ( 0.000000000000000000, -1.000000000000000000, 0.000000000000000000 ) ) ;
#2377 = CARTESIAN_POINT ( 'NONE',  ( -12.65133343644925823, 8.691152131673410608, 1.253321570098529181 ) ) ;
#2378 = TOROIDAL_SURFACE ( 'NONE', #154552, 2.080000000000000071, 0.08000000000000000167 ) ;
#2379 = CARTESIAN_POINT ( 'NONE',  ( -10.99958311221863028, -9.919613946868093279, 0.09579086958121280082 ) ) ;
#2380 = CARTESIAN_POINT ( 'NONE',  ( 6.832946231607457399, 7.074118146404578589, -0.7216878364870257245 ) ) ;
#2381 = B_SPLINE_CURVE_WITH_KNOTS ( 'NONE', 3,
 ( #62739, #78993, #77931, #47596, #28118, #113710, #147221 ),
 .UNSPECIFIED., .F., .F.,
 ( 4, 3, 4 ),
 ( 0.000000000000000000, 6.254153400238295828E-05, 0.0001620526076657094038 ),
 .UNSPECIFIED. ) ;
#2382 = CARTESIAN_POINT ( 'NONE',  ( -2.279742385392243165, 5.811449882932888222, -0.7998128361456281477 ) ) ;
#2383 = CARTESIAN_POINT ( 'NONE',  ( 0.4620835240300471547, 2.137967531602209981, -0.3185850937674692407 ) ) ;
#2384 = CARTESIAN_POINT ( 'NONE',  ( -6.120580001926503755, 6.105374521861167914, -0.7998128361456362523 ) ) ;
#2385 = CARTESIAN_POINT ( 'NONE',  ( 5.554000203453580475, 6.508696987897830688, -1.199719254218452047 ) ) ;
#2386 = CARTESIAN_POINT ( 'NONE',  ( 0.3053143536290473525, -0.4923201697357786344, 1.757875871163572024 ) ) ;
#2387 = CARTESIAN_POINT ( 'NONE',  ( -5.739179097286464248, 5.590130456455974617, -0.7998128361456221525 ) ) ;
#2388 = CARTESIAN_POINT ( 'NONE',  ( 3.241029684393876842, -1.610631872634618933, 0.8593927405577477252 ) ) ;
#2389 = EDGE_CURVE ( 'NONE', #80737, #93709, #181246, .T. ) ;
#2390 = CARTESIAN_POINT ( 'NONE',  ( 12.43511541931632891, 7.569548269842172772, -1.878403980710225518 ) ) ;
#2391 = CARTESIAN_POINT ( 'NONE',  ( 2.523828315609038864, 1.932092998399935091, -0.3813574256018251729 ) ) ;
#2392 = CARTESIAN_POINT ( 'NONE',  ( 4.019036194231017767, -1.857530068489420705, 0.5666795103562488611 ) ) ;
#2393 = CARTESIAN_POINT ( 'NONE',  ( -7.208094944320834863, 8.438474185576302133, -1.199719254218452047 ) ) ;
#2395 = CARTESIAN_POINT ( 'NONE',  ( 4.430007776716601953, -2.079114408633813582, 0.4165480963118637914 ) ) ;
#2394 = CARTESIAN_POINT ( 'NONE',  ( 6.912678218121202534, 9.158153569265168770, 1.599625672291268286 ) ) ;
#2396 = CARTESIAN_POINT ( 'NONE',  ( -11.86145016429273191, 12.69999999999999929, 1.099999999999996758 ) ) ;
#2397 = CARTESIAN_POINT ( 'NONE',  ( 8.934986926605834157, 10.38290515491702770, -1.199719254218446718 ) ) ;
#2398 = CARTESIAN_POINT ( 'NONE',  ( 6.101957686160805139, 6.023808750328159434, -0.2146407016825630509 ) ) ;
#2399 = FACE_OUTER_BOUND ( 'NONE', #26284, .T. ) ;
#2400 = CARTESIAN_POINT ( 'NONE',  ( 4.578903193113299963, 6.365139696764064325, 1.599625672291267398 ) ) ;
#2401 = CARTESIAN_POINT ( 'NONE',  ( 4.549643065837591038, 7.465611455855944101, -1.199719254218452047 ) ) ;
#2402 = DIRECTION ( 'NONE',  ( 0.000000000000000000, -1.000000000000000000, -0.000000000000000000 ) ) ;
#2404 = ADVANCED_FACE ( 'NONE', ( #7621 ), #121100, .F. ) ;
#2403 = CARTESIAN_POINT ( 'NONE',  ( 5.391160240453525709, 1.608232483172780558, -0.8641324296934371763 ) ) ;
#2405 = CARTESIAN_POINT ( 'NONE',  ( 10.99943760478736010, -9.902953797791681723, -0.1112316694888297319 ) ) ;
#2406 = CARTESIAN_POINT ( 'NONE',  ( -7.998947442382709383, 12.27592974951444660, 0.7216878364870478180 ) ) ;
#2407 = CIRCLE ( 'NONE', #109821, 6.264285714285709794 ) ;
#2408 =( BOUNDED_SURFACE ( )  B_SPLINE_SURFACE ( 1, 2, ( 
 ( #177587, #146173, #93153, #94221, #147230, #194889, #145118, #142985, #193814, #211124, #62748, #64885, #30268, #112648, #76866, #178657, #212188, #63825, #208985, #114774, #86479, #182902, #117976, #200203, #85407, #82198, #35580, #168790, #167728, #151492, #202331, #32399, #50775, #164529, #68057, #101660, #150428, #149346, #185023, #70197, #180771, #1993, #925, #199130, #49709, #183969, #83260, #17185, #19329, #134194, #136310, #165593, #66993, #18256, #3061, #69131, #51856, #132071, #201266, #115838, #133131, #135253, #116903, #52907, #98465, #119040, #36649, #102734, #20395, #152543, #34518, #4129, #16115, #181824, #148292, #33456, #214290, #99533, #100591, #166666, #84340, #65924, #198082, #24662, #74503, #188233, #57183, #189310, #205545, #39873, #90769, #103807, #203397, #40949, #187169, #153620, #55050, #105982, #6269, #172005, #156830, #123345, #8417, #140607, #23595, #206619, #138446, #9494, #58247, #5192, #7339, #104879, #121200, #124404, #122275, #190362, #89704, #107055, #75566, #155754, #141675, #42024, #170922, #25732, #108133, #174160, #137381, #173081, #53982, #91842, #73416, #157900, #169856, #120118, #21444, #87552, #22518, #186098, #139519, #37728, #71267, #38798, #88629, #154685, #72340, #204464, #56118, #143810, #194637, #163223, #208742, #79818, #161083, #177335, #175218, #192493, #60369, #28949, #129733, #62504, #142733, #125464, #126532, #76620, #210879, #44145, #207687, #179472, #61442, #128669, #78749, #178407, #26802, #46279, #47352, #112395, #30018, #80896, #191426, #209807, #43092, #12673, #96103, #95033, #27877, #63577, #14805, #59307, #144872, #93973, #77689, #110266, #162158 ),
 ( #13745, #11615, #176275, #145930, #127609, #45217, #211942, #109205, #158951, #193574, #195717, #113467, #10545, #92905, #31096, #97168, #111332, #160014, #168265, #84876, #202869, #85951, #201801, #87011, #146986, #101117, #3594, #186640, #185565, #167204, #183442, #153083, #37194, #152026, #103270, #69672, #104343, #70731, #134728, #170387, #21976, #102199, #88086, #4659, #18793, #35046, #200735, #150965, #2530, #53443, #187705, #52385, #154158, #19866, #184497, #136844, #68605, #213003, #130780, #135778, #118513, #36116, #199677, #171466, #119581, #169332, #20916, #54517, #120661, #38266, #64640, #5725, #71804, #137915, #117448, #203935, #55583, #121738, #39333, #105430, #23055, #51320, #90233, #57722, #72881, #6805, #140065, #43627, #40417, #8962, #175753, #155224, #123880, #106520, #172546, #122820, #42565, #189845, #91311, #93447, #142202, #190901, #141152, #159485, #89172, #207161, #24131, #58784, #107604, #108667, #124938, #156298, #41492, #109742, #138989, #205010, #173635, #25206, #73970, #56657, #191960, #27344, #7882, #174697, #188779, #75037, #206087, #157368, #26271, #92388, #158424, #10024, #76099, #208217, #59849, #126001, #55213, #200368, #184127, #22679, #35750, #154849, #136474, #69294, #52016, #4288, #118142, #21601, #121359, #103971, #102893, #138606, #23761, #134364, #170013, #168952, #152706, #3227, #137543, #36811, #185187, #203561, #87707, #89866, #119201, #20555, #186259, #187334, #71431, #153779, #85567, #6433, #135405, #86639, #5349, #70360, #38963, #155917, #72508, #105048, #171083, #88791, #204629, #202495, #56280, #101824, #201428, #122439, #53068, #167892, #54147, #120284, #37893 ) ),
 .UNSPECIFIED., .F., .F., .T. ) 
 B_SPLINE_SURFACE_WITH_KNOTS ( ( 2, 2 ),
 ( 3, 2, 2, 2, 2, 2, 2, 2, 2, 2, 2, 2, 2, 2, 2, 2, 2, 2, 2, 2, 2, 2, 2, 2, 2, 2, 2, 2, 2, 2, 2, 2, 2, 2, 2, 2, 2, 2, 2, 2, 2, 2, 2, 2, 2, 2, 2, 2, 2, 2, 2, 2, 2, 2, 2, 2, 2, 2, 2, 2, 2, 2, 2, 2, 2, 2, 2, 2, 2, 2, 2, 2, 2, 2, 2, 2, 2, 2, 2, 2, 2, 2, 2, 2, 2, 2, 2, 2, 2, 2, 2, 2, 2, 2, 2, 2, 3 ),
 ( 0.000000000000000000, 1.000000000000000000 ),
 ( 0.000000000000000000, 0.01041666666666666609, 0.02083333333333333218, 0.03125000000000000000, 0.04166666666666666435, 0.05208333333333333565, 0.06250000000000000000, 0.07291666666666667129, 0.08333333333333332871, 0.09375000000000000000, 0.1041666666666666713, 0.1145833333333333287, 0.1250000000000000000, 0.1354166666666666574, 0.1458333333333333426, 0.1562500000000000000, 0.1666666666666666574, 0.1770833333333333426, 0.1875000000000000000, 0.1979166666666666574, 0.2083333333333333426, 0.2187500000000000000, 0.2291666666666666574, 0.2395833333333333426, 0.2500000000000000000, 0.2604166666666666852, 0.2708333333333333148, 0.2812500000000000000, 0.2916666666666666852, 0.3020833333333333148, 0.3125000000000000000, 0.3229166666666666852, 0.3333333333333333148, 0.3437500000000000000, 0.3541666666666666852, 0.3645833333333333148, 0.3750000000000000000, 0.3854166666666666852, 0.3958333333333333148, 0.4062500000000000000, 0.4166666666666666852, 0.4270833333333333148, 0.4375000000000000000, 0.4479166666666666852, 0.4583333333333333148, 0.4687500000000000000, 0.4791666666666666852, 0.4895833333333333148, 0.5000000000000000000, 0.5104166666666666297, 0.5208333333333333703, 0.5312500000000000000, 0.5416666666666666297, 0.5520833333333333703, 0.5625000000000000000, 0.5729166666666666297, 0.5833333333333333703, 0.5937500000000000000, 0.6041666666666666297, 0.6145833333333333703, 0.6250000000000000000, 0.6354166666666666297, 0.6458333333333333703, 0.6562500000000000000, 0.6666666666666666297, 0.6770833333333333703, 0.6875000000000000000, 0.6979166666666666297, 0.7083333333333333703, 0.7187500000000000000, 0.7291666666666666297, 0.7395833333333333703, 0.7500000000000000000, 0.7604166666666666297, 0.7708333333333333703, 0.7812500000000000000, 0.7916666666666666297, 0.8020833333333333703, 0.8125000000000000000, 0.8229166666666666297, 0.8333333333333333703, 0.8437500000000000000, 0.8541666666666666297, 0.8645833333333333703, 0.8750000000000000000, 0.8854166666666666297, 0.8958333333333333703, 0.9062500000000000000, 0.9166666666666666297, 0.9270833333333333703, 0.9375000000000000000, 0.9479166666666666297, 0.9583333333333333703, 0.9687500000000000000, 0.9791666666666666297, 0.9895833333333333703, 1.000000000000000000 ),
 .UNSPECIFIED. ) 
 GEOMETRIC_REPRESENTATION_ITEM ( )  RATIONAL_B_SPLINE_SURFACE ( (
 ( 1.000000000000000000, 0.8660254037844387076, 1.000000000000000000, 0.8660254037844387076, 1.000000000000000000, 0.8660254037844387076, 1.000000000000000000, 0.8660254037844387076, 1.000000000000000000, 0.8660254037844387076, 1.000000000000000000, 0.8660254037844387076, 1.000000000000000000, 0.8660254037844387076, 1.000000000000000000, 0.8660254037844387076, 1.000000000000000000, 0.8660254037844387076, 1.000000000000000000, 0.8660254037844387076, 1.000000000000000000, 0.8660254037844387076, 1.000000000000000000, 0.8660254037844387076, 1.000000000000000000, 0.8660254037844387076, 1.000000000000000000, 0.8660254037844387076, 1.000000000000000000, 0.8660254037844387076, 1.000000000000000000, 0.8660254037844387076, 1.000000000000000000, 0.8660254037844387076, 1.000000000000000000, 0.8660254037844387076, 1.000000000000000000, 0.8660254037844387076, 1.000000000000000000, 0.8660254037844387076, 1.000000000000000000, 0.8660254037844387076, 1.000000000000000000, 0.8660254037844387076, 1.000000000000000000, 0.8660254037844387076, 1.000000000000000000, 0.8660254037844387076, 1.000000000000000000, 0.8660254037844387076, 1.000000000000000000, 0.8660254037844387076, 1.000000000000000000, 0.8660254037844387076, 1.000000000000000000, 0.8660254037844387076, 1.000000000000000000, 0.8660254037844387076, 1.000000000000000000, 0.8660254037844387076, 1.000000000000000000, 0.8660254037844387076, 1.000000000000000000, 0.8660254037844387076, 1.000000000000000000, 0.8660254037844387076, 1.000000000000000000, 0.8660254037844387076, 1.000000000000000000, 0.8660254037844387076, 1.000000000000000000, 0.8660254037844387076, 1.000000000000000000, 0.8660254037844387076, 1.000000000000000000, 0.8660254037844387076, 1.000000000000000000, 0.8660254037844387076, 1.000000000000000000, 0.8660254037844387076, 1.000000000000000000, 0.8660254037844387076, 1.000000000000000000, 0.8660254037844387076, 1.000000000000000000, 0.8660254037844387076, 1.000000000000000000, 0.8660254037844387076, 1.000000000000000000, 0.8660254037844387076, 1.000000000000000000, 0.8660254037844387076, 1.000000000000000000, 0.8660254037844387076, 1.000000000000000000, 0.8660254037844387076, 1.000000000000000000, 0.8660254037844387076, 1.000000000000000000, 0.8660254037844387076, 1.000000000000000000, 0.8660254037844387076, 1.000000000000000000, 0.8660254037844387076, 1.000000000000000000, 0.8660254037844387076, 1.000000000000000000, 0.8660254037844387076, 1.000000000000000000, 0.8660254037844387076, 1.000000000000000000, 0.8660254037844387076, 1.000000000000000000, 0.8660254037844387076, 1.000000000000000000, 0.8660254037844387076, 1.000000000000000000, 0.8660254037844387076, 1.000000000000000000, 0.8660254037844387076, 1.000000000000000000, 0.8660254037844387076, 1.000000000000000000, 0.8660254037844387076, 1.000000000000000000, 0.8660254037844387076, 1.000000000000000000, 0.8660254037844387076, 1.000000000000000000, 0.8660254037844387076, 1.000000000000000000, 0.8660254037844387076, 1.000000000000000000, 0.8660254037844387076, 1.000000000000000000, 0.8660254037844387076, 1.000000000000000000, 0.8660254037844387076, 1.000000000000000000, 0.8660254037844387076, 1.000000000000000000, 0.8660254037844387076, 1.000000000000000000, 0.8660254037844387076, 1.000000000000000000, 0.8660254037844387076, 1.000000000000000000, 0.8660254037844387076, 1.000000000000000000, 0.8660254037844387076, 1.000000000000000000, 0.8660254037844387076, 1.000000000000000000, 0.8660254037844387076, 1.000000000000000000, 0.8660254037844387076, 1.000000000000000000, 0.8660254037844387076, 1.000000000000000000, 0.8660254037844387076, 1.000000000000000000, 0.8660254037844387076, 1.000000000000000000, 0.8660254037844387076, 1.000000000000000000, 0.8660254037844387076, 1.000000000000000000, 0.8660254037844387076, 1.000000000000000000, 0.8660254037844387076, 1.000000000000000000, 0.8660254037844387076, 1.000000000000000000, 0.8660254037844387076, 1.000000000000000000, 0.8660254037844387076, 1.000000000000000000, 0.8660254037844387076, 1.000000000000000000, 0.8660254037844387076, 1.000000000000000000, 0.8660254037844387076, 1.000000000000000000, 0.8660254037844387076, 1.000000000000000000, 0.8660254037844387076, 1.000000000000000000, 0.8660254037844387076, 1.000000000000000000, 0.8660254037844387076, 1.000000000000000000, 0.8660254037844387076, 1.000000000000000000),
 ( 1.000000000000000000, 0.8660254037844387076, 1.000000000000000000, 0.8660254037844387076, 1.000000000000000000, 0.8660254037844387076, 1.000000000000000000, 0.8660254037844387076, 1.000000000000000000, 0.8660254037844387076, 1.000000000000000000, 0.8660254037844387076, 1.000000000000000000, 0.8660254037844387076, 1.000000000000000000, 0.8660254037844387076, 1.000000000000000000, 0.8660254037844387076, 1.000000000000000000, 0.8660254037844387076, 1.000000000000000000, 0.8660254037844387076, 1.000000000000000000, 0.8660254037844387076, 1.000000000000000000, 0.8660254037844387076, 1.000000000000000000, 0.8660254037844387076, 1.000000000000000000, 0.8660254037844387076, 1.000000000000000000, 0.8660254037844387076, 1.000000000000000000, 0.8660254037844387076, 1.000000000000000000, 0.8660254037844387076, 1.000000000000000000, 0.8660254037844387076, 1.000000000000000000, 0.8660254037844387076, 1.000000000000000000, 0.8660254037844387076, 1.000000000000000000, 0.8660254037844387076, 1.000000000000000000, 0.8660254037844387076, 1.000000000000000000, 0.8660254037844387076, 1.000000000000000000, 0.8660254037844387076, 1.000000000000000000, 0.8660254037844387076, 1.000000000000000000, 0.8660254037844387076, 1.000000000000000000, 0.8660254037844387076, 1.000000000000000000, 0.8660254037844387076, 1.000000000000000000, 0.8660254037844387076, 1.000000000000000000, 0.8660254037844387076, 1.000000000000000000, 0.8660254037844387076, 1.000000000000000000, 0.8660254037844387076, 1.000000000000000000, 0.8660254037844387076, 1.000000000000000000, 0.8660254037844387076, 1.000000000000000000, 0.8660254037844387076, 1.000000000000000000, 0.8660254037844387076, 1.000000000000000000, 0.8660254037844387076, 1.000000000000000000, 0.8660254037844387076, 1.000000000000000000, 0.8660254037844387076, 1.000000000000000000, 0.8660254037844387076, 1.000000000000000000, 0.8660254037844387076, 1.000000000000000000, 0.8660254037844387076, 1.000000000000000000, 0.8660254037844387076, 1.000000000000000000, 0.8660254037844387076, 1.000000000000000000, 0.8660254037844387076, 1.000000000000000000, 0.8660254037844387076, 1.000000000000000000, 0.8660254037844387076, 1.000000000000000000, 0.8660254037844387076, 1.000000000000000000, 0.8660254037844387076, 1.000000000000000000, 0.8660254037844387076, 1.000000000000000000, 0.8660254037844387076, 1.000000000000000000, 0.8660254037844387076, 1.000000000000000000, 0.8660254037844387076, 1.000000000000000000, 0.8660254037844387076, 1.000000000000000000, 0.8660254037844387076, 1.000000000000000000, 0.8660254037844387076, 1.000000000000000000, 0.8660254037844387076, 1.000000000000000000, 0.8660254037844387076, 1.000000000000000000, 0.8660254037844387076, 1.000000000000000000, 0.8660254037844387076, 1.000000000000000000, 0.8660254037844387076, 1.000000000000000000, 0.8660254037844387076, 1.000000000000000000, 0.8660254037844387076, 1.000000000000000000, 0.8660254037844387076, 1.000000000000000000, 0.8660254037844387076, 1.000000000000000000, 0.8660254037844387076, 1.000000000000000000, 0.8660254037844387076, 1.000000000000000000, 0.8660254037844387076, 1.000000000000000000, 0.8660254037844387076, 1.000000000000000000, 0.8660254037844387076, 1.000000000000000000, 0.8660254037844387076, 1.000000000000000000, 0.8660254037844387076, 1.000000000000000000, 0.8660254037844387076, 1.000000000000000000, 0.8660254037844387076, 1.000000000000000000, 0.8660254037844387076, 1.000000000000000000, 0.8660254037844387076, 1.000000000000000000, 0.8660254037844387076, 1.000000000000000000, 0.8660254037844387076, 1.000000000000000000, 0.8660254037844387076, 1.000000000000000000, 0.8660254037844387076, 1.000000000000000000, 0.8660254037844387076, 1.000000000000000000, 0.8660254037844387076, 1.000000000000000000, 0.8660254037844387076, 1.000000000000000000, 0.8660254037844387076, 1.000000000000000000, 0.8660254037844387076, 1.000000000000000000, 0.8660254037844387076, 1.000000000000000000, 0.8660254037844387076, 1.000000000000000000, 0.8660254037844387076, 1.000000000000000000, 0.8660254037844387076, 1.000000000000000000, 0.8660254037844387076, 1.000000000000000000, 0.8660254037844387076, 1.000000000000000000, 0.8660254037844387076, 1.000000000000000000, 0.8660254037844387076, 1.000000000000000000, 0.8660254037844387076, 1.000000000000000000, 0.8660254037844387076, 1.000000000000000000) ) ) 
 REPRESENTATION_ITEM ( '' )  SURFACE ( )  );
#2409 = CARTESIAN_POINT ( 'NONE',  ( -4.709679585977568195, 8.347295923589904021, 0.7007048023343342980 ) ) ;
#2410 = CARTESIAN_POINT ( 'NONE',  ( 0.000000000000000000, 0.000000000000000000, -0.5000000000000004441 ) ) ;
#2411 = CARTESIAN_POINT ( 'NONE',  ( 6.086763352761943580, -0.2763008855245497331, -1.850001521387992565 ) ) ;
#2412 = CARTESIAN_POINT ( 'NONE',  ( 7.775764792637399836, 9.030479331953833011, -1.199719254218441611 ) ) ;
#2413 = CARTESIAN_POINT ( 'NONE',  ( 3.563037003841040828, -1.699336121007990918, -0.9075540061579747686 ) ) ;
#2414 = CARTESIAN_POINT ( 'NONE',  ( -3.411848212133334446, 7.132240014130863059, 0.7998128361456341429 ) ) ;
#2415 = CARTESIAN_POINT ( 'NONE',  ( 2.679707916995359263, 6.278076336469897711, -0.7998128361456291469 ) ) ;
#2416 = CARTESIAN_POINT ( 'NONE',  ( 1.364683531250000303, 9.317708333674735499, -0.7879004041258355073 ) ) ;
#2417 = CARTESIAN_POINT ( 'NONE',  ( -6.250472511100020334, 7.250971670160158311, 1.199719254218450271 ) ) ;
#2418 = CARTESIAN_POINT ( 'NONE',  ( 4.304877467538922531, 4.981110786005563007, 1.199719254218464037 ) ) ;
#2419 = CARTESIAN_POINT ( 'NONE',  ( -2.997761361953021009, 6.511488999004883205, -0.7216878364870458196 ) ) ;
#2420 = CARTESIAN_POINT ( 'NONE',  ( 0.7556430218940900501, 2.039295976802601995, -0.5688827987148316057 ) ) ;
#2421 = CARTESIAN_POINT ( 'NONE',  ( 7.242026607993941489, 11.60078147596829901, 0.7998128361456462443 ) ) ;
#2422 = CARTESIAN_POINT ( 'NONE',  ( -6.966220764712148572, 6.002124920821316323, 2.500000000000000444 ) ) ;
#2423 = CARTESIAN_POINT ( 'NONE',  ( 6.420769920452011448, -1.468259139554881409, 1.459777494992514857 ) ) ;
#2425 = CARTESIAN_POINT ( 'NONE',  ( 4.104435073692848768, 7.689436668370499106, -0.6928796192886893524 ) ) ;
#2424 = CARTESIAN_POINT ( 'NONE',  ( 1.593040506729075823, -0.6195558395927207584, 1.734028948791266345 ) ) ;
#2426 = CARTESIAN_POINT ( 'NONE',  ( 6.832946231607457399, 7.074118146404578589, -0.7216878364870257245 ) ) ;
#2428 = DIRECTION ( 'NONE',  ( 0.7797859179643625849, -0.6260462619842693810, -1.666848690107906998E-15 ) ) ;
#2427 = CARTESIAN_POINT ( 'NONE',  ( 3.255366281057017197, 6.812028071292901998, -0.7216878364870338292 ) ) ;
#2429 = CARTESIAN_POINT ( 'NONE',  ( 1.553083273963658639, -1.967900166212281476, -1.175304309182874096 ) ) ;
#2431 = EDGE_CURVE ( 'NONE', #156842, #15788, #193107, .T. ) ;
#2430 = DIRECTION ( 'NONE',  ( -0.6250000000000002220, 1.408756634010579298E-16, -0.7806247497997996776 ) ) ;
#2432 = VECTOR ( 'NONE', #111770, 1000.000000000000000 ) ;
#2433 = CARTESIAN_POINT ( 'NONE',  ( 5.806574285656749268, 1.713600856677459205, 0.9136399477176879724 ) ) ;
#2434 = EDGE_LOOP ( 'NONE', ( #151749, #136029 ) ) ;
#2435 = CARTESIAN_POINT ( 'NONE',  ( 7.659993601596707613, 9.959745173328078849, -1.443375672974058777 ) ) ;
#2436 = ADVANCED_FACE ( 'NONE', ( #136210 ), #138343, .T. ) ;
#2437 = CARTESIAN_POINT ( 'NONE',  ( 0.4045417950784445105, -1.998468379361338698, -0.2424310749817460697 ) ) ;
#2438 = CARTESIAN_POINT ( 'NONE',  ( -1.225000000000048050, 2.791666667349441688, -0.7072540797572957061 ) ) ;
#2440 = CARTESIAN_POINT ( 'NONE',  ( -11.25771003949915539, 3.534410846742664702, -5.930344140359695260 ) ) ;
#2439 = CARTESIAN_POINT ( 'NONE',  ( -7.153898609505128015, 11.49796547773133604, 0.7998128361456481317 ) ) ;
#2441 = CARTESIAN_POINT ( 'NONE',  ( -9.811677024507259759, 4.107325997343203028, 6.339424533126782002 ) ) ;
#2443 = CARTESIAN_POINT ( 'NONE',  ( 2.535733614153494742, 0.8364609567749015095, -1.559706200981937352 ) ) ;
#2442 = CARTESIAN_POINT ( 'NONE',  ( 3.978531085967525360, -0.2047937889433377179, -2.080580830362771305 ) ) ;
#2444 = CARTESIAN_POINT ( 'NONE',  ( -1.992711204631002198E-15, 2.999999999999989342, 1.224999999999989875 ) ) ;
#2446 = CARTESIAN_POINT ( 'NONE',  ( 5.648434673080700463, -1.810194131346474222, 1.406188067625735449 ) ) ;
#2445 = CARTESIAN_POINT ( 'NONE',  ( -11.99141368677939035, 8.009080577729674744, -0.5230012777734741602 ) ) ;
#2447 = CARTESIAN_POINT ( 'NONE',  ( 3.380519863291716387, 1.572804015177066805, -0.7453022471971497698 ) ) ;
#2448 = CARTESIAN_POINT ( 'NONE',  ( 9.622536337397022521, 12.24937836509514710, 1.599625672291281386 ) ) ;
#2449 = CARTESIAN_POINT ( 'NONE',  ( 3.514723022282209897, 1.734034291474368494, 0.002059465714070173124 ) ) ;
#2450 = CARTESIAN_POINT ( 'NONE',  ( 3.842362351650536301, -1.073271228610745309, 1.887301499758537116 ) ) ;
#2451 = CARTESIAN_POINT ( 'NONE',  ( 4.364835388595708743, 7.179726155748598515, 1.199719254218462483 ) ) ;
#2452 = CARTESIAN_POINT ( 'NONE',  ( 4.610564714392807240, 1.931124171932835809, 0.5807562064495259690 ) ) ;
#2453 = CARTESIAN_POINT ( 'NONE',  ( 1.250000000000001110, 7.216295638291068821E-14, 2.052068128417951609 ) ) ;
#2454 = CARTESIAN_POINT ( 'NONE',  ( -1.201851678989727383E-14, 3.868750000682817713, -1.732050807568863648 ) ) ;
#2455 = CARTESIAN_POINT ( 'NONE',  ( 1.764547866544708521, -1.364041108321904616, 1.360535031132574568 ) ) ;
#2456 = CARTESIAN_POINT ( 'NONE',  ( 0.6823417656249969321, 15.02604166700806410, -1.181850606188757036 ) ) ;
#2457 = CARTESIAN_POINT ( 'NONE',  ( 5.238630872344578471, 1.322862460432130849, -1.784462157271723859 ) ) ;
#2458 = ORIENTED_EDGE ( 'NONE', *, *, #64463, .F. ) ;
#2459 = CARTESIAN_POINT ( 'NONE',  ( -0.2110808730067273986, 0.0005491059566040295322, -1.796958327270286704 ) ) ;
#2460 = CARTESIAN_POINT ( 'NONE',  ( -0.7500000000000006661, 1.108333333333356929, -1.299038105676652011 ) ) ;
#2461 = CARTESIAN_POINT ( 'NONE',  ( 5.262536180398716290, 9.291375977107183104, -0.7998128361456291469 ) ) ;
#2462 = CARTESIAN_POINT ( 'NONE',  ( 4.433153041544209749, 7.155467067568137551, -1.082531754730548412 ) ) ;
#2463 = CARTESIAN_POINT ( 'NONE',  ( -3.285556943750000070, -2.209374999522041527, 0.000000000000000000 ) ) ;
#2464 = CARTESIAN_POINT ( 'NONE',  ( 0.5576789645300848086, -1.902086909048054331, 1.147088156025797057 ) ) ;
#2465 = CARTESIAN_POINT ( 'NONE',  ( 5.687936657224680559, -1.243353266631580523, -1.517579924814119074 ) ) ;
#2466 = CARTESIAN_POINT ( 'NONE',  ( 7.782016984564049444, 11.06247500109133064, 1.082531754730557072 ) ) ;
#2467 = CARTESIAN_POINT ( 'NONE',  ( 4.370663978927085580, 5.060324124126027279, -1.009771797811724214 ) ) ;
#2468 = CARTESIAN_POINT ( 'NONE',  ( 6.837213258907510749, -2.025504081721161143, 1.008097451810068268 ) ) ;
#2469 = ADVANCED_FACE ( 'NONE', ( #168689 ), #64454, .T. ) ;
#2470 = CARTESIAN_POINT ( 'NONE',  ( 3.542423274920540432, 7.354853930707762721, -1.734723475976807094E-15 ) ) ;
#2471 = CARTESIAN_POINT ( 'NONE',  ( -5.641601317062259646, 5.754492089426966217, -0.7216878364870338292 ) ) ;
#2472 = CARTESIAN_POINT ( 'NONE',  ( 3.912594259961211574, 0.7396031425229695477, 1.925699983396757409 ) ) ;
#2473 = CARTESIAN_POINT ( 'NONE',  ( -5.928993247877788697, 5.811580298812519807, 0.7998128361456341429 ) ) ;
#2474 = CARTESIAN_POINT ( 'NONE',  ( -1.500000000000011324, 3.702083334016152971, 0.8660254037844403729 ) ) ;
#2475 = CARTESIAN_POINT ( 'NONE',  ( -0.6823417656250003738, -0.2822916663252489355, -1.181850606188749264 ) ) ;
#2477 = B_SPLINE_CURVE_WITH_KNOTS ( 'NONE', 3,
 ( #116896, #51849, #151485, #213248 ),
 .UNSPECIFIED., .F., .F.,
 ( 4, 4 ),
 ( 0.001076902096689604481, 0.001673025196799804177 ),
 .UNSPECIFIED. ) ;
#2476 = CARTESIAN_POINT ( 'NONE',  ( 6.169203917683822702, 0.1378038699498609632, -1.865550841118966297 ) ) ;
#2478 = CARTESIAN_POINT ( 'NONE',  ( 4.324694450628805420, 0.7358571774197277815, -1.570421820497726051 ) ) ;
#2479 = CARTESIAN_POINT ( 'NONE',  ( 4.739680933654325301, 1.736262504677583474, 0.1214163294094624396 ) ) ;
#2480 = CARTESIAN_POINT ( 'NONE',  ( -2.423460580168067757, 1.405705671057797312, 11.75284646727700455 ) ) ;
#2481 = CARTESIAN_POINT ( 'NONE',  ( 2.279227788079383643, 2.094250403060330168, -0.9326617097511098464 ) ) ;
#2482 = CARTESIAN_POINT ( 'NONE',  ( 1.364683531249988535, 4.176041667008081326, 0.7879004041258500513 ) ) ;
#2483 = CARTESIAN_POINT ( 'NONE',  ( 5.513254163946260000, -2.039523011555996579, 0.4591751592910776614 ) ) ;
#2484 = CARTESIAN_POINT ( 'NONE',  ( 0.09336763325077861164, -1.840659761701424646, -0.04852334659839750014 ) ) ;
#2485 = CARTESIAN_POINT ( 'NONE',  ( -4.586165880992525423, 5.350526861157986147, -7.499999999999997335 ) ) ;
#2486 =( NAMED_UNIT ( * ) PLANE_ANGLE_UNIT ( ) SI_UNIT ( $, .RADIAN. ) );
#2487 = CARTESIAN_POINT ( 'NONE',  ( 2.162732623366144136, 1.242727809108796322, 1.587836805404294171 ) ) ;
#2488 = CARTESIAN_POINT ( 'NONE',  ( 5.605114358992040913, 6.317488171369740613, -1.123711807521186490 ) ) ;
#2489 = CARTESIAN_POINT ( 'NONE',  ( 6.938157974219377522, 13.99567801284426416, -9.395936565436949550 ) ) ;
#2490 = CARTESIAN_POINT ( 'NONE',  ( -8.688077508258798431, 9.030511935923748013, -0.7998128361456291469 ) ) ;
#2491 = CARTESIAN_POINT ( 'NONE',  ( 5.982172092127724383, 8.002286745614243912, -1.599625672291262513 ) ) ;
#2492 = CARTESIAN_POINT ( 'NONE',  ( 2.895306150831237879, -0.1582170333116576511, -2.114654843180157950 ) ) ;
#2493 = VECTOR ( 'NONE', #161029, 1000.000000000000000 ) ;
#2494 = CARTESIAN_POINT ( 'NONE',  ( 1.364683531249986981, -1.115624999658580752, 0.000000000000000000 ) ) ;
#2495 = CARTESIAN_POINT ( 'NONE',  ( 5.127504350819418910, -1.732488751877172772, 0.5760870007271366999 ) ) ;
#2496 = ORIENTED_EDGE ( 'NONE', *, *, #183589, .T. ) ;
#2497 = CARTESIAN_POINT ( 'NONE',  ( -5.094831863685302942, 9.165997284266655498, 0.7998128361456291469 ) ) ;
#2498 = DIRECTION ( 'NONE',  ( -8.638326563840814399E-31, 0.000000000000000000, -1.000000000000000000 ) ) ;
#2500 = EDGE_CURVE ( 'NONE', #54417, #1642, #189065, .T. ) ;
#2499 = CARTESIAN_POINT ( 'NONE',  ( 7.309254211098760834, 8.660456346770972758, 1.082531754730549967 ) ) ;
#2501 = CARTESIAN_POINT ( 'NONE',  ( -1.642778471875000035, -0.6052083328553746755, -2.845375778867859751 ) ) ;
#2502 = CARTESIAN_POINT ( 'NONE',  ( -6.175902666224832416, 7.163973517805802160, -1.199719254218446718 ) ) ;
#2503 = CARTESIAN_POINT ( 'NONE',  ( 2.812765223479243737, -0.5904890161391795900, -1.931511402468567340 ) ) ;
#2504 = CARTESIAN_POINT ( 'NONE',  ( 6.774453055690137226, -1.363307072557031985, 1.735998097611628932 ) ) ;
#2505 = CARTESIAN_POINT ( 'NONE',  ( -5.157951095356222204, 4.982307464195829816, 0.000000000000000000 ) ) ;
#2506 = CARTESIAN_POINT ( 'NONE',  ( 4.504654980070036174, 0.4933668235826896287, 1.794306199697106363 ) ) ;
#2507 = CARTESIAN_POINT ( 'NONE',  ( 8.041957671200231417, 12.53403438304231976, 1.040834085586084257E-14 ) ) ;
#2508 = CARTESIAN_POINT ( 'NONE',  ( -9.569358774130488854, 4.446955548196734220, -7.167287524826102540 ) ) ;
#2509 = EDGE_LOOP ( 'NONE', ( #47711, #94882 ) ) ;
#2510 = CARTESIAN_POINT ( 'NONE',  ( -2.428882075142555497, 5.985446187641602300, 1.040834085586084257E-14 ) ) ;
#2511 = CARTESIAN_POINT ( 'NONE',  ( -8.290974629956718189, 9.631557475493025322, -1.199719254218446718 ) ) ;
#2513 = CARTESIAN_POINT ( 'NONE',  ( -4.201283080389795366, 7.561618497949153195, 0.9685097419542560981 ) ) ;
#2512 = CARTESIAN_POINT ( 'NONE',  ( -5.641074431737709283, 8.738948049406083385, -1.199719254218452047 ) ) ;
#2514 = CARTESIAN_POINT ( 'NONE',  ( -0.6823417656250246877, -0.4489583329919111243, 1.181850606188755259 ) ) ;
#2515 = CARTESIAN_POINT ( 'NONE',  ( 1.704000572024838123, -1.251590786289292101, -1.200144391261132482 ) ) ;
#2516 = CARTESIAN_POINT ( 'NONE',  ( 1.411604581429444893, 1.170971978790593448, -1.287647580301202410 ) ) ;
#2518 = CARTESIAN_POINT ( 'NONE',  ( 9.097157885089661278, 9.715698408800516717, 1.040834085586084257E-14 ) ) ;
#2517 = CARTESIAN_POINT ( 'NONE',  ( 6.270204019816865149, 1.180490267363063062, 1.982795515311958079 ) ) ;
#2519 = CARTESIAN_POINT ( 'NONE',  ( 4.523580528814945545, 5.306540700819438960, 1.199719254218452047 ) ) ;
#2520 = CARTESIAN_POINT ( 'NONE',  ( 1.862644954548669185, -1.459483730259679257, 1.455164547919563844 ) ) ;
#2521 = CARTESIAN_POINT ( 'NONE',  ( 4.656335691289526402, 7.519809842224722374, -1.199719254218452047 ) ) ;
#2522 = CARTESIAN_POINT ( 'NONE',  ( 6.731773689652298387, -2.096994807688298934, -0.9412720059410217832 ) ) ;
#2523 = CARTESIAN_POINT ( 'NONE',  ( -0.6125000000000314637, 0.9583333333333388104, -1.060881119635965764 ) ) ;
#2524 = CARTESIAN_POINT ( 'NONE',  ( -5.692444392891315097, 7.734547439830227411, -1.599625672291271394 ) ) ;
#2525 = CARTESIAN_POINT ( 'NONE',  ( 0.3914019522827461017, 1.459281966464224256, 1.325753552615087871 ) ) ;
#2526 = AXIS2_PLACEMENT_3D ( 'NONE', #145885, #98183, #29972 ) ;
#2528 = CARTESIAN_POINT ( 'NONE',  ( -5.912764389335557702, 8.951956649983198844, 1.082531754730550855 ) ) ;
#2527 = CARTESIAN_POINT ( 'NONE',  ( 5.203337695038355193, 1.683698669361912259, -0.9069238330124268499 ) ) ;
#2529 = CARTESIAN_POINT ( 'NONE',  ( 6.252570086353132162, 0.6882034672392455255, 2.096894461246688213 ) ) ;
#2530 = CARTESIAN_POINT ( 'NONE',  ( -1.225000000000016076, 1.812500000682795598, -2.081668171172168513E-14 ) ) ;
#2531 = CARTESIAN_POINT ( 'NONE',  ( 5.031484404002891431, 5.042689024191078673, 0.7216878364870328300 ) ) ;
#2532 = CARTESIAN_POINT ( 'NONE',  ( -6.071018923869249129, 10.30488218781460574, 0.7998128361456291469 ) ) ;
#2533 = CARTESIAN_POINT ( 'NONE',  ( 0.5748750247985534578, -1.461244816878112029, 1.394459567027491076 ) ) ;
#2534 = ORIENTED_EDGE ( 'NONE', *, *, #164125, .F. ) ;
#2535 = CARTESIAN_POINT ( 'NONE',  ( 3.856711057068095805, 0.8274802039119494301, 2.154294293310366371 ) ) ;
#2536 = CARTESIAN_POINT ( 'NONE',  ( 4.562918044398325712, 1.517878595006398212, -1.242988302126393441 ) ) ;
#2537 = CARTESIAN_POINT ( 'NONE',  ( 0.9890223832832998330, 0.1386981244183866091, 1.956888703154149312 ) ) ;
#2538 = CARTESIAN_POINT ( 'NONE',  ( 4.229780737783593203, 4.037091736943370535, -0.7216878364870188411 ) ) ;
#2539 = CARTESIAN_POINT ( 'NONE',  ( 6.634380643896210294, -6.684699857435318471, 6.783773228136968036 ) ) ;
#2540 = ORIENTED_EDGE ( 'NONE', *, *, #181210, .T. ) ;
#2541 = CARTESIAN_POINT ( 'NONE',  ( 0.07561343334091479018, 1.573685453729951833, 1.416787448489342127 ) ) ;
#2543 = CARTESIAN_POINT ( 'NONE',  ( -9.006694118179950692, 9.402231314165087284, 1.040834085586084257E-14 ) ) ;
#2542 = CARTESIAN_POINT ( 'NONE',  ( -5.274285450916075035, 6.112086766612214284, 1.199719254218450271 ) ) ;
#2544 = CARTESIAN_POINT ( 'NONE',  ( 0.02305342982030639948, -1.130023889514218505, -1.454075609423427728 ) ) ;
#2545 = CARTESIAN_POINT ( 'NONE',  ( 2.799877792657178066, -1.606015216909290277, -1.461049007858437054 ) ) ;
#2546 = CARTESIAN_POINT ( 'NONE',  ( 9.605087238846238051, 12.70381962237584972, -7.196083043797907308 ) ) ;
#2547 = CARTESIAN_POINT ( 'NONE',  ( 0.1410940620840978044, 2.031152781523197337, 0.6094965309384676733 ) ) ;
#2548 = CARTESIAN_POINT ( 'NONE',  ( -0.7500000000000215383, 1.472916667349486008, 1.299038105676659116 ) ) ;
#2549 = CARTESIAN_POINT ( 'NONE',  ( 9.565441069641300587, 11.11843498845840905, -1.199719254218440723 ) ) ;
#2550 = CARTESIAN_POINT ( 'NONE',  ( 11.88168329227126563, 13.88000000000000256, -1.685799833707129380 ) ) ;
#2551 = CARTESIAN_POINT ( 'NONE',  ( 6.468016842275610578, 6.857101109195174793, 0.6445861549769070775 ) ) ;
#2552 = EDGE_LOOP ( 'NONE', ( #164602, #2842, #180087, #82500 ) ) ;
#2553 = CARTESIAN_POINT ( 'NONE',  ( 2.319669497725483254, -1.999663683883694532, 0.4976976026799494468 ) ) ;
#2555 = CARTESIAN_POINT ( 'NONE',  ( 1.499999999999990896, 5.025000000000022560, 1.214306433183764966E-14 ) ) ;
#2554 = CARTESIAN_POINT ( 'NONE',  ( -9.504429378379839477, 11.04725468198666150, 1.199719254218462483 ) ) ;
#2556 = CARTESIAN_POINT ( 'NONE',  ( -1.364683531250012516, 2.030208333674750953, 0.7879004041258379498 ) ) ;
#2557 = PLANE ( 'NONE',  #139685 ) ;
#2558 = CARTESIAN_POINT ( 'NONE',  ( -5.690973801483992567, 5.856266416790857576, 2.499999999999998668 ) ) ;
#2559 = ORIENTED_EDGE ( 'NONE', *, *, #185505, .F. ) ;
#2560 = CARTESIAN_POINT ( 'NONE',  ( 4.037688526304391345, -1.829018870347882242, 0.5580751363460645376 ) ) ;
#2561 = B_SPLINE_CURVE_WITH_KNOTS ( 'NONE', 3,
 ( #59467, #111488, #126690, #58410, #193728, #8580, #125626, #176430, #94134, #192652 ),
 .UNSPECIFIED., .F., .F.,
 ( 4, 2, 2, 2, 4 ),
 ( 0.000000000000000000, 0.0003474354322518759990, 0.0006948708645037519980, 0.001042306296755630491, 0.001389741729007509200 ),
 .UNSPECIFIED. ) ;
#2562 = PRESENTATION_LAYER_ASSIGNMENT (  '', '', ( #68271 ) ) ;
#2563 = CARTESIAN_POINT ( 'NONE',  ( 0.4019237886466884846, 9.457585450998170273, -1.499999999999994449 ) ) ;
#2564 = B_SPLINE_CURVE_WITH_KNOTS ( 'NONE', 3,
 ( #171227, #154989, #56421, #6574 ),
 .UNSPECIFIED., .F., .F.,
 ( 4, 4 ),
 ( 5.038702538383248430E-05, 0.0001172081591904372197 ),
 .UNSPECIFIED. ) ;
#2565 = CARTESIAN_POINT ( 'NONE',  ( 1.247787707462020723, -1.783668181329477465, -1.391623327695093115 ) ) ;
#2566 = CARTESIAN_POINT ( 'NONE',  ( -3.277320446201389181, 4.846626492033466072, 1.599625672291267398 ) ) ;
#2567 = CARTESIAN_POINT ( 'NONE',  ( 1.142488074861398140, 1.746299531065167221, 0.4817477467682490522 ) ) ;
#2568 = CARTESIAN_POINT ( 'NONE',  ( 1.305720528479116682, -1.067273574023764438, -1.590657944389769707 ) ) ;
#2569 = CARTESIAN_POINT ( 'NONE',  ( 1.785682506433339478, -1.950172559450613852, 0.6955597780969878796 ) ) ;
#2570 = CARTESIAN_POINT ( 'NONE',  ( 1.364683531249988757, 0.6968750003414209138, 0.000000000000000000 ) ) ;
#2572 = ADVANCED_FACE ( 'NONE', ( #9393 ), #208641, .F. ) ;
#2571 = CIRCLE ( 'NONE', #5975, 12.00000000000000178 ) ;
#2573 = CARTESIAN_POINT ( 'NONE',  ( 6.825078400183573812, 0.002648415797040087893, 1.855566311045192540 ) ) ;
#2574 = CARTESIAN_POINT ( 'NONE',  ( 5.848256421918945236, 1.924412893870678820, 0.09223618542448899782 ) ) ;
#2576 = CARTESIAN_POINT ( 'NONE',  ( 5.488371254093075358, 7.473176909139983337, -1.250075884424824757 ) ) ;
#2575 = CARTESIAN_POINT ( 'NONE',  ( 6.358075476802443227, 2.201304964888863402, -0.1578768562689457922 ) ) ;
#2577 = CARTESIAN_POINT ( 'NONE',  ( 1.364683531249988757, 1.634375000341421691, 0.000000000000000000 ) ) ;
#2578 = CARTESIAN_POINT ( 'NONE',  ( 3.947761307511790552, 1.492003129663575622, 1.424497906600069363 ) ) ;
#2579 = CARTESIAN_POINT ( 'NONE',  ( -6.575868197828002693, 7.630599971342813426, 1.199719254218450271 ) ) ;
#2580 = CARTESIAN_POINT ( 'NONE',  ( 7.079328764629950754, 11.41096732537697633, 0.7998128361456462443 ) ) ;
#2581 = CARTESIAN_POINT ( 'NONE',  ( -1.284279953904156280, 2.921639714193936754, 0.7750000000000117906 ) ) ;
#2582 = CARTESIAN_POINT ( 'NONE',  ( 4.819033534653518025, 7.709623992816043270, -1.199719254218452047 ) ) ;
#2584 = CARTESIAN_POINT ( 'NONE',  ( -0.7500000000000215383, 3.191666666666689967, 1.299038105676671107 ) ) ;
#2583 = CARTESIAN_POINT ( 'NONE',  ( 5.333084004640892495, 0.1517067650670254342, 2.100546829335631749 ) ) ;
#2585 = CARTESIAN_POINT ( 'NONE',  ( 0.5554291532160166023, 1.804893407318912901, -1.206520995182088329 ) ) ;
#2586 = CARTESIAN_POINT ( 'NONE',  ( -1.364683531250012516, 0.8427083336747532849, 0.7879004041258379498 ) ) ;
#2587 = CARTESIAN_POINT ( 'NONE',  ( 4.604844690042745547, 1.674155836469687575, -1.367402732809947397 ) ) ;
#2588 = CARTESIAN_POINT ( 'NONE',  ( 5.567059059060062154, -1.590727130084067964, 1.244318111769521229 ) ) ;
#2589 = CARTESIAN_POINT ( 'NONE',  ( -3.782361668532609134, 7.356579680022602652, 1.040834085586084257E-14 ) ) ;
#2590 = AXIS2_PLACEMENT_3D ( 'NONE', #106985, #204391, #120046 ) ;
#2591 = EDGE_CURVE ( 'NONE', #127623, #140029, #92727, .T. ) ;
#2594 = CARTESIAN_POINT ( 'NONE',  ( 5.748293942514166588, 7.729428904398431222, -1.443375672974057666 ) ) ;
#2593 = CARTESIAN_POINT ( 'NONE',  ( 3.285556943750000070, -2.734374999522042771, 0.000000000000000000 ) ) ;
#2592 = CARTESIAN_POINT ( 'NONE',  ( 7.526711554241970248, 8.810193563817646734, -1.199719254218452047 ) ) ;
#2595 = CARTESIAN_POINT ( 'NONE',  ( -4.932134020321308654, 8.976183133675331050, 0.7998128361456291469 ) ) ;
#2596 = CARTESIAN_POINT ( 'NONE',  ( 3.046111529846948329, 0.9110102549910354952, 1.799122713138465279 ) ) ;
#2597 = CARTESIAN_POINT ( 'NONE',  ( -8.748035429315585532, 11.22912730566677553, -1.599625672291263179 ) ) ;
#2599 = CARTESIAN_POINT ( 'NONE',  ( -10.97067990664313264, -5.250949308401990479, 0.2977236940312626978 ) ) ;
#2598 = CARTESIAN_POINT ( 'NONE',  ( -2.916975605234527702, 6.554888639415577423, 1.040834085586084257E-14 ) ) ;
#2601 = CARTESIAN_POINT ( 'NONE',  ( 4.806723615010448736E-13, -7.868798029037617603, -9.500000000000001776 ) ) ;
#2600 = CARTESIAN_POINT ( 'NONE',  ( 5.049776242366147194, 0.6816224847111511664, -2.051488706027407183 ) ) ;
#2602 = CARTESIAN_POINT ( 'NONE',  ( -11.89942855770814134, 11.29999999999999893, 0.6999999999999992895 ) ) ;
#2603 = CARTESIAN_POINT ( 'NONE',  ( 4.000000000000012434, 4.999999999999997335, -0.7500000000000006661 ) ) ;
#2605 = CARTESIAN_POINT ( 'NONE',  ( 4.569935513796226978, -0.9480243344661150040, 1.779636403143824985 ) ) ;
#2604 = CARTESIAN_POINT ( 'NONE',  ( -6.019457014343129408, 9.966524250134902729, 0.000000000000000000 ) ) ;
#2606 = CARTESIAN_POINT ( 'NONE',  ( 0.7499999999999920064, 4.983333333333353821, 1.299038105676669330 ) ) ;
#2607 = CARTESIAN_POINT ( 'NONE',  ( 0.4160739966224377140, 1.193427498895651029, -1.245624518738875697 ) ) ;
#2608 = CARTESIAN_POINT ( 'NONE',  ( 4.603875680292229156, 7.528882839386387360, 1.199719254218452047 ) ) ;
#2610 = CARTESIAN_POINT ( 'NONE',  ( 0.2619794211619203006, -6.848541063415906294, 10.99716886186657838 ) ) ;
#2609 = CARTESIAN_POINT ( 'NONE',  ( 8.934460041725669655, 9.525884258209195821, 1.040834085586084257E-14 ) ) ;
#2611 = CARTESIAN_POINT ( 'NONE',  ( -11.75854610579106563, 8.612401473491297921, 2.412033672967001774 ) ) ;
#2612 = CARTESIAN_POINT ( 'NONE',  ( 5.026551685794930613, 1.789549103570491573, 0.5443708928771497924 ) ) ;
#2613 = CARTESIAN_POINT ( 'NONE',  ( 0.04752084976851479736, -1.839644132637440865, 0.8178810061007844023 ) ) ;
#2614 = CARTESIAN_POINT ( 'NONE',  ( -4.217958839219735800, 3.978389137448586244, 0.5316758947214468289 ) ) ;
#2615 = CARTESIAN_POINT ( 'NONE',  ( -7.227905289416814760, 7.605180057173966723, -0.7216878364870338292 ) ) ;
#2616 = ORIENTED_EDGE ( 'NONE', *, *, #192096, .F. ) ;
#2618 = CARTESIAN_POINT ( 'NONE',  ( 0.2105648349144396136, 1.930425396462841725, 0.5826343419270894053 ) ) ;
#2617 = CARTESIAN_POINT ( 'NONE',  ( 2.420699464796825850, -0.8139657014685426351, -1.958238820914718792 ) ) ;
#2619 = CARTESIAN_POINT ( 'NONE',  ( 1.142488074861398140, 1.746299531065167221, 0.4817477467682490522 ) ) ;
#2620 = CARTESIAN_POINT ( 'NONE',  ( 5.352436782344940802, 9.466536356036257871, 0.000000000000000000 ) ) ;
#2621 = CARTESIAN_POINT ( 'NONE',  ( 5.963787895669663719, 2.130530397400759668, -0.3648857593604309391 ) ) ;
#2622 = CARTESIAN_POINT ( 'NONE',  ( 6.612626235163189925, 8.737816579155630592, -1.599625672291262513 ) ) ;
#2624 = CARTESIAN_POINT ( 'NONE',  ( 0.8135319083415553099, -1.217954555017298324, -1.478650609923468195 ) ) ;
#2623 = CARTESIAN_POINT ( 'NONE',  ( -6.417086777969760902, 6.381022750586497594, 0.7998128361456341429 ) ) ;
#2625 = FACE_OUTER_BOUND ( 'NONE', #17021, .T. ) ;
#2626 = DIRECTION ( 'NONE',  ( 0.000000000000000000, 1.000000000000000000, 0.000000000000000000 ) ) ;
#2627 = CARTESIAN_POINT ( 'NONE',  ( 0.6823417656249882723, -0.3447916663252489911, 1.181850606188755259 ) ) ;
#2628 = CARTESIAN_POINT ( 'NONE',  ( 2.846849069189655967, 5.304779099821139710, -1.082531754730543083 ) ) ;
#2629 = CARTESIAN_POINT ( 'NONE',  ( -2.676845263694313637, 5.210404343363602919, -1.199719254218446718 ) ) ;
#2630 = CARTESIAN_POINT ( 'NONE',  ( 3.854492016355787420, 0.7758605394001509836, 2.017853709245204463 ) ) ;
#2631 = CARTESIAN_POINT ( 'NONE',  ( -6.048345925472225382, 8.149765894507963182, 1.443375672974058777 ) ) ;
#2632 = CARTESIAN_POINT ( 'NONE',  ( 5.221298555038576872, 9.105615724271411082, 0.000000000000000000 ) ) ;
#2633 = CARTESIAN_POINT ( 'NONE',  ( 1.090261293813089560, 1.267680250814690934, 1.699812782343253170 ) ) ;
#2634 = CARTESIAN_POINT ( 'NONE',  ( 6.370122744524995717, 0.9412729668686821149, 1.564051812004362940 ) ) ;
#2635 = EDGE_CURVE ( 'NONE', #192481, #119756, #206152, .T. ) ;
#2636 = CARTESIAN_POINT ( 'NONE',  ( 1.721884408201577399, -1.091793429770457458, -1.641225607529321229 ) ) ;
#2637 = CARTESIAN_POINT ( 'NONE',  ( 4.939673314881130040, -1.814047719456039154, 0.6055163330952323397 ) ) ;
#2638 = VERTEX_POINT ( 'NONE', #191324 ) ;
#2639 = CARTESIAN_POINT ( 'NONE',  ( 9.484899655072776881, -6.713792789267319705, -0.3525790917591882789 ) ) ;
#2640 = CARTESIAN_POINT ( 'NONE',  ( 6.602011381505620946, 0.7551138498248446407, -1.819252348156335852 ) ) ;
#2641 = CARTESIAN_POINT ( 'NONE',  ( 2.027192386733965179, -1.268372964689370663, -1.470586975900304516 ) ) ;
#2642 = ORIENTED_EDGE ( 'NONE', *, *, #49219, .T. ) ;
#2643 = CARTESIAN_POINT ( 'NONE',  ( -4.767627293860968507, 5.591261926706423857, -1.199719254218453823 ) ) ;
#2645 = DIRECTION ( 'NONE',  ( -5.578564026256490882E-16, -1.000000000000000000, -9.066213480720158442E-32 ) ) ;
#2644 = CARTESIAN_POINT ( 'NONE',  ( -4.065465959251405081, 5.836405933916976707, -1.599625672291271394 ) ) ;
#2647 = CARTESIAN_POINT ( 'NONE',  ( 4.353576723319599218, 8.093273587265928271, -0.7216878364870357165 ) ) ;
#2646 = CARTESIAN_POINT ( 'NONE',  ( 5.282873410819217241, 9.315102745931094219, -0.7998128361456281477 ) ) ;
#2649 = ORIENTED_EDGE ( 'NONE', *, *, #149426, .T. ) ;
#2648 = CARTESIAN_POINT ( 'NONE',  ( 4.951771945676144426, -1.355037094400749487, -1.349591858340569717 ) ) ;
#2650 = CARTESIAN_POINT ( 'NONE',  ( 3.668774463136436736, -1.482526648764719734, 1.634931011441637771 ) ) ;
#2651 = CARTESIAN_POINT ( 'NONE',  ( 1.589210545419886378, -0.3244246349418925535, -2.182665228674217861 ) ) ;
#2652 = CARTESIAN_POINT ( 'NONE',  ( 1.536019160937515116, 8.701056780447510519, 2.509677374737102618 ) ) ;
#2653 = CARTESIAN_POINT ( 'NONE',  ( 0.3813228709106940006, 0.1872568833237615027, -1.903067810102520241 ) ) ;
#2654 = CARTESIAN_POINT ( 'NONE',  ( 0.07661050522431848975, 5.726661425590173771, -2.304854160881860903 ) ) ;
#2655 = DIRECTION ( 'NONE',  ( -7.387867266669436732E-31, -1.000000000000000000, 8.546850786086437571E-32 ) ) ;
#2656 = CARTESIAN_POINT ( 'NONE',  ( -5.204170427930421283E-15, 3.447199233515649386, -11.99999999999998224 ) ) ;
#2657 = CARTESIAN_POINT ( 'NONE',  ( 3.508316276398337319, 2.070544812355082254, 0.002818362966339192730 ) ) ;
#2658 = CARTESIAN_POINT ( 'NONE',  ( -4.577849422908604637, 8.492574760035358494, -0.7998128361456281477 ) ) ;
#2659 = VECTOR ( 'NONE', #54397, 1000.000000000000000 ) ;
#2660 = CARTESIAN_POINT ( 'NONE',  ( -6.370507937826336509, 6.842553425211714391, 0.6026486057824770315 ) ) ;
#2662 = CARTESIAN_POINT ( 'NONE',  ( 1.112450467520700537, -0.9725818059473789745, -1.930612204972524282 ) ) ;
#2661 = CARTESIAN_POINT ( 'NONE',  ( -4.253507506385335368, 5.985511395581417204, 1.599625672291267398 ) ) ;
#2663 = CARTESIAN_POINT ( 'NONE',  ( 3.755584314896889264, 2.174856280799509545, -0.2696606696684644700 ) ) ;
#2664 = CARTESIAN_POINT ( 'NONE',  ( -1.992711204631002198E-15, 2.999999999999989342, 1.224999999999989875 ) ) ;
#2665 = CARTESIAN_POINT ( 'NONE',  ( 4.638297949650961982, 5.544340708415133712, -1.082531754730548412 ) ) ;
#2666 = CARTESIAN_POINT ( 'NONE',  ( 0.4355862708379890647, -6.583980363594969631, 9.606148981167454082 ) ) ;
#2667 = CARTESIAN_POINT ( 'NONE',  ( -1.364683531250010295, 13.44270833367473017, 0.7879004041258445001 ) ) ;
#2668 = CARTESIAN_POINT ( 'NONE',  ( -4.793689830883590020, 7.750332681742931662, 1.199719254218452935 ) ) ;
#2669 = UNCERTAINTY_MEASURE_WITH_UNIT (LENGTH_MEASURE( 1.000000000000000082E-05 ), #201758, 'distance_accuracy_value', 'NONE');
#2670 = CARTESIAN_POINT ( 'NONE',  ( 6.135404405475363809, 0.5537102809010217008, 1.643457313873160741 ) ) ;
#2671 = CARTESIAN_POINT ( 'NONE',  ( -9.002250809794000830, 11.52571191622492464, -1.443375672974059665 ) ) ;
#2672 =( GEOMETRIC_REPRESENTATION_CONTEXT ( 3 ) GLOBAL_UNCERTAINTY_ASSIGNED_CONTEXT ( ( #41987 ) ) GLOBAL_UNIT_ASSIGNED_CONTEXT ( ( #14906, #152407, #132983 ) ) REPRESENTATION_CONTEXT ( 'NONE', 'WORKASPACE' ) );
#2673 = CARTESIAN_POINT ( 'NONE',  ( 3.502843950909264592, 0.4983820457637299639, 2.009271733256080772 ) ) ;
#2674 = CARTESIAN_POINT ( 'NONE',  ( 4.359064374566766986, -0.001685027751544953406, -2.117403152337670846 ) ) ;
#2675 = CARTESIAN_POINT ( 'NONE',  ( 7.447506452608354088, 7.583179037664891098, 0.7998128361456341429 ) ) ;
#2676 = CARTESIAN_POINT ( 'NONE',  ( 1.364683531249988535, 4.905208333674756283, -0.7879004041258300672 ) ) ;
#2677 = CARTESIAN_POINT ( 'NONE',  ( 3.116014175596728109, 1.960399024780419275, -0.1881816519722582237 ) ) ;
#2678 = CARTESIAN_POINT ( 'NONE',  ( 1.160255710619631397, 1.910328232974867868, 0.09094507755665059978 ) ) ;
#2679 = CARTESIAN_POINT ( 'NONE',  ( 4.980587577705724911, -0.2770739538935252932, -2.275404589957805701 ) ) ;
#2681 = ADVANCED_FACE ( 'NONE', ( #110168 ), #108034, .T. ) ;
#2680 = CARTESIAN_POINT ( 'NONE',  ( 3.000428103051573814, -0.5303778429210231904, -1.746945217264872507 ) ) ;
#2682 = CARTESIAN_POINT ( 'NONE',  ( 5.551137550152489553, 5.441024994791534120, 0.7998128361456352531 ) ) ;
#2683 = CARTESIAN_POINT ( 'NONE',  ( 5.083944415000174466, 7.914723669933440675, -1.082531754730549078 ) ) ;
#2684 = CARTESIAN_POINT ( 'NONE',  ( -6.989391883044787868, 8.113044270762433285, -1.199719254218446718 ) ) ;
#2685 = CARTESIAN_POINT ( 'NONE',  ( 4.394793396725252599, -1.953840400094335905, -0.4849018877997012256 ) ) ;
#2686 = CARTESIAN_POINT ( 'NONE',  ( 4.276187414114787089, -1.004825795036960567, -1.684713053385626269 ) ) ;
#2687 = CARTESIAN_POINT ( 'NONE',  ( -7.965578943228732278, 9.251929174310385307, -1.199719254218446718 ) ) ;
#2688 = CARTESIAN_POINT ( 'NONE',  ( -3.927058049452637700, 7.733318157670055371, -0.7998128361456281477 ) ) ;
#2690 = EDGE_CURVE ( 'NONE', #41918, #170318, #144540, .T. ) ;
#2689 = CARTESIAN_POINT ( 'NONE',  ( 0.1755611466353629579, -0.002217706044341584935, -2.244164702216360219 ) ) ;
#2692 = CARTESIAN_POINT ( 'NONE',  ( 6.104346055523492964, -0.6409971714030155976, -1.649885601521252410 ) ) ;
#2691 = CARTESIAN_POINT ( 'NONE',  ( 0.7672655991019157184, 2.013871065616902989, -0.5614242917610365868 ) ) ;
#2693 = CARTESIAN_POINT ( 'NONE',  ( 5.346851039111029991, 6.199209027673978412, 7.500000000000000000 ) ) ;
#2694 = CARTESIAN_POINT ( 'NONE',  ( 2.133021248740565756, -1.956732443736847182, 0.9868821405488172882 ) ) ;
#2695 = CARTESIAN_POINT ( 'NONE',  ( 6.597592293924691376, -1.739768381213904647, 0.05089061930978015791 ) ) ;
#2696 = CARTESIAN_POINT ( 'NONE',  ( 5.940443861082012944, 10.08226827123770697, 0.7998128361456462443 ) ) ;
#2697 = CARTESIAN_POINT ( 'NONE',  ( 0.2333690889706925564, 0.2409277441041447754, -2.087868073146467829 ) ) ;
#2698 = CARTESIAN_POINT ( 'NONE',  ( 0.1172359533097135365, -1.692718506494130359, 0.3305547394890032686 ) ) ;
#2699 = CARTESIAN_POINT ( 'NONE',  ( 0.6503308509665306492, -0.2843267121918050533, -2.280655268134044622 ) ) ;
#2700 = CARTESIAN_POINT ( 'NONE',  ( 0.9256184737543894370, -1.394389637717853514, -1.690728713229103342 ) ) ;
#2701 = CARTESIAN_POINT ( 'NONE',  ( 2.596532132193625664, -2.201043451360765957, -0.1612727490639675743 ) ) ;
#2702 = CARTESIAN_POINT ( 'NONE',  ( 6.496539221175353873, 2.146586416477539672, 0.3252249059467678394 ) ) ;
#2703 = CARTESIAN_POINT ( 'NONE',  ( -1.500000000000051514, 3.920833333333356485, 0.8660254037844170583 ) ) ;
#2704 = CARTESIAN_POINT ( 'NONE',  ( 0.9017390913304748068, -2.064370131783893392, 0.4699791444322827250 ) ) ;
#2705 = CARTESIAN_POINT ( 'NONE',  ( 6.727182134110196721, 7.051813866762763006, 2.787205683092201181 ) ) ;
#2706 = CARTESIAN_POINT ( 'NONE',  ( 5.579104889113781773, -0.04751220352695872257, -1.925958990430853612 ) ) ;
#2707 = ORIENTED_EDGE ( 'NONE', *, *, #46793, .T. ) ;
#2709 = CARTESIAN_POINT ( 'NONE',  ( -1.500000000000011324, 5.629166666666693963, -0.8660254037844313801 ) ) ;
#2708 = CARTESIAN_POINT ( 'NONE',  ( 1.259778491951433654, 2.257442302724984806, -0.3979086512072607107 ) ) ;
#2710 = CARTESIAN_POINT ( 'NONE',  ( 2.361091307074211887, 5.906356958228550447, 0.7998128361456462443 ) ) ;
#2711 = CARTESIAN_POINT ( 'NONE',  ( 6.654354466208897811, 6.657835053532175529, 0.7998128361456341429 ) ) ;
#2712 = CIRCLE ( 'NONE', #189522, 0.04999999999999985706 ) ;
#2713 = CARTESIAN_POINT ( 'NONE',  ( 5.321006124507968060, 1.683121437214535554, -1.449644825538060733 ) ) ;
#2714 = CARTESIAN_POINT ( 'NONE',  ( -6.710922849084449915, 10.77323439066645783, 0.000000000000000000 ) ) ;
#2715 = SURFACE_STYLE_USAGE ( .BOTH. , #5913 ) ;
#2716 = CARTESIAN_POINT ( 'NONE',  ( 5.748293942514166588, 7.729428904398431222, -1.443375672974057666 ) ) ;
#2717 = CARTESIAN_POINT ( 'NONE',  ( -9.300530188850304469, 9.952966096521256745, 1.040834085586084257E-14 ) ) ;
#2718 = EDGE_CURVE ( 'NONE', #5398, #119510, #136351, .T. ) ;
#2719 = CARTESIAN_POINT ( 'NONE',  ( 4.421367491832258523, 8.172362817197399210, 0.7216878364870257245 ) ) ;
#2720 = CARTESIAN_POINT ( 'NONE',  ( 2.303361484738715159, 1.314996338066702242, -1.528741580717301263 ) ) ;
#2722 = CARTESIAN_POINT ( 'NONE',  ( 0.7255239074139888666, 0.2060675592777498066, -2.052282084198739920 ) ) ;
#2721 = CARTESIAN_POINT ( 'NONE',  ( 7.564559641420864899, 10.91273778404466199, -1.199719254218446718 ) ) ;
#2723 = CARTESIAN_POINT ( 'NONE',  ( -11.88172094500854037, 13.87999994398404269, 1.685553348215819147 ) ) ;
#2724 = CARTESIAN_POINT ( 'NONE',  ( 6.658462837642799670, 7.901199744405670522, 1.082531754730549967 ) ) ;
#2725 = FACE_OUTER_BOUND ( 'NONE', #33291, .T. ) ;
#2726 = CARTESIAN_POINT ( 'NONE',  ( -1.201851678989727383E-14, 4.071875000341425022, 1.575800808251672791 ) ) ;
#2727 = CARTESIAN_POINT ( 'NONE',  ( 3.996163734398257894, -0.6867376513691285655, -2.081127982183433645 ) ) ;
#2728 = CARTESIAN_POINT ( 'NONE',  ( 1.178361531996233280, 1.528742360773158282, 1.314995429398260196 ) ) ;
#2729 = CARTESIAN_POINT ( 'NONE',  ( 0.9777802892061361328, -1.796362506263927017, -0.4033719513514141264 ) ) ;
#2730 = B_SPLINE_CURVE_WITH_KNOTS ( 'NONE', 3,
 ( #213653, #83672, #34915, #98882, #85818, #65279, #135648, #200607, #84749, #49067 ),
 .UNSPECIFIED., .F., .F.,
 ( 4, 3, 3, 4 ),
 ( 0.000000000000000000, 4.502046072368915222E-05, 9.004093402560281781E-05, 0.0001800865003231029719 ),
 .UNSPECIFIED. ) ;
#2731 = CARTESIAN_POINT ( 'NONE',  ( 5.407889476941767803, -1.028354611087534787, -2.048866343328694661 ) ) ;
#2732 = CARTESIAN_POINT ( 'NONE',  ( 2.853255899669316697, 1.832232481769331844, -0.1808706098178694266 ) ) ;
#2733 = CARTESIAN_POINT ( 'NONE',  ( 8.772289083241844310, 10.19309100432570148, -1.199719254218446718 ) ) ;
#2734 = SURFACE_STYLE_USAGE ( .BOTH. , #182568 ) ;
#2735 = CARTESIAN_POINT ( 'NONE',  ( 4.471595891589618788, 1.770651423122941548, -0.4439726157009425411 ) ) ;
#2736 = CARTESIAN_POINT ( 'NONE',  ( 4.869767617671093340, -0.2496050341583149201, -2.000857388266870984 ) ) ;
#2737 = CARTESIAN_POINT ( 'NONE',  ( -8.503988664269602538, 10.94440607977979063, 1.599625672291269396 ) ) ;
#2739 = CARTESIAN_POINT ( 'NONE',  ( -5.582925393777276035, 9.735439736040634173, 0.7998128361456291469 ) ) ;
#2738 = CARTESIAN_POINT ( 'NONE',  ( 4.504895162230450723, 1.751659092587343869, -1.432031112679124085 ) ) ;
#2740 = CARTESIAN_POINT ( 'NONE',  ( 6.422895033429510292, 1.963595603779586973, 0.7616278367365038049 ) ) ;
#2741 = CARTESIAN_POINT ( 'NONE',  ( -1.814759087649598923, 3.975067388632297138, -0.4606438099578613055 ) ) ;
#2742 = CARTESIAN_POINT ( 'NONE',  ( 3.156751980976373329, -0.5984545454679365273, -1.982000093670479135 ) ) ;
#2743 = CARTESIAN_POINT ( 'NONE',  ( 9.999301985278609806, 11.62460605670194447, 1.199719254218452047 ) ) ;
#2744 = CARTESIAN_POINT ( 'NONE',  ( -1.752700365193352367E-14, 1.609375000341425777, -1.570758158831794260 ) ) ;
#2745 = SHAPE_DEFINITION_REPRESENTATION ( #178641, #121983 ) ;
#2747 = CARTESIAN_POINT ( 'NONE',  ( 1.611812915071403784, -1.911997954552616008, 0.2354761707349817823 ) ) ;
#2746 = CARTESIAN_POINT ( 'NONE',  ( -7.828943636887387925, 11.22118577875556156, 1.199719254218453823 ) ) ;
#2748 = CARTESIAN_POINT ( 'NONE',  ( -10.50000000000000533, 11.00709944181895494, 3.599999999999998312 ) ) ;
#2749 = CARTESIAN_POINT ( 'NONE',  ( 6.930521655090660538, -1.214226768402311363, 1.551031149239000761 ) ) ;
#2750 = CARTESIAN_POINT ( 'NONE',  ( 5.031484404002889654, 6.003058238492422483, 1.082531754730549078 ) ) ;
#2751 = CARTESIAN_POINT ( 'NONE',  ( 5.449628763635895545, 6.258197423388296876, 1.014392677442396806 ) ) ;
#2752 = CARTESIAN_POINT ( 'NONE',  ( -0.4019237886467001974, 11.08258545099816494, 1.500000000000001998 ) ) ;
#2753 = STYLED_ITEM ( 'NONE', ( #168925 ), #37195 ) ;
#2754 = CARTESIAN_POINT ( 'NONE',  ( -4.451154503988200339, 4.087435097607984957, 1.214306433183764966E-14 ) ) ;
#2755 = CARTESIAN_POINT ( 'NONE',  ( 1.811064542976594360, -0.5979718353220222493, -2.139333889645285147 ) ) ;
#2756 = CARTESIAN_POINT ( 'NONE',  ( 3.786240212431398966, -1.039621666623831597, 1.831390154885542243 ) ) ;
#2757 = CARTESIAN_POINT ( 'NONE',  ( -6.720001414228860881, 7.869031733802326123, -1.199719254218452047 ) ) ;
#2758 = CARTESIAN_POINT ( 'NONE',  ( 7.287671262545424966, 8.461036880179857889, -1.199719254218451159 ) ) ;
#2759 = CARTESIAN_POINT ( 'NONE',  ( 6.895359103435129811, -1.662453150013998515, 0.8363214020891978073 ) ) ;
#2760 = CARTESIAN_POINT ( 'NONE',  ( 7.135668919494039031, 7.219368582364847242, 1.040834085586084257E-14 ) ) ;
#2761 = CARTESIAN_POINT ( 'NONE',  ( 4.904298879841284098, 6.744767997946721216, 1.599625672291267398 ) ) ;
#2762 = CARTESIAN_POINT ( 'NONE',  ( -5.560252395380252288, 7.580323442733986283, 1.443375672974058777 ) ) ;
#2763 = CARTESIAN_POINT ( 'NONE',  ( -7.375272376154081932, 10.58793962461302485, -1.082531754730543971 ) ) ;
#2764 = CARTESIAN_POINT ( 'NONE',  ( 0.9672155168029163974, -1.668165459610539081, 1.309123814877902969 ) ) ;
#2765 = CARTESIAN_POINT ( 'NONE',  ( -5.250750630242457362, 9.347902511916677426, 0.000000000000000000 ) ) ;
#2767 = CARTESIAN_POINT ( 'NONE',  ( 4.070719198475009293, 1.388998261151509039, -1.385754695631277844 ) ) ;
#2766 = CARTESIAN_POINT ( 'NONE',  ( -4.156403723172807449E-14, 0.3125000000000094924, 1.414508159514557439 ) ) ;
#2768 = CARTESIAN_POINT ( 'NONE',  ( 3.415052781332720055, 1.953485055394106107, 0.9259690932504063277 ) ) ;
#2769 = CARTESIAN_POINT ( 'NONE',  ( 1.628196140939692338, 0.1813696128579282696, 1.832309401408799276 ) ) ;
#2770 = CARTESIAN_POINT ( 'NONE',  ( -4.328009424535094851, 7.229878788426305825, -0.9977569098220413490 ) ) ;
#2771 = CARTESIAN_POINT ( 'NONE',  ( -1.364683531250000748, -1.178124999658580752, 0.000000000000000000 ) ) ;
#2772 = CARTESIAN_POINT ( 'NONE',  ( 4.681465254972009049, -0.8165918992961908041, 1.536851246062352905 ) ) ;
#2774 = AXIS2_PLACEMENT_3D ( 'NONE', #61267, #40770, #7156 ) ;
#2773 = CARTESIAN_POINT ( 'NONE',  ( -3.501245407923440300, 14.00000000000179057, -11.28115623562633019 ) ) ;
#2775 = CARTESIAN_POINT ( 'NONE',  ( 4.636525346193557162, 7.392734756325715750, -1.082531754730549078 ) ) ;
#2776 = CARTESIAN_POINT ( 'NONE',  ( -10.07169253693141897, 5.946554136026001913, 5.792750394403223702 ) ) ;
#2777 = CARTESIAN_POINT ( 'NONE',  ( 1.850665834824256173, 0.6780317805383448970, 2.052694239800388676 ) ) ;
#2778 = CARTESIAN_POINT ( 'NONE',  ( 3.304064382408095302, -1.779354530013575131, 0.9478943420064069869 ) ) ;
#2779 = CARTESIAN_POINT ( 'NONE',  ( 0.4019237886466816012, 12.95758545099816850, -1.499999999999998668 ) ) ;
#2780 = CARTESIAN_POINT ( 'NONE',  ( 1.745224485312408813, -1.826185749030174499, 1.156423465944363294 ) ) ;
#2781 = CARTESIAN_POINT ( 'NONE',  ( 3.063307058708428787, 0.2908816738307045680, -1.949781715572605600 ) ) ;
#2782 = CARTESIAN_POINT ( 'NONE',  ( 6.609000000000011532, 3.695567819995113634, 2.514302272609474809 ) ) ;
#2783 = CARTESIAN_POINT ( 'NONE',  ( 3.526839302598220982, -1.793260235690095072, 0.7459913709994684394 ) ) ;
#2786 = ORIENTED_EDGE ( 'NONE', *, *, #64280, .T. ) ;
#2785 = CARTESIAN_POINT ( 'NONE',  ( -2.875737979874388284, 6.369128386579808954, -0.7216878364870458196 ) ) ;
#2784 = CARTESIAN_POINT ( 'NONE',  ( -9.666600336419303829, 11.34041714965307968, 1.082531754730558626 ) ) ;
#2787 = CARTESIAN_POINT ( 'NONE',  ( -3.811250578772977349, 7.460559751961507224, -0.7216878364870458196 ) ) ;
#2788 = CARTESIAN_POINT ( 'NONE',  ( 5.899733120602060232, 6.912052057904395141, -1.199719254218452047 ) ) ;
#2789 = CARTESIAN_POINT ( 'NONE',  ( -6.005335696210345020, 5.970922831858983315, 0.7998128361456281477 ) ) ;
#2791 = ORIENTED_EDGE ( 'NONE', *, *, #98727, .F. ) ;
#2790 = CARTESIAN_POINT ( 'NONE',  ( -6.967964602780620353, 7.093989889524320525, 0.000000000000000000 ) ) ;
#2792 = CARTESIAN_POINT ( 'NONE',  ( -9.788623718942277563, 10.52240854829523187, 1.040834085586084257E-14 ) ) ;
#2793 = CARTESIAN_POINT ( 'NONE',  ( 0.3060867131535297547, -0.5861141839358529060, 2.127432003918772629 ) ) ;
#2794 = CARTESIAN_POINT ( 'NONE',  ( -1.642778471875000035, -3.317708332855374476, -2.845375778867859751 ) ) ;
#2795 = CARTESIAN_POINT ( 'NONE',  ( 4.469553177461598636, -0.3394721387663233170, 1.932013773527320843 ) ) ;
#2796 = CARTESIAN_POINT ( 'NONE',  ( 1.178361531996233280, 1.528742360773158060, 1.314995429398259974 ) ) ;
#2797 = ORIENTED_EDGE ( 'NONE', *, *, #2169, .T. ) ;
#2798 = CARTESIAN_POINT ( 'NONE',  ( 3.380171168471556520, -2.115091482053657934, -0.09962960183704583361 ) ) ;
#2799 = CARTESIAN_POINT ( 'NONE',  ( -1.201851678989727383E-14, 3.368750000682815049, -1.732050807568863648 ) ) ;
#2801 = CARTESIAN_POINT ( 'NONE',  ( -4.706651882238427120, 8.642844295920152575, 1.040834085586084257E-14 ) ) ;
#2800 = CARTESIAN_POINT ( 'NONE',  ( 0.07479286986305544449, 6.948552162806721277, -2.450557996216149892 ) ) ;
#2802 = CARTESIAN_POINT ( 'NONE',  ( 2.624749632297512569, -1.717891791495285592, 0.6627527109525217508 ) ) ;
#2803 = EDGE_LOOP ( 'NONE', ( #93624, #58508, #129338, #132929, #183373, #210468, #60869 ) ) ;
#2804 = CARTESIAN_POINT ( 'NONE',  ( -8.320953590485107298, 10.73086516036454618, 1.599625672291269396 ) ) ;
#2805 = CARTESIAN_POINT ( 'NONE',  ( 3.602337597214539753E-15, 1.000000000682806034, -1.225000000000015410 ) ) ;
#2806 = CARTESIAN_POINT ( 'NONE',  ( 5.308877466510794285, -0.5174029350529658622, -2.056363676157816123 ) ) ;
#2807 = CARTESIAN_POINT ( 'NONE',  ( 6.925078400183548588, 0.0006614011395407459748, 1.855452278108092656 ) ) ;
#2808 = CARTESIAN_POINT ( 'NONE',  ( 5.937581207780954884, 9.014596278131406848, -1.199719254218440723 ) ) ;
#2809 = CARTESIAN_POINT ( 'NONE',  ( 5.571578285044489043, 1.987195396197571462, -0.5455906853745869922 ) ) ;
#2811 = CARTESIAN_POINT ( 'NONE',  ( 2.946635061770470632, -1.506786691049965432, -1.057933238436038925 ) ) ;
#2810 = CARTESIAN_POINT ( 'NONE',  ( 1.064655064206044166, 1.412561167129450457, -1.211817338188374782 ) ) ;
#2812 = CARTESIAN_POINT ( 'NONE',  ( 9.585778300061798873, 11.14216175728232550, -1.199719254218440723 ) ) ;
#2813 = CARTESIAN_POINT ( 'NONE',  ( -7.095713291905736853, 9.371694488680407886, 1.599625672291269396 ) ) ;
#2814 = DIRECTION ( 'NONE',  ( -1.000000000000000000, 0.000000000000000000, 0.000000000000000000 ) ) ;
#2815 = ADVANCED_FACE ( 'NONE', ( #11520 ), #165360, .T. ) ;
#2816 = CARTESIAN_POINT ( 'NONE',  ( 1.946200625105892312, 0.8427435547867198062, -2.039832142532324255 ) ) ;
#2817 = CARTESIAN_POINT ( 'NONE',  ( 4.868612525405347391, -1.482742447731852709, 1.708856814797095725 ) ) ;
#2819 = CARTESIAN_POINT ( 'NONE',  ( -7.537970219518083326, 9.817384560903001045, -1.443375672974059665 ) ) ;
#2818 = B_SPLINE_CURVE_WITH_KNOTS ( 'NONE', 3,
 ( #18413, #150579, #1083, #68218, #17337, #180927, #164686, #117058, #84488, #197176, #201414, #133282, #19477, #33611, #67147, #16269, #2141, #135392, #53053, #166820, #52002, #82354, #168939, #118128, #36796, #48812 ),
 .UNSPECIFIED., .F., .F.,
 ( 4, 2, 2, 2, 2, 2, 2, 2, 2, 2, 2, 2, 4 ),
 ( 8.741117365843410899E-19, 0.0002250267552868354852, 0.0003375401329302527942, 0.0003937968217519613131, 0.0004219251661628155726, 0.0004500535105736698321, 0.0004641176827790974768, 0.0004781818549845251215, 0.0005063101993953802483, 0.0005625668882170907189, 0.0006750802658605122020, 0.0009001070211473549514, 0.001800214042294726599 ),
 .UNSPECIFIED. ) ;
#2820 = CARTESIAN_POINT ( 'NONE',  ( 4.886864132303106345, -1.708302746381512804, -0.6034029335190493892 ) ) ;
#2821 = CARTESIAN_POINT ( 'NONE',  ( 4.258935762849770157, -0.005977556496831581273, -1.915903398800692159 ) ) ;
#2822 = CARTESIAN_POINT ( 'NONE',  ( -0.6823417656249969321, 5.530208333674756283, -1.181850606188749264 ) ) ;
#2823 = EDGE_CURVE ( 'NONE', #173974, #75921, #6244, .T. ) ;
#2824 = CARTESIAN_POINT ( 'NONE',  ( 3.994965595081632959, 1.666078911148192843, -1.053691615683423510 ) ) ;
#2825 = CARTESIAN_POINT ( 'NONE',  ( 5.541831131927607679, 0.7570117910807551143, -1.710825945835430462 ) ) ;
#2826 = CARTESIAN_POINT ( 'NONE',  ( 5.248444859377932481, -1.846993913715170077, -0.2278608691909170259 ) ) ;
#2827 = CARTESIAN_POINT ( 'NONE',  ( 1.730579039399254279E-05, -9.953931234596407052, 9.500331159997204011 ) ) ;
#2829 = CIRCLE ( 'NONE', #144696, 0.07999999999999993228 ) ;
#2828 = AXIS2_PLACEMENT_3D ( 'NONE', #8850, #126966, #62933 ) ;
#2830 = CARTESIAN_POINT ( 'NONE',  ( 0.4972802279516430612, -0.2910764605805628014, 1.995268990643041640 ) ) ;
#2832 = CARTESIAN_POINT ( 'NONE',  ( 1.207801281821162975, -0.5101631384078918474, 2.043215687033891559 ) ) ;
#2831 = CARTESIAN_POINT ( 'NONE',  ( -3.429849674132948500, 5.024577257953626308, -1.443375672974051449 ) ) ;
#2833 = CARTESIAN_POINT ( 'NONE',  ( 10.18233705906309972, 11.83814697611718714, 1.199719254218450271 ) ) ;
#2835 = CARTESIAN_POINT ( 'NONE',  ( -9.829825065107822724, 11.42688298316931572, 1.199719254218462483 ) ) ;
#2834 = DIRECTION ( 'NONE',  ( -0.6507913734559641616, -0.7592566023653004592, 0.000000000000000000 ) ) ;
#2836 = CARTESIAN_POINT ( 'NONE',  ( 2.865608904542978674, -1.736054085904148669, -1.217558864107195715 ) ) ;
#2837 = CARTESIAN_POINT ( 'NONE',  ( 2.977454500823585093, 6.499579965040511276, -0.5808385047149626779 ) ) ;
#2838 = CARTESIAN_POINT ( 'NONE',  ( 1.371359653073561891, -1.734546099648653472, -1.034550878434212784 ) ) ;
#2839 = CARTESIAN_POINT ( 'NONE',  ( 0.6823417656249882723, 2.426041667008084435, -1.181850606188749264 ) ) ;
#2840 = FACE_OUTER_BOUND ( 'NONE', #99831, .T. ) ;
#2841 = CARTESIAN_POINT ( 'NONE',  ( 4.955668840994886359, 5.740367388370866131, 1.199719254218462483 ) ) ;
#2842 = ORIENTED_EDGE ( 'NONE', *, *, #188328, .T. ) ;
#2843 = CARTESIAN_POINT ( 'NONE',  ( 2.460438939752377152, 0.9218109643280818499, 1.955300211207489758 ) ) ;
#2844 = CARTESIAN_POINT ( 'NONE',  ( 6.890000000000047642, 4.686644152421160392, 2.842524626796953946 ) ) ;
#2847 = CARTESIAN_POINT ( 'NONE',  ( -3.894033820048823813, 8.999999999999998224, -0.7749999999999979128 ) ) ;
#2846 = FACE_OUTER_BOUND ( 'NONE', #122610, .T. ) ;
#2845 = CARTESIAN_POINT ( 'NONE',  ( 5.734172623936983904, 5.654565914206774124, 0.7998128361456352531 ) ) ;
#2848 = LINE ( 'NONE', #201050, #103212 ) ;
#2849 = CARTESIAN_POINT ( 'NONE',  ( -7.727353211424288659, -6.453073674884717725, 7.679448064523577422 ) ) ;
#2850 = CARTESIAN_POINT ( 'NONE',  ( -6.805829924380121909, 8.963220883242035697, 1.443375672974078761 ) ) ;
#2851 = CARTESIAN_POINT ( 'NONE',  ( 0.8377433530848135135, 0.8832496248250313320, -2.005872107257236969 ) ) ;
#2852 = CARTESIAN_POINT ( 'NONE',  ( -1.179069862577986269E-15, -8.198316280121948907, -9.513083155459820972 ) ) ;
#2854 = CARTESIAN_POINT ( 'NONE',  ( -1.364683531250014514, 11.58854166700806410, -0.7879004041258335089 ) ) ;
#2853 = CARTESIAN_POINT ( 'NONE',  ( 1.147787885906520033, -1.784999543274916611, -1.390116309797536864 ) ) ;
#2855 = CARTESIAN_POINT ( 'NONE',  ( -7.700141177557535244, 11.07091624287075859, -1.199719254218446718 ) ) ;
#2856 = CARTESIAN_POINT ( 'NONE',  ( -3.863710589770277259, 6.491117540498504646, 1.082531754730560403 ) ) ;
#2857 = CARTESIAN_POINT ( 'NONE',  ( 0.6823417656249882723, 1.988541667008083991, -1.181850606188749264 ) ) ;
#2858 = CARTESIAN_POINT ( 'NONE',  ( 4.594747986498664005, 8.374059380672374431, -0.03693212167796278145 ) ) ;
#2859 = CARTESIAN_POINT ( 'NONE',  ( -1.500000000000015099, 10.22916666666667318, -0.8660254037844309360 ) ) ;
#2860 = CARTESIAN_POINT ( 'NONE',  ( 4.072648179469573471, -1.610461668677556801, -0.6182406629154230115 ) ) ;
#2861 = CARTESIAN_POINT ( 'NONE',  ( 7.851580356089786328, 8.332800968292465527, 0.000000000000000000 ) ) ;
#2862 = CARTESIAN_POINT ( 'NONE',  ( 2.143481220494340533, 0.6824282661134513095, -1.633078482676100007 ) ) ;
#2863 = CARTESIAN_POINT ( 'NONE',  ( 2.965492324039080252, -1.647071928310759326, -1.157207142784054010 ) ) ;
#2864 = CARTESIAN_POINT ( 'NONE',  ( 5.772568991252683190, -1.404203161598962968, 1.702366421003978392 ) ) ;
#2865 = EDGE_LOOP ( 'NONE', ( #190728, #42834, #5149, #106081 ) ) ;
#2866 = CARTESIAN_POINT ( 'NONE',  ( 4.605726162909654420, 1.499404818428259345, 1.353488595782571524 ) ) ;
#2867 = CARTESIAN_POINT ( 'NONE',  ( -5.367048706163331850, 7.354919138647580290, -1.599625672291271394 ) ) ;
#2868 = CARTESIAN_POINT ( 'NONE',  ( 5.712517600013327979, 1.944077172375497264, 0.5350714256760412679 ) ) ;
#2870 = EDGE_LOOP ( 'NONE', ( #204909, #147403, #53351, #186088 ) ) ;
#2869 = CARTESIAN_POINT ( 'NONE',  ( 4.763805435907580765, 0.5614848394812530508, -1.722472548925155778 ) ) ;
#2871 = CARTESIAN_POINT ( 'NONE',  ( 2.817106861211693847, -0.1851908181382568019, 1.861470920997858380 ) ) ;
#2872 = CARTESIAN_POINT ( 'NONE',  ( -11.94654170777226376, 11.15174326158935969, -1.134972293687621647 ) ) ;
#2873 = CARTESIAN_POINT ( 'NONE',  ( 2.056764645581514728, 0.4224895836346024280, 1.864965418913032913 ) ) ;
#2874 = DIRECTION ( 'NONE',  ( -1.000000000000000000, 0.000000000000000000, 3.491481338843133355E-15 ) ) ;
#2875 = CARTESIAN_POINT ( 'NONE',  ( -11.29167836119662738, 5.103960725615834804, -5.764738477843053488 ) ) ;
#2876 = DIRECTION ( 'NONE',  ( 0.000000000000000000, -1.000000000000000000, 0.000000000000000000 ) ) ;
#2877 = CARTESIAN_POINT ( 'NONE',  ( 1.364683531249988535, 3.176041667008084435, 0.7879004041258500513 ) ) ;
#2878 = CARTESIAN_POINT ( 'NONE',  ( 0.01762790050853849447, -0.5081247445114078776, 1.843608005305336528 ) ) ;
#2879 = CARTESIAN_POINT ( 'NONE',  ( 6.373741612200174878, 6.608655767087927124, 0.7216878364870328300 ) ) ;
#2880 = CARTESIAN_POINT ( 'NONE',  ( 1.240593047436115759, -1.913272810121857237, -0.4332019784048374289 ) ) ;
#2881 = DIRECTION ( 'NONE',  ( 0.7592566023653005702, -0.6507913734559639396, 0.000000000000000000 ) ) ;
#2882 = CARTESIAN_POINT ( 'NONE',  ( -7.123883369337781879, 7.275895117174344229, 0.7998128361456341429 ) ) ;
#2883 = CARTESIAN_POINT ( 'NONE',  ( 5.273731010124149243, 0.4114677744767555878, -2.080124947408354963 ) ) ;
#2885 = CARTESIAN_POINT ( 'NONE',  ( -15.75000000000000000, 9.799999999999982947, 3.199999999999997957 ) ) ;
#2884 = CARTESIAN_POINT ( 'NONE',  ( 9.154780037725547714, 11.70366268214508487, 1.599625672291279388 ) ) ;
#2886 = CARTESIAN_POINT ( 'NONE',  ( 5.694591516259816188, -0.4762896487527890632, -1.912855984147985744 ) ) ;
#2887 = CARTESIAN_POINT ( 'NONE',  ( 1.364683531249988535, 2.363541667008088432, 0.7879004041258500513 ) ) ;
#2888 = CARTESIAN_POINT ( 'NONE',  ( 0.3342400628787962624, -1.080556536492575770, -1.698484060877824886 ) ) ;
#2889 = ORIENTED_EDGE ( 'NONE', *, *, #89791, .F. ) ;
#2890 = CARTESIAN_POINT ( 'NONE',  ( 1.335737955381975928, 0.6106153762303926369, -2.027287256620951439 ) ) ;
#2891 = CARTESIAN_POINT ( 'NONE',  ( 10.91404093077409243, 8.232440706712328193, 5.004496970253279109 ) ) ;
#2892 = CARTESIAN_POINT ( 'NONE',  ( 2.963400493335893948, 1.747644659881589568, 1.109742091278065113 ) ) ;
#2893 = CARTESIAN_POINT ( 'NONE',  ( 5.876533236880477240, 5.820653295974182129, 0.7998128361456352531 ) ) ;
#2894 = CARTESIAN_POINT ( 'NONE',  ( 4.552505719138623341, 8.533283448962240669, 0.7998128361456341429 ) ) ;
#2895 = VERTEX_POINT ( 'NONE', #94937 ) ;
#2897 = CARTESIAN_POINT ( 'NONE',  ( 3.330499290451326200, 7.037332938835193730, -0.7998128361456291469 ) ) ;
#2896 = CARTESIAN_POINT ( 'NONE',  ( 4.628904841183094199, -1.911603206638176511, 0.8469096376574613005 ) ) ;
#2900 = EDGE_LOOP ( 'NONE', ( #47457, #196132, #160277, #122236 ) ) ;
#2899 = CARTESIAN_POINT ( 'NONE',  ( 2.508236654460756387, -1.806733793710820324, -0.1315605372460958433 ) ) ;
#2898 = CARTESIAN_POINT ( 'NONE',  ( 3.610199614654508338, -0.7391254383575728282, -1.669438027971142047 ) ) ;
#2901 = CARTESIAN_POINT ( 'NONE',  ( 8.530051201292206287, 13.10347683481629488, 0.000000000000000000 ) ) ;
#2902 = STYLED_ITEM ( 'NONE', ( #95623 ), #40584 ) ;
#2903 = DIRECTION ( 'NONE',  ( -0.000000000000000000, 1.000000000000000000, -0.000000000000000000 ) ) ;
#2904 = CARTESIAN_POINT ( 'NONE',  ( 9.476778946274437843, 12.06403068260519795, 6.318147453416640857 ) ) ;
#2905 = CARTESIAN_POINT ( 'NONE',  ( 4.981566806912655743, 2.060606067865732527, -0.7902562557115796471 ) ) ;
#2906 = CARTESIAN_POINT ( 'NONE',  ( -1.402160292154681736E-14, 9.984375000341401574, 1.575800808251682339 ) ) ;
#2907 = ORIENTED_EDGE ( 'NONE', *, *, #117967, .T. ) ;
#2908 = CARTESIAN_POINT ( 'NONE',  ( 3.580628178849315280, -1.282259035790348722, 1.418852674340838060 ) ) ;
#2909 = CARTESIAN_POINT ( 'NONE',  ( -2.788173145904702555, 6.404619103530779789, -0.7998128361456281477 ) ) ;
#2910 = CARTESIAN_POINT ( 'NONE',  ( 8.609591239877852686, 10.00327685373437347, -1.199719254218445830 ) ) ;
#2911 = CARTESIAN_POINT ( 'NONE',  ( 6.602015318333181781, 0.7961593463888805289, -1.911361562896146671 ) ) ;
#2912 = CARTESIAN_POINT ( 'NONE',  ( 0.6801582343749865700, 0.08854166700808518975, -1.178068619123869398 ) ) ;
#2913 = CARTESIAN_POINT ( 'NONE',  ( 4.433153041544209749, 7.155467067568137551, -1.082531754730548412 ) ) ;
#2914 = LINE ( 'NONE', #200062, #99689 ) ;
#2915 = CARTESIAN_POINT ( 'NONE',  ( 8.731305104352237834, 13.51198939287863610, -8.232175732474900087 ) ) ;
#2916 = CARTESIAN_POINT ( 'NONE',  ( -8.140681553543240412, 15.44816072426944409, -8.801270232398126225 ) ) ;
#2917 = ORIENTED_EDGE ( 'NONE', *, *, #1100, .F. ) ;
#2918 = CARTESIAN_POINT ( 'NONE',  ( 5.948130214252392634, 7.161930257618140949, 1.164772078525571075 ) ) ;
#2919 = CARTESIAN_POINT ( 'NONE',  ( 3.831198023013999698, -1.729401117988647707, 0.7132991360168300377 ) ) ;
#2920 = DIRECTION ( 'NONE',  ( 1.561558963378126405E-12, 1.000000000000000000, 1.535693738323023938E-12 ) ) ;
#2921 = CARTESIAN_POINT ( 'NONE',  ( -7.834948825496940827, -6.134628647623485698, -7.720982897393570354 ) ) ;
#2922 =( BOUNDED_CURVE ( )  B_SPLINE_CURVE ( 3, ( #143401, #28547, #44819, #156418 ),
 .UNSPECIFIED., .F., .T. ) 
 B_SPLINE_CURVE_WITH_KNOTS ( ( 4, 4 ),
 ( 0.000000000000000000, 0.4999999999999970579 ),
 .UNSPECIFIED. ) 
 CURVE ( )  GEOMETRIC_REPRESENTATION_ITEM ( )  RATIONAL_B_SPLINE_CURVE ( ( 1.000000000000000222, 0.3333333333333373671, 0.3333333333333334259, 0.9999999999999963363 ) ) 
 REPRESENTATION_ITEM ( '' )  );
#2923 = CARTESIAN_POINT ( 'NONE',  ( -5.897433632264490910, 9.824163637709826702, 0.000000000000000000 ) ) ;
#2924 = CARTESIAN_POINT ( 'NONE',  ( 2.898410978271408922, 6.603506251283770112, -0.7998128361456362523 ) ) ;
#2925 = CARTESIAN_POINT ( 'NONE',  ( 3.811813743736467419, 7.598866467667865443, 1.040834085586084257E-14 ) ) ;
#2926 = CARTESIAN_POINT ( 'NONE',  ( 6.930528400284448054, -1.278709912597691511, 1.628784411136071197 ) ) ;
#2927 = EDGE_CURVE ( 'NONE', #104013, #15383, #204212, .T. ) ;
#2928 = CARTESIAN_POINT ( 'NONE',  ( 1.159780049612362030, 1.203373692603469935, 1.617804775344060308 ) ) ;
#2929 = CARTESIAN_POINT ( 'NONE',  ( -8.971744963941075568, 11.49012176272984931, 1.599625672291269396 ) ) ;
#2930 = CARTESIAN_POINT ( 'NONE',  ( 5.722423353419669567, 8.833855124701747386, 1.199719254218451159 ) ) ;
#2931 =( NAMED_UNIT ( * ) SI_UNIT ( $, .STERADIAN. ) SOLID_ANGLE_UNIT ( ) );
#2932 = CARTESIAN_POINT ( 'NONE',  ( 0.9729166594223404019, -0.05710519180573449260, -2.190871861337650994 ) ) ;
#2933 = CARTESIAN_POINT ( 'NONE',  ( 6.234959169399230561, 0.1841439077357870380, 1.816378869960999509 ) ) ;
#2934 = CARTESIAN_POINT ( 'NONE',  ( -4.471491734408701291, 4.111161866431900513, 1.214306433183764966E-14 ) ) ;
#2935 = CARTESIAN_POINT ( 'NONE',  ( 4.082413651490639062, 7.776916670132135501, 0.000000000000000000 ) ) ;
#2936 = CARTESIAN_POINT ( 'NONE',  ( 9.911173986789782120, 11.52179005846497972, -1.199719254218440723 ) ) ;
#2937 = CARTESIAN_POINT ( 'NONE',  ( 2.544126380858701797, 6.119897877643793116, 0.7998128361456462443 ) ) ;
#2938 = CARTESIAN_POINT ( 'NONE',  ( 2.891631901464575272, 6.595597328342462262, 0.000000000000000000 ) ) ;
#2939 = ORIENTED_EDGE ( 'NONE', *, *, #137004, .T. ) ;
#2941 = CARTESIAN_POINT ( 'NONE',  ( 0.1529896150729666005, 0.3463191217260193633, 1.982936507005612414 ) ) ;
#2940 = CARTESIAN_POINT ( 'NONE',  ( 3.720104550828434942, 1.749555917645674530, 0.5740644926693627692 ) ) ;
#2942 = CARTESIAN_POINT ( 'NONE',  ( 2.513387927098627905, 2.297807174607501057, 0.05796762653747893068 ) ) ;
#2944 = CARTESIAN_POINT ( 'NONE',  ( 0.4790722831046652641, -0.09921120595577682943, 1.858460205838560864 ) ) ;
#2943 = CARTESIAN_POINT ( 'NONE',  ( 3.633221978782282147, 5.261844946711204507, -1.443375672974057666 ) ) ;
#2945 = CARTESIAN_POINT ( 'NONE',  ( 3.285556943749998737, -3.755208332855373587, -1.896917185911906500 ) ) ;
#2946 = CARTESIAN_POINT ( 'NONE',  ( -4.069418662396130593, 7.899405539437467816, -0.7998128361456281477 ) ) ;
#2947 = CARTESIAN_POINT ( 'NONE',  ( 4.379179108948761723, 7.028642110670195287, -1.191602461106481936 ) ) ;
#2948 = CARTESIAN_POINT ( 'NONE',  ( 4.324404969281474109, -0.8226261416362996570, -1.726585468271451651 ) ) ;
#2949 = CARTESIAN_POINT ( 'NONE',  ( -10.30827686509187835, 10.92074451889568643, 1.040834085586084257E-14 ) ) ;
#2951 = ADVANCED_FACE ( 'NONE', ( #43763 ), #141285, .T. ) ;
#2950 = CARTESIAN_POINT ( 'NONE',  ( 6.403672513108120690, 6.804938187689173468, -0.5019199613840990004 ) ) ;
#2952 = CARTESIAN_POINT ( 'NONE',  ( -6.997416678428844072, 8.296645891989347987, 1.082531754730549078 ) ) ;
#2954 = CARTESIAN_POINT ( 'NONE',  ( 2.184254540302111636, -1.834043650784190405, -0.3674020703766100460 ) ) ;
#2953 = CARTESIAN_POINT ( 'NONE',  ( 3.773056988009905410, 1.967892522216899476, -0.7064651350525589235 ) ) ;
#2955 = CARTESIAN_POINT ( 'NONE',  ( 7.443063144222396232, 11.62739806832741785, 1.040834085586084257E-14 ) ) ;
#2956 = CARTESIAN_POINT ( 'NONE',  ( -0.6823417656249969321, 5.280208333674756283, -1.181850606188749264 ) ) ;
#2957 = CARTESIAN_POINT ( 'NONE',  ( 3.632115859802576008, 0.2593814109021801984, 1.720877339435398667 ) ) ;
#2958 = CARTESIAN_POINT ( 'NONE',  ( 5.196852952739813070, 4.957416621151553571, -0.7998128361456221525 ) ) ;
#2960 = CARTESIAN_POINT ( 'NONE',  ( 5.854423403002611437, 5.724582146458163656, 1.040834085586084257E-14 ) ) ;
#2959 = CARTESIAN_POINT ( 'NONE',  ( 1.220146605508150803E-14, 11.46875000068279604, -1.499999999999998446 ) ) ;
#2961 = CARTESIAN_POINT ( 'NONE',  ( 3.914446297384760243, 1.218041307117226690, -1.221573883832317575 ) ) ;
#2962 = CARTESIAN_POINT ( 'NONE',  ( -5.876569516519495551, 8.943415971659659292, 1.199719254218452047 ) ) ;
#2963 = CARTESIAN_POINT ( 'NONE',  ( 3.650093349144762023, 0.7902683543556283663, 2.044282924279612779 ) ) ;
#2964 = CARTESIAN_POINT ( 'NONE',  ( 6.674453038267287752, -1.361800985140369402, 1.737325302230605883 ) ) ;
#2965 = CARTESIAN_POINT ( 'NONE',  ( 1.499999999999996891, 8.645833333333337478, -0.8660254037844378194 ) ) ;
#2966 = AXIS2_PLACEMENT_3D ( 'NONE', #78648, #112296, #209704 ) ;
#2967 = CARTESIAN_POINT ( 'NONE',  ( 3.625983508040203862, 2.119313185944927902, -0.4706255054970372997 ) ) ;
#2968 = CARTESIAN_POINT ( 'NONE',  ( 2.490611698265518648, -0.3118145247060916114, -1.798701865878708839 ) ) ;
#2969 = DIRECTION ( 'NONE',  ( 1.000000000000000000, 0.000000000000000000, 0.000000000000000000 ) ) ;
#2971 = CARTESIAN_POINT ( 'NONE',  ( 6.051990796818580876, 1.090527953092842894, 1.814802726937503330 ) ) ;
#2970 = B_SPLINE_CURVE_WITH_KNOTS ( 'NONE', 3,
 ( #68679, #58594, #2610, #119655, #169405, #70808 ),
 .UNSPECIFIED., .F., .F.,
 ( 4, 2, 4 ),
 ( 0.000000000000000000, 0.0003147459536107388863, 0.0006294919072214776642 ),
 .UNSPECIFIED. ) ;
#2972 = ORIENTED_EDGE ( 'NONE', *, *, #194076, .T. ) ;
#2974 = CARTESIAN_POINT ( 'NONE',  ( -1.364683531250012516, 2.801041667008090652, -0.7879004041258289570 ) ) ;
#2973 = CARTESIAN_POINT ( 'NONE',  ( 5.407889476941767803, -1.028354611087534787, -2.048866343328694661 ) ) ;
#2975 = CARTESIAN_POINT ( 'NONE',  ( 6.720655732516650716, 1.307757891114844417, 1.844004982043083940 ) ) ;
#2976 = CARTESIAN_POINT ( 'NONE',  ( 8.218213668177886788, 12.73966637951625813, 0.7998128361456462443 ) ) ;
#2977 = CARTESIAN_POINT ( 'NONE',  ( 1.893382502257603850, -0.1070854039621378373, -2.117916637519041689 ) ) ;
#2978 = CARTESIAN_POINT ( 'NONE',  ( -4.094199201646926412, 7.720390135322642067, 0.7216878364870317197 ) ) ;
#2979 = DIRECTION ( 'NONE',  ( -0.000000000000000000, -1.000000000000000000, -0.000000000000000000 ) ) ;
#2980 = CARTESIAN_POINT ( 'NONE',  ( -4.243338890952892406, 7.894386439512932618, -0.7216878364870257245 ) ) ;
#2981 = VECTOR ( 'NONE', #30547, 1000.000000000000000 ) ;
#2982 = EDGE_CURVE ( 'NONE', #8666, #41918, #10157, .T. ) ;
#2984 = CARTESIAN_POINT ( 'NONE',  ( 1.500000000000001332, 13.15625000068279604, 0.000000000000000000 ) ) ;
#2983 = CARTESIAN_POINT ( 'NONE',  ( 6.883263157960362477, 2.445608615952394871, 2.336423753955836791 ) ) ;
#2985 = EDGE_LOOP ( 'NONE', ( #132684, #96087, #82644, #101049 ) ) ;
#2986 = CARTESIAN_POINT ( 'NONE',  ( 6.065077313367789102, -1.076319894221990259, 1.704936797084610101 ) ) ;
#2988 = CARTESIAN_POINT ( 'NONE',  ( 4.891499300893256574, -1.887858789894794054, 0.8311416006015391877 ) ) ;
#2987 = CARTESIAN_POINT ( 'NONE',  ( 5.332434488876471868, 5.115595079977664383, 0.7998128361456341429 ) ) ;
#2990 = CARTESIAN_POINT ( 'NONE',  ( -0.2409995289980246258, 7.629137130509076492, -2.600476469121239198 ) ) ;
#2989 = CARTESIAN_POINT ( 'NONE',  ( 7.178115983792402233, 7.339166500704784823, 0.7998128361456281477 ) ) ;
#2991 = CARTESIAN_POINT ( 'NONE',  ( 7.212011367826596242, 7.378711115411311638, 0.000000000000000000 ) ) ;
#2992 = CARTESIAN_POINT ( 'NONE',  ( -1.642778471874998480, -0.7510416661887092671, 2.845375778867863303 ) ) ;
#2993 = CARTESIAN_POINT ( 'NONE',  ( 0.3047781727255130524, 1.820093451774043691, 1.028452505696121344 ) ) ;
#2994 = CARTESIAN_POINT ( 'NONE',  ( 5.027970288326706338, -1.728003250605243180, 1.038991650911202713 ) ) ;
#2995 = CARTESIAN_POINT ( 'NONE',  ( 4.423293856316495187, -1.136390847421838490, -1.448631019334602144 ) ) ;
#2996 = CARTESIAN_POINT ( 'NONE',  ( 6.602984505055297326, 7.662235663108029726, 1.199719254218462483 ) ) ;
#2997 = CARTESIAN_POINT ( 'NONE',  ( 0.8852880119799062530, 1.153610147808200370, 1.282378885572494465 ) ) ;
#2998 = CARTESIAN_POINT ( 'NONE',  ( 0.1281391398850126040, 2.011452084832816123, 0.1435147193784985509 ) ) ;
#2999 = CARTESIAN_POINT ( 'NONE',  ( 1.178858319146030009, 1.745148694481736484, 1.496268366688303653 ) ) ;
#3000 = CARTESIAN_POINT ( 'NONE',  ( -6.413170354464012846, 7.440785820751486312, 1.199719254218450271 ) ) ;
#3001 = CARTESIAN_POINT ( 'NONE',  ( 1.054439146255849780, 2.259743442402757818, -0.1116689827955052033 ) ) ;
#3002 = CARTESIAN_POINT ( 'NONE',  ( 3.053452221204506323, -1.721964003836244039, -1.212301904834027333 ) ) ;
#3003 = CARTESIAN_POINT ( 'NONE',  ( -4.610654757099099221, 7.536791762327691657, 1.199719254218452935 ) ) ;
#3004 = CARTESIAN_POINT ( 'NONE',  ( 7.019370843573166319, 9.212351955633947043, 1.599625672291281386 ) ) ;
#3005 = CARTESIAN_POINT ( 'NONE',  ( 5.194182247366868843, 8.113610817686430110, 1.082531754730548412 ) ) ;
#3006 = CARTESIAN_POINT ( 'NONE',  ( -5.331380718671772101, 7.243030143248949670, -1.599625672291256295 ) ) ;
#3007 = CARTESIAN_POINT ( 'NONE',  ( 6.927853306458752414, 7.184843067064434763, 0.7216878364870317197 ) ) ;
#3008 = CARTESIAN_POINT ( 'NONE',  ( 4.945911955618520928, 6.845357471522081738, 1.424928946000488583 ) ) ;
#3009 = CARTESIAN_POINT ( 'NONE',  ( -2.788173145904702555, 6.404619103530779789, -0.7998128361456281477 ) ) ;
#3010 = CARTESIAN_POINT ( 'NONE',  ( 4.974942202162922378, -1.608427002576447995, 1.532403895573146491 ) ) ;
#3011 = CARTESIAN_POINT ( 'NONE',  ( 2.994263412949604852, -0.6367403190770392074, -2.096898073876966251 ) ) ;
#3012 = CARTESIAN_POINT ( 'NONE',  ( -4.412288926243578935, 7.235088616337731260, 1.199719254218464037 ) ) ;
#3014 = CIRCLE ( 'NONE', #44663, 9.999999999999996447 ) ;
#3013 = CARTESIAN_POINT ( 'NONE',  ( -4.442231607132987925, 5.211633625523774960, -1.199719254218453823 ) ) ;
#3015 = CARTESIAN_POINT ( 'NONE',  ( 5.072687121480487171, 1.354251660176824856, -1.419695456575476689 ) ) ;
#3016 =( BOUNDED_CURVE ( )  B_SPLINE_CURVE ( 2, ( #161431, #140943, #193908, #209072, #208021, #73765, #108473, #206957, #124741 ),
 .UNSPECIFIED., .F., .T. ) 
 B_SPLINE_CURVE_WITH_KNOTS ( ( 3, 2, 2, 2, 3 ),
 ( 0.6875000000000000000, 0.6904761904761904656, 0.6964285714285713969, 0.7023809523809523281, 0.7053571428571427937 ),
 .UNSPECIFIED. ) 
 CURVE ( )  GEOMETRIC_REPRESENTATION_ITEM ( )  RATIONAL_B_SPLINE_CURVE ( ( 0.9330127018922194093, 0.9330127018922194093, 1.000000000000000000, 0.8660254037844387076, 1.000000000000000000, 0.8660254037844387076, 1.000000000000000000, 0.9330127018922206306, 0.9330127018922194093 ) ) 
 REPRESENTATION_ITEM ( '' )  );
#3017 = CARTESIAN_POINT ( 'NONE',  ( 1.364683531249986537, 1.905208333674750287, -0.7879004041258239610 ) ) ;
#3018 = CARTESIAN_POINT ( 'NONE',  ( 6.609999999999973674, -0.005249217919313375023, 2.280159464062641916 ) ) ;
#3019 = CARTESIAN_POINT ( 'NONE',  ( -4.256897045010916258, 7.910204285913967404, 0.7216878364870317197 ) ) ;
#3020 = CARTESIAN_POINT ( 'NONE',  ( 4.535463010148616192, -0.1012041512906610846, 2.118281909017679432 ) ) ;
#3021 = CARTESIAN_POINT ( 'NONE',  ( -6.075462232699549325, 9.141770800574526845, 1.082531754730549967 ) ) ;
#3022 = ORIENTED_EDGE ( 'NONE', *, *, #119577, .T. ) ;
#3024 = CARTESIAN_POINT ( 'NONE',  ( 6.754756207809571755, -1.674487575904315406, 1.366813541845832924 ) ) ;
#3023 = CARTESIAN_POINT ( 'NONE',  ( -4.475600106286965918, 8.235634200727838916, 0.7216878364870338292 ) ) ;
#3025 = CARTESIAN_POINT ( 'NONE',  ( 4.482942347612929979, 8.381849838857084123, 1.040834085586084257E-14 ) ) ;
#3026 = CARTESIAN_POINT ( 'NONE',  ( 5.425302022954732628, -1.172690680311109901, -1.419496581506813904 ) ) ;
#3027 = PRESENTATION_STYLE_ASSIGNMENT (( #17146 ) ) ;
#3028 = CARTESIAN_POINT ( 'NONE',  ( -0.6823417656250003738, 2.530208333674753618, -1.181850606188749264 ) ) ;
#3029 = CARTESIAN_POINT ( 'NONE',  ( 1.012787145881738793, -1.698268246007793802, 0.3799501884491280901 ) ) ;
#3030 = CARTESIAN_POINT ( 'NONE',  ( 1.220146605508150803E-14, 11.21875000068279249, -1.499999999999998446 ) ) ;
#3031 = CARTESIAN_POINT ( 'NONE',  ( -1.364683531250000748, -0.9281249996585805295, 0.000000000000000000 ) ) ;
#3032 = DIRECTION ( 'NONE',  ( -0.000000000000000000, -1.000000000000000000, 0.000000000000000000 ) ) ;
#3033 = CARTESIAN_POINT ( 'NONE',  ( 5.647404790089923132, -1.701416311724871067, -1.333359258283283166 ) ) ;
#3034 = TOROIDAL_SURFACE ( 'NONE', #20367, 11.92000000000000171, 0.08000000000000000167 ) ;
#3035 = CARTESIAN_POINT ( 'NONE',  ( -4.295235737431041478, 3.905529869957963029, -0.7998128361456221525 ) ) ;
#3036 = CARTESIAN_POINT ( 'NONE',  ( -7.171900071504745178, 9.390302721554109056, -1.443375672974058777 ) ) ;
#3037 = CARTESIAN_POINT ( 'NONE',  ( 4.241217004700631676, -1.882188537963986219, 1.063020064016991117 ) ) ;
#3038 = CARTESIAN_POINT ( 'NONE',  ( 1.364683531249988535, 3.405208333674749621, -0.7879004041258239610 ) ) ;
#3039 = CARTESIAN_POINT ( 'NONE',  ( 4.323478126428228485, -1.887445700180546915, 0.5691147572158322676 ) ) ;
#3040 = CARTESIAN_POINT ( 'NONE',  ( 4.463993690379265189, 1.392342236284923152, 1.032948281618131903 ) ) ;
#3041 = CARTESIAN_POINT ( 'NONE',  ( 0.8025787753177977546, 1.655945718051672566, -1.435626523826734280 ) ) ;
#3042 = CARTESIAN_POINT ( 'NONE',  ( 2.081525663035548757, -0.1140690627178981842, -2.304871973535598251 ) ) ;
#3043 = CARTESIAN_POINT ( 'NONE',  ( 5.202442474109128412, -0.6904536177961515531, -1.941828258638809368 ) ) ;
#3044 = CARTESIAN_POINT ( 'NONE',  ( 0.4099697989727095204, 1.339763683568921504, -1.405998798013205819 ) ) ;
#3045 = CARTESIAN_POINT ( 'NONE',  ( -8.148087131688699358, 8.608449196499371681, -0.7216878364870267237 ) ) ;
#3046 = CARTESIAN_POINT ( 'NONE',  ( -6.479871072688648148, 6.524547437750345402, 0.000000000000000000 ) ) ;
#3047 = DIRECTION ( 'NONE',  ( 0.000000000000000000, 0.000000000000000000, 1.000000000000000000 ) ) ;
#3048 = CYLINDRICAL_SURFACE ( 'NONE', #146909, 1.250000000000000000 ) ;
#3049 = CARTESIAN_POINT ( 'NONE',  ( 0.9850002542920628379, -2.016597020373378513, 0.002813405579435435122 ) ) ;
#3050 = CARTESIAN_POINT ( 'NONE',  ( -6.846504384776758378, 9.010674420371453053, -1.443375672974058777 ) ) ;
#3051 = CARTESIAN_POINT ( 'NONE',  ( 3.839080194659278966, 0.3211572903306300075, 2.183152695405643051 ) ) ;
#3052 = CARTESIAN_POINT ( 'NONE',  ( 3.285556943750000070, -2.121874999522044281, 0.000000000000000000 ) ) ;
#3053 = CARTESIAN_POINT ( 'NONE',  ( 0.9536794021071954841, -0.6768100219149524310, 1.733691362649824264 ) ) ;
#3054 = LINE ( 'NONE', #51848, #199489 ) ;
#3055 = CARTESIAN_POINT ( 'NONE',  ( -7.887197531381538340, -6.766388843766927508, 7.667935170093262975 ) ) ;
#3057 = CARTESIAN_POINT ( 'NONE',  ( 6.925078400183569904, 6.033938712579569597, 2.739235483740619426 ) ) ;
#3056 = CARTESIAN_POINT ( 'NONE',  ( -4.762026763822442277, 8.287006692039220468, -0.8189809589772244491 ) ) ;
#3058 = CARTESIAN_POINT ( 'NONE',  ( 6.087831982560696353, -1.832735460234231617, -0.1757473516527594259 ) ) ;
#3059 = EDGE_LOOP ( 'NONE', ( #52191, #98069, #29595, #193700 ) ) ;
#3060 = CARTESIAN_POINT ( 'NONE',  ( 3.555589940775650604, 0.5024415226424256975, -1.998565159594118068 ) ) ;
#3061 = CARTESIAN_POINT ( 'NONE',  ( 1.360316468749966257, 1.765625000341414230, -3.642919299551294898E-14 ) ) ;
#3062 = CARTESIAN_POINT ( 'NONE',  ( -5.259673527097670664, 8.223703984000886535, -1.199719254218446718 ) ) ;
#3063 = CARTESIAN_POINT ( 'NONE',  ( 2.139325021376851765, 0.002241307429765720949, 2.019862492052142855 ) ) ;
#3064 = CARTESIAN_POINT ( 'NONE',  ( -1.500000000000015099, 0.1291666666666918539, -0.8660254037844383745 ) ) ;
#3065 = CARTESIAN_POINT ( 'NONE',  ( 4.142179624174931796, 4.791296635414242111, 1.199719254218464037 ) ) ;
#3066 = CARTESIAN_POINT ( 'NONE',  ( 2.008734545381769543, 1.527802914727709016, -1.383344190003793495 ) ) ;
#3068 = CARTESIAN_POINT ( 'NONE',  ( 1.364683531250000303, 12.75520833367473550, -0.7879004041258355073 ) ) ;
#3067 = CARTESIAN_POINT ( 'NONE',  ( 6.883263157960362477, -0.004191378316371896506, 2.053658919477070910 ) ) ;
#3069 = CARTESIAN_POINT ( 'NONE',  ( 6.063521013809720195, 8.097193820909906137, 1.599625672291281386 ) ) ;
#3070 = CARTESIAN_POINT ( 'NONE',  ( -0.1411974294641838990, 5.723166529328228336, -2.494358352568406545 ) ) ;
#3071 = CARTESIAN_POINT ( 'NONE',  ( 5.496761087669068679, -0.5331231007881258588, -2.141394884921154151 ) ) ;
#3072 = CARTESIAN_POINT ( 'NONE',  ( 1.546389740860309781, 2.159050155192781872, 0.1077149563947499555 ) ) ;
#3073 = VECTOR ( 'NONE', #149450, 1000.000000000000000 ) ;
#3074 = CARTESIAN_POINT ( 'NONE',  ( -4.446711195602252253, 6.210915699667823198, -1.443375672974053447 ) ) ;
#3075 = CARTESIAN_POINT ( 'NONE',  ( 1.780482797753998092, -0.5424726148271253878, -1.942096288550937411 ) ) ;
#3076 = CARTESIAN_POINT ( 'NONE',  ( 2.179500908114082591, -1.083194949601238521, -2.027108130913716444 ) ) ;
#3077 = EDGE_CURVE ( 'NONE', #80044, #196686, #78774, .T. ) ;
#3078 = SURFACE_STYLE_USAGE ( .BOTH. , #103821 ) ;
#3079 = CARTESIAN_POINT ( 'NONE',  ( -0.5167901049056953244, 6.690130572215640115, 3.553507429615057056 ) ) ;
#3080 = CARTESIAN_POINT ( 'NONE',  ( 3.194898696050481934, 6.432863918183953089, -0.8190951789856844023 ) ) ;
#3081 = CARTESIAN_POINT ( 'NONE',  ( 1.832664747978371533, 0.1804508633567840359, 1.861920966532565336 ) ) ;
#3082 = CARTESIAN_POINT ( 'NONE',  ( 3.063685658700274761, 1.282989771343697294, 1.555699169480361022 ) ) ;
#3084 = CARTESIAN_POINT ( 'NONE',  ( 6.639320575229257670, 2.957073754255258535, 2.555924021811271540 ) ) ;
#3083 = CARTESIAN_POINT ( 'NONE',  ( -1.364683531250012516, 2.488541667008088876, -0.7879004041258289570 ) ) ;
#3086 = CARTESIAN_POINT ( 'NONE',  ( 5.162764661449575243, -1.526107291725445236, 1.451632374922463553 ) ) ;
#3085 = CARTESIAN_POINT ( 'NONE',  ( -8.202846631467911820, 9.528741477256060577, 1.199719254218462483 ) ) ;
#3087 = CARTESIAN_POINT ( 'NONE',  ( 6.500244582748090139, 9.671036882259738121, 1.199719254218460707 ) ) ;
#3088 = CARTESIAN_POINT ( 'NONE',  ( -7.389357414647957256, 8.579670724299436557, 1.199719254218450271 ) ) ;
#3089 = CARTESIAN_POINT ( 'NONE',  ( -0.3728355200475085285, -6.583727468837148322, -9.609247538825096413 ) ) ;
#3090 = CARTESIAN_POINT ( 'NONE',  ( 5.238538122511118722, 1.199862898965612823, -1.624631798562142793 ) ) ;
#3091 = CARTESIAN_POINT ( 'NONE',  ( -1.364683531250010295, 5.738541667008088432, -0.7879004041258300672 ) ) ;
#3092 = EDGE_CURVE ( 'NONE', #147946, #136086, #58918, .T. ) ;
#3093 = CARTESIAN_POINT ( 'NONE',  ( 1.270463096138880088, -0.9239429406890822261, -1.844087381150324001 ) ) ;
#3094 = CARTESIAN_POINT ( 'NONE',  ( 7.782016984564054773, 10.10210578678999482, 1.443375672974076540 ) ) ;
#3095 = CARTESIAN_POINT ( 'NONE',  ( 5.855142236255289845, 7.924361590421551860, -1.599625672291281386 ) ) ;
#3096 = CARTESIAN_POINT ( 'NONE',  ( 4.688087255275310561, 8.691461907788344377, -0.7998128361456381397 ) ) ;
#3097 = CARTESIAN_POINT ( 'NONE',  ( -0.6823417656250212460, 0.8635416670080899859, 1.181850606188755259 ) ) ;
#3098 = CARTESIAN_POINT ( 'NONE',  ( 4.258142763143749399, 7.125527769379820242, 1.199719254218451159 ) ) ;
#3099 = CARTESIAN_POINT ( 'NONE',  ( 6.412643469139427843, 10.42524178073059993, -0.7216878364870267237 ) ) ;
#3101 = CARTESIAN_POINT ( 'NONE',  ( -4.064664930713566271, 3.791393346161858080, -2.445650103046228985 ) ) ;
#3100 = CARTESIAN_POINT ( 'NONE',  ( 3.104148162264197985, 0.7838245717375692534, -2.024915708489416044 ) ) ;
#3103 = CARTESIAN_POINT ( 'NONE',  ( 1.874305484616908934, -0.09156810461483089192, -1.839108553062768214 ) ) ;
#3102 = CARTESIAN_POINT ( 'NONE',  ( -5.910991785878183080, 5.998504626387068051, -0.7216878364870278340 ) ) ;
#3104 = CARTESIAN_POINT ( 'NONE',  ( -1.364683531250012516, 3.988541667008088876, -0.7879004041258300672 ) ) ;
#3105 = CARTESIAN_POINT ( 'NONE',  ( 4.441096743985088580, -1.694418930461354611, -1.389946530008886905 ) ) ;
#3106 = CARTESIAN_POINT ( 'NONE',  ( 6.883263157960369583, 7.629137130509070275, 2.653810918356712900 ) ) ;
#3107 = CARTESIAN_POINT ( 'NONE',  ( 4.909165057579100377, 1.966063467186284663, 1.119528758242648525 ) ) ;
#3108 = CARTESIAN_POINT ( 'NONE',  ( -5.371001409308059138, 9.417918744168066070, -0.7998128361456231517 ) ) ;
#3109 = CARTESIAN_POINT ( 'NONE',  ( -0.6823417656249969321, 5.780208333674756283, -1.181850606188749264 ) ) ;
#3110 = CARTESIAN_POINT ( 'NONE',  ( 5.834480046583573554, 7.201333694826374199, -1.164487238324034557 ) ) ;
#3111 = CARTESIAN_POINT ( 'NONE',  ( -0.7500000000000179856, 14.29166666666666785, 1.299038105676658228 ) ) ;
#3112 = CARTESIAN_POINT ( 'NONE',  ( -6.143253000323532831, 7.300121600866474658, 1.082531754730548412 ) ) ;
#3113 = CARTESIAN_POINT ( 'NONE',  ( 5.722950238744211937, 5.849399164722627553, 0.7216878364870328300 ) ) ;
#3114 = CARTESIAN_POINT ( 'NONE',  ( 5.747242073547443653, -1.395821259116083013, -1.087781934379092874 ) ) ;
#3116 = CARTESIAN_POINT ( 'NONE',  ( 3.229155175764964802, 1.820814436659716096, 0.8588418517583608081 ) ) ;
#3115 = COLOUR_RGB ( '', 0.40784314, 0.44705882, 0.49803922) ;
#3117 = CARTESIAN_POINT ( 'NONE',  ( 6.259060471003163428, 10.45398764947904624, -0.7998128361456291469 ) ) ;
#3118 = CARTESIAN_POINT ( 'NONE',  ( 2.256984296129550760, -1.628445616851754263, 1.335386477757320778 ) ) ;
#3121 = EDGE_CURVE ( 'NONE', #36876, #158170, #96130, .T. ) ;
#3120 = CARTESIAN_POINT ( 'NONE',  ( -1.500000000000013101, 3.129166666666689967, -0.8660254037844313801 ) ) ;
#3119 = CARTESIAN_POINT ( 'NONE',  ( -0.6823417656250003738, 11.90104166700806054, 1.181850606188754593 ) ) ;
#3122 = CARTESIAN_POINT ( 'NONE',  ( 1.486696478045932635, 1.897211281248304848, 0.5285659569534242319 ) ) ;
#3123 = CARTESIAN_POINT ( 'NONE',  ( 0.6373110600932235803, -1.319858442276698129, -1.325903642019378381 ) ) ;
#3124 = CARTESIAN_POINT ( 'NONE',  ( 0.7835587076311965049, -1.864072139945194717, 0.6119401183290391621 ) ) ;
#3126 = VERTEX_POINT ( 'NONE', #76233 ) ;
#3125 = CARTESIAN_POINT ( 'NONE',  ( 5.713115418873079498, 1.475880075617709730, -1.050242514106846992 ) ) ;
#3127 = CARTESIAN_POINT ( 'NONE',  ( 5.016153647376196290, 8.796003655340152605, 0.7216878364870438212 ) ) ;
#3128 = CARTESIAN_POINT ( 'NONE',  ( -1.402160292154681736E-14, -0.3656249996585805295, 1.575800808251672791 ) ) ;
#3129 = CARTESIAN_POINT ( 'NONE',  ( 5.647288160985431738, -1.475499438119257878, -1.149758287351684949 ) ) ;
#3130 = CARTESIAN_POINT ( 'NONE',  ( 3.837121167867449945, 4.435395103055503441, 1.199719254218464037 ) ) ;
#3131 = CARTESIAN_POINT ( 'NONE',  ( 9.007749180437182090, 1.970899860167747653, 7.589917856494929893 ) ) ;
#3132 = CARTESIAN_POINT ( 'NONE',  ( 5.032118066406459533, 1.187563481491529682, 1.695602288408842417 ) ) ;
#3133 = CARTESIAN_POINT ( 'NONE',  ( 1.224999999999979217, 2.604166666666692276, 0.7072540797572558491 ) ) ;
#3134 = CARTESIAN_POINT ( 'NONE',  ( -6.414416072596857532, 6.656109304217339151, -0.7216878364870338292 ) ) ;
#3135 = CARTESIAN_POINT ( 'NONE',  ( 0.3091450132529197647, -1.663722454078466306, 1.232067777400827069 ) ) ;
#3136 = CARTESIAN_POINT ( 'NONE',  ( 1.499999999999987121, 0.7541666666666868579, 0.8660254037844524744 ) ) ;
#3137 = CARTESIAN_POINT ( 'NONE',  ( 6.076025397218672630, 10.24044673006381245, -0.7998128361456291469 ) ) ;
#3138 = CARTESIAN_POINT ( 'NONE',  ( -9.124801077197171040, 10.60435499727357289, -1.199719254218441611 ) ) ;
#3139 = CARTESIAN_POINT ( 'NONE',  ( 6.801350335910821165, 7.963938809097990124, 1.199719254218452047 ) ) ;
#3140 = EDGE_CURVE ( 'NONE', #7595, #204603, #137712, .T. ) ;
#3141 = CARTESIAN_POINT ( 'NONE',  ( 0.6823417656249899377, 1.342708333674752508, 1.181850606188755259 ) ) ;
#3142 = EDGE_CURVE ( 'NONE', #106915, #35846, #25835, .T. ) ;
#3143 = CARTESIAN_POINT ( 'NONE',  ( -0.7500000000000215383, 1.691666666666688634, 1.299038105676659116 ) ) ;
#3145 = CARTESIAN_POINT ( 'NONE',  ( 5.009901455449552010, 5.803638771901306725, -1.199719254218452047 ) ) ;
#3144 = CARTESIAN_POINT ( 'NONE',  ( 5.107842384611220865, 0.6171798735227496113, -1.862306164846748491 ) ) ;
#3146 = CARTESIAN_POINT ( 'NONE',  ( 3.128279665134887644, 0.2985813455266342342, -1.993766061640166232 ) ) ;
#3147 = CARTESIAN_POINT ( 'NONE',  ( 2.624132809847005365, 1.901796678110598382, 0.2296932149444090299 ) ) ;
#3148 = CARTESIAN_POINT ( 'NONE',  ( 0.8201894534925309177, 1.301127354658284663, -1.763390660798454634 ) ) ;
#3149 = DIRECTION ( 'NONE',  ( 8.638326563840809144E-31, 5.962633348652903386E-61, -1.000000000000000000 ) ) ;
#3150 = CARTESIAN_POINT ( 'NONE',  ( 3.708139779478221598, -0.7553879706188313392, -1.711406342686023541 ) ) ;
#3151 = CARTESIAN_POINT ( 'NONE',  ( 0.7499999999999885647, -0.9854166659838472508, 1.299038105676657340 ) ) ;
#3152 = CARTESIAN_POINT ( 'NONE',  ( -8.532158741701643123, 8.848606708273724308, 0.7998128361456462443 ) ) ;
#3154 = CARTESIAN_POINT ( 'NONE',  ( 4.130539392780770314, 0.5663510459464686786, 2.039993263092474418 ) ) ;
#3153 = CARTESIAN_POINT ( 'NONE',  ( -5.965224400332865606, 7.022145224218852455, 1.082531754730549967 ) ) ;
#3155 = CARTESIAN_POINT ( 'NONE',  ( -0.04481625915950731426, -9.999534456186221831, -9.500049708090200440 ) ) ;
#3156 = CARTESIAN_POINT ( 'NONE',  ( 5.881320641815353412, -0.05461762546566179682, 2.069818975884097689 ) ) ;
#3158 = CARTESIAN_POINT ( 'NONE',  ( 6.620655732516679493, 7.051632961313193171, 2.871890384929445261 ) ) ;
#3157 = CARTESIAN_POINT ( 'NONE',  ( 0.6969597590469852610, 1.711416582936477804, 1.200673393543179479 ) ) ;
#3160 = ORIENTED_EDGE ( 'NONE', *, *, #11469, .F. ) ;
#3159 = CARTESIAN_POINT ( 'NONE',  ( 6.633835642106551411, -1.195214757176918496, -1.380038946949893486 ) ) ;
#3161 = CARTESIAN_POINT ( 'NONE',  ( 6.414979237560321401, 10.63589287712906462, 1.040834085586084257E-14 ) ) ;
#3162 = CARTESIAN_POINT ( 'NONE',  ( -5.398914348987532641, 6.259949555863199677, -2.500000000000000444 ) ) ;
#3163 = CARTESIAN_POINT ( 'NONE',  ( -0.09481041353608977984, -9.919511983836045488, -9.499526882191805299 ) ) ;
#3164 = CARTESIAN_POINT ( 'NONE',  ( -9.541824394042135893, 5.027248526908232762, 6.730710380108894775 ) ) ;
#3165 = CARTESIAN_POINT ( 'NONE',  ( 7.429504990164394584, 7.770103364721017591, 1.040834085586084257E-14 ) ) ;
#3166 = CARTESIAN_POINT ( 'NONE',  ( -1.162044386198238837E-16, 1.437500000000019540, -1.225000000000020739 ) ) ;
#3168 = CARTESIAN_POINT ( 'NONE',  ( 0.01197859805690624189, -1.811022649853447630, -0.04676520365421397291 ) ) ;
#3167 = CARTESIAN_POINT ( 'NONE',  ( 7.343676480457483002, 8.596652644402405841, -1.199719254218452047 ) ) ;
#3169 = CARTESIAN_POINT ( 'NONE',  ( -7.157815033010924921, 10.43820240756634199, 1.199719254218453823 ) ) ;
#3170 = CARTESIAN_POINT ( 'NONE',  ( 5.738125327081736060, 7.717565519727259904, 1.599625672291267398 ) ) ;
#3171 = CARTESIAN_POINT ( 'NONE',  ( 5.677832469072920496, 9.846164657218904992, 0.000000000000000000 ) ) ;
#3172 = CARTESIAN_POINT ( 'NONE',  ( 0.07917133907661091929, -6.459673408256485949, 11.00057242252814760 ) ) ;
#3173 = CARTESIAN_POINT ( 'NONE',  ( 4.088303131848604721, 7.475188365022519932, -0.6044521916458069910 ) ) ;
#3174 = CARTESIAN_POINT ( 'NONE',  ( 2.333974999846879061, 5.874721266463329705, -0.7998128361456291469 ) ) ;
#3175 = ORIENTED_EDGE ( 'NONE', *, *, #3623, .T. ) ;
#3176 = TOROIDAL_SURFACE ( 'NONE', #93235, 12.18000000000000149, 0.5000000000000008882 ) ;
#3177 = CARTESIAN_POINT ( 'NONE',  ( 6.573846656420020196, -0.8593871168269312522, 1.822298249534954673 ) ) ;
#3178 = CARTESIAN_POINT ( 'NONE',  ( 0.9090200710941964690, -0.5189423241485704441, -2.055877189782874481 ) ) ;
#3179 = CARTESIAN_POINT ( 'NONE',  ( 4.000000000000022204, 5.999999999999998224, 2.024999999999999023 ) ) ;
#3180 = CARTESIAN_POINT ( 'NONE',  ( 0.1405533004714799583, 1.991423289015941345, -2.694406653617386294 ) ) ;
#3181 = CARTESIAN_POINT ( 'NONE',  ( 6.773846765317333762, -7.246166700180801001, 6.773846765317311558 ) ) ;
#3182 = CARTESIAN_POINT ( 'NONE',  ( -4.446711195602252253, 6.210915699667823198, -1.443375672974053447 ) ) ;
#3183 = CARTESIAN_POINT ( 'NONE',  ( 8.812436659202669276, 10.34389285956704363, -1.082531754730543083 ) ) ;
#3184 = CARTESIAN_POINT ( 'NONE',  ( 3.748844217038479698, -0.3797678475170936929, -1.932296744971262692 ) ) ;
#3185 = CARTESIAN_POINT ( 'NONE',  ( 4.974232547167513729, -2.001514726140873890, -0.2440111082952014510 ) ) ;
#3186 = CARTESIAN_POINT ( 'NONE',  ( -5.687809136132860210, 6.594531066031826150, -1.199719254218446718 ) ) ;
#3187 = CARTESIAN_POINT ( 'NONE',  ( 0.4336004510535496626, 3.058108253035741964, -0.4198436715061193980 ) ) ;
#3188 = CARTESIAN_POINT ( 'NONE',  ( -9.499606442108964544, -9.746166700193986898, 0.08647222121513538362 ) ) ;
#3189 = CARTESIAN_POINT ( 'NONE',  ( 4.857479518068650748, 2.167902099161696849, -0.3196092617779102696 ) ) ;
#3190 = CARTESIAN_POINT ( 'NONE',  ( 0.000000000000000000, -7.723431457505077979, 0.000000000000000000 ) ) ;
#3191 = CARTESIAN_POINT ( 'NONE',  ( 4.278288924157873652, -1.109688035731031475, 1.574481611047764851 ) ) ;
#3192 = CARTESIAN_POINT ( 'NONE',  ( -6.170932472514347289, 10.35117165124207972, 0.000000000000000000 ) ) ;
#3193 = CARTESIAN_POINT ( 'NONE',  ( -0.1296875068448125057, 1.390030859318210688, -2.083197486262199138 ) ) ;
#3194 = CARTESIAN_POINT ( 'NONE',  ( 0.1331565106231606399, 5.723858289613107608, -2.539976893513963052 ) ) ;
#3195 = SURFACE_SIDE_STYLE ('',( #85540 ) ) ;
#3196 =( BOUNDED_CURVE ( )  B_SPLINE_CURVE ( 2, ( #79841, #46301, #211960, #66750, #180542, #83028, #683 ),
 .UNSPECIFIED., .F., .T. ) 
 B_SPLINE_CURVE_WITH_KNOTS ( ( 3, 2, 2, 3 ),
 ( 0.3602265381971914149, 0.3630952380952380820, 0.3690476190476190688, 0.3719163189456657359 ),
 .UNSPECIFIED. ) 
 CURVE ( )  GEOMETRIC_REPRESENTATION_ITEM ( )  RATIONAL_B_SPLINE_CURVE ( ( 0.9331000818465633451, 0.9354320710352566071, 1.000000000000000000, 0.8660254037844387076, 1.000000000000000000, 0.9354320710352564960, 0.9331000818465632340 ) ) 
 REPRESENTATION_ITEM ( '' )  );
#3197 = EDGE_LOOP ( 'NONE', ( #209100, #72520, #9846, #141144 ) ) ;
#3198 = CARTESIAN_POINT ( 'NONE',  ( 4.584065335196260804, 6.441438539186039591, 1.443375672974065660 ) ) ;
#3199 = ORIENTED_EDGE ( 'NONE', *, *, #79298, .T. ) ;
#3200 = CARTESIAN_POINT ( 'NONE',  ( 5.594576842560746499, 1.939643975919752572, 0.3403973628498639936 ) ) ;
#3202 = CARTESIAN_POINT ( 'NONE',  ( 4.160795161724285762, 0.5389290103979550439, 1.939535095694967959 ) ) ;
#3201 = CARTESIAN_POINT ( 'NONE',  ( 0.3099700162084629285, 1.338387961458173070, -1.407469107711552425 ) ) ;
#3203 = CARTESIAN_POINT ( 'NONE',  ( 6.011119390975155241, 2.295276066174879670, 0.1220560631845988148 ) ) ;
#3205 = CARTESIAN_POINT ( 'NONE',  ( 4.698021595848828724, 0.7982989760673472324, -1.681190670221676120 ) ) ;
#3204 = CARTESIAN_POINT ( 'NONE',  ( -5.759181390754928742, 9.941071732514568993, 0.000000000000000000 ) ) ;
#3206 = CARTESIAN_POINT ( 'NONE',  ( 6.770317605177710085, 8.992066187497757213, 1.599625672291268286 ) ) ;
#3207 = CARTESIAN_POINT ( 'NONE',  ( -10.97895254167818990, -5.212340523078042409, 0.4373349612950744314 ) ) ;
#3208 = FILL_AREA_STYLE ('',( #71413 ) ) ;
#3209 = CARTESIAN_POINT ( 'NONE',  ( -7.705111371268023923, 7.883718109434487253, 1.040834085586084257E-14 ) ) ;
#3210 = ADVANCED_FACE ( 'NONE', ( #41628 ), #28556, .T. ) ;
#3211 = CARTESIAN_POINT ( 'NONE',  ( -3.024877669624710386, 6.543124691288523920, 0.000000000000000000 ) ) ;
#3212 = CARTESIAN_POINT ( 'NONE',  ( 0.7322823680011962821, 2.160084099745246178, 0.3691886501416344335 ) ) ;
#3213 = CARTESIAN_POINT ( 'NONE',  ( 5.178851490740207453, 5.144340948726102702, 0.7216878364870317197 ) ) ;
#3214 = ORIENTED_EDGE ( 'NONE', *, *, #200691, .T. ) ;
#3215 = AXIS2_PLACEMENT_3D ( 'NONE', #186064, #37700, #103776 ) ;
#3216 = CARTESIAN_POINT ( 'NONE',  ( 0.000000000000000000, 2.999999999999999112, -2.500000000000000444 ) ) ;
#3217 = CARTESIAN_POINT ( 'NONE',  ( 9.305047017613615523, 4.518459255872631530, 7.450000000000001954 ) ) ;
#3218 = CARTESIAN_POINT ( 'NONE',  ( 0.5744775230259161480, -1.718042477583326066, -0.6180270036199516648 ) ) ;
#3219 = CARTESIAN_POINT ( 'NONE',  ( -5.610376637956639101, 5.439860920571172542, 0.000000000000000000 ) ) ;
#3220 = CARTESIAN_POINT ( 'NONE',  ( 2.777623227853244003, 1.486122661887591123, -0.8934276201044144550 ) ) ;
#3221 = DIRECTION ( 'NONE',  ( -1.276756478318932585E-15, 1.000000000000000000, -1.665334536937738262E-16 ) ) ;
#3222 = CARTESIAN_POINT ( 'NONE',  ( 6.509000000000021657, 1.267728212239338959, 2.115804336118334295 ) ) ;
#3223 = CARTESIAN_POINT ( 'NONE',  ( 8.543609354905870035, 13.11929468069890525, 0.7998128361456462443 ) ) ;
#3224 = CARTESIAN_POINT ( 'NONE',  ( 5.250558533952181861, 0.5335417292645014964, 1.745990657226546894 ) ) ;
#3225 = CARTESIAN_POINT ( 'NONE',  ( 3.590630163336411051, 1.912927474663427496, 0.4342120235502828218 ) ) ;
#3226 = AXIS2_PLACEMENT_3D ( 'NONE', #149518, #38967, #133299 ) ;
#3227 = CARTESIAN_POINT ( 'NONE',  ( -1.225000000000040057, -0.4583333326505021343, -0.7072540797573018123 ) ) ;
#3228 = CARTESIAN_POINT ( 'NONE',  ( -7.669108446824431269, 12.09904362127053545, -0.7998128361456291469 ) ) ;
#3229 = CARTESIAN_POINT ( 'NONE',  ( 5.750629710490689384, 9.860818428881154674, -0.7998128361456291469 ) ) ;
#3230 = MECHANICAL_DESIGN_GEOMETRIC_PRESENTATION_REPRESENTATION (  '', ( #89724 ), #203779 ) ;
#3231 = CARTESIAN_POINT ( 'NONE',  ( 4.635462950926918957, -0.1032030737609032217, 2.118083805499561656 ) ) ;
#3232 = EDGE_CURVE ( 'NONE', #63041, #179285, #73016, .T. ) ;
#3233 = CARTESIAN_POINT ( 'NONE',  ( 5.982890925380405456, 10.20206618957764100, 0.000000000000000000 ) ) ;
#3234 = CARTESIAN_POINT ( 'NONE',  ( -9.215791728987058562, 11.77484298861683598, -1.599625672291263179 ) ) ;
#3235 = CARTESIAN_POINT ( 'NONE',  ( 3.291909242638372923, -1.386922682245657734, -1.537212927083357217 ) ) ;
#3237 = CARTESIAN_POINT ( 'NONE',  ( 1.364683531249986537, -0.3239583329919163424, 0.7879004041258500513 ) ) ;
#3236 = FILL_AREA_STYLE ('',( #151664 ) ) ;
#3239 = ORIENTED_EDGE ( 'NONE', *, *, #70073, .T. ) ;
#3238 = CARTESIAN_POINT ( 'NONE',  ( 4.301594116137519741, 1.984124119141786657, -0.9988866673766303439 ) ) ;
#3240 = CARTESIAN_POINT ( 'NONE',  ( 3.006738235175490548, -2.214768494356106121, 0.6152039052057678425 ) ) ;
#3241 = CARTESIAN_POINT ( 'NONE',  ( 7.429504990608736037, 11.61158022244479682, -0.7216878364870267237 ) ) ;
#3243 = CARTESIAN_POINT ( 'NONE',  ( -3.285556943749998737, -2.180208332855376518, 1.896917185911908499 ) ) ;
#3242 = CARTESIAN_POINT ( 'NONE',  ( 6.455090533882185788, 8.624301270986276080, -1.443375672974078761 ) ) ;
#3244 =( NAMED_UNIT ( * ) SI_UNIT ( $, .STERADIAN. ) SOLID_ANGLE_UNIT ( ) );
#3245 = CARTESIAN_POINT ( 'NONE',  ( 0.000000000000000000, 2.099999999999997868, 0.000000000000000000 ) ) ;
#3246 = CARTESIAN_POINT ( 'NONE',  ( 3.357576282340120066, -1.451192137084562628, -1.245647637661301044 ) ) ;
#3247 = CARTESIAN_POINT ( 'NONE',  ( -0.3380113051594444973, 6.991913160484415357, -3.863100633853273624 ) ) ;
#3248 = CARTESIAN_POINT ( 'NONE',  ( 4.383650571098846704, 1.127723038421009738, 1.305118705121767420 ) ) ;
#3249 = CARTESIAN_POINT ( 'NONE',  ( 3.134000194803722383, 2.016708403948695771, -0.004836970814638129855 ) ) ;
#3250 = CARTESIAN_POINT ( 'NONE',  ( 4.483195000112350392, -2.298113444969139607, -0.05724751674645797012 ) ) ;
#3251 = CARTESIAN_POINT ( 'NONE',  ( -11.48243876534946040, 12.30000000000000071, -3.200000000000001510 ) ) ;
#3252 = CARTESIAN_POINT ( 'NONE',  ( 6.586557477600968546, -2.065026496990796101, -0.4128237726619687353 ) ) ;
#3253 = CARTESIAN_POINT ( 'NONE',  ( -5.153507786970275006, 7.105788066255672497, -1.443375672974066548 ) ) ;
#3254 = VERTEX_POINT ( 'NONE', #57848 ) ;
#3255 = CARTESIAN_POINT ( 'NONE',  ( 4.393649985211129483, -0.6784793013954493190, 1.634714195790587077 ) ) ;
#3257 = CARTESIAN_POINT ( 'NONE',  ( 0.7973255588549054140, 1.877056169618742443, 1.315483550797888812 ) ) ;
#3256 = CARTESIAN_POINT ( 'NONE',  ( 6.984385409695311964, 8.177479728513226576, 1.199719254218452935 ) ) ;
#3258 = CARTESIAN_POINT ( 'NONE',  ( 6.369096972855497363, 1.760372669148374758, -0.5393517311068628528 ) ) ;
#3259 = CARTESIAN_POINT ( 'NONE',  ( 0.4842345852037197029, 4.104600205398202917, 0.4350569428522614857 ) ) ;
#3260 = CARTESIAN_POINT ( 'NONE',  ( 6.544889499999918314, -1.757580744090202041, -1.308772488114395616 ) ) ;
#3261 = CARTESIAN_POINT ( 'NONE',  ( -8.100070429521727178, 8.414780020722290033, 0.7998128361456341429 ) ) ;
#3262 = CARTESIAN_POINT ( 'NONE',  ( 0.6801582343749796866, -0.9114583329919088150, -1.178068619123886718 ) ) ;
#3263 = SPHERICAL_SURFACE ( 'NONE', #125756, 0.08000000000000000167 ) ;
#3264 = CARTESIAN_POINT ( 'NONE',  ( 0.6433370543819162402, -0.2662039958584628829, -2.154713702345659510 ) ) ;
#3265 = CARTESIAN_POINT ( 'NONE',  ( 1.130092623156966347, 2.014433208573155110, 0.09411304420373775570 ) ) ;
#3266 = PRESENTATION_LAYER_ASSIGNMENT (  '', '', ( #3437 ) ) ;
#3267 = CARTESIAN_POINT ( 'NONE',  ( -1.500000000000001332, -0.5687499993171779566, 0.000000000000000000 ) ) ;
#3268 = CARTESIAN_POINT ( 'NONE',  ( 5.549420396211061757, -1.520166291496179323, -1.183330462961203589 ) ) ;
#3269 = CARTESIAN_POINT ( 'NONE',  ( -1.364683531250000748, 11.60937500034139802, 0.000000000000000000 ) ) ;
#3270 = CARTESIAN_POINT ( 'NONE',  ( 1.600152846412273844, 1.536270192620782238, 1.604750372702767214 ) ) ;
#3272 = ORIENTED_EDGE ( 'NONE', *, *, #211780, .T. ) ;
#3271 = CARTESIAN_POINT ( 'NONE',  ( 9.836604141914616406, 11.43479190611061647, 1.199719254218452047 ) ) ;
#3274 = CARTESIAN_POINT ( 'NONE',  ( -11.55950211276791428, 9.719999999999982876, 3.221476510067114329 ) ) ;
#3273 = LINE ( 'NONE', #134409, #50861 ) ;
#3275 = CARTESIAN_POINT ( 'NONE',  ( 3.714048807681376463, 7.355992446056095702, -0.08329438042602502201 ) ) ;
#3276 = CARTESIAN_POINT ( 'NONE',  ( 9.836604141914616406, 11.43479190611061647, 1.199719254218452047 ) ) ;
#3277 = DIRECTION ( 'NONE',  ( 0.000000000000000000, 1.000000000000000000, 0.000000000000000000 ) ) ;
#3278 = CARTESIAN_POINT ( 'NONE',  ( -11.86145016429273014, 13.40000000000000036, -1.100000000000002087 ) ) ;
#3279 = CARTESIAN_POINT ( 'NONE',  ( 4.212277857634297185, 1.593487861523819271, 0.7003764074154511521 ) ) ;
#3280 = CARTESIAN_POINT ( 'NONE',  ( 2.822649888979886335, -1.354935067541668259, 1.419045635080482093 ) ) ;
#3282 = CARTESIAN_POINT ( 'NONE',  ( -1.364683531249997417, 2.821875000341422801, 1.214306433183764966E-14 ) ) ;
#3281 = CARTESIAN_POINT ( 'NONE',  ( 5.118366684358879759, 5.930181538962194132, 1.199719254218462483 ) ) ;
#3283 = EDGE_CURVE ( 'NONE', #56620, #154122, #103069, .T. ) ;
#3284 = CARTESIAN_POINT ( 'NONE',  ( -5.877243123607416742, 6.020912620514094371, 0.3151507616369741416 ) ) ;
#3285 = CARTESIAN_POINT ( 'NONE',  ( 8.353795204314554468, 12.89784483834236184, -0.7998128361456352531 ) ) ;
#3286 = CARTESIAN_POINT ( 'NONE',  ( 0.1685210592646404493, -0.8794871949406095624, -1.863628177300826305 ) ) ;
#3287 = CARTESIAN_POINT ( 'NONE',  ( -8.453672473320708036, 9.821371626084353323, -1.199719254218446718 ) ) ;
#3288 = CARTESIAN_POINT ( 'NONE',  ( -3.429849674132936066, 6.945315686556313040, -0.7216878364870257245 ) ) ;
#3289 = CARTESIAN_POINT ( 'NONE',  ( 5.401577436481666439, -1.966305606708594667, 0.4464985920552416720 ) ) ;
#3290 = CARTESIAN_POINT ( 'NONE',  ( 1.130147970125170431, -1.436987675322987101, -1.747601730595295333 ) ) ;
#3292 = ORIENTED_EDGE ( 'NONE', *, *, #59260, .F. ) ;
#3291 = CARTESIAN_POINT ( 'NONE',  ( -6.728924311084075960, 6.744833205886536120, 1.040834085586084257E-14 ) ) ;
#3293 = CARTESIAN_POINT ( 'NONE',  ( -1.402160292154681736E-14, 0.6187500006828180465, -1.732050807568863648 ) ) ;
#3294 = CARTESIAN_POINT ( 'NONE',  ( 1.792056902697708454, -1.861051795492570049, -0.1884349046137670514 ) ) ;
#3295 = CARTESIAN_POINT ( 'NONE',  ( 1.635018144205732771, 0.5444147220468772419, 1.646514679669469849 ) ) ;
#3296 = CARTESIAN_POINT ( 'NONE',  ( 4.441096743985088580, -1.694418930461354611, -1.389946530008886905 ) ) ;
#3297 = CARTESIAN_POINT ( 'NONE',  ( 5.104635005266920267, -0.7716809915320420599, -2.174869537816104703 ) ) ;
#3298 = CARTESIAN_POINT ( 'NONE',  ( 1.041951191326966342, 0.8359002368949167705, -1.883948988615320896 ) ) ;
#3299 = CARTESIAN_POINT ( 'NONE',  ( 3.310425057758420664, 1.755882755489517999, 0.8297573096471222431 ) ) ;
#3300 = CARTESIAN_POINT ( 'NONE',  ( -5.572037945092175981, 5.603058478803387032, 0.7216878364870317197 ) ) ;
#3301 = CARTESIAN_POINT ( 'NONE',  ( 5.712129104542990277, -0.8404194184173617854, -1.671158263034502767 ) ) ;
#3302 = CARTESIAN_POINT ( 'NONE',  ( 4.034853869772982549, 7.546986718285443985, 0.4065704115671017749 ) ) ;
#3303 = CARTESIAN_POINT ( 'NONE',  ( 6.573592277014387086, 1.495820547097842068, -1.351949839681469090 ) ) ;
#3304 = CARTESIAN_POINT ( 'NONE',  ( -0.6801582343750403048, 1.598958333674738164, -1.178068619123869398 ) ) ;
#3305 = CARTESIAN_POINT ( 'NONE',  ( 4.975232503164924935, -2.001511053420693020, -0.2440319332882301961 ) ) ;
#3306 = CARTESIAN_POINT ( 'NONE',  ( -5.070386261386537363, 5.017798181146802428, 1.214306433183764966E-14 ) ) ;
#3307 = CARTESIAN_POINT ( 'NONE',  ( 8.235688245297327015, 11.69572115523387268, -1.199719254218446718 ) ) ;
#3309 = CARTESIAN_POINT ( 'NONE',  ( -6.940534579975167873, -6.675176078274437153, 6.653311379900154421 ) ) ;
#3308 = CARTESIAN_POINT ( 'NONE',  ( 1.699542765152612711, -0.6164703606487754728, 1.718597393154073671 ) ) ;
#3310 = CARTESIAN_POINT ( 'NONE',  ( -5.255720823952942489, 6.160704378480398979, -1.199719254218453823 ) ) ;
#3311 = CYLINDRICAL_SURFACE ( 'NONE', #106397, 0.08000000000000020983 ) ;
#3312 = CARTESIAN_POINT ( 'NONE',  ( -9.399990540229763880, 5.000000000000003553, 6.933248713717822476 ) ) ;
#3313 = ORIENTED_EDGE ( 'NONE', *, *, #102930, .F. ) ;
#3314 = CARTESIAN_POINT ( 'NONE',  ( -6.577113915960849155, 6.845923454808663600, -0.7216878364870338292 ) ) ;
#3315 = UNCERTAINTY_MEASURE_WITH_UNIT (LENGTH_MEASURE( 1.000000000000000082E-05 ), #57416, 'distance_accuracy_value', 'NONE');
#3316 = CARTESIAN_POINT ( 'NONE',  ( 6.610000000000006537, 0.002781820520842553934, 2.000159646111852929 ) ) ;
#3317 = CARTESIAN_POINT ( 'NONE',  ( -8.286004436246233951, 12.81875560892930466, 1.040834085586084257E-14 ) ) ;
#3318 = CARTESIAN_POINT ( 'NONE',  ( 6.076820933934619084, -1.426746821240878704, 1.429770112406039795 ) ) ;
#3320 = VERTEX_POINT ( 'NONE', #191033 ) ;
#3319 = CARTESIAN_POINT ( 'NONE',  ( 0.2234921222181683598, 1.847112181986635626, 1.041312259928407702 ) ) ;
#3321 = CARTESIAN_POINT ( 'NONE',  ( -7.123883369337781879, 7.275895117174344229, 0.7998128361456341429 ) ) ;
#3322 = CARTESIAN_POINT ( 'NONE',  ( 6.505214776458575265, 6.483838748823460563, 1.040834085586084257E-14 ) ) ;
#3323 = CARTESIAN_POINT ( 'NONE',  ( 5.805559403952022635, -0.5031923959765474130, 1.998377753082048347 ) ) ;
#3324 = CARTESIAN_POINT ( 'NONE',  ( 4.676407821165474488, 1.496050514612049742, 1.352155788975975437 ) ) ;
#3325 = ORIENTED_EDGE ( 'NONE', *, *, #12700, .F. ) ;
#3326 = ORIENTED_EDGE ( 'NONE', *, *, #166535, .F. ) ;
#3327 = DIRECTION ( 'NONE',  ( 0.000000000000000000, -1.000000000000000000, 0.000000000000000000 ) ) ;
#3328 = CARTESIAN_POINT ( 'NONE',  ( 4.729096653068339151, 4.411700938201493116, -0.7998128361456211532 ) ) ;
#3330 = VERTEX_POINT ( 'NONE', #125077 ) ;
#3329 = CARTESIAN_POINT ( 'NONE',  ( -6.656127069666307072, 6.730179434224282886, 0.7998128361456341429 ) ) ;
#3331 = CARTESIAN_POINT ( 'NONE',  ( 4.639288533706844575, 8.435234533841581950, -0.4270733708018232822 ) ) ;
#3332 = CARTESIAN_POINT ( 'NONE',  ( 4.587267430073429963, 1.242536178122002344, -1.587594670648798445 ) ) ;
#3333 = CARTESIAN_POINT ( 'NONE',  ( 3.626748959588219634, -1.700609458330613055, 0.7059681596332522124 ) ) ;
#3334 = CARTESIAN_POINT ( 'NONE',  ( -2.064209525776537379, 8.524375063532971808, 2.459883114193454734 ) ) ;
#3335 = CARTESIAN_POINT ( 'NONE',  ( 1.735461890456877487, 0.2295834678119219041, 2.296248630371207966 ) ) ;
#3336 = CARTESIAN_POINT ( 'NONE',  ( 5.806634928402749196, 9.996434193103704402, -0.7998128361456481317 ) ) ;
#3337 = EDGE_CURVE ( 'NONE', #95100, #171070, #193035, .T. ) ;
#3338 = CARTESIAN_POINT ( 'NONE',  ( 4.481803774187195444, 1.408218611193782221, 1.640057829624480101 ) ) ;
#3339 = CARTESIAN_POINT ( 'NONE',  ( 6.923409998072794558, 11.22906209772695618, 1.040834085586084257E-14 ) ) ;
#3341 = CARTESIAN_POINT ( 'NONE',  ( 2.782435679340321766, -0.5899881929209308540, -1.928257399728677601 ) ) ;
#3340 = CARTESIAN_POINT ( 'NONE',  ( 0.5384922876028491734, -1.664970009179422616, 0.9995421319052009146 ) ) ;
#3342 = CARTESIAN_POINT ( 'NONE',  ( -5.436983294280064882, 6.301900917203534291, 1.199719254218450271 ) ) ;
#3343 = CIRCLE ( 'NONE', #148711, 0.04999999999999991257 ) ;
#3344 = CARTESIAN_POINT ( 'NONE',  ( 4.060169364306280393, 1.944150891614861543, -1.225672094199470985 ) ) ;
#3345 = CARTESIAN_POINT ( 'NONE',  ( -9.498276863157586902, 15.41940897614170147, -7.333831086994896609 ) ) ;
#3346 = CARTESIAN_POINT ( 'NONE',  ( 3.098369316282158614, -0.5415621961667067552, -1.790553177708480215 ) ) ;
#3347 = CARTESIAN_POINT ( 'NONE',  ( 6.297732458894883756, -0.6644727202288897017, 1.856229495857963263 ) ) ;
#3349 = SURFACE_SIDE_STYLE ('',( #151777 ) ) ;
#3348 = CARTESIAN_POINT ( 'NONE',  ( -1.500000000000015099, -0.8395833326505166561, -0.8660254037844383745 ) ) ;
#3350 = CARTESIAN_POINT ( 'NONE',  ( 2.034064749695370100, -1.442962035976073309, -1.669870808145665020 ) ) ;
#3351 = ORIENTED_EDGE ( 'NONE', *, *, #39947, .F. ) ;
#3352 = CARTESIAN_POINT ( 'NONE',  ( -3.946537740505278613, 2.817530495244580102, 0.7750000000000135669 ) ) ;
#3353 = CARTESIAN_POINT ( 'NONE',  ( 3.517450787741589036, 6.191110788085444128, -1.199719254218446718 ) ) ;
#3354 = CARTESIAN_POINT ( 'NONE',  ( -5.284980951228653190, 5.060232619388524533, 0.000000000000000000 ) ) ;
#3355 = CARTESIAN_POINT ( 'NONE',  ( -6.983858524370814003, 9.241197259889665006, 1.443375672974064550 ) ) ;
#3356 = CARTESIAN_POINT ( 'NONE',  ( 0.4035112227387879225, -0.5299352985012796280, 1.898712856893035816 ) ) ;
#3357 = CARTESIAN_POINT ( 'NONE',  ( 0.5698726823011552867, 0.2221484770595567870, -2.296888066578778087 ) ) ;
#3359 = ADVANCED_FACE ( 'NONE', ( #193180 ), #42332, .T. ) ;
#3358 = CARTESIAN_POINT ( 'NONE',  ( 0.5726126529861442771, 1.355618539282506640, -1.418395753018865113 ) ) ;
#3360 = CARTESIAN_POINT ( 'NONE',  ( 3.819230306994053858, -1.816680642618787145, -0.9767294869839551197 ) ) ;
#3361 = CARTESIAN_POINT ( 'NONE',  ( 4.663641653420880218, 8.384739662392275861, -0.7216878364870207285 ) ) ;
#3362 = CARTESIAN_POINT ( 'NONE',  ( 5.830888582329017744, 8.960397891762626799, -1.199719254218452047 ) ) ;
#3363 = ORIENTED_EDGE ( 'NONE', *, *, #64050, .T. ) ;
#3364 = CARTESIAN_POINT ( 'NONE',  ( 7.036318535368067728, 10.19249347702934294, -1.082531754730537976 ) ) ;
#3365 = CARTESIAN_POINT ( 'NONE',  ( 1.364683531249990311, 4.946875000341417916, 1.214306433183764966E-14 ) ) ;
#3366 = FACE_OUTER_BOUND ( 'NONE', #203772, .T. ) ;
#3367 = CARTESIAN_POINT ( 'NONE',  ( 5.138177029454847222, 6.057256624861201644, 1.082531754730560403 ) ) ;
#3368 = CARTESIAN_POINT ( 'NONE',  ( 6.848074921520021618, -0.9335981340678388696, 1.958013476854936652 ) ) ;
#3369 = B_SPLINE_CURVE_WITH_KNOTS ( 'NONE', 3,
 ( #163944, #67452, #212656, #15519, #199603, #168192 ),
 .UNSPECIFIED., .F., .F.,
 ( 4, 1, 1, 4 ),
 ( 0.000000000000000000, 0.3720156466326168809, 0.4720156466326168587, 1.000000000000000000 ),
 .UNSPECIFIED. ) ;
#3371 = CARTESIAN_POINT ( 'NONE',  ( 5.478019777291557979, -1.797689181224306321, -0.3974485807837144224 ) ) ;
#3370 = FACE_OUTER_BOUND ( 'NONE', #25693, .T. ) ;
#3372 = CARTESIAN_POINT ( 'NONE',  ( 5.299301323368958094, 6.361497809228795930, -1.122821758042211959 ) ) ;
#3373 = CARTESIAN_POINT ( 'NONE',  ( -0.4000000000000322742, -2.775557561562891351E-14, 0.4999999999999535927 ) ) ;
#3374 = CARTESIAN_POINT ( 'NONE',  ( 0.5966796567213605851, 1.558732183387041781, -1.033768272189788950 ) ) ;
#3375 = CARTESIAN_POINT ( 'NONE',  ( -4.797329538616279976, 6.965272035667838146, 1.434408638962878957 ) ) ;
#3376 = CARTESIAN_POINT ( 'NONE',  ( 11.41381675112453387, 13.40000000000000036, -3.704697986577182522 ) ) ;
#3377 = CARTESIAN_POINT ( 'NONE',  ( 6.007156502879952953, 7.179297369210805080, -1.191424252104013037 ) ) ;
#3378 = CARTESIAN_POINT ( 'NONE',  ( 1.364683531249988535, 5.467708333674750953, -0.7879004041258300672 ) ) ;
#3379 = CARTESIAN_POINT ( 'NONE',  ( 1.400873256076972329, -0.2815782128867699852, -1.891321520182134508 ) ) ;
#3380 = CARTESIAN_POINT ( 'NONE',  ( 2.799370285489965138, -0.5572909556486020932, 1.679871745949900408 ) ) ;
#3381 = CARTESIAN_POINT ( 'NONE',  ( 0.01216826571975513152, -1.911853497171299265, -0.04704278909201110859 ) ) ;
#3383 = CARTESIAN_POINT ( 'NONE',  ( 4.411684386003834391, -1.181747345438967312, -1.507543049613221386 ) ) ;
#3382 = CARTESIAN_POINT ( 'NONE',  ( -10.01677656239806247, 10.58066083241955901, 0.7998128361456462443 ) ) ;
#3384 = CARTESIAN_POINT ( 'NONE',  ( -0.1409997244346122836, 0.7174646053854060179, -2.082770303449644977 ) ) ;
#3385 = CARTESIAN_POINT ( 'NONE',  ( 5.213322861785598228, -1.662839039401903696, -1.055205849181278799 ) ) ;
#3386 = CARTESIAN_POINT ( 'NONE',  ( 0.5453776912951785460, 0.1620316879334358084, 2.114494688702214020 ) ) ;
#3387 = DIRECTION ( 'NONE',  ( 0.000000000000000000, 0.000000000000000000, 1.000000000000000000 ) ) ;
#3388 = CARTESIAN_POINT ( 'NONE',  ( 4.258574955689950592, -1.386304660245713860, 1.256184814050688603 ) ) ;
#3390 = ORIENTED_EDGE ( 'NONE', *, *, #85316, .T. ) ;
#3389 = CARTESIAN_POINT ( 'NONE',  ( 5.760297821273290708, 0.7050700890500715134, 1.574392225784694066 ) ) ;
#3392 = CARTESIAN_POINT ( 'NONE',  ( 4.690757960648234359, 4.574898496952131133, 0.7216878364870317197 ) ) ;
#3391 = CARTESIAN_POINT ( 'NONE',  ( 2.912931060594741162, 1.598032330669514778, -1.522282275181946032 ) ) ;
#3393 =( GEOMETRIC_REPRESENTATION_CONTEXT ( 3 ) GLOBAL_UNCERTAINTY_ASSIGNED_CONTEXT ( ( #195972 ) ) GLOBAL_UNIT_ASSIGNED_CONTEXT ( ( #189438, #41080, #178527 ) ) REPRESENTATION_CONTEXT ( 'NONE', 'WORKASPACE' ) );
#3394 = CARTESIAN_POINT ( 'NONE',  ( 0.6823417656249899377, 4.988541667008086655, -1.181850606188754593 ) ) ;
#3395 = CARTESIAN_POINT ( 'NONE',  ( 1.152864133210535824, -0.4991712053786099279, -2.001264041248071113 ) ) ;
#3396 = CARTESIAN_POINT ( 'NONE',  ( 6.479907352327590964, 9.647310113435821677, 1.199719254218462483 ) ) ;
#3397 = CARTESIAN_POINT ( 'NONE',  ( -10.31505594189871111, 10.92865344183699428, -0.7998128361456291469 ) ) ;
#3398 = CYLINDRICAL_SURFACE ( 'NONE', #154398, 1.500000000000000222 ) ;
#3399 = CARTESIAN_POINT ( 'NONE',  ( 11.86145016429272836, 10.90000000000000036, -1.100000000000000533 ) ) ;
#3400 = CARTESIAN_POINT ( 'NONE',  ( -4.669937115657131876, 8.128295656576590034, -0.7159178489368930309 ) ) ;
#3401 = ORIENTED_EDGE ( 'NONE', *, *, #139587, .T. ) ;
#3402 = CARTESIAN_POINT ( 'NONE',  ( 3.086448098943677998, 1.152334561581969785, -1.719836228861029603 ) ) ;
#3403 = CARTESIAN_POINT ( 'NONE',  ( 1.499999999999990896, 5.025000000000022560, 1.214306433183764966E-14 ) ) ;
#3404 = CARTESIAN_POINT ( 'NONE',  ( 5.684946482831785275, 5.526859072925533134, -0.7998128361456231517 ) ) ;
#3405 = CARTESIAN_POINT ( 'NONE',  ( -6.486551268120854807, 6.767445667853342783, -0.2095380678983837508 ) ) ;
#3407 = EDGE_CURVE ( 'NONE', #7144, #39666, #210193, .T. ) ;
#3406 = CARTESIAN_POINT ( 'NONE',  ( 1.190109814708179670, 1.204940744830071075, 1.620691797242173937 ) ) ;
#3408 = CARTESIAN_POINT ( 'NONE',  ( -11.84668730067608600, 13.39999999999998259, 1.319999999999998286 ) ) ;
#3409 = ORIENTED_EDGE ( 'NONE', *, *, #85916, .F. ) ;
#3410 = EDGE_CURVE ( 'NONE', #81409, #108056, #78356, .T. ) ;
#3412 = CARTESIAN_POINT ( 'NONE',  ( 7.293923454472077239, 10.49303254931736262, 1.082531754730558626 ) ) ;
#3411 = CARTESIAN_POINT ( 'NONE',  ( 0.07499057489260704812, 2.034159190454051913, -2.372362849262329210 ) ) ;
#3413 = CARTESIAN_POINT ( 'NONE',  ( 6.257185446134499784, -2.006139278912861368, -0.2004013049526700285 ) ) ;
#3414 = CARTESIAN_POINT ( 'NONE',  ( 5.946487413881851758, -1.349596479577100272, 1.359900094196204279 ) ) ;
#3415 = CARTESIAN_POINT ( 'NONE',  ( 6.539320575229258914, 2.958022083381315337, 2.556018433155104574 ) ) ;
#3416 = CARTESIAN_POINT ( 'NONE',  ( 4.107102485094754840, -0.3736803571842537974, 2.159302612355806339 ) ) ;
#3417 = CARTESIAN_POINT ( 'NONE',  ( 1.499999999999989120, 3.035416667349485564, 0.8660254037844524744 ) ) ;
#3418 = CARTESIAN_POINT ( 'NONE',  ( 3.568532368641282648, 0.6928216322696268969, 1.782650395559831180 ) ) ;
#3419 = CARTESIAN_POINT ( 'NONE',  ( -4.554649539187067830, 7.401175998105142817, 1.199719254218464037 ) ) ;
#3420 = CARTESIAN_POINT ( 'NONE',  ( 4.541618270453549044, 5.361271406026338227, -1.082531754730548412 ) ) ;
#3422 = CARTESIAN_POINT ( 'NONE',  ( 1.212517793387542842, 1.944078472882956987, 0.5350667013180390175 ) ) ;
#3421 = DIRECTION ( 'NONE',  ( 0.8079921913844798631, -2.168404344971001295E-14, -0.5891931929865669160 ) ) ;
#3423 = CARTESIAN_POINT ( 'NONE',  ( 0.6823417656249934904, 11.50520833367473017, 1.181850606188764807 ) ) ;
#3425 = CARTESIAN_POINT ( 'NONE',  ( -5.978219388983010418, 5.939287140093762574, -0.7998128361456362523 ) ) ;
#3424 = CARTESIAN_POINT ( 'NONE',  ( -0.1112335732281382050, -0.5161050057324081397, -2.242239947022279356 ) ) ;
#3427 = EDGE_LOOP ( 'NONE', ( #194768, #195116, #182169, #158522 ) ) ;
#3426 = CARTESIAN_POINT ( 'NONE',  ( 4.717633463169556229, -1.691034389814783712, 0.3384810450017295969 ) ) ;
#3428 = CARTESIAN_POINT ( 'NONE',  ( -0.1405533004718676759, 7.629137130509054288, -2.320277334263821434 ) ) ;
#3429 = CARTESIAN_POINT ( 'NONE',  ( 5.933664784275179294, 10.07435934829639912, -0.7998128361456291469 ) ) ;
#3430 = CARTESIAN_POINT ( 'NONE',  ( 4.578903193113299963, 6.365139696764064325, 1.599625672291267398 ) ) ;
#3431 = CARTESIAN_POINT ( 'NONE',  ( -3.094265954482842140, 2.800000000000024691, -2.490342512183689294 ) ) ;
#3432 = CARTESIAN_POINT ( 'NONE',  ( 1.451531895509536874, 1.483362660712842063, 1.284035263222626844 ) ) ;
#3433 = CARTESIAN_POINT ( 'NONE',  ( -4.124095526617549778E-13, -0.9769569599453676867, 3.449959810851647823 ) ) ;
#3434 = CARTESIAN_POINT ( 'NONE',  ( 4.517891501851804215, 6.293959390292322986, -1.599625672291255185 ) ) ;
#3435 = CARTESIAN_POINT ( 'NONE',  ( 0.07556134207195497332, 5.719716873484223640, -2.838244455430352087 ) ) ;
#3436 = ORIENTED_EDGE ( 'NONE', *, *, #120152, .T. ) ;
#3437 = STYLED_ITEM ( 'NONE', ( #132805 ), #122417 ) ;
#3438 = ORIENTED_EDGE ( 'NONE', *, *, #195789, .T. ) ;
#3439 = CARTESIAN_POINT ( 'NONE',  ( 3.738735263490736926, 1.721172062854194218, 0.5650376532472713986 ) ) ;
#3440 = ORIENTED_EDGE ( 'NONE', *, *, #3532, .T. ) ;
#3441 = CARTESIAN_POINT ( 'NONE',  ( 4.004454267989866700, 5.765225627445230927, 1.599625672291262513 ) ) ;
#3442 = CARTESIAN_POINT ( 'NONE',  ( 4.934136933359813071, -0.9735637292621384109, -1.527415209752202019 ) ) ;
#3443 = DIRECTION ( 'NONE',  ( 0.000000000000000000, -1.000000000000000000, 0.000000000000000000 ) ) ;
#3444 = DIRECTION ( 'NONE',  ( -1.000000000000000000, 4.984021416236792516E-16, 0.000000000000000000 ) ) ;
#3445 = CARTESIAN_POINT ( 'NONE',  ( 5.808322585208748556, 6.028124808163927817, -0.4837759047566763670 ) ) ;
#3447 = CARTESIAN_POINT ( 'NONE',  ( 10.37606763316019531, 10.99983374830873650, 0.7998128361456462443 ) ) ;
#3446 = CARTESIAN_POINT ( 'NONE',  ( 4.615577964900333008, 0.4086796715298928184, -1.815441397462829398 ) ) ;
#3448 = CARTESIAN_POINT ( 'NONE',  ( 2.478032317504985649, -1.910654254087537307, -0.1382841363062360662 ) ) ;
#3449 = CARTESIAN_POINT ( 'NONE',  ( -6.773376349083140013, -7.473374494058229622, -6.661184041420940893 ) ) ;
#3450 = CARTESIAN_POINT ( 'NONE',  ( -10.48266952940149466, 5.268049057482275366, -5.154014898524191146 ) ) ;
#3451 = CARTESIAN_POINT ( 'NONE',  ( -15.75000000000000000, 10.90000000000000036, -1.400000000000001910 ) ) ;
#3452 = CARTESIAN_POINT ( 'NONE',  ( 4.868786560638885597, 7.733982516503781213, 1.082531754730548412 ) ) ;
#3453 = CARTESIAN_POINT ( 'NONE',  ( 5.490689023854504747, 9.349628261231513804, 1.040834085586084257E-14 ) ) ;
#3454 = CARTESIAN_POINT ( 'NONE',  ( -2.819205876637805641, 5.376491725131008259, -1.199719254218446718 ) ) ;
#3455 = CARTESIAN_POINT ( 'NONE',  ( 0.4972265960483426284, 1.796464302094663346, -1.202062886709959422 ) ) ;
#3456 = CARTESIAN_POINT ( 'NONE',  ( -6.074935347375019390, 9.245119117649618801, 1.199719254218452047 ) ) ;
#3457 = CARTESIAN_POINT ( 'NONE',  ( 4.193214648376505593, 8.114110533073061404, 0.000000000000000000 ) ) ;
#3458 = CARTESIAN_POINT ( 'NONE',  ( 1.219449367515994309, -1.782015241123528826, 0.3957228718986585680 ) ) ;
#3459 = CARTESIAN_POINT ( 'NONE',  ( -4.822949958159302497, 6.649860922651058992, -1.599625672291256295 ) ) ;
#3460 = CARTESIAN_POINT ( 'NONE',  ( 1.869861807837460921, 0.9356042063937074493, 1.567457579366556386 ) ) ;
#3461 = FACE_OUTER_BOUND ( 'NONE', #173063, .T. ) ;
#3462 = CARTESIAN_POINT ( 'NONE',  ( 2.390748813209525814, -1.831196095803063528, -0.5514187292172747501 ) ) ;
#3463 = CARTESIAN_POINT ( 'NONE',  ( 3.209381719453743287, -1.608569549925453313, -1.136198915559688105 ) ) ;
#3465 = B_SPLINE_CURVE_WITH_KNOTS ( 'NONE', 3,
 ( #152853, #149657, #133439, #18570, #199446, #35891, #54290, #84648, #20692, #202640, #150737, #134505, #101968, #4430, #2297, #68374, #151797, #3372 ),
 .UNSPECIFIED., .F., .F.,
 ( 4, 2, 2, 2, 2, 2, 2, 2, 4 ),
 ( 0.7195170131146431114, 0.7275020556221073464, 0.7354870981295715815, 0.7434721406370357055, 0.7514571831444999406, 0.7594422256519641756, 0.7674272681594282997, 0.7754123106668925347, 0.7833973531743566587 ),
 .UNSPECIFIED. ) ;
#3464 = CARTESIAN_POINT ( 'NONE',  ( 3.737779845645439636, 1.932976868219363764, 0.1874624384631869700 ) ) ;
#3466 = CARTESIAN_POINT ( 'NONE',  ( -3.156015896931072540, 6.904045323053366268, 0.000000000000000000 ) ) ;
#3468 = CARTESIAN_POINT ( 'NONE',  ( 4.640951271726033056, 2.030106984047326701, 0.6129599860185754867 ) ) ;
#3467 = CARTESIAN_POINT ( 'NONE',  ( 5.671053392266061977, 9.838255734277600695, 0.7998128361456331437 ) ) ;
#3469 = CARTESIAN_POINT ( 'NONE',  ( 6.756361134959112391, -6.891066458783287274, 6.828399852920186142 ) ) ;
#3470 = CARTESIAN_POINT ( 'NONE',  ( 8.748035429315576650, 11.22912730566677553, -1.599625672291255185 ) ) ;
#3471 = CARTESIAN_POINT ( 'NONE',  ( 5.971451247601332391, 6.106144735068791185, -0.6754856502540294017 ) ) ;
#3472 = CARTESIAN_POINT ( 'NONE',  ( 0.000000000000000000, 1.000000000000000888, 0.000000000000000000 ) ) ;
#3473 = ORIENTED_EDGE ( 'NONE', *, *, #13918, .F. ) ;
#3474 = CARTESIAN_POINT ( 'NONE',  ( 5.525830126021535449, 8.604496359403894346, -1.199719254218452047 ) ) ;
#3475 = LINE ( 'NONE', #4532, #47724 ) ;
#3476 = CARTESIAN_POINT ( 'NONE',  ( 3.703562413045482060, -0.5285312144065814621, 1.747510042522756990 ) ) ;
#3477 = DIRECTION ( 'NONE',  ( 0.000000000000000000, -1.000000000000000000, 0.000000000000000000 ) ) ;
#3478 = CARTESIAN_POINT ( 'NONE',  ( -8.026063749610043985, 12.30756544127966912, -0.7216878364870267237 ) ) ;
#3479 = CARTESIAN_POINT ( 'NONE',  ( -5.242543201390849283, 7.800132786123255002, 1.293859303942331840 ) ) ;
#3480 = CARTESIAN_POINT ( 'NONE',  ( 3.511198596259284876, 6.271927390929313617, -1.052294140492317842 ) ) ;
#3481 = CARTESIAN_POINT ( 'NONE',  ( 4.504681594071535677, 1.446009304718363087, -1.186774495104812699 ) ) ;
#3482 = CARTESIAN_POINT ( 'NONE',  ( 8.599949509769960088, 8.927695937686774386, 1.040834085586084257E-14 ) ) ;
#3483 = CARTESIAN_POINT ( 'NONE',  ( 3.053258290938072772, -1.575281680543440643, -1.108752609043755832 ) ) ;
#3484 = CARTESIAN_POINT ( 'NONE',  ( 6.578960362708798471, 1.829258725439562916, 0.7091506158454219388 ) ) ;
#3485 = CARTESIAN_POINT ( 'NONE',  ( -1.364683531250010295, 9.192708333674733723, 0.7879004041258445001 ) ) ;
#3486 = CARTESIAN_POINT ( 'NONE',  ( -6.911959384868566758, 6.958374125301778790, 1.040834085586084257E-14 ) ) ;
#3487 = COLOUR_RGB ( '', 0.31764706, 0.68627451, 0.89019608) ;
#3488 = CARTESIAN_POINT ( 'NONE',  ( -3.309598895067336510, 6.875299454304925284, 0.000000000000000000 ) ) ;
#3489 = CARTESIAN_POINT ( 'NONE',  ( 1.370887597065591823, -0.3147031148599331307, -2.093612404753260492 ) ) ;
#3490 = CARTESIAN_POINT ( 'NONE',  ( 8.218213668177886788, 12.73966637951625813, 0.7998128361456462443 ) ) ;
#3491 = CARTESIAN_POINT ( 'NONE',  ( -5.339680242214989825, 4.685059543140638105, 2.440369273555149210 ) ) ;
#3492 = CARTESIAN_POINT ( 'NONE',  ( 6.121949425127414024, 2.040613181561203859, -0.3481179853092666865 ) ) ;
#3494 = CARTESIAN_POINT ( 'NONE',  ( 4.021084497595363239, 7.798870403269500429, 0.3307836955792880507 ) ) ;
#3493 = CARTESIAN_POINT ( 'NONE',  ( 0.09881949811249221560, -0.4921898920670075839, 1.774194203830472993 ) ) ;
#3495 = CARTESIAN_POINT ( 'NONE',  ( 5.871801794802778751, -0.3338885390306855494, -2.274238935559732333 ) ) ;
#3496 = CARTESIAN_POINT ( 'NONE',  ( 5.666945020832177882, 6.674152614801420746, 1.082531754730558626 ) ) ;
#3498 = DIRECTION ( 'NONE',  ( 1.000000000000000000, 0.000000000000000000, 0.000000000000000000 ) ) ;
#3497 = CARTESIAN_POINT ( 'NONE',  ( 3.933273961740298752, 5.682181936820735579, 1.443375672974058777 ) ) ;
#3499 = CARTESIAN_POINT ( 'NONE',  ( 1.641004737452517626, -1.934627630680013199, 1.229243952562808939 ) ) ;
#3500 = CARTESIAN_POINT ( 'NONE',  ( -0.005637892868452093476, -0.3948761927005627337, -1.788892068844874395 ) ) ;
#3501 = CARTESIAN_POINT ( 'NONE',  ( -6.069210040772897052, 7.109775131437022999, -1.199719254218453823 ) ) ;
#3502 = CARTESIAN_POINT ( 'NONE',  ( 5.947205882781483766, 0.5613781043299302942, -1.859040749089553524 ) ) ;
#3503 = ORIENTED_EDGE ( 'NONE', *, *, #34131, .T. ) ;
#3504 = CARTESIAN_POINT ( 'NONE',  ( 9.070041577417981671, 9.684062716516882219, -0.7216878364870197293 ) ) ;
#3505 = CARTESIAN_POINT ( 'NONE',  ( 0.6857920578585029459, 1.939116618559855842, -0.5408100507186993644 ) ) ;
#3506 = CARTESIAN_POINT ( 'NONE',  ( 6.315638730379727228, -1.320822524126588515, -1.523799118890494020 ) ) ;
#3508 = CARTESIAN_POINT ( 'NONE',  ( -11.78331023100045627, 9.719999999999998863, -1.800000000000001155 ) ) ;
#3507 = CARTESIAN_POINT ( 'NONE',  ( -9.013473194986783454, 9.410140237106395134, -0.7998128361456291469 ) ) ;
#3509 = CARTESIAN_POINT ( 'NONE',  ( 1.419999999999989049, 6.280000000000042881, -2.873333333333328632 ) ) ;
#3511 = CARTESIAN_POINT ( 'NONE',  ( 1.709447022217532641, -1.756973726300320449, 0.2123998563456699906 ) ) ;
#3510 = CARTESIAN_POINT ( 'NONE',  ( 2.712926231669846810, -0.2040156676378352685, 2.080649193556554533 ) ) ;
#3512 = DIRECTION ( 'NONE',  ( 0.000000000000000000, 0.000000000000000000, 1.000000000000000000 ) ) ;
#3514 = CARTESIAN_POINT ( 'NONE',  ( 4.470831859796895458, 0.002540009476469616122, -2.292435214262526166 ) ) ;
#3513 = CARTESIAN_POINT ( 'NONE',  ( -0.6125000000000192513, 1.958333333333318826, -1.060881119635962211 ) ) ;
#3515 = CARTESIAN_POINT ( 'NONE',  ( 3.257457426684560620, 0.7833967258410595713, 1.554110229252920528 ) ) ;
#3516 = CARTESIAN_POINT ( 'NONE',  ( 4.241003122976366058, 3.842258486427521103, -0.7998128361456211532 ) ) ;
#3517 = CARTESIAN_POINT ( 'NONE',  ( 3.444447550215405052, 1.098527548611628601, 1.341433071544478217 ) ) ;
#3518 = CARTESIAN_POINT ( 'NONE',  ( 3.104148162264197985, 0.7838245717375692534, -2.024915708489416044 ) ) ;
#3519 = CARTESIAN_POINT ( 'NONE',  ( 4.955668840994886359, 5.740367388370866131, 1.199719254218462483 ) ) ;
#3520 = CARTESIAN_POINT ( 'NONE',  ( 5.014861385384292269, 0.1531656238677771009, 2.010801456750747285 ) ) ;
#3521 = CARTESIAN_POINT ( 'NONE',  ( 2.468750000000001776, 0.7852924748298570901, -1.895863743164139859 ) ) ;
#3522 = CARTESIAN_POINT ( 'NONE',  ( 1.499999999999989120, 4.285416667349482900, 0.8660254037844524744 ) ) ;
#3523 = CARTESIAN_POINT ( 'NONE',  ( 1.641497204607924809, -1.393575563620005786, -1.330239063421148948 ) ) ;
#3524 = CARTESIAN_POINT ( 'NONE',  ( 1.499999999999997113, 8.677083334016131744, -0.8660254037844378194 ) ) ;
#3525 = CARTESIAN_POINT ( 'NONE',  ( 4.517978939158282969, -0.5908935252547321548, 2.141346583060988351 ) ) ;
#3526 = EDGE_LOOP ( 'NONE', ( #192939, #177773 ) ) ;
#3527 = DIRECTION ( 'NONE',  ( 1.000000000000000000, -0.000000000000000000, -0.000000000000000000 ) ) ;
#3528 = CARTESIAN_POINT ( 'NONE',  ( 0.7499999999999885647, 1.816666666666688634, -1.299038105676652899 ) ) ;
#3529 = CARTESIAN_POINT ( 'NONE',  ( 6.531277313481192337, 8.642909503859968368, 1.599625672291281386 ) ) ;
#3530 = CARTESIAN_POINT ( 'NONE',  ( 4.867013957181530515, 5.740899707208986236, -1.082531754730548412 ) ) ;
#3531 = CARTESIAN_POINT ( 'NONE',  ( 1.001543065824772753E-15, -2.471874999522041705, 3.793834371823810780 ) ) ;
#3532 = EDGE_CURVE ( 'NONE', #157260, #71638, #13059, .T. ) ;
#3533 = CARTESIAN_POINT ( 'NONE',  ( 0.9619568641448449364, -1.754440713604523916, -1.362318395052774633 ) ) ;
#3535 = CARTESIAN_POINT ( 'NONE',  ( 6.021922112293466967, 1.933069186966931863, -0.3339256516061983038 ) ) ;
#3534 = AXIS2_PLACEMENT_3D ( 'NONE', #143410, #145552, #92518 ) ;
#3536 = CARTESIAN_POINT ( 'NONE',  ( 8.270110514656026979, 10.67154823856396817, 1.443375672974076540 ) ) ;
#3537 = EDGE_CURVE ( 'NONE', #105884, #200355, #58064, .T. ) ;
#3538 = CARTESIAN_POINT ( 'NONE',  ( 0.4774960025711667555, 3.000292809610445754, 1.942428730326982711 ) ) ;
#3539 = CARTESIAN_POINT ( 'NONE',  ( 0.4741787938652639034, 1.244221353789766837, 1.767418780601250017 ) ) ;
#3540 = CARTESIAN_POINT ( 'NONE',  ( 6.215487077222150880, 6.216099443039444949, 0.000000000000000000 ) ) ;
#3541 = B_SPLINE_CURVE_WITH_KNOTS ( 'NONE', 3,
 ( #196882, #64746, #148151, #181682 ),
 .UNSPECIFIED., .F., .F.,
 ( 4, 4 ),
 ( 0.000000000000000000, 9.170750102249441526E-05 ),
 .UNSPECIFIED. ) ;
#3542 = CARTESIAN_POINT ( 'NONE',  ( -4.584065335196305213, 6.441438539186039591, 1.443375672974058777 ) ) ;
#3543 = CARTESIAN_POINT ( 'NONE',  ( 3.631348232279749233, 0.05352869315983609100, -2.062151203995182147 ) ) ;
#3544 = CARTESIAN_POINT ( 'NONE',  ( -4.218558352146454915, 8.073401844146177453, 1.040834085586084257E-14 ) ) ;
#3545 = B_SPLINE_CURVE_WITH_KNOTS ( 'NONE', 3,
 ( #74509, #140613, #124411, #190369, #86484, #21450, #4136, #70204 ),
 .UNSPECIFIED., .F., .F.,
 ( 4, 2, 2, 4 ),
 ( 0.000000000000000000, 0.0007626201316526405984, 0.001525240263305281197, 0.003050480526610564996 ),
 .UNSPECIFIED. ) ;
#3546 = CARTESIAN_POINT ( 'NONE',  ( 1.499999999999987121, 3.577083334016152527, -0.8660254037844262731 ) ) ;
#3547 = CARTESIAN_POINT ( 'NONE',  ( 0.6823417656249899377, 5.738541667008087543, -1.181850606188754593 ) ) ;
#3548 = CARTESIAN_POINT ( 'NONE',  ( 6.432864026670258362, 0.1834693771665257822, 1.861492386831371748 ) ) ;
#3549 = CARTESIAN_POINT ( 'NONE',  ( 4.693871744853702843, 1.512258256419211078, 0.8485452647231973566 ) ) ;
#3550 = CARTESIAN_POINT ( 'NONE',  ( 3.333312927339195930, 0.7792813341828198626, -1.556285420506423600 ) ) ;
#3551 = CARTESIAN_POINT ( 'NONE',  ( 2.191363998320290385, 1.774703082125920428, 1.451028844865470901 ) ) ;
#3552 = CARTESIAN_POINT ( 'NONE',  ( 1.364683531249990311, 3.946875000341417028, 1.214306433183764966E-14 ) ) ;
#3553 = CARTESIAN_POINT ( 'NONE',  ( 5.829650940335100451, 1.029561424092540589, -1.819573902328343484 ) ) ;
#3554 = CARTESIAN_POINT ( 'NONE',  ( 0.2691533882960769897, 1.057504993221158873, 1.506941669042777265 ) ) ;
#3555 = DIRECTION ( 'NONE',  ( -5.578564026256490882E-16, -1.000000000000000000, -9.066213480720158442E-32 ) ) ;
#3556 = CARTESIAN_POINT ( 'NONE',  ( 1.582657950916711131, -0.6767122143778031562, 1.899619169727875700 ) ) ;
#3557 = DIRECTION ( 'NONE',  ( 0.000000000000000000, 1.000000000000000000, 0.000000000000000000 ) ) ;
#3558 = CARTESIAN_POINT ( 'NONE',  ( 7.320801413324473650, 15.00000000000000000, -10.35317664616355771 ) ) ;
#3559 = CARTESIAN_POINT ( 'NONE',  ( -9.027031348600448979, 9.425958082989001952, 1.040834085586084257E-14 ) ) ;
#3560 = CARTESIAN_POINT ( 'NONE',  ( 5.632522751473472589, 8.658694745772667289, -1.199719254218440723 ) ) ;
#3561 = CARTESIAN_POINT ( 'NONE',  ( 2.912858673564645784, -0.6176872867308530468, -2.028511212565413224 ) ) ;
#3562 = CARTESIAN_POINT ( 'NONE',  ( -1.602468905319636405E-14, -1.053124999658583638, -1.575800808251665908 ) ) ;
#3563 = CARTESIAN_POINT ( 'NONE',  ( 5.057177669875371429, -1.544152220135000420, -0.9737345633797565014 ) ) ;
#3564 = ORIENTED_EDGE ( 'NONE', *, *, #105759, .T. ) ;
#3565 = CARTESIAN_POINT ( 'NONE',  ( -5.257529707049291900, 9.355811434857983500, 0.7998128361456291469 ) ) ;
#3566 = CARTESIAN_POINT ( 'NONE',  ( 2.665787623643367521, -4.288499431575266918, -2.473491168755026948 ) ) ;
#3567 = CARTESIAN_POINT ( 'NONE',  ( -4.720210035852093533, 8.658662141802762946, -0.7998128361456281477 ) ) ;
#3568 = CARTESIAN_POINT ( 'NONE',  ( 1.617450697425420802, 1.681603173096592796, 1.118491831857356456 ) ) ;
#3569 = CARTESIAN_POINT ( 'NONE',  ( 6.791986947960565679, -0.9495855537378705691, 1.990061496475347802 ) ) ;
#3570 = CARTESIAN_POINT ( 'NONE',  ( 10.24048609702354717, 10.84165528948263457, -0.7998128361456281477 ) ) ;
#3571 = EDGE_CURVE ( 'NONE', #129112, #183707, #115658, .T. ) ;
#3572 = CARTESIAN_POINT ( 'NONE',  ( 3.889374201350876525, -1.720966249256241865, 0.7085912657165122086 ) ) ;
#3573 = CARTESIAN_POINT ( 'NONE',  ( 7.567422294721922960, 11.98040977715095323, 0.7998128361456462443 ) ) ;
#3574 = CARTESIAN_POINT ( 'NONE',  ( 11.92051736251532823, 13.65180243792678638, -1.381800029228912763 ) ) ;
#3575 = CARTESIAN_POINT ( 'NONE',  ( -3.928111819657352566, 5.605883094398769195, 1.599625672291267398 ) ) ;
#3576 = CARTESIAN_POINT ( 'NONE',  ( -6.184490626128011925, 10.36698949712469364, -0.7998128361456291469 ) ) ;
#3577 = CARTESIAN_POINT ( 'NONE',  ( 5.250558533952181861, 0.5335417292645014964, 1.745990657226546894 ) ) ;
#3579 = CARTESIAN_POINT ( 'NONE',  ( -4.031038109533945146, 7.773819255970239261, -0.5157005294549130703 ) ) ;
#3578 = CARTESIAN_POINT ( 'NONE',  ( -6.180537922983287302, 8.303989891604203422, -1.599625672291271394 ) ) ;
#3580 = FACE_OUTER_BOUND ( 'NONE', #92498, .T. ) ;
#3581 = CARTESIAN_POINT ( 'NONE',  ( 1.950155486560195772, 1.191851295230661467, 1.259505011191792923 ) ) ;
#3582 = CARTESIAN_POINT ( 'NONE',  ( 0.3920123891120600446, 1.449622948667350641, -0.9626461102210502885 ) ) ;
#3584 = CARTESIAN_POINT ( 'NONE',  ( 8.446366511633696561, 8.956441806435218922, 1.040834085586084257E-14 ) ) ;
#3583 = CARTESIAN_POINT ( 'NONE',  ( 5.285860113471884780, 1.546311580504238670, 1.713158476844111933 ) ) ;
#3585 = CARTESIAN_POINT ( 'NONE',  ( -11.14501278000869355, 7.223412960316487386, -3.546411330735405265 ) ) ;
#3586 = CARTESIAN_POINT ( 'NONE',  ( 1.669287087933446490, 0.1544451976582127406, -2.055073672515697059 ) ) ;
#3587 = CARTESIAN_POINT ( 'NONE',  ( 6.837282040791485827, -1.423258038995322661, 1.805902563099166080 ) ) ;
#3588 = CARTESIAN_POINT ( 'NONE',  ( 7.204675194429079505E-15, -1.487500000000000044, -3.475000000000000089 ) ) ;
#3589 = CARTESIAN_POINT ( 'NONE',  ( -5.576146316970437944, 9.727530813099326323, 0.000000000000000000 ) ) ;
#3590 = CARTESIAN_POINT ( 'NONE',  ( 0.08089089327990153788, -0.1352431037574420292, -1.940231264204687722 ) ) ;
#3592 = CARTESIAN_POINT ( 'NONE',  ( -7.105881907338169157, 8.423188659050232729, -1.082531754730549967 ) ) ;
#3591 = CARTESIAN_POINT ( 'NONE',  ( 3.093911922779784440, 1.216618333484908998, 1.475457842794763996 ) ) ;
#3593 = CARTESIAN_POINT ( 'NONE',  ( 4.705825944637973990, -0.5905853116198942487, 2.126329296355852883 ) ) ;
#3594 = CARTESIAN_POINT ( 'NONE',  ( -0.6125000000000158096, 2.270833334016133964, -1.060881119635972647 ) ) ;
#3595 = B_SPLINE_CURVE_WITH_KNOTS ( 'NONE', 3,
 ( #166565, #52809, #5093, #18154, #84241, #20297, #86383, #182800, #150328, #4029, #67954 ),
 .UNSPECIFIED., .F., .F.,
 ( 4, 1, 1, 1, 1, 1, 1, 1, 4 ),
 ( 0.000000000000000000, 0.2255509035172358623, 0.3975895543896152406, 0.5252637114030099807, 0.6177357421269481508, 0.6841390318922365710, 0.7334310489036851566, 0.7741974304450970346, 1.000000000000000000 ),
 .UNSPECIFIED. ) ;
#3596 = CARTESIAN_POINT ( 'NONE',  ( 1.500000000000001332, 10.62499999999999645, 0.000000000000000000 ) ) ;
#3597 = CARTESIAN_POINT ( 'NONE',  ( 3.675669042636310557, 6.342012078834061484, -1.082531754730549967 ) ) ;
#3598 = CARTESIAN_POINT ( 'NONE',  ( -4.516274566683622815, 5.401980094953223066, 1.082531754730549078 ) ) ;
#3599 = CARTESIAN_POINT ( 'NONE',  ( 6.076833508651091620, -1.499762292660647311, 1.499315088411487640 ) ) ;
#3600 = ORIENTED_EDGE ( 'NONE', *, *, #25641, .F. ) ;
#3601 = CARTESIAN_POINT ( 'NONE',  ( 3.874305460179793048, 1.279221729648010175, 1.920377363040247420 ) ) ;
#3603 = ADVANCED_FACE ( 'NONE', ( #77901 ), #61609, .T. ) ;
#3602 = CARTESIAN_POINT ( 'NONE',  ( 4.299235682465595509, -1.708000122724560477, 0.9650500775852040025 ) ) ;
#3604 = CARTESIAN_POINT ( 'NONE',  ( 1.270277045833507312, -0.8771146801004360283, -1.754798696806989078 ) ) ;
#3605 = DIRECTION ( 'NONE',  ( 0.000000000000000000, -1.000000000000000000, 0.000000000000000000 ) ) ;
#3606 = CARTESIAN_POINT ( 'NONE',  ( -9.380315450342122219, 15.46908200564950775, 7.483989756882012401 ) ) ;
#3607 = ORIENTED_EDGE ( 'NONE', *, *, #5122, .F. ) ;
#3608 = CARTESIAN_POINT ( 'NONE',  ( 5.735564631760892595, 0.5807582108038509272, -1.931123567068816493 ) ) ;
#3609 = DIRECTION ( 'NONE',  ( -1.000000000000000000, 0.000000000000000000, -5.551115123125765446E-17 ) ) ;
#3610 = CARTESIAN_POINT ( 'NONE',  ( 2.958077724197702096, -0.6850214551260015439, 2.060201288156039645 ) ) ;
#3611 = FACE_OUTER_BOUND ( 'NONE', #77172, .T. ) ;
#3612 = CARTESIAN_POINT ( 'NONE',  ( 0.6859744409541921328, 2.042103856186634925, -0.5713114342573709648 ) ) ;
#3613 = CARTESIAN_POINT ( 'NONE',  ( -0.7500000000000006661, 2.139583334016155636, -1.299038105676652011 ) ) ;
#3614 = CARTESIAN_POINT ( 'NONE',  ( 8.204655514564224816, 12.72384853363364066, 1.040834085586084257E-14 ) ) ;
#3615 = CARTESIAN_POINT ( 'NONE',  ( 1.347111479062088405E-15, 0.000000000000000000, 11.00000000000000000 ) ) ;
#3616 = CARTESIAN_POINT ( 'NONE',  ( 6.596403382356258227, 6.772441155557838321, -0.1798620802159808241 ) ) ;
#3617 = CARTESIAN_POINT ( 'NONE',  ( 1.862644954548669185, -1.459483730259679257, 1.455164547919563844 ) ) ;
#3619 = CARTESIAN_POINT ( 'NONE',  ( 0.000000000000000000, -1.399999999999998579, 0.000000000000000000 ) ) ;
#3618 = CARTESIAN_POINT ( 'NONE',  ( -8.306341666666730461, 12.84248237775322643, 1.040834085586084257E-14 ) ) ;
#3620 = CARTESIAN_POINT ( 'NONE',  ( 1.364683531249986537, 1.655208333674748955, -0.7879004041258239610 ) ) ;
#3621 = FACE_OUTER_BOUND ( 'NONE', #70263, .T. ) ;
#3622 =( BOUNDED_CURVE ( )  B_SPLINE_CURVE ( 2, ( #210191, #208060, #46661, #58630, #142045, #10921, #27183 ),
 .UNSPECIFIED., .F., .T. ) 
 B_SPLINE_CURVE_WITH_KNOTS ( ( 3, 2, 2, 3 ),
 ( 0.3500000000000000888, 0.3583333333333333925, 0.3666666666666666963, 0.3750000000000000000 ),
 .UNSPECIFIED. ) 
 CURVE ( )  GEOMETRIC_REPRESENTATION_ITEM ( )  RATIONAL_B_SPLINE_CURVE ( ( 0.9999999999999982236, 0.8660254037844404840, 1.000000000000000000, 0.8660254037844387076, 1.000000000000000000, 0.8660254037844387076, 1.000000000000000000 ) ) 
 REPRESENTATION_ITEM ( '' )  );
#3623 = EDGE_CURVE ( 'NONE', #183133, #82411, #22756, .T. ) ;
#3624 = ORIENTED_EDGE ( 'NONE', *, *, #28439, .T. ) ;
#3625 = CARTESIAN_POINT ( 'NONE',  ( 4.969353466749234727, -1.617520173792227567, -1.019718193788564209 ) ) ;
#3626 = CARTESIAN_POINT ( 'NONE',  ( 11.81905481421901705, 9.842643443827320482, 1.592167362352177262 ) ) ;
#3627 = CARTESIAN_POINT ( 'NONE',  ( -9.490344339885973923, 12.09515436799890331, -1.443375672974059665 ) ) ;
#3628 = CARTESIAN_POINT ( 'NONE',  ( 0.2635251908490592876, 0.5682291949154983923, -1.720254828205844966 ) ) ;
#3630 = CARTESIAN_POINT ( 'NONE',  ( 0.8310839537030527691, -1.512174478060366534, -1.176066492228915017 ) ) ;
#3629 = CARTESIAN_POINT ( 'NONE',  ( -6.661184042391488980, -7.215568602681072363, 6.773376348128680391 ) ) ;
#3631 = CARTESIAN_POINT ( 'NONE',  ( 2.154816067267216084, -0.5500195584662926906, -1.995915215819036748 ) ) ;
#3632 = CARTESIAN_POINT ( 'NONE',  ( 1.364683531249986537, 0.4677083336747514530, -0.7879004041258309554 ) ) ;
#3633 = CARTESIAN_POINT ( 'NONE',  ( 0.7429697149608678330, -1.692012040804885098, 1.011587418319284781 ) ) ;
#3634 = CARTESIAN_POINT ( 'NONE',  ( 2.297230901563730665, 1.410920830412419003, 1.158640757216542028 ) ) ;
#3636 = CARTESIAN_POINT ( 'NONE',  ( 5.886377668569586774, 7.162856863344262415, 1.137212067324339104 ) ) ;
#3635 = CARTESIAN_POINT ( 'NONE',  ( 0.01296380302724577452, -0.9916191462571806170, -2.081274906121612034 ) ) ;
#3637 = CARTESIAN_POINT ( 'NONE',  ( -1.201851678989727383E-14, 1.071875000341418138, 1.575800808251672791 ) ) ;
#3638 = CARTESIAN_POINT ( 'NONE',  ( 4.633292856664962933, 0.003200217577232782832, -2.062851381006901352 ) ) ;
#3639 = CARTESIAN_POINT ( 'NONE',  ( -6.093499974338126179, 9.196501505781426999, -1.199719254218440723 ) ) ;
#3640 = CARTESIAN_POINT ( 'NONE',  ( 6.726816770674637347, 10.99970333242910669, -0.7998128361456291469 ) ) ;
#3641 = CARTESIAN_POINT ( 'NONE',  ( 5.366329872910639232, 5.155139694684188534, 1.040834085586084257E-14 ) ) ;
#3642 = CARTESIAN_POINT ( 'NONE',  ( 6.003563092752934871, 5.898578451166879510, 0.7998128361456341429 ) ) ;
#3644 = CARTESIAN_POINT ( 'NONE',  ( 0.7499999999999920064, 4.233333333333352932, 1.299038105676669330 ) ) ;
#3643 = CARTESIAN_POINT ( 'NONE',  ( 5.157299734135989411, -1.777537633589726163, -1.129047594716176217 ) ) ;
#3645 = CARTESIAN_POINT ( 'NONE',  ( 6.004363041306050697, 2.067815565686380364, 0.1054426792976848049 ) ) ;
#3646 = CARTESIAN_POINT ( 'NONE',  ( 0.6823417656249882723, 1.988541667008083991, -1.181850606188749264 ) ) ;
#3647 = CARTESIAN_POINT ( 'NONE',  ( 4.956408742875526130, 0.8222144862577386304, 1.999314050312686275 ) ) ;
#3649 = EDGE_CURVE ( 'NONE', #171443, #25476, #165651, .T. ) ;
#3648 = CARTESIAN_POINT ( 'NONE',  ( 4.512370939326771691, -2.019285345247460839, -0.04732774261236893931 ) ) ;
#3650 = CARTESIAN_POINT ( 'NONE',  ( 6.720655732516648051, 1.999557737031621540, 2.575425662770465252 ) ) ;
#3651 = EDGE_CURVE ( 'NONE', #96370, #115058, #48028, .T. ) ;
#3653 = CARTESIAN_POINT ( 'NONE',  ( 6.507550544879468823, 6.694489845221929691, -0.7216878364870257245 ) ) ;
#3652 = CARTESIAN_POINT ( 'NONE',  ( -1.642778471874998480, -3.551041666188709645, 2.845375778867863303 ) ) ;
#3654 = CARTESIAN_POINT ( 'NONE',  ( -5.108390017298964914, 9.181815130149269422, 0.000000000000000000 ) ) ;
#3655 = CARTESIAN_POINT ( 'NONE',  ( 2.096888995370162156, 1.803417055948232761, 0.9023429676050932491 ) ) ;
#3656 = CARTESIAN_POINT ( 'NONE',  ( -7.316596452869116973, 11.68777962832266049, 0.7998128361456481317 ) ) ;
#3658 = CARTESIAN_POINT ( 'NONE',  ( 6.614806895146394972, -0.1608752592793839531, 2.155998228907447523 ) ) ;
#3657 = CARTESIAN_POINT ( 'NONE',  ( -5.603597561149804562, 5.431951997629870910, 0.7998128361456341429 ) ) ;
#3659 = CARTESIAN_POINT ( 'NONE',  ( -11.89942855770814134, 12.30000000000000071, -0.7000000000000009548 ) ) ;
#3660 = CARTESIAN_POINT ( 'NONE',  ( -11.86687934130374522, 11.10951949616558565, 1.056332641424306606 ) ) ;
#3661 = CARTESIAN_POINT ( 'NONE',  ( 6.720655732516665815, 6.034026441762381232, 2.768628153821062199 ) ) ;
#3663 = CARTESIAN_POINT ( 'NONE',  ( 4.692982559244565088, 1.755779632255444422, 0.9913831279167032440 ) ) ;
#3662 = CARTESIAN_POINT ( 'NONE',  ( -7.578644679914719795, 9.864838098032418401, 1.443375672974090751 ) ) ;
#3664 = CARTESIAN_POINT ( 'NONE',  ( 1.499999999999990896, 5.275000000000022560, 1.214306433183764966E-14 ) ) ;
#3665 = CARTESIAN_POINT ( 'NONE',  ( 0.8907089605301542479, 1.523294409195220966, -0.8092020298176191284 ) ) ;
#3666 = CARTESIAN_POINT ( 'NONE',  ( 6.222266154028957885, 6.224008365980749247, 0.7998128361456352531 ) ) ;
#3668 = CARTESIAN_POINT ( 'NONE',  ( 0.4499999999999747535, 4.000000000000003553, -5.377642775528101993E-14 ) ) ;
#3667 = CARTESIAN_POINT ( 'NONE',  ( 9.110716038703335684, 9.731516254683127087, -0.7216878364870197293 ) ) ;
#3669 = CIRCLE ( 'NONE', #187065, 8.049999999999993605 ) ;
#3670 = CARTESIAN_POINT ( 'NONE',  ( -11.56555315273234719, 8.166926488375429116, 3.210420282871015996 ) ) ;
#3671 = CARTESIAN_POINT ( 'NONE',  ( 5.887941446147332947, -0.8415115861447747259, 1.670666529855535654 ) ) ;
#3672 = CARTESIAN_POINT ( 'NONE',  ( -0.02280469861281903335, -1.799075986276091887, -0.9034098368623093567 ) ) ;
#3673 =( BOUNDED_SURFACE ( )  B_SPLINE_SURFACE ( 1, 2, ( 
 ( #76699, #125547, #9572, #157984, #209883, #127687, #61521, #96181, #109286, #95114, #161163, #26882, #192571, #92985, #12749, #110348, #159030, #176351, #78823, #144944, #210951, #62577, #126608, #79892, #190445, #94051, #11695, #75649, #77769, #10623, #142815, #194713, #60451, #112472, #178481, #42104, #108217, #174241, #25814, #208821, #195790, #183794, #101481, #18075, #14875, #83084, #167551, #149163, #131893, #35403, #47428, #117802, #113543, #179546, #196850, #198953, #65747, #19152, #132948, #48487, #17008, #99361, #214119, #31167, #114605, #82024, #50595, #740, #66806, #148116, #129810, #115655, #97240, #130853, #147059, #181650, #67876, #116720, #80967, #63655, #64710, #213079, #182720, #163294, #32221, #146002, #212012, #200029, #34338, #180596, #98294, #100413, #51681, #166483, #84162, #164356, #15940, #197901, #49531, #165412, #150250, #33276, #1818, #134022, #40776, #151314, #121027, #119939, #169681, #20214, #154512, #86302, #152372, #123178, #70017, #106882, #136133, #37549, #203229, #72161, #88452, #170752, #102549, #171822, #3950, #185915, #22338, #71090, #172908, #205371, #137207, #138270, #186994, #87374, #38625, #153444, #73234, #103629, #202149, #204284, #89527, #53810, #155580, #21269, #168612, #118862, #5016, #54874, #104701, #6093, #189137, #55941, #122094, #139341, #188058, #39687, #105798, #85225, #68953, #23416, #7164, #57006, #135074, #2882, #201087, #52728, #184848, #36476, #12511, #177162, #158778, #156653, #209634, #141507, #206444, #76451, #207516, #26631, #127436, #91673, #190194, #28780, #9321, #191252, #8246, #74330, #59135, #144704, #94863, #24482, #11444, #125294, #109027, #173990, #41852, #124234, #25562, #128503, #107962, #77519, #160917, #159842, #43977, #112231, #90594, #142559, #157726, #60199, #42917, #110096, #208565, #58071, #75395, #46113, #93802, #176107, #140432, #27707, #210715, #175046, #61274, #111162, #92733, #126360, #10374, #192319, #143640, #193406, #62343, #45050, #78582, #194471, #132266, #183105, #85604, #3261, #118176, #48860, #32597, #151692, #116037 ),
 ( #134399, #2190, #148492, #69329, #66123, #17384, #68266, #117104, #86674, #36845, #34714, #184163, #114974, #165799, #102927, #201461, #131231, #35784, #99728, #1133, #198274, #59, #16317, #49916, #20588, #82402, #101860, #135440, #52049, #150629, #4322, #197219, #100785, #182024, #166867, #149547, #200401, #18461, #98672, #33654, #152741, #167928, #19527, #180975, #53105, #168989, #83468, #119238, #185221, #164728, #84539, #67195, #133332, #199336, #50982, #111272, #60308, #203596, #45158, #71465, #125398, #27816, #159954, #126467, #202529, #186293, #93913, #55248, #11558, #137578, #110204, #6468, #77628, #88829, #5388, #192430, #72544, #191363, #10484, #70392, #21633, #138642, #176214, #207622, #121395, #154884, #109142, #175155, #59239, #26741, #43030, #61387, #105083, #187368, #44085, #143750, #38998, #209745, #171121, #153817, #104004, #22715, #87741, #92844, #158888, #177275, #76558, #142668, #127546, #208679, #193517, #28891, #136509, #54178, #94975, #161021, #120318, #37930, #170048, #97109, #29959, #32082, #13687, #597, #165273, #146928, #144814, #197762, #129674, #194576, #64582, #195659, #14746, #115519, #79757, #178351, #16868, #211881, #179414, #210821, #46222, #63522, #65607, #212945, #100271, #213987, #47293, #98170, #180466, #80838, #112339, #113408, #163161, #131757, #15805, #164218, #130723, #62446, #196714, #96045, #31035, #145873, #48355, #149022, #81891, #162098, #128609, #114466, #147977, #49400, #181514, #33143, #198814, #78689, #66663, #99223, #50460, #12616, #82948, #132810, #116579, #182574, #34196, #84012, #102400, #1675, #119785, #153285, #201995, #200937, #22182, #121941, #17928, #53653, #52585, #36322, #101330, #21115, #167411, #19003, #204131, #151168, #187907, #2739, #118713, #69871, #4861, #169535, #37398, #183650, #38475, #85084, #184701, #103473, #152226, #39537, #72009, #3797, #70940, #87221, #137050, #203076, #55784, #68810, #54720, #120869, #134932, #135980, #168468, #186843, #185766, #20066, #104552, #170596, #88298, #154359, #5938, #86155, #166336, #150103, #138122 ) ),
 .UNSPECIFIED., .F., .F., .T. ) 
 B_SPLINE_SURFACE_WITH_KNOTS ( ( 2, 2 ),
 ( 3, 2, 2, 2, 2, 2, 2, 2, 2, 2, 2, 2, 2, 2, 2, 2, 2, 2, 2, 2, 2, 2, 2, 2, 2, 2, 2, 2, 2, 2, 2, 2, 2, 2, 2, 2, 2, 2, 2, 2, 2, 2, 2, 2, 2, 2, 2, 2, 2, 2, 2, 2, 2, 2, 2, 2, 2, 2, 2, 2, 2, 2, 2, 2, 2, 2, 2, 2, 2, 2, 2, 2, 2, 2, 2, 2, 2, 2, 2, 2, 2, 2, 2, 2, 2, 2, 2, 2, 2, 2, 2, 2, 2, 2, 2, 2, 2, 2, 2, 2, 2, 2, 2, 2, 2, 2, 2, 2, 2, 2, 2, 2, 2, 2, 2, 2, 2, 2, 2, 2, 3 ),
 ( 0.000000000000000000, 1.000000000000000000 ),
 ( 0.000000000000000000, 0.008333333333333333218, 0.01666666666666666644, 0.02500000000000000139, 0.03333333333333333287, 0.04166666666666666435, 0.05000000000000000278, 0.05833333333333333426, 0.06666666666666666574, 0.07499999999999999722, 0.08333333333333332871, 0.09166666666666666019, 0.1000000000000000056, 0.1083333333333333370, 0.1166666666666666685, 0.1250000000000000000, 0.1333333333333333315, 0.1416666666666666630, 0.1499999999999999944, 0.1583333333333333259, 0.1666666666666666574, 0.1749999999999999889, 0.1833333333333333204, 0.1916666666666666796, 0.2000000000000000111, 0.2083333333333333426, 0.2166666666666666741, 0.2250000000000000056, 0.2333333333333333370, 0.2416666666666666685, 0.2500000000000000000, 0.2583333333333333592, 0.2666666666666666630, 0.2750000000000000222, 0.2833333333333333259, 0.2916666666666666852, 0.2999999999999999889, 0.3083333333333333481, 0.3166666666666666519, 0.3250000000000000111, 0.3333333333333333148, 0.3416666666666666741, 0.3499999999999999778, 0.3583333333333333370, 0.3666666666666666408, 0.3750000000000000000, 0.3833333333333333592, 0.3916666666666666630, 0.4000000000000000222, 0.4083333333333333259, 0.4166666666666666852, 0.4249999999999999889, 0.4333333333333333481, 0.4416666666666666519, 0.4500000000000000111, 0.4583333333333333148, 0.4666666666666666741, 0.4749999999999999778, 0.4833333333333333370, 0.4916666666666666408, 0.5000000000000000000, 0.5083333333333333037, 0.5166666666666667185, 0.5250000000000000222, 0.5333333333333333259, 0.5416666666666666297, 0.5500000000000000444, 0.5583333333333333481, 0.5666666666666666519, 0.5749999999999999556, 0.5833333333333333703, 0.5916666666666666741, 0.5999999999999999778, 0.6083333333333332815, 0.6166666666666666963, 0.6250000000000000000, 0.6333333333333333037, 0.6416666666666667185, 0.6500000000000000222, 0.6583333333333333259, 0.6666666666666666297, 0.6750000000000000444, 0.6833333333333333481, 0.6916666666666666519, 0.6999999999999999556, 0.7083333333333333703, 0.7166666666666666741, 0.7249999999999999778, 0.7333333333333332815, 0.7416666666666666963, 0.7500000000000000000, 0.7583333333333333037, 0.7666666666666667185, 0.7750000000000000222, 0.7833333333333333259, 0.7916666666666666297, 0.8000000000000000444, 0.8083333333333333481, 0.8166666666666666519, 0.8249999999999999556, 0.8333333333333333703, 0.8416666666666666741, 0.8499999999999999778, 0.8583333333333332815, 0.8666666666666666963, 0.8750000000000000000, 0.8833333333333333037, 0.8916666666666667185, 0.9000000000000000222, 0.9083333333333333259, 0.9166666666666666297, 0.9250000000000000444, 0.9333333333333333481, 0.9416666666666666519, 0.9499999999999999556, 0.9583333333333333703, 0.9666666666666666741, 0.9749999999999999778, 0.9833333333333332815, 0.9916666666666666963, 1.000000000000000000 ),
 .UNSPECIFIED. ) 
 GEOMETRIC_REPRESENTATION_ITEM ( )  RATIONAL_B_SPLINE_SURFACE ( (
 ( 1.000000000000000000, 0.8660254037844387076, 1.000000000000000000, 0.8660254037844387076, 1.000000000000000000, 0.8660254037844387076, 1.000000000000000000, 0.8660254037844387076, 1.000000000000000000, 0.8660254037844387076, 1.000000000000000000, 0.8660254037844387076, 1.000000000000000000, 0.8660254037844387076, 1.000000000000000000, 0.8660254037844387076, 1.000000000000000000, 0.8660254037844387076, 1.000000000000000000, 0.8660254037844387076, 1.000000000000000000, 0.8660254037844387076, 1.000000000000000000, 0.8660254037844387076, 1.000000000000000000, 0.8660254037844387076, 1.000000000000000000, 0.8660254037844387076, 1.000000000000000000, 0.8660254037844387076, 1.000000000000000000, 0.8660254037844387076, 1.000000000000000000, 0.8660254037844387076, 1.000000000000000000, 0.8660254037844387076, 1.000000000000000000, 0.8660254037844387076, 1.000000000000000000, 0.8660254037844387076, 1.000000000000000000, 0.8660254037844387076, 1.000000000000000000, 0.8660254037844387076, 1.000000000000000000, 0.8660254037844387076, 1.000000000000000000, 0.8660254037844387076, 1.000000000000000000, 0.8660254037844387076, 1.000000000000000000, 0.8660254037844387076, 1.000000000000000000, 0.8660254037844387076, 1.000000000000000000, 0.8660254037844387076, 1.000000000000000000, 0.8660254037844387076, 1.000000000000000000, 0.8660254037844387076, 1.000000000000000000, 0.8660254037844387076, 1.000000000000000000, 0.8660254037844387076, 1.000000000000000000, 0.8660254037844387076, 1.000000000000000000, 0.8660254037844387076, 1.000000000000000000, 0.8660254037844387076, 1.000000000000000000, 0.8660254037844387076, 1.000000000000000000, 0.8660254037844387076, 1.000000000000000000, 0.8660254037844387076, 1.000000000000000000, 0.8660254037844387076, 1.000000000000000000, 0.8660254037844387076, 1.000000000000000000, 0.8660254037844387076, 1.000000000000000000, 0.8660254037844387076, 1.000000000000000000, 0.8660254037844387076, 1.000000000000000000, 0.8660254037844387076, 1.000000000000000000, 0.8660254037844387076, 1.000000000000000000, 0.8660254037844387076, 1.000000000000000000, 0.8660254037844387076, 1.000000000000000000, 0.8660254037844387076, 1.000000000000000000, 0.8660254037844387076, 1.000000000000000000, 0.8660254037844387076, 1.000000000000000000, 0.8660254037844387076, 1.000000000000000000, 0.8660254037844387076, 1.000000000000000000, 0.8660254037844387076, 1.000000000000000000, 0.8660254037844387076, 1.000000000000000000, 0.8660254037844387076, 1.000000000000000000, 0.8660254037844387076, 1.000000000000000000, 0.8660254037844387076, 1.000000000000000000, 0.8660254037844387076, 1.000000000000000000, 0.8660254037844387076, 1.000000000000000000, 0.8660254037844387076, 1.000000000000000000, 0.8660254037844387076, 1.000000000000000000, 0.8660254037844387076, 1.000000000000000000, 0.8660254037844387076, 1.000000000000000000, 0.8660254037844387076, 1.000000000000000000, 0.8660254037844387076, 1.000000000000000000, 0.8660254037844387076, 1.000000000000000000, 0.8660254037844387076, 1.000000000000000000, 0.8660254037844387076, 1.000000000000000000, 0.8660254037844387076, 1.000000000000000000, 0.8660254037844387076, 1.000000000000000000, 0.8660254037844387076, 1.000000000000000000, 0.8660254037844387076, 1.000000000000000000, 0.8660254037844387076, 1.000000000000000000, 0.8660254037844387076, 1.000000000000000000, 0.8660254037844387076, 1.000000000000000000, 0.8660254037844387076, 1.000000000000000000, 0.8660254037844387076, 1.000000000000000000, 0.8660254037844387076, 1.000000000000000000, 0.8660254037844387076, 1.000000000000000000, 0.8660254037844387076, 1.000000000000000000, 0.8660254037844387076, 1.000000000000000000, 0.8660254037844387076, 1.000000000000000000, 0.8660254037844387076, 1.000000000000000000, 0.8660254037844387076, 1.000000000000000000, 0.8660254037844387076, 1.000000000000000000, 0.8660254037844387076, 1.000000000000000000, 0.8660254037844387076, 1.000000000000000000, 0.8660254037844387076, 1.000000000000000000, 0.8660254037844387076, 1.000000000000000000, 0.8660254037844387076, 1.000000000000000000, 0.8660254037844387076, 1.000000000000000000, 0.8660254037844387076, 1.000000000000000000, 0.8660254037844387076, 1.000000000000000000, 0.8660254037844387076, 1.000000000000000000, 0.8660254037844387076, 1.000000000000000000, 0.8660254037844387076, 1.000000000000000000, 0.8660254037844387076, 1.000000000000000000, 0.8660254037844387076, 1.000000000000000000, 0.8660254037844387076, 1.000000000000000000, 0.8660254037844387076, 1.000000000000000000, 0.8660254037844387076, 1.000000000000000000, 0.8660254037844387076, 1.000000000000000000, 0.8660254037844387076, 1.000000000000000000, 0.8660254037844387076, 1.000000000000000000, 0.8660254037844387076, 1.000000000000000000, 0.8660254037844387076, 1.000000000000000000, 0.8660254037844387076, 1.000000000000000000, 0.8660254037844387076, 1.000000000000000000, 0.8660254037844387076, 1.000000000000000000, 0.8660254037844387076, 1.000000000000000000, 0.8660254037844387076, 1.000000000000000000, 0.8660254037844387076, 1.000000000000000000, 0.8660254037844387076, 1.000000000000000000, 0.8660254037844387076, 1.000000000000000000, 0.8660254037844387076, 1.000000000000000000, 0.8660254037844387076, 1.000000000000000000, 0.8660254037844387076, 1.000000000000000000, 0.8660254037844387076, 1.000000000000000000, 0.8660254037844387076, 1.000000000000000000, 0.8660254037844387076, 1.000000000000000000),
 ( 1.000000000000000000, 0.8660254037844387076, 1.000000000000000000, 0.8660254037844387076, 1.000000000000000000, 0.8660254037844387076, 1.000000000000000000, 0.8660254037844387076, 1.000000000000000000, 0.8660254037844387076, 1.000000000000000000, 0.8660254037844387076, 1.000000000000000000, 0.8660254037844387076, 1.000000000000000000, 0.8660254037844387076, 1.000000000000000000, 0.8660254037844387076, 1.000000000000000000, 0.8660254037844387076, 1.000000000000000000, 0.8660254037844387076, 1.000000000000000000, 0.8660254037844387076, 1.000000000000000000, 0.8660254037844387076, 1.000000000000000000, 0.8660254037844387076, 1.000000000000000000, 0.8660254037844387076, 1.000000000000000000, 0.8660254037844387076, 1.000000000000000000, 0.8660254037844387076, 1.000000000000000000, 0.8660254037844387076, 1.000000000000000000, 0.8660254037844387076, 1.000000000000000000, 0.8660254037844387076, 1.000000000000000000, 0.8660254037844387076, 1.000000000000000000, 0.8660254037844387076, 1.000000000000000000, 0.8660254037844387076, 1.000000000000000000, 0.8660254037844387076, 1.000000000000000000, 0.8660254037844387076, 1.000000000000000000, 0.8660254037844387076, 1.000000000000000000, 0.8660254037844387076, 1.000000000000000000, 0.8660254037844387076, 1.000000000000000000, 0.8660254037844387076, 1.000000000000000000, 0.8660254037844387076, 1.000000000000000000, 0.8660254037844387076, 1.000000000000000000, 0.8660254037844387076, 1.000000000000000000, 0.8660254037844387076, 1.000000000000000000, 0.8660254037844387076, 1.000000000000000000, 0.8660254037844387076, 1.000000000000000000, 0.8660254037844387076, 1.000000000000000000, 0.8660254037844387076, 1.000000000000000000, 0.8660254037844387076, 1.000000000000000000, 0.8660254037844387076, 1.000000000000000000, 0.8660254037844387076, 1.000000000000000000, 0.8660254037844387076, 1.000000000000000000, 0.8660254037844387076, 1.000000000000000000, 0.8660254037844387076, 1.000000000000000000, 0.8660254037844387076, 1.000000000000000000, 0.8660254037844387076, 1.000000000000000000, 0.8660254037844387076, 1.000000000000000000, 0.8660254037844387076, 1.000000000000000000, 0.8660254037844387076, 1.000000000000000000, 0.8660254037844387076, 1.000000000000000000, 0.8660254037844387076, 1.000000000000000000, 0.8660254037844387076, 1.000000000000000000, 0.8660254037844387076, 1.000000000000000000, 0.8660254037844387076, 1.000000000000000000, 0.8660254037844387076, 1.000000000000000000, 0.8660254037844387076, 1.000000000000000000, 0.8660254037844387076, 1.000000000000000000, 0.8660254037844387076, 1.000000000000000000, 0.8660254037844387076, 1.000000000000000000, 0.8660254037844387076, 1.000000000000000000, 0.8660254037844387076, 1.000000000000000000, 0.8660254037844387076, 1.000000000000000000, 0.8660254037844387076, 1.000000000000000000, 0.8660254037844387076, 1.000000000000000000, 0.8660254037844387076, 1.000000000000000000, 0.8660254037844387076, 1.000000000000000000, 0.8660254037844387076, 1.000000000000000000, 0.8660254037844387076, 1.000000000000000000, 0.8660254037844387076, 1.000000000000000000, 0.8660254037844387076, 1.000000000000000000, 0.8660254037844387076, 1.000000000000000000, 0.8660254037844387076, 1.000000000000000000, 0.8660254037844387076, 1.000000000000000000, 0.8660254037844387076, 1.000000000000000000, 0.8660254037844387076, 1.000000000000000000, 0.8660254037844387076, 1.000000000000000000, 0.8660254037844387076, 1.000000000000000000, 0.8660254037844387076, 1.000000000000000000, 0.8660254037844387076, 1.000000000000000000, 0.8660254037844387076, 1.000000000000000000, 0.8660254037844387076, 1.000000000000000000, 0.8660254037844387076, 1.000000000000000000, 0.8660254037844387076, 1.000000000000000000, 0.8660254037844387076, 1.000000000000000000, 0.8660254037844387076, 1.000000000000000000, 0.8660254037844387076, 1.000000000000000000, 0.8660254037844387076, 1.000000000000000000, 0.8660254037844387076, 1.000000000000000000, 0.8660254037844387076, 1.000000000000000000, 0.8660254037844387076, 1.000000000000000000, 0.8660254037844387076, 1.000000000000000000, 0.8660254037844387076, 1.000000000000000000, 0.8660254037844387076, 1.000000000000000000, 0.8660254037844387076, 1.000000000000000000, 0.8660254037844387076, 1.000000000000000000, 0.8660254037844387076, 1.000000000000000000, 0.8660254037844387076, 1.000000000000000000, 0.8660254037844387076, 1.000000000000000000, 0.8660254037844387076, 1.000000000000000000, 0.8660254037844387076, 1.000000000000000000, 0.8660254037844387076, 1.000000000000000000, 0.8660254037844387076, 1.000000000000000000, 0.8660254037844387076, 1.000000000000000000, 0.8660254037844387076, 1.000000000000000000, 0.8660254037844387076, 1.000000000000000000, 0.8660254037844387076, 1.000000000000000000, 0.8660254037844387076, 1.000000000000000000, 0.8660254037844387076, 1.000000000000000000, 0.8660254037844387076, 1.000000000000000000, 0.8660254037844387076, 1.000000000000000000, 0.8660254037844387076, 1.000000000000000000, 0.8660254037844387076, 1.000000000000000000, 0.8660254037844387076, 1.000000000000000000, 0.8660254037844387076, 1.000000000000000000, 0.8660254037844387076, 1.000000000000000000, 0.8660254037844387076, 1.000000000000000000, 0.8660254037844387076, 1.000000000000000000, 0.8660254037844387076, 1.000000000000000000, 0.8660254037844387076, 1.000000000000000000, 0.8660254037844387076, 1.000000000000000000, 0.8660254037844387076, 1.000000000000000000) ) ) 
 REPRESENTATION_ITEM ( '' )  SURFACE ( )  );
#3674 = CARTESIAN_POINT ( 'NONE',  ( -7.065207446052822249, 7.415365906582643163, -0.7216878364870338292 ) ) ;
#3675 = ORIENTED_EDGE ( 'NONE', *, *, #198470, .F. ) ;
#3676 = CARTESIAN_POINT ( 'NONE',  ( 0.1226730236999207246, 0.3474926252081366185, 1.986097365194151809 ) ) ;
#3677 = CARTESIAN_POINT ( 'NONE',  ( 1.054613590283080660, 0.3547985653672180439, 1.776302104178028252 ) ) ;
#3678 = CARTESIAN_POINT ( 'NONE',  ( 5.338878628731272613, 9.450718510153643948, -0.7998128361456481317 ) ) ;
#3679 = CARTESIAN_POINT ( 'NONE',  ( 2.580963302752299349, -0.4788041664876945269, 0.000000000000000000 ) ) ;
#3680 = EDGE_CURVE ( 'NONE', #71477, #169163, #189478, .T. ) ;
#3681 = PRESENTATION_LAYER_ASSIGNMENT (  '', '', ( #190472 ) ) ;
#3682 = CARTESIAN_POINT ( 'NONE',  ( 8.148087131688683371, 10.52918762510205042, -1.443375672974063439 ) ) ;
#3683 = CARTESIAN_POINT ( 'NONE',  ( 7.949158136313996259, 8.168439335321471262, 1.040834085586084257E-14 ) ) ;
#3685 = CARTESIAN_POINT ( 'NONE',  ( 0.3213152726999657927, -1.356817153130492004, -1.352679412961822925 ) ) ;
#3684 = CARTESIAN_POINT ( 'NONE',  ( -4.205000198532790279, 8.057583998263570635, 0.7998128361456341429 ) ) ;
#3686 = DIRECTION ( 'NONE',  ( 0.000000000000000000, 0.000000000000000000, -1.000000000000000000 ) ) ;
#3687 = CARTESIAN_POINT ( 'NONE',  ( 5.572037945092146671, 8.484166121707415797, -1.082531754730543971 ) ) ;
#3688 = CARTESIAN_POINT ( 'NONE',  ( 1.364683531249986537, -0.5322916663252452718, -0.7879004041258309554 ) ) ;
#3690 = ORIENTED_EDGE ( 'NONE', *, *, #95199, .F. ) ;
#3689 = CARTESIAN_POINT ( 'NONE',  ( 2.901081683644319842, 5.368050483351580304, 1.082531754730548412 ) ) ;
#3691 = CARTESIAN_POINT ( 'NONE',  ( -10.63367255181986160, 11.30037282007833532, 1.040834085586084257E-14 ) ) ;
#3692 = CARTESIAN_POINT ( 'NONE',  ( 3.889662759143839299, 1.564074849111227516, 1.492423382767386508 ) ) ;
#3693 = CARTESIAN_POINT ( 'NONE',  ( -6.116136693540540570, 10.14959355252370266, 0.000000000000000000 ) ) ;
#3694 = CARTESIAN_POINT ( 'NONE',  ( 5.045042558060919724, 8.899983727797476263, -0.7216878364870458196 ) ) ;
#3695 = CARTESIAN_POINT ( 'NONE',  ( 0.4398875993102538962, -2.011672884243600024, 0.6710486789910232730 ) ) ;
#3696 = CARTESIAN_POINT ( 'NONE',  ( -0.6125000000000037081, 2.458333333333319271, -1.060881119635955327 ) ) ;
#3697 = CARTESIAN_POINT ( 'NONE',  ( 2.091034261367350933, 1.717025232345986252, -0.9683794122406997884 ) ) ;
#3698 = CARTESIAN_POINT ( 'NONE',  ( 4.974826827724895928, -1.381046924789817831, 1.323090558688621909 ) ) ;
#3699 = VERTEX_POINT ( 'NONE', #161302 ) ;
#3700 = CARTESIAN_POINT ( 'NONE',  ( 11.92619526913699879, 13.39999999999998259, 1.328859060402684644 ) ) ;
#3701 = CARTESIAN_POINT ( 'NONE',  ( 6.443809999611881167, 1.357174585993505378, 1.427557633841854967 ) ) ;
#3702 = CARTESIAN_POINT ( 'NONE',  ( 0.8494333778440340543, 1.939759575794866242, -0.09477157414044742878 ) ) ;
#3703 = ORIENTED_EDGE ( 'NONE', *, *, #93584, .T. ) ;
#3704 = CARTESIAN_POINT ( 'NONE',  ( -3.959863383643135393, 6.777535159962392086, 1.199719254218452935 ) ) ;
#3705 = CARTESIAN_POINT ( 'NONE',  ( -3.526002468005825286, 6.271364091718859335, -1.199719254218450271 ) ) ;
#3707 = CARTESIAN_POINT ( 'NONE',  ( 6.658462837642799670, 6.940830530104329377, 0.7216878364870328300 ) ) ;
#3706 = CARTESIAN_POINT ( 'NONE',  ( 8.145751363712157911, 8.397798100619326078, -0.7998128361456281477 ) ) ;
#3709 = ORIENTED_EDGE ( 'NONE', *, *, #84508, .T. ) ;
#3708 = CARTESIAN_POINT ( 'NONE',  ( 5.145129553670328981, 0.1446803459003667691, 1.906877450533929874 ) ) ;
#3710 = CARTESIAN_POINT ( 'NONE',  ( 2.221956617217385244, -2.140583525707707935, 0.5359638216213060691 ) ) ;
#3711 = CARTESIAN_POINT ( 'NONE',  ( 0.000000000000000000, 13.24045051524828231, 0.000000000000000000 ) ) ;
#3712 = CARTESIAN_POINT ( 'NONE',  ( 0.6274217273865910771, -0.2802014979648696502, 1.891502685196179812 ) ) ;
#3713 = CARTESIAN_POINT ( 'NONE',  ( -0.02338929933909470252, 5.726375320706490690, -2.305055744220934066 ) ) ;
#3715 = CARTESIAN_POINT ( 'NONE',  ( -6.257301848505791853, 6.998106085372876706, 0.9978569239010106617 ) ) ;
#3714 =( GEOMETRIC_REPRESENTATION_CONTEXT ( 3 ) GLOBAL_UNCERTAINTY_ASSIGNED_CONTEXT ( ( #180394 ) ) GLOBAL_UNIT_ASSIGNED_CONTEXT ( ( #122217, #57124, #138389 ) ) REPRESENTATION_CONTEXT ( 'NONE', 'WORKASPACE' ) );
#3716 = CARTESIAN_POINT ( 'NONE',  ( -6.484567079770451770, -6.583980363594983842, -7.100579091573043122 ) ) ;
#3717 = CARTESIAN_POINT ( 'NONE',  ( 3.191909353267761151, -1.388477207968623839, -1.535938721777901472 ) ) ;
#3718 = CARTESIAN_POINT ( 'NONE',  ( -5.331380718671772101, 7.243030143248949670, -1.599625672291256295 ) ) ;
#3719 = CIRCLE ( 'NONE', #173397, 1.500000000000000222 ) ;
#3720 = CARTESIAN_POINT ( 'NONE',  ( -4.603423314590644466, 8.384863137925270493, -0.01591256823598764802 ) ) ;
#3722 = CARTESIAN_POINT ( 'NONE',  ( 0.2159880523044250267, -2.119658899406823505, 0.4233941889316418239 ) ) ;
#3721 = CARTESIAN_POINT ( 'NONE',  ( -4.334856428067329404, 6.080418470877079429, -1.599625672291256295 ) ) ;
#3723 = CARTESIAN_POINT ( 'NONE',  ( 2.999763140970078901, -2.188934734890151113, 0.1099877568606702771 ) ) ;
#3724 = AXIS2_PLACEMENT_3D ( 'NONE', #115620, #133988, #166450 ) ;
#3725 = CARTESIAN_POINT ( 'NONE',  ( -11.99998504853427583, 9.073077996143771529, -0.6178450063080842547 ) ) ;
#3726 = CARTESIAN_POINT ( 'NONE',  ( 3.607878275012313285, 6.262922849939428716, 1.082531754730549078 ) ) ;
#3727 = CARTESIAN_POINT ( 'NONE',  ( 1.499999999999993117, 12.85416666666666785, 0.8660254037844408170 ) ) ;
#3728 = CARTESIAN_POINT ( 'NONE',  ( 1.364683531249997417, 13.29687500034139980, 2.602085213965210642E-15 ) ) ;
#3729 = CARTESIAN_POINT ( 'NONE',  ( -4.468294144155606773, 7.370704380560280100, 1.199719254218452935 ) ) ;
#3730 = CARTESIAN_POINT ( 'NONE',  ( 5.854130254062820171, 0.1179724184225266898, -1.730206517700397795 ) ) ;
#3731 = CARTESIAN_POINT ( 'NONE',  ( -3.090368948911150770, 5.692848642783215674, 1.199719254218462483 ) ) ;
#3732 = CARTESIAN_POINT ( 'NONE',  ( 3.239188805615275335, -0.1476314317495740769, -2.065021578984991724 ) ) ;
#3733 = CARTESIAN_POINT ( 'NONE',  ( 4.148151592129151410, 0.9998098737230370903, 1.866312969332243998 ) ) ;
#3734 = CARTESIAN_POINT ( 'NONE',  ( 5.937581207780954884, 9.014596278131406848, -1.199719254218440723 ) ) ;
#3735 = CARTESIAN_POINT ( 'NONE',  ( 0.6823417656249899377, 4.926041667008086655, -1.181850606188754593 ) ) ;
#3736 = CARTESIAN_POINT ( 'NONE',  ( 3.133609412646401360, 1.871568317120005265, -0.6134489921753321084 ) ) ;
#3737 = CARTESIAN_POINT ( 'NONE',  ( 0.7383556378116812313, 1.137082172773289379, -1.537495029474859276 ) ) ;
#3738 = CARTESIAN_POINT ( 'NONE',  ( 4.839906306838932970, 2.285852466752227752, 0.1720476854494106811 ) ) ;
#3739 = CARTESIAN_POINT ( 'NONE',  ( 3.475057130574196407, 0.04366187338752242769, -1.825333387291371512 ) ) ;
#3740 = CARTESIAN_POINT ( 'NONE',  ( 3.528865121306874464, 7.339036084825155015, -0.7998128361456362523 ) ) ;
#3741 = CARTESIAN_POINT ( 'NONE',  ( 4.812781342726850653, 8.558735966582574406, 0.7216878364870438212 ) ) ;
#3742 = CARTESIAN_POINT ( 'NONE',  ( -5.696397096036042385, 9.797547045350714967, -0.7998128361456231517 ) ) ;
#3743 = CARTESIAN_POINT ( 'NONE',  ( 4.095951438411546519, 1.318107682886668242, 1.521754241968393373 ) ) ;
#3744 = CARTESIAN_POINT ( 'NONE',  ( 2.817183829107517745, -1.704460984269993817, -0.9711623693852902139 ) ) ;
#3745 = CARTESIAN_POINT ( 'NONE',  ( -8.681298431451969222, 9.022603012982438386, 1.040834085586084257E-14 ) ) ;
#3746 = CARTESIAN_POINT ( 'NONE',  ( -4.900382456335551140, 7.804531068111707270, 1.199719254218464037 ) ) ;
#3747 = CARTESIAN_POINT ( 'NONE',  ( 0.1751657365761547791, 2.016170943927285908, -2.458682602970231112 ) ) ;
#3750 = CARTESIAN_POINT ( 'NONE',  ( 5.629715507205930614, -1.125428185119830005, -1.365942169508828741 ) ) ;
#3749 = CARTESIAN_POINT ( 'NONE',  ( 6.650343161644081569, -1.616936162011050948, 1.324992778059615128 ) ) ;
#3748 = B_SPLINE_CURVE_WITH_KNOTS ( 'NONE', 3,
 ( #3480, #53326, #137797, #55461 ),
 .UNSPECIFIED., .F., .F.,
 ( 4, 4 ),
 ( 0.000000000000000000, 0.0007855215049759376551 ),
 .UNSPECIFIED. ) ;
#3751 = CARTESIAN_POINT ( 'NONE',  ( 10.94526678918447971, -5.600264386821002915, -0.03132844593992607785 ) ) ;
#3752 = CARTESIAN_POINT ( 'NONE',  ( 1.658417429842372393, -1.548019161032044844, 1.551412955586493947 ) ) ;
#3753 = CARTESIAN_POINT ( 'NONE',  ( 6.158121301954061266, -1.225565299391921936, 1.235896697784558906 ) ) ;
#3754 = CARTESIAN_POINT ( 'NONE',  ( 8.260995669428309540, 8.532249790621511565, 0.7998128361456481317 ) ) ;
#3755 = CARTESIAN_POINT ( 'NONE',  ( 0.08204731311520391257, -1.671590265245853413, -0.4250796685295650246 ) ) ;
#3756 = CARTESIAN_POINT ( 'NONE',  ( 0.5096300131263042932, 2.292432092913086361, 0.1664806320332279099 ) ) ;
#3757 = CARTESIAN_POINT ( 'NONE',  ( 0.7147126110796617748, 2.027027023440019171, 0.8336157706642086662 ) ) ;
#3758 = CARTESIAN_POINT ( 'NONE',  ( 2.948105999307056635, 0.7938017206191756436, -2.059354589195587337 ) ) ;
#3759 = CARTESIAN_POINT ( 'NONE',  ( 6.456263137377813877, -1.236968576560824040, 1.593241027169020052 ) ) ;
#3760 = CARTESIAN_POINT ( 'NONE',  ( 0.3390589225593713674, -2.105617620008819468, -0.5285623031292383533 ) ) ;
#3761 = CARTESIAN_POINT ( 'NONE',  ( 0.000000000000000000, 2.999999999999999112, 10.25000000000000000 ) ) ;
#3762 = CARTESIAN_POINT ( 'NONE',  ( 1.306030339497979531, -1.181222338749428280, -1.757047197724722620 ) ) ;
#3763 = CARTESIAN_POINT ( 'NONE',  ( 6.620655732516645742, 7.051964633898824886, 2.771890290588132189 ) ) ;
#3764 = CARTESIAN_POINT ( 'NONE',  ( 5.420897863522853299, 1.779935589243306859, 0.7372156234431108679 ) ) ;
#3765 = ORIENTED_EDGE ( 'NONE', *, *, #142604, .T. ) ;
#3767 = CARTESIAN_POINT ( 'NONE',  ( -1.500000000000011324, 5.420833333333356485, 0.8660254037844403729 ) ) ;
#3766 = CARTESIAN_POINT ( 'NONE',  ( 1.822231264363738834, 1.315867814366477484, -1.876927872033665956 ) ) ;
#3768 = CARTESIAN_POINT ( 'NONE',  ( 4.681643115420508039, 4.356338477612361260, 0.7998128361456341429 ) ) ;
#3769 = CARTESIAN_POINT ( 'NONE',  ( 4.482942347612929979, 8.381849838857084123, 1.040834085586084257E-14 ) ) ;
#3770 = ADVANCED_FACE ( 'NONE', ( #43300, #210018 ), #44358, .F. ) ;
#3771 = CARTESIAN_POINT ( 'NONE',  ( 3.317226741293349157, 1.750174726733638497, -1.367746370967915626 ) ) ;
#3772 = CARTESIAN_POINT ( 'NONE',  ( -7.782016984564068096, 10.10210578678999482, 1.443375672974090751 ) ) ;
#3773 = CARTESIAN_POINT ( 'NONE',  ( 5.666945020832170776, 7.634521829102760115, 1.443375672974062551 ) ) ;
#3774 = EDGE_CURVE ( 'NONE', #12777, #158047, #212151, .T. ) ;
#3775 = CARTESIAN_POINT ( 'NONE',  ( -8.148087131688692253, 9.568818410800712826, -1.082531754730543083 ) ) ;
#3776 = CIRCLE ( 'NONE', #107649, 0.07999999999999994615 ) ;
#3777 = CARTESIAN_POINT ( 'NONE',  ( 5.614485009834906393, 6.683225611963085733, -1.082531754730548412 ) ) ;
#3778 = CARTESIAN_POINT ( 'NONE',  ( 1.582657950916711131, -0.6767122143778031562, 1.899619169727875700 ) ) ;
#3780 = CARTESIAN_POINT ( 'NONE',  ( 1.569262014403381755, 1.817060349070098724, 0.9760215062899217919 ) ) ;
#3779 = CARTESIAN_POINT ( 'NONE',  ( 6.753933077901968396, 11.03133902419432566, 0.7998128361456462443 ) ) ;
#3781 = DIRECTION ( 'NONE',  ( 5.551115123125766062E-17, 0.000000000000000000, -1.000000000000000000 ) ) ;
#3782 = CARTESIAN_POINT ( 'NONE',  ( 5.763624699140868834, 7.817591130454727200, -1.443375672974078761 ) ) ;
#3783 = CARTESIAN_POINT ( 'NONE',  ( 6.603062865972897377, -0.3679811349713958957, 1.707173594542527040 ) ) ;
#3784 = CARTESIAN_POINT ( 'NONE',  ( 1.364683531249988535, 2.863541667008082658, 0.7879004041258500513 ) ) ;
#3785 = CARTESIAN_POINT ( 'NONE',  ( 2.319294515261476342, -1.717818424975267932, 0.4250260156472511208 ) ) ;
#3786 = CARTESIAN_POINT ( 'NONE',  ( 1.406875202279284753, -1.122500148236497575, -1.674886495921081631 ) ) ;
#3787 = CARTESIAN_POINT ( 'NONE',  ( 0.02850758872123548837, -1.683968158181762043, 0.7450552726024004535 ) ) ;
#3788 = CARTESIAN_POINT ( 'NONE',  ( 4.880587636231574322, -0.2790779774165750293, -2.275280792031343147 ) ) ;
#3789 = CARTESIAN_POINT ( 'NONE',  ( 3.538839456958355889, -1.395042877683351890, -1.201619466480362108 ) ) ;
#3790 = CARTESIAN_POINT ( 'NONE',  ( 8.880754312151170282, 10.31963377138658089, 1.199719254218453823 ) ) ;
#3792 = EDGE_CURVE ( 'NONE', #191954, #56186, #148063, .T. ) ;
#3791 = SHAPE_REPRESENTATION_RELATIONSHIP ( 'NONE' , 'NONE' ,  #211717, #174158 ) ;
#3793 = CARTESIAN_POINT ( 'NONE',  ( 4.260648785556298890, -1.352668379831567069, 1.226179085325199258 ) ) ;
#3794 = CARTESIAN_POINT ( 'NONE',  ( 4.658827374183164949, 1.163267680695536876, 1.646840100852072997 ) ) ;
#3795 = CARTESIAN_POINT ( 'NONE',  ( -7.991641480251377772, 11.41099992934688956, 1.199719254218453823 ) ) ;
#3797 = CARTESIAN_POINT ( 'NONE',  ( -5.772739544368596043, 9.956889578397179363, -0.7998128361456362523 ) ) ;
#3796 = CARTESIAN_POINT ( 'NONE',  ( 3.749113412367131914, -1.851274732041636950, 1.300436299091920045 ) ) ;
#3798 = CARTESIAN_POINT ( 'NONE',  ( 6.053767517140953736, 0.6149031373867475114, -2.014179596626505919 ) ) ;
#3799 = CARTESIAN_POINT ( 'NONE',  ( 1.500000000000001332, 4.285416667349482900, 0.8660254037844450359 ) ) ;
#3800 = CARTESIAN_POINT ( 'NONE',  ( 3.895033709675084221, 0.3008086390649654662, 2.048262060622765279 ) ) ;
#3801 = CARTESIAN_POINT ( 'NONE',  ( 8.516493047678546091, 13.08765898893368629, -0.7998128361456352531 ) ) ;
#3802 = CARTESIAN_POINT ( 'NONE',  ( 1.360316468749957597, 1.776041667008106506, 0.7853790794158801436 ) ) ;
#3803 = APPLICATION_PROTOCOL_DEFINITION ( 'draft international standard', 'automotive_design', 1998, #198672 ) ;
#3805 = CARTESIAN_POINT ( 'NONE',  ( 2.525899207762692722, -1.109253551102797664, -1.574925972939792418 ) ) ;
#3804 = CARTESIAN_POINT ( 'NONE',  ( -10.17947440576205054, 10.77047498301088346, 0.7998128361456462443 ) ) ;
#3806 = UNCERTAINTY_MEASURE_WITH_UNIT (LENGTH_MEASURE( 1.000000000000000082E-05 ), #124958, 'distance_accuracy_value', 'NONE');
#3807 = CARTESIAN_POINT ( 'NONE',  ( -2.993318053567081360, 6.714231172462041819, 0.000000000000000000 ) ) ;
#3808 = CARTESIAN_POINT ( 'NONE',  ( 0.2737963954951051493, -1.932246063674218473, 0.3805649573235761474 ) ) ;
#3809 = CARTESIAN_POINT ( 'NONE',  ( 3.729901657090938460, 7.365652676665848553, 0.7216878364870257245 ) ) ;
#3810 = CARTESIAN_POINT ( 'NONE',  ( 5.740253418993177981, 6.070215967746060315, 0.6401420356763661834 ) ) ;
#3811 = CARTESIAN_POINT ( 'NONE',  ( -0.7500000000000179856, 9.572916667349467446, 1.299038105676658228 ) ) ;
#3812 = CARTESIAN_POINT ( 'NONE',  ( -10.48008955368359629, 11.32911868882677986, 1.040834085586084257E-14 ) ) ;
#3813 = CARTESIAN_POINT ( 'NONE',  ( 0.3697636260225238836, -1.880949819439242443, -1.181558314010826116 ) ) ;
#3814 = CARTESIAN_POINT ( 'NONE',  ( 3.434694453818935678, 2.054221006159732354, 0.4631738978765443382 ) ) ;
#3816 = CARTESIAN_POINT ( 'NONE',  ( -7.435720902452096936, 7.639705572474380091, 0.000000000000000000 ) ) ;
#3815 = VECTOR ( 'NONE', #3943, 1000.000000000000000 ) ;
#3817 = CARTESIAN_POINT ( 'NONE',  ( 6.642605195691581699, 9.837124264027149678, 1.199719254218462483 ) ) ;
#3818 = CARTESIAN_POINT ( 'NONE',  ( 0.4318009167844725771, 1.066696818439222039, 1.524822319796947934 ) ) ;
#3819 = CARTESIAN_POINT ( 'NONE',  ( 5.425234023762710578, 9.481190127698507553, -0.7998128361456291469 ) ) ;
#3820 = CARTESIAN_POINT ( 'NONE',  ( 5.847644326195776010, 5.716673223516856694, -0.7998128361456281477 ) ) ;
#3821 = CARTESIAN_POINT ( 'NONE',  ( -5.966997003790217136, 9.975597247814986801, -0.7216878364870338292 ) ) ;
#3822 = CARTESIAN_POINT ( 'NONE',  ( -8.514157279702033065, 9.995900250149611921, -1.082531754730543971 ) ) ;
#3823 = CARTESIAN_POINT ( 'NONE',  ( 1.353939357992512305, -1.539690173578952770, -1.458446627980537480 ) ) ;
#3824 = CARTESIAN_POINT ( 'NONE',  ( -6.587282531393266360, 8.778525268082516320, 1.599625672291269396 ) ) ;
#3826 = CARTESIAN_POINT ( 'NONE',  ( 4.685966490639408732, -1.205361723144786845, -1.547842780461285761 ) ) ;
#3825 = CARTESIAN_POINT ( 'NONE',  ( 1.224999999999947020, 0.8958333333333401427, -0.7072540797573197979 ) ) ;
#3827 = CARTESIAN_POINT ( 'NONE',  ( 3.661132068870280420, -1.905464569931826446, -1.020879743040298271 ) ) ;
#3828 = CARTESIAN_POINT ( 'NONE',  ( 1.364538772237647413, 0.1349417713633893900, -1.836341338755695718 ) ) ;
#3830 = CARTESIAN_POINT ( 'NONE',  ( -4.397708481796120950, 7.154691356138512148, -1.067048916732843411 ) ) ;
#3829 = CARTESIAN_POINT ( 'NONE',  ( 0.08058608058607032165, -5.907420853759267843, -10.99970480893079916 ) ) ;
#3831 = CARTESIAN_POINT ( 'NONE',  ( 4.980260712887213614, -0.2176769249225460612, -1.726585916463187376 ) ) ;
#3832 = CARTESIAN_POINT ( 'NONE',  ( 0.7124089920921370389, 15.00000000000000711, -12.66466791154696558 ) ) ;
#3833 = CARTESIAN_POINT ( 'NONE',  ( 5.585596099150174965, 7.539614753807099667, -1.443375672974057666 ) ) ;
#3834 = CARTESIAN_POINT ( 'NONE',  ( -11.52114515671133610, 8.081606464056415362, 2.192706985476595261 ) ) ;
#3835 = AXIS2_PLACEMENT_3D ( 'NONE', #173719, #205098, #39419 ) ;
#3836 = CARTESIAN_POINT ( 'NONE',  ( 1.393688021309073433, 1.637156065531343740, 1.411701162175371893 ) ) ;
#3837 = CARTESIAN_POINT ( 'NONE',  ( 2.952499795743710020, 1.423742661936340470, 1.427719607385954381 ) ) ;
#3838 = CARTESIAN_POINT ( 'NONE',  ( 0.000000000000000000, 12.31951671548121219, 10.25000000000000000 ) ) ;
#3839 = CARTESIAN_POINT ( 'NONE',  ( 1.200320640528436789, -2.161883444890321915, 0.0006282887012112879947 ) ) ;
#3840 = CARTESIAN_POINT ( 'NONE',  ( 3.590661340855735961, -0.3832702008734929500, -1.933690442540521470 ) ) ;
#3841 = CARTESIAN_POINT ( 'NONE',  ( 6.509000000000034092, 7.052765612591089806, 2.598154238703707541 ) ) ;
#3842 = CARTESIAN_POINT ( 'NONE',  ( 2.894010800797857108, -0.5660635412718226789, -1.857715926975093135 ) ) ;
#3845 = EDGE_LOOP ( 'NONE', ( #61817, #107068, #146519, #143070, #69421, #145271, #154020 ) ) ;
#3844 = CARTESIAN_POINT ( 'NONE',  ( -3.287551290890295519, -0.1090402198146262214, -0.08054459095556501524 ) ) ;
#3843 = DIRECTION ( 'NONE',  ( -0.000000000000000000, 0.000000000000000000, -1.000000000000000000 ) ) ;
#3846 = CARTESIAN_POINT ( 'NONE',  ( -4.543390873910949423, 6.393985001019784953, 1.443375672974058777 ) ) ;
#3847 = CARTESIAN_POINT ( 'NONE',  ( -0.2106854629475244378, 7.629137130509075604, -2.597154134060948749 ) ) ;
#3848 = CARTESIAN_POINT ( 'NONE',  ( 4.064412189046650248, 7.963840997188264659, 0.7998128361456271485 ) ) ;
#3849 = CARTESIAN_POINT ( 'NONE',  ( -5.842637852846353397, 5.781108681267656202, 0.7998128361456281477 ) ) ;
#3850 = CARTESIAN_POINT ( 'NONE',  ( -5.745623237141265882, 9.925253886631958622, 0.7998128361456291469 ) ) ;
#3851 = CARTESIAN_POINT ( 'NONE',  ( -8.473482818416657736, 12.82955435488738516, -0.7216878364870267237 ) ) ;
#3852 = CARTESIAN_POINT ( 'NONE',  ( 0.4994150495197279271, 1.833458848295946186, -1.227822027206025179 ) ) ;
#3854 = EDGE_CURVE ( 'NONE', #157380, #188684, #180468, .T. ) ;
#3853 = PLANE ( 'NONE',  #118770 ) ;
#3855 = CARTESIAN_POINT ( 'NONE',  ( 3.713678095275750657, 0.4809820416172749802, -1.901733992618503066 ) ) ;
#3856 = CARTESIAN_POINT ( 'NONE',  ( 6.825640269476072497, 10.05066518344239412, 1.199719254218460707 ) ) ;
#3857 = CARTESIAN_POINT ( 'NONE',  ( 1.195935645703485761, 1.779627574718087635, 0.9480385367472211611 ) ) ;
#3858 = ORIENTED_EDGE ( 'NONE', *, *, #8612, .T. ) ;
#3859 = CARTESIAN_POINT ( 'NONE',  ( 3.872345094350841510, -2.094861191690357227, -0.3068023397686749920 ) ) ;
#3860 = CARTESIAN_POINT ( 'NONE',  ( -0.7500000000000006661, 2.139583334016155636, -1.299038105676652011 ) ) ;
#3862 = CARTESIAN_POINT ( 'NONE',  ( -4.855791571988752331, 8.816840600628864877, 0.7998128361456481317 ) ) ;
#3861 =( NAMED_UNIT ( * ) PLANE_ANGLE_UNIT ( ) SI_UNIT ( $, .RADIAN. ) );
#3863 = CARTESIAN_POINT ( 'NONE',  ( 3.503688343963582863, -0.7473321665184138318, -1.682825604429179833 ) ) ;
#3864 = ORIENTED_EDGE ( 'NONE', *, *, #113758, .T. ) ;
#3865 = CARTESIAN_POINT ( 'NONE',  ( -9.155833807930273238, 9.576227618873799585, -0.7998128361456291469 ) ) ;
#3866 = CARTESIAN_POINT ( 'NONE',  ( -3.307826292054345974, 6.802955074131202373, -0.7216878364870574769 ) ) ;
#3867 = CARTESIAN_POINT ( 'NONE',  ( 3.779626292077961747, 0.2561244552635975058, -2.104982076983111572 ) ) ;
#3868 = PLANE ( 'NONE',  #156537 ) ;
#3869 = CARTESIAN_POINT ( 'NONE',  ( 5.289652487626049115, 9.323011668872403845, 0.7998128361456462443 ) ) ;
#3870 = CARTESIAN_POINT ( 'NONE',  ( 5.255176862235733992, -1.738700696582769378, -1.105936373271217521 ) ) ;
#3872 = CARTESIAN_POINT ( 'NONE',  ( 2.313779677144182312, 1.201330555204615180, -1.395457044143719072 ) ) ;
#3871 = CARTESIAN_POINT ( 'NONE',  ( -5.391338639728555648, 9.441645512991978961, -0.7998128361456231517 ) ) ;
#3873 = CARTESIAN_POINT ( 'NONE',  ( 9.531545685607134999, 11.07889037375188401, 1.199719254218450271 ) ) ;
#3874 = CARTESIAN_POINT ( 'NONE',  ( 0.6823417656249899377, 5.676041667008087543, -1.181850606188754593 ) ) ;
#3875 = CARTESIAN_POINT ( 'NONE',  ( -5.914749137557818059, 6.074338953224275528, -0.6118981238392419142 ) ) ;
#3876 = AXIS2_PLACEMENT_3D ( 'NONE', #130728, #162103, #45163 ) ;
#3877 = SURFACE_STYLE_USAGE ( .BOTH. , #85161 ) ;
#3878 = CARTESIAN_POINT ( 'NONE',  ( 0.9311234436981545848, -1.459380368602566369, -3.474999999999999201 ) ) ;
#3879 = AXIS2_PLACEMENT_3D ( 'NONE', #113728, #933, #69137 ) ;
#3880 = CARTESIAN_POINT ( 'NONE',  ( 1.875870136999336246, 2.111227540014638304, -0.6426800678154330759 ) ) ;
#3881 = CARTESIAN_POINT ( 'NONE',  ( 4.147957446309138874, 0.7671257181886274035, -2.128492778801443830 ) ) ;
#3882 = AXIS2_PLACEMENT_3D ( 'NONE', #113039, #62086, #78321 ) ;
#3883 = CARTESIAN_POINT ( 'NONE',  ( -6.995644074971465010, 10.14503993989993091, 1.082531754730549967 ) ) ;
#3884 = CARTESIAN_POINT ( 'NONE',  ( 4.798965708296219823, -0.2289270959113845205, -1.797013726050479709 ) ) ;
#3885 = CARTESIAN_POINT ( 'NONE',  ( 4.680823747822191017, 1.589204433792507087, -1.069448900409355030 ) ) ;
#3886 = CARTESIAN_POINT ( 'NONE',  ( 1.364683531249990311, 4.676041667008083103, 0.7879004041258500513 ) ) ;
#3887 = CARTESIAN_POINT ( 'NONE',  ( 3.379716691394366368, 1.249474069150168454, 1.524969178572218809 ) ) ;
#3888 = CARTESIAN_POINT ( 'NONE',  ( 4.768341783539651324, -1.221614081569386334, 1.416756073533788518 ) ) ;
#3889 = CARTESIAN_POINT ( 'NONE',  ( 3.862222655691281759, 2.290455142492770602, -0.2811034502991411888 ) ) ;
#3890 = CARTESIAN_POINT ( 'NONE',  ( 4.773795620589037725, -1.825254877749547866, 0.3623055857514579370 ) ) ;
#3891 = CARTESIAN_POINT ( 'NONE',  ( -1.001543065824772872E-14, 5.321875000341422357, 1.575800808251672791 ) ) ;
#3892 = CARTESIAN_POINT ( 'NONE',  ( 0.6203277878081385754, 1.987498645412737908, 0.3399528957561820386 ) ) ;
#3894 = CARTESIAN_POINT ( 'NONE',  ( 1.840588936376737372, 2.083348874589638466, 0.3076409294043966902 ) ) ;
#3893 = CARTESIAN_POINT ( 'NONE',  ( -4.297571505407598025, 5.076550180139354218, 1.082531754730558626 ) ) ;
#3895 = CARTESIAN_POINT ( 'NONE',  ( 8.224992744984721327, 12.74757530245756243, 1.040834085586084257E-14 ) ) ;
#3897 = CARTESIAN_POINT ( 'NONE',  ( -8.469039510030723861, 13.03229652834454733, 1.040834085586084257E-14 ) ) ;
#3896 = CARTESIAN_POINT ( 'NONE',  ( -0.6823417656249969321, 5.780208333674756283, -1.181850606188749264 ) ) ;
#3898 = CARTESIAN_POINT ( 'NONE',  ( 2.812858766682566181, -0.6196351552101020399, -2.028021595557969015 ) ) ;
#3899 = CARTESIAN_POINT ( 'NONE',  ( 1.220000000000002194, 5.900000000000022560, 1.214306433183764966E-14 ) ) ;
#3901 = ADVANCED_FACE ( 'NONE', ( #93117 ), #122745, .T. ) ;
#3900 = CARTESIAN_POINT ( 'NONE',  ( 0.8615889817988997557, -1.594800366461980756, -1.239340803694780835 ) ) ;
#3902 = CARTESIAN_POINT ( 'NONE',  ( -0.6823417656250212460, 2.051041667008083991, 1.181850606188767472 ) ) ;
#3903 = CARTESIAN_POINT ( 'NONE',  ( -4.460269349215930212, 4.305995116947750390, 1.214306433183764966E-14 ) ) ;
#3904 = CARTESIAN_POINT ( 'NONE',  ( 5.671388329218120639, 5.511041227042920099, 1.040834085586084257E-14 ) ) ;
#3905 = ORIENTED_EDGE ( 'NONE', *, *, #25840, .T. ) ;
#3906 = CARTESIAN_POINT ( 'NONE',  ( 2.372553944209778720, -1.331880425775422205, 1.702409713178254069 ) ) ;
#3907 = CARTESIAN_POINT ( 'NONE',  ( 6.610000000000026077, 2.442988107647511509, 2.382821027452782570 ) ) ;
#3910 = DIRECTION ( 'NONE',  ( 0.000000000000000000, -0.7999999999999973799, -0.6000000000000034195 ) ) ;
#3909 = CARTESIAN_POINT ( 'NONE',  ( -3.001048869802147134, 2.786623193720125791, -2.499999999999995115 ) ) ;
#3908 = CARTESIAN_POINT ( 'NONE',  ( 4.213551878797002992, 8.137837301896977849, 0.000000000000000000 ) ) ;
#3911 = CARTESIAN_POINT ( 'NONE',  ( 9.693716643646590470, 12.33242205571964512, 1.443375672974076540 ) ) ;
#3912 = DIRECTION ( 'NONE',  ( -0.1510067114093955887, -0.000000000000000000, -0.9885327375000383388 ) ) ;
#3913 = CARTESIAN_POINT ( 'NONE',  ( -7.361714222540411967, 11.53249099303175385, 0.000000000000000000 ) ) ;
#3914 = EDGE_CURVE ( 'NONE', #204988, #120419, #141146, .T. ) ;
#3915 = CARTESIAN_POINT ( 'NONE',  ( 6.550343146927733784, -1.615745695573450824, 1.326605865911892002 ) ) ;
#3916 = DIRECTION ( 'NONE',  ( 0.000000000000000000, 0.000000000000000000, -1.000000000000000000 ) ) ;
#3918 = CARTESIAN_POINT ( 'NONE',  ( 0.6823417656249934904, 11.44270833367473728, 1.181850606188764807 ) ) ;
#3917 = CARTESIAN_POINT ( 'NONE',  ( 2.008995473212730865, 1.676182761729711590, -1.519857458481475909 ) ) ;
#3919 = CARTESIAN_POINT ( 'NONE',  ( -9.494787648271923786, 9.971673765939062406, 1.040834085586084257E-14 ) ) ;
#3920 = CARTESIAN_POINT ( 'NONE',  ( -5.897433631820158340, 5.982686779986042147, 0.7216878364870317197 ) ) ;
#3921 = CARTESIAN_POINT ( 'NONE',  ( -1.364683531250000748, 2.321875000341422357, 1.214306433183764966E-14 ) ) ;
#3922 = CARTESIAN_POINT ( 'NONE',  ( -1.001543065824772872E-14, 4.462500000000024336, 1.732050807568877637 ) ) ;
#3923 = CARTESIAN_POINT ( 'NONE',  ( -1.500000000000001110, 9.770833333333333925, 0.8660254037844419273 ) ) ;
#3924 = CARTESIAN_POINT ( 'NONE',  ( 3.756244407761480275, 0.6229016427463770489, 1.608663766957881824 ) ) ;
#3925 = CARTESIAN_POINT ( 'NONE',  ( 5.890091390494168522, 5.836471141856793388, 0.000000000000000000 ) ) ;
#3926 = CARTESIAN_POINT ( 'NONE',  ( 1.598528592787134883, 1.450519685958560512, -1.013601284844565908 ) ) ;
#3927 = CARTESIAN_POINT ( 'NONE',  ( 2.631496214491501728, -0.1952657482040425496, 2.003584891602292473 ) ) ;
#3928 = CARTESIAN_POINT ( 'NONE',  ( 5.508869005905306260, 1.674340917344345536, -1.437622030140395912 ) ) ;
#3929 = ORIENTED_EDGE ( 'NONE', *, *, #161141, .F. ) ;
#3930 = CARTESIAN_POINT ( 'NONE',  ( -5.237192476628793614, 9.332084666034067055, 0.7998128361456291469 ) ) ;
#3932 = CARTESIAN_POINT ( 'NONE',  ( 4.165638788432171502, 1.319243065725501429, 1.525032742243138228 ) ) ;
#3931 = CARTESIAN_POINT ( 'NONE',  ( 4.969442291489525765, -1.791676405564743169, -1.133875526122554156 ) ) ;
#3934 = ORIENTED_EDGE ( 'NONE', *, *, #112984, .F. ) ;
#3933 = CARTESIAN_POINT ( 'NONE',  ( 4.623216614435611937, 1.579690555364177351, 0.8866180403494609008 ) ) ;
#3935 = ORIENTED_EDGE ( 'NONE', *, *, #52342, .F. ) ;
#3936 = CARTESIAN_POINT ( 'NONE',  ( 1.867826558377215118, 0.9591755677602132879, 1.605880698980370225 ) ) ;
#3938 = EDGE_CURVE ( 'NONE', #101924, #2318, #9654, .T. ) ;
#3937 = AXIS2_PLACEMENT_3D ( 'NONE', #168326, #86007, #119639 ) ;
#3939 = CARTESIAN_POINT ( 'NONE',  ( 2.034713692888018954, 8.461455076002922127, -2.499999999999988898 ) ) ;
#3940 = CARTESIAN_POINT ( 'NONE',  ( 1.476665317443916603, -1.350161712199383413, 1.354623164920423450 ) ) ;
#3941 = CARTESIAN_POINT ( 'NONE',  ( 0.4019237886466884846, 9.676335450315368902, -1.499999999999994449 ) ) ;
#3942 = CARTESIAN_POINT ( 'NONE',  ( -10.83049189199067719, 4.361170120774730208, -4.636001201543571426 ) ) ;
#3943 = DIRECTION ( 'NONE',  ( 0.000000000000000000, 1.000000000000000000, 0.000000000000000000 ) ) ;
#3944 = B_SPLINE_CURVE_WITH_KNOTS ( 'NONE', 3,
 ( #102434, #103511, #37433, #116615, #169570, #166371, #21151, #197796, #87257, #35291 ),
 .UNSPECIFIED., .F., .F.,
 ( 4, 3, 3, 4 ),
 ( 0.000000000000000000, 6.251636445012719089E-05, 0.0001877505388839963824, 0.0003462489540127104736 ),
 .UNSPECIFIED. ) ;
#3945 = CARTESIAN_POINT ( 'NONE',  ( 0.6823417656249882723, 2.488541667008084435, -1.181850606188749264 ) ) ;
#3946 = FACE_BOUND ( 'NONE', #188223, .T. ) ;
#3947 = CARTESIAN_POINT ( 'NONE',  ( 6.048345925472191631, 7.189396680206621149, 1.082531754730549967 ) ) ;
#3948 = CARTESIAN_POINT ( 'NONE',  ( 2.084357000244409175, 1.132115006494602394, -1.602057852124554316 ) ) ;
#3949 = DIRECTION ( 'NONE',  ( 0.6507913734559640506, -0.7592566023653004592, 0.000000000000000000 ) ) ;
#3950 = CARTESIAN_POINT ( 'NONE',  ( -6.069210040772897052, 7.109775131437022999, -1.199719254218453823 ) ) ;
#3951 = CARTESIAN_POINT ( 'NONE',  ( 4.728832233812888752, 1.460412846248357210, -1.537820402542383169 ) ) ;
#3953 = CARTESIAN_POINT ( 'NONE',  ( 0.000000000000000000, 13.79999999999999893, 0.000000000000000000 ) ) ;
#3952 = CARTESIAN_POINT ( 'NONE',  ( 8.585337585951586803, 11.03931315507545108, -1.599625672291255185 ) ) ;
#3954 = CARTESIAN_POINT ( 'NONE',  ( 5.272717044759430927, -1.855309747074182836, -0.6666870051924634888 ) ) ;
#3955 = CARTESIAN_POINT ( 'NONE',  ( -1.402160292154681736E-14, 1.446875000341420137, -1.575800808251659024 ) ) ;
#3956 = CARTESIAN_POINT ( 'NONE',  ( 0.9846361663228007099, -1.273826410524713459, 1.558997777263083417 ) ) ;
#3957 = ORIENTED_EDGE ( 'NONE', *, *, #138240, .F. ) ;
#3958 = CARTESIAN_POINT ( 'NONE',  ( 1.107202915679715405, -0.04781017987004822223, 2.116844178444466706 ) ) ;
#3959 = CARTESIAN_POINT ( 'NONE',  ( 11.65634836436412947, 7.079629224059313053, -2.645114728738123144 ) ) ;
#3960 = CARTESIAN_POINT ( 'NONE',  ( 3.068866956829822801, 1.501395149897828851, -1.425812640530661479 ) ) ;
#3961 = CARTESIAN_POINT ( 'NONE',  ( 3.607351389687783794, 6.366271167014519783, 1.199719254218451159 ) ) ;
#3962 = CARTESIAN_POINT ( 'NONE',  ( 4.064412189046650248, 7.963840997188264659, 0.7998128361456271485 ) ) ;
#3963 = ORIENTED_EDGE ( 'NONE', *, *, #75861, .T. ) ;
#3965 = CARTESIAN_POINT ( 'NONE',  ( 6.342516933094585418, 6.294024598232139667, 1.040834085586084257E-14 ) ) ;
#3964 = CARTESIAN_POINT ( 'NONE',  ( 5.103505634659632584, -2.080644823048905412, 0.2041521072984452956 ) ) ;
#3968 = ORIENTED_EDGE ( 'NONE', *, *, #108052, .T. ) ;
#3967 = CARTESIAN_POINT ( 'NONE',  ( 1.031567638852897373, -1.767431343716918013, 0.3961611186833951526 ) ) ;
#3966 = CARTESIAN_POINT ( 'NONE',  ( 2.871877888313049354, 0.9750061419492547232, 1.543211660213184899 ) ) ;
#3969 = CARTESIAN_POINT ( 'NONE',  ( 6.463508838306311510, 0.3818026259072569983, -2.173449913608488160 ) ) ;
#3970 = CARTESIAN_POINT ( 'NONE',  ( 4.017950238124170959, 5.837568840759415068, 1.364652132238639348 ) ) ;
#3971 = CARTESIAN_POINT ( 'NONE',  ( 9.390682975800181964, 11.17576483377143681, 6.985571074475002362 ) ) ;
#3972 = AXIS2_PLACEMENT_3D ( 'NONE', #186734, #173725, #206181 ) ;
#3973 = CARTESIAN_POINT ( 'NONE',  ( 4.911249081476435130, 1.917979745144289261, 1.091307337132418454 ) ) ;
#3974 = CARTESIAN_POINT ( 'NONE',  ( -8.012344526598182026E-15, 8.859375000341405126, -1.575800808251669460 ) ) ;
#3975 = VERTEX_POINT ( 'NONE', #81812 ) ;
#3976 = CARTESIAN_POINT ( 'NONE',  ( 4.441997247558228779, -1.179148908705367482, -1.505365500079666852 ) ) ;
#3977 = CARTESIAN_POINT ( 'NONE',  ( -4.457933580795036654, 4.095344020549286590, -0.7998128361456221525 ) ) ;
#3978 = CARTESIAN_POINT ( 'NONE',  ( 6.923409998072794558, 11.22906209772695618, 1.040834085586084257E-14 ) ) ;
#3979 = CARTESIAN_POINT ( 'NONE',  ( 6.338344951546218908, -1.110931056888088353, 1.746890944850579830 ) ) ;
#3980 = CARTESIAN_POINT ( 'NONE',  ( 1.360316468749955598, 0.5260416670081086155, 0.7853790794158820310 ) ) ;
#3981 = CARTESIAN_POINT ( 'NONE',  ( 5.517805330637495231, 6.500156309574290248, -1.082531754730543083 ) ) ;
#3982 = CARTESIAN_POINT ( 'NONE',  ( 6.304242050522723240, 1.625252681175231029, -1.470355468214133543 ) ) ;
#3983 = CARTESIAN_POINT ( 'NONE',  ( 5.894874513638865388, 7.262872338272549300, -1.253420816524719150 ) ) ;
#3984 = DIRECTION ( 'NONE',  ( -0.000000000000000000, -1.000000000000000000, -0.000000000000000000 ) ) ;
#3985 = VERTEX_POINT ( 'NONE', #80756 ) ;
#3986 = CIRCLE ( 'NONE', #152759, 1.962502847949850526 ) ;
#3987 = CARTESIAN_POINT ( 'NONE',  ( 0.000000000000000000, 6.999999999999992006, 0.000000000000000000 ) ) ;
#3988 = CARTESIAN_POINT ( 'NONE',  ( 4.094877388769967652, 1.581529129216452390, -0.9985332613470514485 ) ) ;
#3989 = CARTESIAN_POINT ( 'NONE',  ( 3.285556943749998737, -1.742708332855374076, -1.896917185911906722 ) ) ;
#3990 = FACE_OUTER_BOUND ( 'NONE', #157458, .T. ) ;
#3991 = CARTESIAN_POINT ( 'NONE',  ( -8.541273586929371220, 9.067166727613487964, 0.7216878364870438212 ) ) ;
#3992 = CARTESIAN_POINT ( 'NONE',  ( 4.115782150200256950, 6.959440387612411349, 1.199719254218452047 ) ) ;
#3993 = CARTESIAN_POINT ( 'NONE',  ( 6.311484202361478779, 7.322151976631905868, -1.199719254218446718 ) ) ;
#3994 = CARTESIAN_POINT ( 'NONE',  ( 0.2390023523631857882, -0.1431304410692470219, -1.937466148627289719 ) ) ;
#3995 = CARTESIAN_POINT ( 'NONE',  ( 0.9136856707930467447, -1.281379520587552889, -1.556895127150646374 ) ) ;
#3996 = CARTESIAN_POINT ( 'NONE',  ( -8.622095623286845978, 12.14652976288826913, 1.199719254218462483 ) ) ;
#3997 = CARTESIAN_POINT ( 'NONE',  ( 6.099189001301251523, 8.209082816308541197, 1.599625672291268286 ) ) ;
#3998 = FACE_OUTER_BOUND ( 'NONE', #11820, .T. ) ;
#3999 = CARTESIAN_POINT ( 'NONE',  ( 1.236564921189796662, 0.4304113295856801247, 2.148598399174222351 ) ) ;
#4000 = CARTESIAN_POINT ( 'NONE',  ( 5.848246728868278232, 1.823843535133644389, 0.08496628090458313576 ) ) ;
#4001 = CARTESIAN_POINT ( 'NONE',  ( -4.810445574750349174, 4.506608013497163334, 0.7998128361456341429 ) ) ;
#4002 = CARTESIAN_POINT ( 'NONE',  ( 4.068855497876973537, 7.761098824249525130, -0.7216878364870338292 ) ) ;
#4003 = CARTESIAN_POINT ( 'NONE',  ( 10.23370702021670020, 10.83374636654133383, 0.7998128361456462443 ) ) ;
#4004 = CARTESIAN_POINT ( 'NONE',  ( 3.167801447087334576, 6.847518788243868393, -0.7998128361456291469 ) ) ;
#4005 = CARTESIAN_POINT ( 'NONE',  ( 7.024532985656128936, 9.288650798055913427, 1.443375672974065660 ) ) ;
#4006 = ORIENTED_EDGE ( 'NONE', *, *, #98111, .F. ) ;
#4008 = CARTESIAN_POINT ( 'NONE',  ( 0.7682272020711936600, 2.010684543107125410, -0.1010625827991030873 ) ) ;
#4007 = CARTESIAN_POINT ( 'NONE',  ( 3.632213977189250098, 0.2737156317273430894, 1.820677940640710979 ) ) ;
#4009 = CARTESIAN_POINT ( 'NONE',  ( 1.599382804601066743, 1.132622197759477478, -1.999898178936350357 ) ) ;
#4011 = CARTESIAN_POINT ( 'NONE',  ( 0.9536794021071954841, -0.6768100219149524310, 1.733691362649824264 ) ) ;
#4010 = CARTESIAN_POINT ( 'NONE',  ( 3.877268743828270470, 5.546566172598190292, 1.443375672974062551 ) ) ;
#4012 = CARTESIAN_POINT ( 'NONE',  ( 1.642778471875001811, -3.842708332855375275, 2.845375778867859751 ) ) ;
#4013 = CARTESIAN_POINT ( 'NONE',  ( -5.752737250900127997, 5.605948302338584099, 0.000000000000000000 ) ) ;
#4014 = PRESENTATION_STYLE_ASSIGNMENT (( #149227 ) ) ;
#4015 = CARTESIAN_POINT ( 'NONE',  ( 4.007995338699682719, -0.7271224857151190601, 1.768968726348684406 ) ) ;
#4016 = CARTESIAN_POINT ( 'NONE',  ( -8.299562589859897699, 12.83457345481192036, -0.7998128361456281477 ) ) ;
#4017 = CARTESIAN_POINT ( 'NONE',  ( 6.490673131624099312, 6.748652840683030618, -0.08655830178419705867 ) ) ;
#4018 = CARTESIAN_POINT ( 'NONE',  ( -5.804299160426224624, 9.785783097223662352, -0.7216878364870338292 ) ) ;
#4020 = CARTESIAN_POINT ( 'NONE',  ( 2.324885834233282544, -0.002380789299309681549, 1.870836310375329381 ) ) ;
#4019 = CARTESIAN_POINT ( 'NONE',  ( 3.351197789220595080, 0.5058271172731694243, -2.028516034726547623 ) ) ;
#4021 = CARTESIAN_POINT ( 'NONE',  ( 7.280365300858406385, 11.43758391773608984, 1.040834085586084257E-14 ) ) ;
#4022 = CARTESIAN_POINT ( 'NONE',  ( -1.364683531250010740, 5.342708333674750953, 0.7879004041258379498 ) ) ;
#4023 = CARTESIAN_POINT ( 'NONE',  ( 2.911345607792231949, -0.8600081332746039031, -1.513042209403854699 ) ) ;
#4024 = CARTESIAN_POINT ( 'NONE',  ( 3.822509244049070887, 6.547012320444182798, -1.199719254218452047 ) ) ;
#4025 = CARTESIAN_POINT ( 'NONE',  ( -5.480535539083196461, 6.054881262792200403, 1.008611741575331289 ) ) ;
#4026 = CARTESIAN_POINT ( 'NONE',  ( 3.562884411436726850, -1.522066076379503974, -0.8114761229951471533 ) ) ;
#4027 = CARTESIAN_POINT ( 'NONE',  ( 4.370767597569780172, -0.0006098066561242150270, -2.191739723162715592 ) ) ;
#4028 = CARTESIAN_POINT ( 'NONE',  ( 5.918643953348324160, 1.484978324971843566, -1.632713241052483832 ) ) ;
#4029 = CARTESIAN_POINT ( 'NONE',  ( 6.983263157960349687, 0.5706719223780298833, 2.105707282093812083 ) ) ;
#4030 = AXIS2_PLACEMENT_3D ( 'NONE', #178607, #77890, #98413 ) ;
#4031 = CARTESIAN_POINT ( 'NONE',  ( 3.274467656630496659, -1.066080149914239161, -1.891199154716957098 ) ) ;
#4032 = CARTESIAN_POINT ( 'NONE',  ( 2.736711336054332921, 0.2235625380298221498, 1.811883384933578256 ) ) ;
#4033 = CARTESIAN_POINT ( 'NONE',  ( 3.998552357014331982, 7.829812261164016185, 1.248643980066187585E-14 ) ) ;
#4034 = CARTESIAN_POINT ( 'NONE',  ( 4.610634390349757084, 2.027228601534016406, 0.6112464051817678712 ) ) ;
#4035 = MECHANICAL_DESIGN_GEOMETRIC_PRESENTATION_REPRESENTATION (  '', ( #132131 ), #83686 ) ;
#4036 = ORIENTED_EDGE ( 'NONE', *, *, #72494, .F. ) ;
#4038 = CARTESIAN_POINT ( 'NONE',  ( -1.364683531250012516, 2.842708333674754506, 0.7879004041258379498 ) ) ;
#4037 = CARTESIAN_POINT ( 'NONE',  ( 5.091491514903929705, -0.8269519956315901643, 2.138199492833972482 ) ) ;
#4039 = CARTESIAN_POINT ( 'NONE',  ( 6.620655732516648406, 2.482285041548700111, 2.111775279032622521 ) ) ;
#4040 = CARTESIAN_POINT ( 'NONE',  ( 8.594979316059474073, 12.11489407112305372, 1.199719254218450271 ) ) ;
#4041 = EDGE_CURVE ( 'NONE', #37994, #61984, #37334, .T. ) ;
#4042 = CARTESIAN_POINT ( 'NONE',  ( 0.5398874254142792539, -2.012210497580559476, 0.6691108114003360141 ) ) ;
#4043 = CARTESIAN_POINT ( 'NONE',  ( -5.016153647376219382, 6.875265226737464985, 1.443375672974064550 ) ) ;
#4044 = DIRECTION ( 'NONE',  ( 0.000000000000000000, 0.000000000000000000, 1.000000000000000000 ) ) ;
#4045 = CARTESIAN_POINT ( 'NONE',  ( -5.056828107772860292, 6.922718763866881453, -1.443375672974051449 ) ) ;
#4047 = CARTESIAN_POINT ( 'NONE',  ( 0.7500000000000006661, 11.69791666734946389, -1.299038105676657340 ) ) ;
#4046 = CARTESIAN_POINT ( 'NONE',  ( -5.000000000000009770, 3.850000000000006306, 6.071532165918824830E-15 ) ) ;
#4048 = ORIENTED_EDGE ( 'NONE', *, *, #197756, .F. ) ;
#4049 = CARTESIAN_POINT ( 'NONE',  ( 5.502577337681268332, -1.966645332631598908, 0.4444998760482973821 ) ) ;
#4051 = CARTESIAN_POINT ( 'NONE',  ( 4.539923930118438200, 1.343280314546798637, 1.565306332949261803 ) ) ;
#4050 = CARTESIAN_POINT ( 'NONE',  ( 5.443762371086860341, 6.309809840144842141, 1.199719254218462483 ) ) ;
#4053 = CARTESIAN_POINT ( 'NONE',  ( -0.2411972340276022364, 0.7381021182278154624, -1.984382818515282532 ) ) ;
#4052 = CARTESIAN_POINT ( 'NONE',  ( 4.830447868218803897, 8.857549289555754157, -0.7998128361456481317 ) ) ;
#4054 = CARTESIAN_POINT ( 'NONE',  ( 7.550965208168244125, 7.774157262476569130, -0.7998128361456341429 ) ) ;
#4055 = CARTESIAN_POINT ( 'NONE',  ( -3.285556943749998737, -0.7802083328553744979, 1.896917185911908499 ) ) ;
#4056 = CARTESIAN_POINT ( 'NONE',  ( 0.1329588055935760349, 4.094961471249922269, -2.400852151441670745 ) ) ;
#4057 = CARTESIAN_POINT ( 'NONE',  ( 0.9551577523512165824, 0.4061005957273036704, -2.050632492140195939 ) ) ;
#4058 = CARTESIAN_POINT ( 'NONE',  ( 5.010388774477189777, -1.913804350592800629, 0.6351971752796632398 ) ) ;
#4059 = CARTESIAN_POINT ( 'NONE',  ( 4.212339636135824961, 1.685202893791247769, 0.7422218904534692019 ) ) ;
#4060 = CARTESIAN_POINT ( 'NONE',  ( 4.984594031318565932, 8.967110136513669616, 0.7998128361456462443 ) ) ;
#4062 = ADVANCED_FACE ( 'NONE', ( #182490 ), #100491, .T. ) ;
#4061 = CARTESIAN_POINT ( 'NONE',  ( 2.187500000000001332, -1.451031289061030849, 1.451031289061208041 ) ) ;
#4063 = CARTESIAN_POINT ( 'NONE',  ( 0.3402809042804251227, 0.2871511109263942818, 1.700534619074739906 ) ) ;
#4064 = CARTESIAN_POINT ( 'NONE',  ( 4.000000000000012434, 4.999999999999997335, -1.214306433183764966E-14 ) ) ;
#4065 = CARTESIAN_POINT ( 'NONE',  ( 1.126083094664981799, 0.4549445381971609637, 2.253098081826758303 ) ) ;
#4066 = CARTESIAN_POINT ( 'NONE',  ( -4.388035272317281077, 8.271124917678806199, 0.7998128361456481317 ) ) ;
#4067 = CARTESIAN_POINT ( 'NONE',  ( 0.7204656808509112276, -1.211343046821738101, -1.910610397963452112 ) ) ;
#4068 = CARTESIAN_POINT ( 'NONE',  ( 3.088603512095712045, -2.074978072712420296, -0.3595722787458465186 ) ) ;
#4069 = CARTESIAN_POINT ( 'NONE',  ( -3.447516199624892419, 7.244129009529488350, 0.7998128361456352531 ) ) ;
#4070 = CARTESIAN_POINT ( 'NONE',  ( 6.317209508963599340, 9.457495962844502557, 1.199719254218462483 ) ) ;
#4071 = CARTESIAN_POINT ( 'NONE',  ( 6.997416677984476863, 7.336276677169590421, 0.000000000000000000 ) ) ;
#4072 = CARTESIAN_POINT ( 'NONE',  ( 5.875000000000001776, 2.052068128417940951, -3.214650538869141380E-13 ) ) ;
#4073 = CARTESIAN_POINT ( 'NONE',  ( -5.605406444246153974, 8.627059054007450101, -1.199719254218440723 ) ) ;
#4074 = CARTESIAN_POINT ( 'NONE',  ( 6.493992390821439642, 7.639041213122241381, -1.082531754730543971 ) ) ;
#4075 = CARTESIAN_POINT ( 'NONE',  ( 4.666586266758273815, 7.089143983547513628, 1.366926838653566012 ) ) ;
#4076 = CARTESIAN_POINT ( 'NONE',  ( -3.249150368769345043, 6.942425863539538611, 0.7998128361456341429 ) ) ;
#4077 = CARTESIAN_POINT ( 'NONE',  ( 5.097972104635399404, 1.492264293747805226, 1.645667271412653898 ) ) ;
#4078 = CARTESIAN_POINT ( 'NONE',  ( 1.886939110189549185, 1.905679594745551819, -1.081921739459410059 ) ) ;
#4079 = CARTESIAN_POINT ( 'NONE',  ( -4.089755892816631544, 7.923132308261379819, -0.7998128361456281477 ) ) ;
#4080 = CARTESIAN_POINT ( 'NONE',  ( -11.86685672517501899, 9.990810821401886699, 1.056525322636010289 ) ) ;
#4081 = CARTESIAN_POINT ( 'NONE',  ( 5.916451087343006954, 0.7937011933104149985, 1.794315766958521241 ) ) ;
#4082 = CARTESIAN_POINT ( 'NONE',  ( 1.364683531249988757, 2.134375000341422357, 1.214306433183764966E-14 ) ) ;
#4083 = CARTESIAN_POINT ( 'NONE',  ( 6.890000000000012115, 1.205492346117660762, 2.388860368086835884 ) ) ;
#4085 = ORIENTED_EDGE ( 'NONE', *, *, #79933, .T. ) ;
#4084 = CARTESIAN_POINT ( 'NONE',  ( -4.772106882330227506, 7.550913215151819458, -1.082531754730549967 ) ) ;
#4086 = CARTESIAN_POINT ( 'NONE',  ( 5.027636390373714903, -0.3086946445357250379, 2.097867224209007730 ) ) ;
#4087 = CARTESIAN_POINT ( 'NONE',  ( -6.780486220610186798, 8.043560357867583832, -1.082531754730549967 ) ) ;
#4088 = EDGE_LOOP ( 'NONE', ( #114985, #53281, #184745, #68979 ) ) ;
#4090 = CARTESIAN_POINT ( 'NONE',  ( 6.772347375734490527, -1.334533509509854943, 1.701269717329929820 ) ) ;
#4089 = CARTESIAN_POINT ( 'NONE',  ( -5.560252395380252288, 7.580323442733986283, 1.443375672974058777 ) ) ;
#4091 = CARTESIAN_POINT ( 'NONE',  ( 7.156006149914539982, 7.243095351188763686, 1.040834085586084257E-14 ) ) ;
#4092 = CARTESIAN_POINT ( 'NONE',  ( 5.161589042655139181, 0.9124512986629171873, 1.599201395118980740 ) ) ;
#4093 = DIRECTION ( 'NONE',  ( 0.000000000000000000, 0.000000000000000000, 1.000000000000000000 ) ) ;
#4094 = CARTESIAN_POINT ( 'NONE',  ( -0.6823417656249969321, 3.280208333674754062, -1.181850606188749264 ) ) ;
#4095 = B_SPLINE_CURVE_WITH_KNOTS ( 'NONE', 3,
 ( #171376, #88001, #55498, #187619, #185480, #54437, #37105, #20833 ),
 .UNSPECIFIED., .F., .F.,
 ( 4, 2, 2, 4 ),
 ( 0.000000000000000000, 0.0002185754043082796050, 0.0004371508086165592100, 0.0008743016172331182032 ),
 .UNSPECIFIED. ) ;
#4096 = CARTESIAN_POINT ( 'NONE',  ( 1.047962540061377679, -1.372746097444921043, 1.069743175550162295 ) ) ;
#4097 = DIRECTION ( 'NONE',  ( 0.000000000000000000, 1.000000000000000000, 0.000000000000000000 ) ) ;
#4098 = CYLINDRICAL_SURFACE ( 'NONE', #203756, 1.224999999999996980 ) ;
#4099 = CARTESIAN_POINT ( 'NONE',  ( 0.000000000000000000, 5.499999999999998224, 0.000000000000000000 ) ) ;
#4100 = CARTESIAN_POINT ( 'NONE',  ( 5.014612968065254250, 1.493337269798940881, -1.563205770552501761 ) ) ;
#4101 = CARTESIAN_POINT ( 'NONE',  ( -4.783329267523015460, 4.474972321731942593, -0.7998128361456221525 ) ) ;
#4102 = VECTOR ( 'NONE', #211672, 1000.000000000000000 ) ;
#4103 = CARTESIAN_POINT ( 'NONE',  ( -8.310784975052689205, 8.798263347090697906, -0.7216878364870267237 ) ) ;
#4104 = CARTESIAN_POINT ( 'NONE',  ( 4.118171802502921253, -1.108985364570359566, -1.855417305202881506 ) ) ;
#4105 = CARTESIAN_POINT ( 'NONE',  ( -1.364683531250012516, 2.988541667008091096, -0.7879004041258289570 ) ) ;
#4106 = CARTESIAN_POINT ( 'NONE',  ( 5.061777102197771327, 1.950294035894485356, -0.2865203566276338654 ) ) ;
#4107 = CARTESIAN_POINT ( 'NONE',  ( 4.481622980438174864, 1.585354267084694957, 0.7024943803609559057 ) ) ;
#4108 = CARTESIAN_POINT ( 'NONE',  ( 0.3983070667218471805, -0.7439898890007863308, -2.061537379893277677 ) ) ;
#4109 = CARTESIAN_POINT ( 'NONE',  ( 2.573609363736366618, 0.1136701668994527237, -2.304911326000145699 ) ) ;
#4110 = CARTESIAN_POINT ( 'NONE',  ( 4.200502791967850591, -0.6429285697095908914, -1.958015678616845445 ) ) ;
#4111 = CARTESIAN_POINT ( 'NONE',  ( 0.005655660794708254786, -0.8285957215397036224, -1.754384556632330838 ) ) ;
#4112 = CARTESIAN_POINT ( 'NONE',  ( -5.843201017365469596, 9.760892253660966134, 0.7216878364870458196 ) ) ;
#4113 = CARTESIAN_POINT ( 'NONE',  ( -6.317173229324657413, 6.334733287159020954, 0.000000000000000000 ) ) ;
#4114 = CARTESIAN_POINT ( 'NONE',  ( -1.201851678989727383E-14, 2.993750000682821266, 1.732050807568877637 ) ) ;
#4115 =( LENGTH_UNIT ( ) NAMED_UNIT ( * ) SI_UNIT ( .MILLI., .METRE. ) );
#4116 = CARTESIAN_POINT ( 'NONE',  ( -7.497295758232736418, 7.849192594134070333, -0.7216878364870267237 ) ) ;
#4117 = CARTESIAN_POINT ( 'NONE',  ( 3.382038520680182181, 1.398480293485371284, 1.707083182650385389 ) ) ;
#4118 = CARTESIAN_POINT ( 'NONE',  ( -1.642778471875000035, -2.355208332855376341, -2.845375778867859751 ) ) ;
#4119 = ORIENTED_EDGE ( 'NONE', *, *, #170395, .F. ) ;
#4120 = CARTESIAN_POINT ( 'NONE',  ( 0.9009385260731802569, -1.599958946562014539, 0.9501217156336287939 ) ) ;
#4121 = CARTESIAN_POINT ( 'NONE',  ( -0.1290005225502432740, 4.081813041011835175, -2.728655865233818201 ) ) ;
#4122 = CARTESIAN_POINT ( 'NONE',  ( -1.500000000000011324, 5.410416667349489117, -0.8660254037844313801 ) ) ;
#4123 = CARTESIAN_POINT ( 'NONE',  ( 6.966220764712146796, 6.002124920821316323, -2.500000000000000444 ) ) ;
#4125 = CARTESIAN_POINT ( 'NONE',  ( 6.825078400183550720, 7.629137130509051623, 2.644348168701659674 ) ) ;
#4124 = CARTESIAN_POINT ( 'NONE',  ( -5.393601776927423153, 7.665310133586674901, -1.338224700579364379 ) ) ;
#4126 = CARTESIAN_POINT ( 'NONE',  ( 6.404252597826388893, 1.360807738692754176, -1.240355271200761056 ) ) ;
#4127 = ORIENTED_EDGE ( 'NONE', *, *, #163291, .T. ) ;
#4128 = CARTESIAN_POINT ( 'NONE',  ( 2.870052109166462362, 1.101224123558439905, 1.741800865840010593 ) ) ;
#4129 = CARTESIAN_POINT ( 'NONE',  ( -1.360316468750044860, 1.411458333674720622, 0.7853790794158801436 ) ) ;
#4130 = CARTESIAN_POINT ( 'NONE',  ( -6.552668314106420588, 6.539201209412602189, -0.7998128361456291469 ) ) ;
#4131 = CARTESIAN_POINT ( 'NONE',  ( 2.332681060731033540, 1.317659697769531624, -1.530744237074317171 ) ) ;
#4132 = CARTESIAN_POINT ( 'NONE',  ( -15.75000000000000000, 9.799999999999998934, -0.7000000000000009548 ) ) ;
#4133 = CARTESIAN_POINT ( 'NONE',  ( 3.714044015139744914, 6.420469553383295391, 1.199719254218462483 ) ) ;
#4134 = STYLED_ITEM ( 'NONE', ( #8897 ), #173118 ) ;
#4135 = CARTESIAN_POINT ( 'NONE',  ( 1.850533416564412725, 0.6455992098736047513, 1.957236905219070566 ) ) ;
#4137 = CARTESIAN_POINT ( 'NONE',  ( -1.364683531250000748, 13.35937500034139980, 0.000000000000000000 ) ) ;
#4136 = CARTESIAN_POINT ( 'NONE',  ( -9.913101724262725511, 3.481548657788669399, -6.781968449710928049 ) ) ;
#4138 = CARTESIAN_POINT ( 'NONE',  ( 6.993308306550549247, 7.053281200597435685, 1.040834085586084257E-14 ) ) ;
#4139 = CARTESIAN_POINT ( 'NONE',  ( -0.2409995289980038091, 6.947781193150415646, -2.595509233728268583 ) ) ;
#4140 = CARTESIAN_POINT ( 'NONE',  ( 6.006501602161061548, -0.7906231143557163055, -2.060575041408031272 ) ) ;
#4141 = CARTESIAN_POINT ( 'NONE',  ( 1.792469030454997059, -2.151019407201111289, -0.2137723215496489249 ) ) ;
#4142 = CARTESIAN_POINT ( 'NONE',  ( -4.555176424511596878, 7.297827681030051750, 1.082531754730560403 ) ) ;
#4143 = CARTESIAN_POINT ( 'NONE',  ( 1.270720652900014791, -0.3006520276036573902, -1.993892820393451615 ) ) ;
#4144 = CARTESIAN_POINT ( 'NONE',  ( 2.214639623771569088, -1.845710301178200119, -1.369457037089250484 ) ) ;
#4145 = CARTESIAN_POINT ( 'NONE',  ( 4.618660464418627321, 8.442828270562628745, 0.5404566954739065121 ) ) ;
#4146 = CARTESIAN_POINT ( 'NONE',  ( 6.639320575229252341, 0.005161017367553630275, 1.896863882003448021 ) ) ;
#4148 = ORIENTED_EDGE ( 'NONE', *, *, #189189, .F. ) ;
#4147 = CARTESIAN_POINT ( 'NONE',  ( 2.969872605471133742, 6.610326516918480166, 0.1088621377024363707 ) ) ;
#4149 = CARTESIAN_POINT ( 'NONE',  ( 1.551402291579254022, 0.5461136009352780540, -1.789155053659279071 ) ) ;
#4150 = CARTESIAN_POINT ( 'NONE',  ( 3.538296236868877731, 0.7303062672313584969, 1.879804216660937666 ) ) ;
#4152 = DIRECTION ( 'NONE',  ( 0.000000000000000000, 0.000000000000000000, -1.000000000000000000 ) ) ;
#4151 = CARTESIAN_POINT ( 'NONE',  ( 1.364683531249988535, 1.363541667008083769, 0.7879004041258500513 ) ) ;
#4154 = CARTESIAN_POINT ( 'NONE',  ( 4.688165273298999125, -0.9932770932522380081, 1.857119049063939320 ) ) ;
#4153 = CARTESIAN_POINT ( 'NONE',  ( -6.353967546298838087, 10.56471257065732416, 0.000000000000000000 ) ) ;
#4155 = CARTESIAN_POINT ( 'NONE',  ( 7.253775878511261155, 8.421492265473332850, 1.199719254218462483 ) ) ;
#4157 = CARTESIAN_POINT ( 'NONE',  ( -6.353967546298838087, 10.56471257065732416, 0.000000000000000000 ) ) ;
#4156 = CARTESIAN_POINT ( 'NONE',  ( 4.386945222473598527, 7.275797305264619652, -1.199719254218452047 ) ) ;
#4158 = CARTESIAN_POINT ( 'NONE',  ( 1.264911064067342217, 3.850000000000006306, -0.4999999999999987232 ) ) ;
#4159 = CARTESIAN_POINT ( 'NONE',  ( 4.992447118679333329, -1.118567257517719460, 1.681552772592603384 ) ) ;
#4160 = CARTESIAN_POINT ( 'NONE',  ( -1.402160292154681736E-14, -0.8812499993171809543, -1.732050807568870754 ) ) ;
#4161 = CARTESIAN_POINT ( 'NONE',  ( 0.9188877648007650611, -1.496628706349166338, 1.419512306474308261 ) ) ;
#4162 = CARTESIAN_POINT ( 'NONE',  ( 7.443063144222396232, 11.62739806832741785, 1.040834085586084257E-14 ) ) ;
#4163 = CARTESIAN_POINT ( 'NONE',  ( 5.571600594950134600, 2.084881007647599205, -0.5705972643132785072 ) ) ;
#4164 = CARTESIAN_POINT ( 'NONE',  ( 4.877901405866606588, 8.912911750144889567, 0.7998128361456341429 ) ) ;
#4165 = CARTESIAN_POINT ( 'NONE',  ( -0.6823417656250003738, -0.9697916663252494907, -1.181850606188749264 ) ) ;
#4166 = CARTESIAN_POINT ( 'NONE',  ( 4.342354338126830804, 8.288106837781779035, -0.7998128361456381397 ) ) ;
#4167 = CARTESIAN_POINT ( 'NONE',  ( 7.253248993186720561, 10.44557901115111065, 1.082531754730558626 ) ) ;
#4169 = DIRECTION ( 'NONE',  ( 1.224643483124941457E-16, 0.002327115863041261980, 0.9999972922622142324 ) ) ;
#4168 = CARTESIAN_POINT ( 'NONE',  ( 3.279888855285200577, -2.093262694144955027, 0.5762538248230695270 ) ) ;
#4171 = CARTESIAN_POINT ( 'NONE',  ( 1.891909123491273492, -0.4922293657834125313, -1.774144672653771293 ) ) ;
#4170 = CARTESIAN_POINT ( 'NONE',  ( -5.639828713604883248, 6.642516923036197340, 1.082531754730548412 ) ) ;
#4172 = EDGE_CURVE ( 'NONE', #157711, #182623, #58845, .T. ) ;
#4173 = CARTESIAN_POINT ( 'NONE',  ( -0.6823417656250212460, 3.051041667008084879, 1.181850606188767472 ) ) ;
#4174 = CARTESIAN_POINT ( 'NONE',  ( 4.353197867323560288, 0.4795420089713005041, -2.138300074133951068 ) ) ;
#4175 = CARTESIAN_POINT ( 'NONE',  ( 6.883263157960341161, 7.051904271082326758, 2.751962465287846271 ) ) ;
#4176 = CARTESIAN_POINT ( 'NONE',  ( 4.680719170653036443, -2.193521624435289752, -0.5540208151394544478 ) ) ;
#4177 = CARTESIAN_POINT ( 'NONE',  ( -5.194745412330402878, 9.212286747694129474, 0.000000000000000000 ) ) ;
#4178 = CARTESIAN_POINT ( 'NONE',  ( 11.41381675112453387, 12.69999999999998153, 3.704697986577180746 ) ) ;
#4179 = CARTESIAN_POINT ( 'NONE',  ( 4.807910157829258679, 8.239027388120819140, -0.8806314816870459694 ) ) ;
#4180 = CARTESIAN_POINT ( 'NONE',  ( -0.7500000000000179856, 13.79166666666666785, 1.299038105676658228 ) ) ;
#4181 = CARTESIAN_POINT ( 'NONE',  ( -6.753369912938502750, 7.051555451282599307, 0.000000000000000000 ) ) ;
#4182 = CARTESIAN_POINT ( 'NONE',  ( 5.722950238744200391, 7.770137593325314285, 1.443375672974065660 ) ) ;
#4183 = CARTESIAN_POINT ( 'NONE',  ( 5.589024195967314590, 1.560314836579352438, -0.8350092274562578298 ) ) ;
#4184 = CARTESIAN_POINT ( 'NONE',  ( 7.584896871841365851, 10.93646455286856956, -1.199719254218446718 ) ) ;
#4185 = CARTESIAN_POINT ( 'NONE',  ( 2.116374960856721277, -0.9918371849380368532, -1.857756019195427877 ) ) ;
#4186 =( GEOMETRIC_REPRESENTATION_CONTEXT ( 3 ) GLOBAL_UNCERTAINTY_ASSIGNED_CONTEXT ( ( #153294 ) ) GLOBAL_UNIT_ASSIGNED_CONTEXT ( ( #105235, #6623, #42376 ) ) REPRESENTATION_CONTEXT ( 'NONE', 'WORKASPACE' ) );
#4188 = CARTESIAN_POINT ( 'NONE',  ( -1.500000000000013101, 1.920833333333356263, 0.8660254037844403729 ) ) ;
#4187 = CARTESIAN_POINT ( 'NONE',  ( -8.012344526598182026E-15, 11.29687500034139980, -1.575800808251669460 ) ) ;
#4189 = CARTESIAN_POINT ( 'NONE',  ( 2.348051406654600104, -0.8447338538565999366, 1.779358369178071886 ) ) ;
#4190 = CARTESIAN_POINT ( 'NONE',  ( 0.000000000000000000, -7.666862915010147717, 0.000000000000000000 ) ) ;
#4191 = CARTESIAN_POINT ( 'NONE',  ( 3.697477691155363289, 7.355658039646863600, 0.1550784054364961473 ) ) ;
#4193 = ORIENTED_EDGE ( 'NONE', *, *, #105660, .F. ) ;
#4192 = CARTESIAN_POINT ( 'NONE',  ( 5.730666697864316816, 1.210223194361861543, -1.348246716841319692 ) ) ;
#4194 = CARTESIAN_POINT ( 'NONE',  ( 5.287316719649520991, 8.151991358691011769, -1.082531754730549078 ) ) ;
#4195 = CARTESIAN_POINT ( 'NONE',  ( 1.364683531249984538, -1.032291666325247714, -0.7879004041258309554 ) ) ;
#4196 = CARTESIAN_POINT ( 'NONE',  ( 5.981297838379463272, 1.727768277425823396, -0.7175292643646775659 ) ) ;
#4197 = CARTESIAN_POINT ( 'NONE',  ( 3.891353782322113375, 4.498666486585943147, -1.199719254218446718 ) ) ;
#4198 = CARTESIAN_POINT ( 'NONE',  ( 5.348515126027269417, -2.053966340784090239, -0.2589089449258550890 ) ) ;
#4199 = CARTESIAN_POINT ( 'NONE',  ( 1.224999999999995204, 2.875000000000002665, 0.000000000000000000 ) ) ;
#4201 = EDGE_CURVE ( 'NONE', #168636, #175139, #105282, .T. ) ;
#4200 =( BOUNDED_SURFACE ( )  B_SPLINE_SURFACE ( 1, 2, ( 
 ( #106976, #176197, #23515, #156751, #92826, #174080, #142651, #206537, #192413, #110187, #93896, #25651, #140524, #40871, #173001, #61370, #205469, #58167, #39788, #8339, #158870, #89621, #155673, #73331, #57101, #123269, #189232, #24582, #41942, #108055, #91762, #157817, #47274, #64562, #129654, #131739, #98153, #32064, #63501, #48337, #115501, #213970, #195639, #81872, #13667, #65590, #147957, #197744, #46202, #28870, #149002, #112318, #62428, #49382, #113387, #78670, #181496, #196697, #164199, #163143, #130706, #96027, #33124, #99203, #162078, #29941, #165253, #578, #16846, #114448, #82929, #66644, #12597, #161003, #193500, #178333, #179396, #94955, #45141, #15787, #111253, #177256, #144796, #212927, #210803, #128591, #194557, #79739, #145856, #180447, #31016, #211862, #97090, #80819, #14727, #146908, #170577, #103454, #3777, #102380, #17907, #152207, #137029, #203055, #52565, #135961, #150082, #132789, #88273, #83993, #101310, #1652, #198791, #69851, #116560, #2719, #50441, #18981, #201977, #85064, #67710, #184682, #199868, #118696, #117636, #54699, #183628, #133860, #51511, #120850, #182553, #35235, #53633, #36303, #21097, #119766, #168449, #167391, #185745, #186823, #38453, #20048, #37379, #151149, #34177, #154340, #68791, #134910, #200918, #100249, #169515, #166318, #86136, #87200, #153264, #4840, #70918, #104531, #22159, #5916, #57900, #56837, #76286, #123008, #89354, #139165, #208403, #204112, #188962, #75227, #206278, #174883, #125127, #40603, #55764, #106709, #73066, #207352, #60037, #74163, #24311, #172735, #93631, #8075, #140255, #155403, #6986, #205196, #25397, #156486, #105615, #142395, #92572, #90417, #121921, #23242, #124065, #190030, #157557, #41683, #10212, #191085, #42754, #107794, #141338, #126190, #158615, #173819, #26464, #91497, #192152, #43816, #109930, #9151, #187888, #27536, #58972, #108858, #175940, #159673, #171645, #71990, #138101, #39517, #195381, #162886, #128340, #180199, #31821, #194306, #62183, #97897, #181247, #163956, #80557, #15534, #131491, #44885, #193238, #65344, #210547 ),
 ( #197495, #94702, #61107, #130456, #114201, #129401, #160743, #64311, #145608, #127266, #196444, #48089, #176996, #110991, #45947, #81618, #147702, #112067, #178068, #213720, #32874, #49138, #146656, #115254, #98951, #28612, #12337, #11275, #29685, #95769, #78418, #77354, #143467, #209463, #144538, #161824, #30758, #13413, #79488, #211603, #63239, #47012, #212670, #113128, #179133, #96837, #14468, #51263, #68545, #185508, #102141, #134674, #18736, #132548, #2470, #69612, #135720, #34990, #200677, #50195, #165002, #169273, #198547, #1408, #182305, #82678, #52326, #148761, #117388, #330, #67468, #118456, #133616, #33932, #167149, #166073, #101061, #83745, #201744, #149838, #116314, #100008, #53385, #66403, #199618, #184442, #84820, #19807, #36060, #17661, #183384, #150908, #168208, #85891, #119521, #151968, #3540, #37131, #20859, #103211, #16595, #161462, #13042, #79121, #97532, #14098, #177706, #148403, #164641, #145237, #61814, #95410, #62867, #212305, #15172, #80188, #82308, #48769, #197131, #146293, #213366, #66032, #16225, #63940, #32505, #178778, #214402, #98580, #132180, #211242, #193935, #99637, #129034, #195010, #198186, #130094, #29316, #49821, #147337, #114884, #113838, #81259, #196089, #47721, #46643, #112765, #30390, #163589, #179834, #96478, #115946, #181935, #162525, #127982, #31455, #64987, #131142, #180883, #33566, #165705, #17294, #144183, #210174, #45582, #111699, #106892, #19433, #186201, #118086, #172919, #40787, #24494, #150536, #133237, #41862, #2099, #166775, #90605, #85513, #183011, #156665, #86584, #202436, #53013, #20499, #200312, #8257, #74340, #51963, #134304, #140444, #107972, #206455, #152650, #58082, #124244, #117012, #50889, #190203, #68174, #167835, #199242, #174000, #54090, #1038, #83371, #34628, #102840, #149455, #100698, #18371, #67101, #84448, #4234, #151599, #120228, #184072, #185129, #3167, #168896, #35691, #101767, #70304, #119147, #69238, #136420, #135355, #201372, #36754, #98736, #163743, #179987, #32657, #164793, #178932, #15322, #2256, #34777, #212457, #162680, #132333 ) ),
 .UNSPECIFIED., .F., .F., .T. ) 
 B_SPLINE_SURFACE_WITH_KNOTS ( ( 2, 2 ),
 ( 3, 2, 2, 2, 2, 2, 2, 2, 2, 2, 2, 2, 2, 2, 2, 2, 2, 2, 2, 2, 2, 2, 2, 2, 2, 2, 2, 2, 2, 2, 2, 2, 2, 2, 2, 2, 2, 2, 2, 2, 2, 2, 2, 2, 2, 2, 2, 2, 2, 2, 2, 2, 2, 2, 2, 2, 2, 2, 2, 2, 2, 2, 2, 2, 2, 2, 2, 2, 2, 2, 2, 2, 2, 2, 2, 2, 2, 2, 2, 2, 2, 2, 2, 2, 2, 2, 2, 2, 2, 2, 2, 2, 2, 2, 2, 2, 2, 2, 2, 2, 2, 2, 2, 2, 2, 2, 2, 2, 2, 2, 2, 2, 2, 2, 2, 2, 2, 2, 2, 2, 3 ),
 ( 0.000000000000000000, 1.000000000000000000 ),
 ( 0.000000000000000000, 0.008333333333333333218, 0.01666666666666666644, 0.02500000000000000139, 0.03333333333333333287, 0.04166666666666666435, 0.05000000000000000278, 0.05833333333333333426, 0.06666666666666666574, 0.07499999999999999722, 0.08333333333333332871, 0.09166666666666666019, 0.1000000000000000056, 0.1083333333333333370, 0.1166666666666666685, 0.1250000000000000000, 0.1333333333333333315, 0.1416666666666666630, 0.1499999999999999944, 0.1583333333333333259, 0.1666666666666666574, 0.1749999999999999889, 0.1833333333333333204, 0.1916666666666666796, 0.2000000000000000111, 0.2083333333333333426, 0.2166666666666666741, 0.2250000000000000056, 0.2333333333333333370, 0.2416666666666666685, 0.2500000000000000000, 0.2583333333333333592, 0.2666666666666666630, 0.2750000000000000222, 0.2833333333333333259, 0.2916666666666666852, 0.2999999999999999889, 0.3083333333333333481, 0.3166666666666666519, 0.3250000000000000111, 0.3333333333333333148, 0.3416666666666666741, 0.3499999999999999778, 0.3583333333333333370, 0.3666666666666666408, 0.3750000000000000000, 0.3833333333333333592, 0.3916666666666666630, 0.4000000000000000222, 0.4083333333333333259, 0.4166666666666666852, 0.4249999999999999889, 0.4333333333333333481, 0.4416666666666666519, 0.4500000000000000111, 0.4583333333333333148, 0.4666666666666666741, 0.4749999999999999778, 0.4833333333333333370, 0.4916666666666666408, 0.5000000000000000000, 0.5083333333333333037, 0.5166666666666667185, 0.5250000000000000222, 0.5333333333333333259, 0.5416666666666666297, 0.5500000000000000444, 0.5583333333333333481, 0.5666666666666666519, 0.5749999999999999556, 0.5833333333333333703, 0.5916666666666666741, 0.5999999999999999778, 0.6083333333333332815, 0.6166666666666666963, 0.6250000000000000000, 0.6333333333333333037, 0.6416666666666667185, 0.6500000000000000222, 0.6583333333333333259, 0.6666666666666666297, 0.6750000000000000444, 0.6833333333333333481, 0.6916666666666666519, 0.6999999999999999556, 0.7083333333333333703, 0.7166666666666666741, 0.7249999999999999778, 0.7333333333333332815, 0.7416666666666666963, 0.7500000000000000000, 0.7583333333333333037, 0.7666666666666667185, 0.7750000000000000222, 0.7833333333333333259, 0.7916666666666666297, 0.8000000000000000444, 0.8083333333333333481, 0.8166666666666666519, 0.8249999999999999556, 0.8333333333333333703, 0.8416666666666666741, 0.8499999999999999778, 0.8583333333333332815, 0.8666666666666666963, 0.8750000000000000000, 0.8833333333333333037, 0.8916666666666667185, 0.9000000000000000222, 0.9083333333333333259, 0.9166666666666666297, 0.9250000000000000444, 0.9333333333333333481, 0.9416666666666666519, 0.9499999999999999556, 0.9583333333333333703, 0.9666666666666666741, 0.9749999999999999778, 0.9833333333333332815, 0.9916666666666666963, 1.000000000000000000 ),
 .UNSPECIFIED. ) 
 GEOMETRIC_REPRESENTATION_ITEM ( )  RATIONAL_B_SPLINE_SURFACE ( (
 ( 1.000000000000000000, 0.8660254037844387076, 1.000000000000000000, 0.8660254037844387076, 1.000000000000000000, 0.8660254037844387076, 1.000000000000000000, 0.8660254037844387076, 1.000000000000000000, 0.8660254037844387076, 1.000000000000000000, 0.8660254037844387076, 1.000000000000000000, 0.8660254037844387076, 1.000000000000000000, 0.8660254037844387076, 1.000000000000000000, 0.8660254037844387076, 1.000000000000000000, 0.8660254037844387076, 1.000000000000000000, 0.8660254037844387076, 1.000000000000000000, 0.8660254037844387076, 1.000000000000000000, 0.8660254037844387076, 1.000000000000000000, 0.8660254037844387076, 1.000000000000000000, 0.8660254037844387076, 1.000000000000000000, 0.8660254037844387076, 1.000000000000000000, 0.8660254037844387076, 1.000000000000000000, 0.8660254037844387076, 1.000000000000000000, 0.8660254037844387076, 1.000000000000000000, 0.8660254037844387076, 1.000000000000000000, 0.8660254037844387076, 1.000000000000000000, 0.8660254037844387076, 1.000000000000000000, 0.8660254037844387076, 1.000000000000000000, 0.8660254037844387076, 1.000000000000000000, 0.8660254037844387076, 1.000000000000000000, 0.8660254037844387076, 1.000000000000000000, 0.8660254037844387076, 1.000000000000000000, 0.8660254037844387076, 1.000000000000000000, 0.8660254037844387076, 1.000000000000000000, 0.8660254037844387076, 1.000000000000000000, 0.8660254037844387076, 1.000000000000000000, 0.8660254037844387076, 1.000000000000000000, 0.8660254037844387076, 1.000000000000000000, 0.8660254037844387076, 1.000000000000000000, 0.8660254037844387076, 1.000000000000000000, 0.8660254037844387076, 1.000000000000000000, 0.8660254037844387076, 1.000000000000000000, 0.8660254037844387076, 1.000000000000000000, 0.8660254037844387076, 1.000000000000000000, 0.8660254037844387076, 1.000000000000000000, 0.8660254037844387076, 1.000000000000000000, 0.8660254037844387076, 1.000000000000000000, 0.8660254037844387076, 1.000000000000000000, 0.8660254037844387076, 1.000000000000000000, 0.8660254037844387076, 1.000000000000000000, 0.8660254037844387076, 1.000000000000000000, 0.8660254037844387076, 1.000000000000000000, 0.8660254037844387076, 1.000000000000000000, 0.8660254037844387076, 1.000000000000000000, 0.8660254037844387076, 1.000000000000000000, 0.8660254037844387076, 1.000000000000000000, 0.8660254037844387076, 1.000000000000000000, 0.8660254037844387076, 1.000000000000000000, 0.8660254037844387076, 1.000000000000000000, 0.8660254037844387076, 1.000000000000000000, 0.8660254037844387076, 1.000000000000000000, 0.8660254037844387076, 1.000000000000000000, 0.8660254037844387076, 1.000000000000000000, 0.8660254037844387076, 1.000000000000000000, 0.8660254037844387076, 1.000000000000000000, 0.8660254037844387076, 1.000000000000000000, 0.8660254037844387076, 1.000000000000000000, 0.8660254037844387076, 1.000000000000000000, 0.8660254037844387076, 1.000000000000000000, 0.8660254037844387076, 1.000000000000000000, 0.8660254037844387076, 1.000000000000000000, 0.8660254037844387076, 1.000000000000000000, 0.8660254037844387076, 1.000000000000000000, 0.8660254037844387076, 1.000000000000000000, 0.8660254037844387076, 1.000000000000000000, 0.8660254037844387076, 1.000000000000000000, 0.8660254037844387076, 1.000000000000000000, 0.8660254037844387076, 1.000000000000000000, 0.8660254037844387076, 1.000000000000000000, 0.8660254037844387076, 1.000000000000000000, 0.8660254037844387076, 1.000000000000000000, 0.8660254037844387076, 1.000000000000000000, 0.8660254037844387076, 1.000000000000000000, 0.8660254037844387076, 1.000000000000000000, 0.8660254037844387076, 1.000000000000000000, 0.8660254037844387076, 1.000000000000000000, 0.8660254037844387076, 1.000000000000000000, 0.8660254037844387076, 1.000000000000000000, 0.8660254037844387076, 1.000000000000000000, 0.8660254037844387076, 1.000000000000000000, 0.8660254037844387076, 1.000000000000000000, 0.8660254037844387076, 1.000000000000000000, 0.8660254037844387076, 1.000000000000000000, 0.8660254037844387076, 1.000000000000000000, 0.8660254037844387076, 1.000000000000000000, 0.8660254037844387076, 1.000000000000000000, 0.8660254037844387076, 1.000000000000000000, 0.8660254037844387076, 1.000000000000000000, 0.8660254037844387076, 1.000000000000000000, 0.8660254037844387076, 1.000000000000000000, 0.8660254037844387076, 1.000000000000000000, 0.8660254037844387076, 1.000000000000000000, 0.8660254037844387076, 1.000000000000000000, 0.8660254037844387076, 1.000000000000000000, 0.8660254037844387076, 1.000000000000000000, 0.8660254037844387076, 1.000000000000000000, 0.8660254037844387076, 1.000000000000000000, 0.8660254037844387076, 1.000000000000000000, 0.8660254037844387076, 1.000000000000000000, 0.8660254037844387076, 1.000000000000000000, 0.8660254037844387076, 1.000000000000000000, 0.8660254037844387076, 1.000000000000000000, 0.8660254037844387076, 1.000000000000000000, 0.8660254037844387076, 1.000000000000000000, 0.8660254037844387076, 1.000000000000000000, 0.8660254037844387076, 1.000000000000000000, 0.8660254037844387076, 1.000000000000000000, 0.8660254037844387076, 1.000000000000000000, 0.8660254037844387076, 1.000000000000000000, 0.8660254037844387076, 1.000000000000000000, 0.8660254037844387076, 1.000000000000000000, 0.8660254037844387076, 1.000000000000000000, 0.8660254037844387076, 1.000000000000000000, 0.8660254037844387076, 1.000000000000000000, 0.8660254037844387076, 1.000000000000000000),
 ( 1.000000000000000000, 0.8660254037844387076, 1.000000000000000000, 0.8660254037844387076, 1.000000000000000000, 0.8660254037844387076, 1.000000000000000000, 0.8660254037844387076, 1.000000000000000000, 0.8660254037844387076, 1.000000000000000000, 0.8660254037844387076, 1.000000000000000000, 0.8660254037844387076, 1.000000000000000000, 0.8660254037844387076, 1.000000000000000000, 0.8660254037844387076, 1.000000000000000000, 0.8660254037844387076, 1.000000000000000000, 0.8660254037844387076, 1.000000000000000000, 0.8660254037844387076, 1.000000000000000000, 0.8660254037844387076, 1.000000000000000000, 0.8660254037844387076, 1.000000000000000000, 0.8660254037844387076, 1.000000000000000000, 0.8660254037844387076, 1.000000000000000000, 0.8660254037844387076, 1.000000000000000000, 0.8660254037844387076, 1.000000000000000000, 0.8660254037844387076, 1.000000000000000000, 0.8660254037844387076, 1.000000000000000000, 0.8660254037844387076, 1.000000000000000000, 0.8660254037844387076, 1.000000000000000000, 0.8660254037844387076, 1.000000000000000000, 0.8660254037844387076, 1.000000000000000000, 0.8660254037844387076, 1.000000000000000000, 0.8660254037844387076, 1.000000000000000000, 0.8660254037844387076, 1.000000000000000000, 0.8660254037844387076, 1.000000000000000000, 0.8660254037844387076, 1.000000000000000000, 0.8660254037844387076, 1.000000000000000000, 0.8660254037844387076, 1.000000000000000000, 0.8660254037844387076, 1.000000000000000000, 0.8660254037844387076, 1.000000000000000000, 0.8660254037844387076, 1.000000000000000000, 0.8660254037844387076, 1.000000000000000000, 0.8660254037844387076, 1.000000000000000000, 0.8660254037844387076, 1.000000000000000000, 0.8660254037844387076, 1.000000000000000000, 0.8660254037844387076, 1.000000000000000000, 0.8660254037844387076, 1.000000000000000000, 0.8660254037844387076, 1.000000000000000000, 0.8660254037844387076, 1.000000000000000000, 0.8660254037844387076, 1.000000000000000000, 0.8660254037844387076, 1.000000000000000000, 0.8660254037844387076, 1.000000000000000000, 0.8660254037844387076, 1.000000000000000000, 0.8660254037844387076, 1.000000000000000000, 0.8660254037844387076, 1.000000000000000000, 0.8660254037844387076, 1.000000000000000000, 0.8660254037844387076, 1.000000000000000000, 0.8660254037844387076, 1.000000000000000000, 0.8660254037844387076, 1.000000000000000000, 0.8660254037844387076, 1.000000000000000000, 0.8660254037844387076, 1.000000000000000000, 0.8660254037844387076, 1.000000000000000000, 0.8660254037844387076, 1.000000000000000000, 0.8660254037844387076, 1.000000000000000000, 0.8660254037844387076, 1.000000000000000000, 0.8660254037844387076, 1.000000000000000000, 0.8660254037844387076, 1.000000000000000000, 0.8660254037844387076, 1.000000000000000000, 0.8660254037844387076, 1.000000000000000000, 0.8660254037844387076, 1.000000000000000000, 0.8660254037844387076, 1.000000000000000000, 0.8660254037844387076, 1.000000000000000000, 0.8660254037844387076, 1.000000000000000000, 0.8660254037844387076, 1.000000000000000000, 0.8660254037844387076, 1.000000000000000000, 0.8660254037844387076, 1.000000000000000000, 0.8660254037844387076, 1.000000000000000000, 0.8660254037844387076, 1.000000000000000000, 0.8660254037844387076, 1.000000000000000000, 0.8660254037844387076, 1.000000000000000000, 0.8660254037844387076, 1.000000000000000000, 0.8660254037844387076, 1.000000000000000000, 0.8660254037844387076, 1.000000000000000000, 0.8660254037844387076, 1.000000000000000000, 0.8660254037844387076, 1.000000000000000000, 0.8660254037844387076, 1.000000000000000000, 0.8660254037844387076, 1.000000000000000000, 0.8660254037844387076, 1.000000000000000000, 0.8660254037844387076, 1.000000000000000000, 0.8660254037844387076, 1.000000000000000000, 0.8660254037844387076, 1.000000000000000000, 0.8660254037844387076, 1.000000000000000000, 0.8660254037844387076, 1.000000000000000000, 0.8660254037844387076, 1.000000000000000000, 0.8660254037844387076, 1.000000000000000000, 0.8660254037844387076, 1.000000000000000000, 0.8660254037844387076, 1.000000000000000000, 0.8660254037844387076, 1.000000000000000000, 0.8660254037844387076, 1.000000000000000000, 0.8660254037844387076, 1.000000000000000000, 0.8660254037844387076, 1.000000000000000000, 0.8660254037844387076, 1.000000000000000000, 0.8660254037844387076, 1.000000000000000000, 0.8660254037844387076, 1.000000000000000000, 0.8660254037844387076, 1.000000000000000000, 0.8660254037844387076, 1.000000000000000000, 0.8660254037844387076, 1.000000000000000000, 0.8660254037844387076, 1.000000000000000000, 0.8660254037844387076, 1.000000000000000000, 0.8660254037844387076, 1.000000000000000000, 0.8660254037844387076, 1.000000000000000000, 0.8660254037844387076, 1.000000000000000000, 0.8660254037844387076, 1.000000000000000000, 0.8660254037844387076, 1.000000000000000000, 0.8660254037844387076, 1.000000000000000000, 0.8660254037844387076, 1.000000000000000000, 0.8660254037844387076, 1.000000000000000000, 0.8660254037844387076, 1.000000000000000000, 0.8660254037844387076, 1.000000000000000000, 0.8660254037844387076, 1.000000000000000000, 0.8660254037844387076, 1.000000000000000000, 0.8660254037844387076, 1.000000000000000000, 0.8660254037844387076, 1.000000000000000000, 0.8660254037844387076, 1.000000000000000000, 0.8660254037844387076, 1.000000000000000000, 0.8660254037844387076, 1.000000000000000000, 0.8660254037844387076, 1.000000000000000000) ) ) 
 REPRESENTATION_ITEM ( '' )  SURFACE ( )  );
#4202 = CARTESIAN_POINT ( 'NONE',  ( -4.868786560638931782, 6.773613302202437403, 1.443375672974058777 ) ) ;
#4203 = CARTESIAN_POINT ( 'NONE',  ( 1.489652919843037271, -0.9674398443463784192, 3.089271823530293393 ) ) ;
#4204 = CARTESIAN_POINT ( 'NONE',  ( -0.7500000000000006661, 1.108333333333356929, -1.299038105676652011 ) ) ;
#4205 = CARTESIAN_POINT ( 'NONE',  ( 7.401861798056875053, 10.72292363345333399, -1.199719254218441611 ) ) ;
#4206 = CARTESIAN_POINT ( 'NONE',  ( -7.804689982961090955, 12.25722208009664094, 0.7998128361456481317 ) ) ;
#4207 = CARTESIAN_POINT ( 'NONE',  ( 5.180097208873055692, 8.201141289397330780, -1.199719254218450271 ) ) ;
#4208 = CARTESIAN_POINT ( 'NONE',  ( -0.6823417656250003738, -0.5322916663252491576, -1.181850606188749264 ) ) ;
#4209 = CARTESIAN_POINT ( 'NONE',  ( -1.500000000000013101, 1.379166666666689745, -0.8660254037844313801 ) ) ;
#4211 = CARTESIAN_POINT ( 'NONE',  ( 5.443762371086860341, 6.309809840144842141, 1.199719254218462483 ) ) ;
#4210 = CARTESIAN_POINT ( 'NONE',  ( 5.336364984333265227, -1.091323163865608459, 1.630109012322231266 ) ) ;
#4212 = CARTESIAN_POINT ( 'NONE',  ( 3.497422563753574298, 1.966343570655813666, 0.4444343670074250574 ) ) ;
#4213 = CARTESIAN_POINT ( 'NONE',  ( 2.835059001918965649, -1.568902116443865236, -1.099054045514812117 ) ) ;
#4214 = CARTESIAN_POINT ( 'NONE',  ( -0.1108833634136975610, 0.7331455517814323697, -1.980187714524218823 ) ) ;
#4215 = CARTESIAN_POINT ( 'NONE',  ( 0.2752733618501881363, 2.042644424557562122, -0.7945232813236638991 ) ) ;
#4216 = CARTESIAN_POINT ( 'NONE',  ( 0.1331715793776600265, 2.877549198462618474, -2.442236402435117526 ) ) ;
#4217 = CARTESIAN_POINT ( 'NONE',  ( 2.547943918863291302, 1.870051909910470878, 0.05015897750767356333 ) ) ;
#4218 = CARTESIAN_POINT ( 'NONE',  ( -1.364683531250010295, 5.530208333674751842, 0.7879004041258379498 ) ) ;
#4219 = CARTESIAN_POINT ( 'NONE',  ( 4.148693527746351251, 1.975194156771160170, 0.3885511358477158894 ) ) ;
#4220 = CARTESIAN_POINT ( 'NONE',  ( -8.843996274815957293, 9.212417163573759282, 1.040834085586084257E-14 ) ) ;
#4222 = CARTESIAN_POINT ( 'NONE',  ( 4.974263482967073990, -2.101360013415910721, -0.2580830166784564006 ) ) ;
#4221 = CARTESIAN_POINT ( 'NONE',  ( -5.016153647376219382, 6.875265226737464985, 1.443375672974064550 ) ) ;
#4223 = CARTESIAN_POINT ( 'NONE',  ( 6.531696417657103737, 1.982406992490031383, -0.5971068152322634992 ) ) ;
#4225 = CARTESIAN_POINT ( 'NONE',  ( 4.040754838981084340, 7.538853419981225379, -0.4347147375480670539 ) ) ;
#4224 = CARTESIAN_POINT ( 'NONE',  ( 0.7672655991019157184, 2.013871065616902989, -0.5614242917610365868 ) ) ;
#4227 = ORIENTED_EDGE ( 'NONE', *, *, #28879, .T. ) ;
#4226 = CARTESIAN_POINT ( 'NONE',  ( 6.247073575888860475, -1.540555741078741825, 0.9791950884799265342 ) ) ;
#4228 = CARTESIAN_POINT ( 'NONE',  ( 6.740374924288304648, 11.01552117831172062, 1.040834085586084257E-14 ) ) ;
#4229 = CARTESIAN_POINT ( 'NONE',  ( -4.456559383047711265, 7.083366476587958260, -1.119882773345021842 ) ) ;
#4230 = VECTOR ( 'NONE', #185116, 1000.000000000000114 ) ;
#4232 = CARTESIAN_POINT ( 'NONE',  ( 6.602457619730760285, 8.725953194484466380, 1.443375672974076540 ) ) ;
#4231 = CARTESIAN_POINT ( 'NONE',  ( 6.795661308947685164, 8.951357498570873261, -1.599625672291262513 ) ) ;
#4233 = CARTESIAN_POINT ( 'NONE',  ( -0.6823417656250039265, 13.13020833367473017, -1.181850606188755259 ) ) ;
#4235 = CARTESIAN_POINT ( 'NONE',  ( 0.5393639851597960000, -1.720521155456521400, 0.5669088471357224268 ) ) ;
#4234 = CARTESIAN_POINT ( 'NONE',  ( 6.749980374757213575, 8.968339418673846097, 1.599625672291268286 ) ) ;
#4236 = CARTESIAN_POINT ( 'NONE',  ( -9.020252271793614440, 9.418049160047695878, 0.7998128361456462443 ) ) ;
#4237 = CARTESIAN_POINT ( 'NONE',  ( 5.518332215962025167, 6.396807992499198292, -1.199719254218445830 ) ) ;
#4238 = CARTESIAN_POINT ( 'NONE',  ( 0.01400375820003852204, -6.304807775344445808, 11.00039779440905896 ) ) ;
#4239 = CARTESIAN_POINT ( 'NONE',  ( 4.065672160753666553, 7.505179260319745360, -0.5311146244057519672 ) ) ;
#4240 = CARTESIAN_POINT ( 'NONE',  ( 10.56143847536557878, 11.42402576412244386, 0.000000000000000000 ) ) ;
#4241 = ORIENTED_EDGE ( 'NONE', *, *, #201124, .T. ) ;
#4242 = CARTESIAN_POINT ( 'NONE',  ( 6.151970292378349470, 1.039009440890667824, 1.727993850779283802 ) ) ;
#4243 = CARTESIAN_POINT ( 'NONE',  ( 0.6805317496583452863, 1.048634805427307359, 1.842989218901350812 ) ) ;
#4244 = CARTESIAN_POINT ( 'NONE',  ( 1.284915497622363123, -5.970188836749928864E-15, -0.3104282545687488959 ) ) ;
#4245 = VECTOR ( 'NONE', #197041, 1000.000000000000227 ) ;
#4246 = AXIS2_PLACEMENT_3D ( 'NONE', #61852, #191832, #43495 ) ;
#4247 = CARTESIAN_POINT ( 'NONE',  ( 0.1405533004714175083, 0.2365636613079393491, -2.314604644119310439 ) ) ;
#4248 = CARTESIAN_POINT ( 'NONE',  ( 1.807716826991497161, 2.517780620582467765, 2.499994708711101854 ) ) ;
#4249 = CARTESIAN_POINT ( 'NONE',  ( -3.578989364327652467, 6.158942777482099729, 1.082531754730560403 ) ) ;
#4250 = CARTESIAN_POINT ( 'NONE',  ( 9.951321562750607086, 11.67259191370631477, -1.082531754730537088 ) ) ;
#4251 = CARTESIAN_POINT ( 'NONE',  ( 3.080859285270169057, 1.852775266960526412, 0.6680929264101590492 ) ) ;
#4252 = CARTESIAN_POINT ( 'NONE',  ( 4.341422844945469706, 0.4390097190783425196, -1.967893369681630311 ) ) ;
#4253 = CARTESIAN_POINT ( 'NONE',  ( -6.718228810771495141, 7.796687353110217877, 1.199719254218450271 ) ) ;
#4254 = LINE ( 'NONE', #106106, #38900 ) ;
#4255 = CARTESIAN_POINT ( 'NONE',  ( 5.314472526525434226, 2.023830839259177949, 0.8410439265160507549 ) ) ;
#4256 = CARTESIAN_POINT ( 'NONE',  ( 5.427887300360813683, 4.356806483369909166, 2.440341253675380351 ) ) ;
#4257 = CARTESIAN_POINT ( 'NONE',  ( 3.575144680771982220, 0.04857402364528973226, -1.925943534667476476 ) ) ;
#4258 = CARTESIAN_POINT ( 'NONE',  ( -7.507464373665155399, 9.781794407407920389, 1.599625672291295375 ) ) ;
#4259 = CARTESIAN_POINT ( 'NONE',  ( -0.02968770228137587730, 6.948707269782667062, -2.421356871654921417 ) ) ;
#4260 = CARTESIAN_POINT ( 'NONE',  ( 0.1333542156527140476, 0.7077123155428012291, -2.127987941987404596 ) ) ;
#4261 = CARTESIAN_POINT ( 'NONE',  ( 7.084367489069545069E-14, 8.210952333604106812, 2.038660652713624177 ) ) ;
#4262 = ORIENTED_EDGE ( 'NONE', *, *, #73605, .F. ) ;
#4263 = CARTESIAN_POINT ( 'NONE',  ( 4.963693636378940788, 5.923969009597785274, -1.082531754730548412 ) ) ;
#4264 = CARTESIAN_POINT ( 'NONE',  ( 5.049637312653283416, 1.456549282395647849, 1.325737238711437893 ) ) ;
#4266 = CARTESIAN_POINT ( 'NONE',  ( 3.563142721848435279, -1.644496397275853505, 1.160845683069864798 ) ) ;
#4265 = CARTESIAN_POINT ( 'NONE',  ( 0.1341856092403709844, 0.3330598185416616119, 1.913145364980510799 ) ) ;
#4267 = CARTESIAN_POINT ( 'NONE',  ( 4.921405902946369260, 0.8734970824106644827, 2.126109943308290617 ) ) ;
#4269 = CARTESIAN_POINT ( 'NONE',  ( 3.871788065385643574, -1.834046284760854961, 0.3141801383321814467 ) ) ;
#4268 = DIRECTION ( 'NONE',  ( 0.000000000000000000, 0.000000000000000000, -1.000000000000000000 ) ) ;
#4270 = CARTESIAN_POINT ( 'NONE',  ( 6.230854113932139171, 9.427024345299638952, 1.199719254218452047 ) ) ;
#4271 = CARTESIAN_POINT ( 'NONE',  ( -9.827407719474578585, -6.362962251424048254, 0.4359508081056245876 ) ) ;
#4272 = CARTESIAN_POINT ( 'NONE',  ( -5.994676475536691029, 10.14553965476814845, 0.7998128361456481317 ) ) ;
#4273 = CARTESIAN_POINT ( 'NONE',  ( 6.720655732516671144, 1.288224904612661925, 1.942155157606942240 ) ) ;
#4274 = CARTESIAN_POINT ( 'NONE',  ( 0.8377433530848135135, 0.8832496248250313320, -2.005872107257236969 ) ) ;
#4275 = CARTESIAN_POINT ( 'NONE',  ( 5.992340707560163793, 6.093411701682730275, 0.7216878364870317197 ) ) ;
#4276 = ORIENTED_EDGE ( 'NONE', *, *, #48686, .F. ) ;
#4277 = CIRCLE ( 'NONE', #159863, 0.8299999999999999600 ) ;
#4278 = CARTESIAN_POINT ( 'NONE',  ( 11.86145016429272836, 12.69999999999999929, 1.179999999999997051 ) ) ;
#4279 = CARTESIAN_POINT ( 'NONE',  ( 0.1174333910212103232, -1.791171220025630895, 0.3524246893974944395 ) ) ;
#4280 = CARTESIAN_POINT ( 'NONE',  ( -3.588104209110990706, 7.337872010604796991, 1.040834085586084257E-14 ) ) ;
#4281 =( BOUNDED_SURFACE ( )  B_SPLINE_SURFACE ( 1, 2, ( 
 ( #60722, #125819, #11968, #92201, #191780, #158251, #174510, #8773, #194993, #46627, #45566, #13027, #144166, #43436, #208033, #74856, #109560, #9839, #193920, #140958, #160365, #126885, #175564, #75915, #206969, #94324, #192843, #27155, #210158, #93259, #159293, #10892, #76967, #58599, #112750, #178762, #111683, #79104, #61799, #127968, #124754, #143094, #209087, #145222, #44502, #177690, #29301, #110619, #190714, #176619, #95395, #161447, #129016, #181921, #213352, #214388, #200296, #96461, #197117, #63923, #162511, #84434, #50874, #33551, #116996, #14082, #180869, #182996, #48755, #179819, #64974, #148387, #32490, #51949, #30375, #196073, #98564, #67087, #97517, #147324, #150523, #118071, #80172, #146278, #164625, #66017, #212290, #130078, #2084, #31438, #132166, #47705, #113820, #34613, #149440, #163573, #133221, #15156, #82294, #68157, #81242, #199227, #18356, #49805, #131128, #115931, #114868, #16210, #198172, #99624, #165690, #134291, #17279, #83355, #1022, #100683, #166761, #172096, #121287, #171015, #56205, #120213, #203488, #35676, #19421, #151586, #138534, #86571, #36740, #135343, #187263, #153712, #204557, #188325, #89799, #104974, #37820, #57274, #152634, #102826, #20485, #4221, #154779, #201357, #72432, #39966, #185114, #70290, #168881, #186187, #54077, #52998, #38889, #22612, #103898, #101754, #69224, #88720, #136406, #202422, #184058, #139614, #205636, #169945, #23689, #122369, #21531, #106073, #87641, #155844, #6363, #167821, #85499, #5281, #71358, #137474, #3153, #55141, #7430, #73511, #119134, #58336, #9577, #60457, #126614, #42109, #95120, #26887, #123436, #191513, #207769, #124492, #190451, #160098, #24754, #45295, #78829, #108222, #90856, #177419, #175301, #74590, #189398, #142820, #77775, #144950, #12755, #174247, #161169, #127693, #210956, #44232, #140693, #76703, #25819, #91929, #41040, #110353, #107149, #157989, #143895, #75654, #176356, #141761, #193653, #94057, #173174, #109291, #11701, #27964, #59396, #61527, #125552, #156920, #43178, #92990, #159035, #10628, #8509, #206709, #208827, #192577, #209889, #111415, #29037, #84169, #99367, #100419, #182727, #113549, #166490, #163300, #165419, #97246, #34346, #194719, #63661, #149170, #18081, #179552, #13824, #146007, #31173, #132956, #164362, #114611, #130858, #46358, #150258, #14881, #80975, #147065, #112478, #213086, #79898, #17015, #178487, #131900, #98299, #64716, #212017, #30097, #214124, #32227, #196854, #197907, #129815, #48493, #195797, #47434, #62583, #128745, #96187, #83091, #198959, #49536, #747, #162238, #180602, #15947, #116727, #82030, #115662, #181656, #148124, #65753, #33282, #66813, #50602, #57812, #156394, #187802, #188875, #174795, #67885, #171557, #35411, #134030, #58884, #25306, #7980, #91408, #200037, #155318, #157468, #23153, #154257, #39430, #122917, #6902, #26371, #1826, #170489, #72979, #41591, #71903, #121831, #125039, #92483, #51689, #117811, #139082, #40515, #183801, #101489, #190995, #5830, #106618, #22073, #88185, #9063, #123975, #138012, #107703, #204027, #56752, #42661, #55675, #173729, #207256, #24223, #105523, #90325, #89268, #205109, #172647, #74069, #140162, #108770, #206185, #189942, #75138, #141247, #210454, #146569, #95682, #145518, #30668, #94611, #177981, #10120, #208315, #126101, #113043, #61018, #11182, #109838, #161736, #128251, #179049, #162801, #64226, #79401, #12252, #31733, #127176, #77261, #45859, #62092, #78329, #142304, #114116, #193145, #129318, #175853, #46925, #14378, #159584, #44795, #143375, #160654, #28521, #27442, #13327, #211517, #144451, #76195, #43724, #63153, #110900, #209374, #158523, #180109, #59945, #176906, #212587, #96751, #194214, #80470, #111980, #130368, #195294, #192061, #93540, #29596, #196358, #47999, #65259, #116227, #17569, #199529, #184352, #32786, #198462, #34897, #100970, #16507, #69523, #1320, #97806, #165983, #182218, #98862, #164914, #134588, #213633, #19721, #53300, #82589, #131406, #151880, #149743, #49047, #163869, #117295, #52236, #119432, #201650, #148676, #135630, #102054, #185419, #18651, #115167, #51172, #244, #66316, #15445, #84730, #81534, #132460 ),
 ( #50106, #33841, #67381, #99922, #147615, #197406, #83653, #181162, #133522, #183292, #167059, #150819, #200588, #2382, #3454, #68460, #118363, #35974, #168120, #85800, #157216, #169179, #38122, #123732, #8813, #87935, #202723, #120513, #154008, #107454, #6662, #71655, #20772, #207006, #5575, #58637, #137769, #74890, #170242, #124790, #73817, #140998, #37037, #203787, #103121, #55433, #139911, #121585, #86867, #152933, #104195, #189694, #4510, #187557, #54376, #186491, #39185, #173481, #138836, #89021, #105273, #70582, #136698, #171310, #7732, #21827, #205942, #41346, #22904, #155073, #72739, #204852, #56507, #122668, #188630, #23984, #40261, #106373, #172396, #90087, #156150, #57574, #25058, #91160, #146310, #109595, #30414, #145260, #192881, #79143, #60763, #96498, #161486, #174548, #212324, #27190, #143130, #94360, #158285, #209126, #110654, #78078, #62890, #125856, #77004, #128002, #193956, #175601, #162548, #160402, #190750, #44538, #126924, #191813, #43477, #13064, #92235, #112787, #63963, #93296, #9875, #14118, #28268, #142053, #42414, #210199, #211266, #108519, #80210, #159332, #26123, #195032, #75951, #111720, #208068, #144203, #10928, #176655, #59693, #177728, #12004, #61835, #129058, #45603, #29340, #95433, #46666, #178798, #3186, #115970, #100719, #50910, #114907, #68194, #180905, #113860, #197153, #48790, #85530, #1061, #131162, #130118, #179855, #198207, #196108, #184092, #35711, #31478, #97553, #165728, #181958, #118107, #67126, #117038, #2119, #66056, #149478, #47744, #163611, #15192, #84467, #32528, #98603, #81283, #133259, #99659, #150559, #134326, #101788, #183033, #49842, #147359, #164664, #16246, #82332, #148424, #66031, #213386, #132200, #65010, #18390, #33587, #199266, #17316, #83394, #34649, #166796, #200332, #51982, #167857, #19454, #151620, #37853, #136439, #20520, #69257, #173207, #24787, #23721, #205668, #56240, #106105, #90890, #103932, #4253, #123469, #38921, #122399, #188357, #169976, #135374, #54109, #72467, #105005, #39997, #6394, #21564, #171044, #156949, #201392, #87670, #102859, #53030, #189432, #89828, #138567, #155876, #119163, #5310, #7465, #153742, #70322, #71391, #187295, #137503, #185149, #36773, #86603, #203520, #172127, #202455, #186222, #41074, #168915, #152669, #120244, #55174, #22643, #121319, #88751, #107181, #154808, #204588, #73544, #139647, #57306, #127728, #42141, #111449, #178521, #60488, #62616, #59428, #45330, #210989, #27996, #30131, #126646, #128778, #125586, #177454, #194755, #94093, #96220, #160132, #9609, #8541, #206740, #76735, #74623, #46392, #112509, #58371, #124525, #44264, #192611, #140727, #11731, #209923, #95151, #159067, #77807, #190482, #108256, #174277, #29068, #191546, #75686, #25852, #143928, #110386, #161203, #12789, #91962, #61562, #142853, #158021, #43211, #141796, #109327, #175335, #26917, #207800, #93026, #10663, #78863, #208857, #193686, #176391, #144984, #97282, #63694, #99400, #131934, #130894, #83127, #163337, #196888, #14916, #113584, #162271, #51724, #117846, #116766, #84206, #149207, #198994, #183838, #48526, #81010, #1861, #197944, #782, #66849, #114646, #13858, #147098, #165453, #49572, #132993, #17048, #180639, #115697, #35447, #79935, #32264, #195831, #146040, #67922, #182764, #50640, #34381, #212054, #98331, #100454, #164397, #213122, #15980, #65784, #82065, #129848, #47469, #179586, #148157, #166527, #64752, #214158, #134066, #31208, #181689, #33319, #18118, #150294, #200075, #201134, #7206, #102603, #203271, #52772, #135118, #188104, #6135, #118909, #204327, #155621, #152417, #138312, #89572, #121068, #57054, #187036, #168657, #101527, #85273, #169725, #189182, #73279, #139383, #151360, #2929, #137251, #153488, #205416, #38668, #88495, #39734, #37594, #104747, #167596, #69001, #184892, #55985, #3996, #20262, #36516, #170795, #71133, #122137, #105839, #123218, #22386, #21314, #19195, #70065, #86346, #136178, #202196, #53852, #119985, #185962, #103677, #171866, #87421, #154556, #54917, #5058, #72204, #23460, #10419, #109072, #25604, #208611, #124277, #91716, #190235, #140476, #40819, #193452, #45096, #27751, #77563 ) ),
 .UNSPECIFIED., .F., .F., .T. ) 
 B_SPLINE_SURFACE_WITH_KNOTS ( ( 2, 2 ),
 ( 3, 2, 2, 2, 2, 2, 2, 2, 2, 2, 2, 2, 2, 2, 2, 2, 2, 2, 2, 2, 2, 2, 2, 2, 2, 2, 2, 2, 2, 2, 2, 2, 2, 2, 2, 2, 2, 2, 2, 2, 2, 2, 2, 2, 2, 2, 2, 2, 2, 2, 2, 2, 2, 2, 2, 2, 2, 2, 2, 2, 2, 2, 2, 2, 2, 2, 2, 2, 2, 2, 2, 2, 2, 2, 2, 2, 2, 2, 2, 2, 2, 2, 2, 2, 2, 2, 2, 2, 2, 2, 2, 2, 2, 2, 2, 2, 2, 2, 2, 2, 2, 2, 2, 2, 2, 2, 2, 2, 2, 2, 2, 2, 2, 2, 2, 2, 2, 2, 2, 2, 2, 2, 2, 2, 2, 2, 2, 2, 2, 2, 2, 2, 2, 2, 2, 2, 2, 2, 2, 2, 2, 2, 2, 2, 2, 2, 2, 2, 2, 2, 2, 2, 2, 2, 2, 2, 2, 2, 2, 2, 2, 2, 2, 2, 2, 2, 2, 2, 2, 2, 2, 2, 2, 2, 2, 2, 2, 2, 2, 2, 2, 2, 2, 2, 2, 2, 2, 2, 2, 2, 2, 2, 2, 2, 2, 2, 2, 2, 2, 2, 2, 2, 2, 2, 2, 2, 2, 2, 2, 2, 2, 2, 2, 2, 2, 2, 2, 2, 2, 2, 2, 2, 2, 2, 2, 2, 2, 2, 2, 2, 2, 2, 2, 2, 2, 2, 2, 2, 2, 2, 3 ),
 ( 0.000000000000000000, 1.000000000000000000 ),
 ( 0.000000000000000000, 0.004166666666666666609, 0.008333333333333333218, 0.01250000000000000069, 0.01666666666666666644, 0.02083333333333333218, 0.02500000000000000139, 0.02916666666666666713, 0.03333333333333333287, 0.03749999999999999861, 0.04166666666666666435, 0.04583333333333333010, 0.05000000000000000278, 0.05416666666666666852, 0.05833333333333333426, 0.06250000000000000000, 0.06666666666666666574, 0.07083333333333333148, 0.07499999999999999722, 0.07916666666666666297, 0.08333333333333332871, 0.08749999999999999445, 0.09166666666666666019, 0.09583333333333333981, 0.1000000000000000056, 0.1041666666666666713, 0.1083333333333333370, 0.1125000000000000028, 0.1166666666666666685, 0.1208333333333333343, 0.1250000000000000000, 0.1291666666666666796, 0.1333333333333333315, 0.1375000000000000111, 0.1416666666666666630, 0.1458333333333333426, 0.1499999999999999944, 0.1541666666666666741, 0.1583333333333333259, 0.1625000000000000056, 0.1666666666666666574, 0.1708333333333333370, 0.1749999999999999889, 0.1791666666666666685, 0.1833333333333333204, 0.1875000000000000000, 0.1916666666666666796, 0.1958333333333333315, 0.2000000000000000111, 0.2041666666666666630, 0.2083333333333333426, 0.2124999999999999944, 0.2166666666666666741, 0.2208333333333333259, 0.2250000000000000056, 0.2291666666666666574, 0.2333333333333333370, 0.2374999999999999889, 0.2416666666666666685, 0.2458333333333333204, 0.2500000000000000000, 0.2541666666666666519, 0.2583333333333333592, 0.2625000000000000111, 0.2666666666666666630, 0.2708333333333333148, 0.2750000000000000222, 0.2791666666666666741, 0.2833333333333333259, 0.2874999999999999778, 0.2916666666666666852, 0.2958333333333333370, 0.2999999999999999889, 0.3041666666666666408, 0.3083333333333333481, 0.3125000000000000000, 0.3166666666666666519, 0.3208333333333333592, 0.3250000000000000111, 0.3291666666666666630, 0.3333333333333333148, 0.3375000000000000222, 0.3416666666666666741, 0.3458333333333333259, 0.3499999999999999778, 0.3541666666666666852, 0.3583333333333333370, 0.3624999999999999889, 0.3666666666666666408, 0.3708333333333333481, 0.3750000000000000000, 0.3791666666666666519, 0.3833333333333333592, 0.3875000000000000111, 0.3916666666666666630, 0.3958333333333333148, 0.4000000000000000222, 0.4041666666666666741, 0.4083333333333333259, 0.4124999999999999778, 0.4166666666666666852, 0.4208333333333333370, 0.4249999999999999889, 0.4291666666666666408, 0.4333333333333333481, 0.4375000000000000000, 0.4416666666666666519, 0.4458333333333333592, 0.4500000000000000111, 0.4541666666666666630, 0.4583333333333333148, 0.4625000000000000222, 0.4666666666666666741, 0.4708333333333333259, 0.4749999999999999778, 0.4791666666666666852, 0.4833333333333333370, 0.4874999999999999889, 0.4916666666666666408, 0.4958333333333333481, 0.5000000000000000000, 0.5041666666666666519, 0.5083333333333333037, 0.5124999999999999556, 0.5166666666666667185, 0.5208333333333333703, 0.5250000000000000222, 0.5291666666666666741, 0.5333333333333333259, 0.5374999999999999778, 0.5416666666666666297, 0.5458333333333332815, 0.5500000000000000444, 0.5541666666666666963, 0.5583333333333333481, 0.5625000000000000000, 0.5666666666666666519, 0.5708333333333333037, 0.5749999999999999556, 0.5791666666666667185, 0.5833333333333333703, 0.5875000000000000222, 0.5916666666666666741, 0.5958333333333333259, 0.5999999999999999778, 0.6041666666666666297, 0.6083333333333332815, 0.6125000000000000444, 0.6166666666666666963, 0.6208333333333333481, 0.6250000000000000000, 0.6291666666666666519, 0.6333333333333333037, 0.6374999999999999556, 0.6416666666666667185, 0.6458333333333333703, 0.6500000000000000222, 0.6541666666666666741, 0.6583333333333333259, 0.6624999999999999778, 0.6666666666666666297, 0.6708333333333332815, 0.6750000000000000444, 0.6791666666666666963, 0.6833333333333333481, 0.6875000000000000000, 0.6916666666666666519, 0.6958333333333333037, 0.6999999999999999556, 0.7041666666666667185, 0.7083333333333333703, 0.7125000000000000222, 0.7166666666666666741, 0.7208333333333333259, 0.7249999999999999778, 0.7291666666666666297, 0.7333333333333332815, 0.7375000000000000444, 0.7416666666666666963, 0.7458333333333333481, 0.7500000000000000000, 0.7541666666666666519, 0.7583333333333333037, 0.7624999999999999556, 0.7666666666666667185, 0.7708333333333333703, 0.7750000000000000222, 0.7791666666666666741, 0.7833333333333333259, 0.7874999999999999778, 0.7916666666666666297, 0.7958333333333332815, 0.8000000000000000444, 0.8041666666666666963, 0.8083333333333333481, 0.8125000000000000000, 0.8166666666666666519, 0.8208333333333333037, 0.8249999999999999556, 0.8291666666666667185, 0.8333333333333333703, 0.8375000000000000222, 0.8416666666666666741, 0.8458333333333333259, 0.8499999999999999778, 0.8541666666666666297, 0.8583333333333332815, 0.8625000000000000444, 0.8666666666666666963, 0.8708333333333333481, 0.8750000000000000000, 0.8791666666666666519, 0.8833333333333333037, 0.8874999999999999556, 0.8916666666666667185, 0.8958333333333333703, 0.9000000000000000222, 0.9041666666666666741, 0.9083333333333333259, 0.9124999999999999778, 0.9166666666666666297, 0.9208333333333332815, 0.9250000000000000444, 0.9291666666666666963, 0.9333333333333333481, 0.9375000000000000000, 0.9416666666666666519, 0.9458333333333333037, 0.9499999999999999556, 0.9541666666666667185, 0.9583333333333333703, 0.9625000000000000222, 0.9666666666666666741, 0.9708333333333333259, 0.9749999999999999778, 0.9791666666666666297, 0.9833333333333332815, 0.9875000000000000444, 0.9916666666666666963, 0.9958333333333333481, 1.000000000000000000 ),
 .UNSPECIFIED. ) 
 GEOMETRIC_REPRESENTATION_ITEM ( )  RATIONAL_B_SPLINE_SURFACE ( (
 ( 1.000000000000000000, 0.8660254037844387076, 1.000000000000000000, 0.8660254037844387076, 1.000000000000000000, 0.8660254037844387076, 1.000000000000000000, 0.8660254037844387076, 1.000000000000000000, 0.8660254037844387076, 1.000000000000000000, 0.8660254037844387076, 1.000000000000000000, 0.8660254037844387076, 1.000000000000000000, 0.8660254037844387076, 1.000000000000000000, 0.8660254037844387076, 1.000000000000000000, 0.8660254037844387076, 1.000000000000000000, 0.8660254037844387076, 1.000000000000000000, 0.8660254037844387076, 1.000000000000000000, 0.8660254037844387076, 1.000000000000000000, 0.8660254037844387076, 1.000000000000000000, 0.8660254037844387076, 1.000000000000000000, 0.8660254037844387076, 1.000000000000000000, 0.8660254037844387076, 1.000000000000000000, 0.8660254037844387076, 1.000000000000000000, 0.8660254037844387076, 1.000000000000000000, 0.8660254037844387076, 1.000000000000000000, 0.8660254037844387076, 1.000000000000000000, 0.8660254037844387076, 1.000000000000000000, 0.8660254037844387076, 1.000000000000000000, 0.8660254037844387076, 1.000000000000000000, 0.8660254037844387076, 1.000000000000000000, 0.8660254037844387076, 1.000000000000000000, 0.8660254037844387076, 1.000000000000000000, 0.8660254037844387076, 1.000000000000000000, 0.8660254037844387076, 1.000000000000000000, 0.8660254037844387076, 1.000000000000000000, 0.8660254037844387076, 1.000000000000000000, 0.8660254037844387076, 1.000000000000000000, 0.8660254037844387076, 1.000000000000000000, 0.8660254037844387076, 1.000000000000000000, 0.8660254037844387076, 1.000000000000000000, 0.8660254037844387076, 1.000000000000000000, 0.8660254037844387076, 1.000000000000000000, 0.8660254037844387076, 1.000000000000000000, 0.8660254037844387076, 1.000000000000000000, 0.8660254037844387076, 1.000000000000000000, 0.8660254037844387076, 1.000000000000000000, 0.8660254037844387076, 1.000000000000000000, 0.8660254037844387076, 1.000000000000000000, 0.8660254037844387076, 1.000000000000000000, 0.8660254037844387076, 1.000000000000000000, 0.8660254037844387076, 1.000000000000000000, 0.8660254037844387076, 1.000000000000000000, 0.8660254037844387076, 1.000000000000000000, 0.8660254037844387076, 1.000000000000000000, 0.8660254037844387076, 1.000000000000000000, 0.8660254037844387076, 1.000000000000000000, 0.8660254037844387076, 1.000000000000000000, 0.8660254037844387076, 1.000000000000000000, 0.8660254037844387076, 1.000000000000000000, 0.8660254037844387076, 1.000000000000000000, 0.8660254037844387076, 1.000000000000000000, 0.8660254037844387076, 1.000000000000000000, 0.8660254037844387076, 1.000000000000000000, 0.8660254037844387076, 1.000000000000000000, 0.8660254037844387076, 1.000000000000000000, 0.8660254037844387076, 1.000000000000000000, 0.8660254037844387076, 1.000000000000000000, 0.8660254037844387076, 1.000000000000000000, 0.8660254037844387076, 1.000000000000000000, 0.8660254037844387076, 1.000000000000000000, 0.8660254037844387076, 1.000000000000000000, 0.8660254037844387076, 1.000000000000000000, 0.8660254037844387076, 1.000000000000000000, 0.8660254037844387076, 1.000000000000000000, 0.8660254037844387076, 1.000000000000000000, 0.8660254037844387076, 1.000000000000000000, 0.8660254037844387076, 1.000000000000000000, 0.8660254037844387076, 1.000000000000000000, 0.8660254037844387076, 1.000000000000000000, 0.8660254037844387076, 1.000000000000000000, 0.8660254037844387076, 1.000000000000000000, 0.8660254037844387076, 1.000000000000000000, 0.8660254037844387076, 1.000000000000000000, 0.8660254037844387076, 1.000000000000000000, 0.8660254037844387076, 1.000000000000000000, 0.8660254037844387076, 1.000000000000000000, 0.8660254037844387076, 1.000000000000000000, 0.8660254037844387076, 1.000000000000000000, 0.8660254037844387076, 1.000000000000000000, 0.8660254037844387076, 1.000000000000000000, 0.8660254037844387076, 1.000000000000000000, 0.8660254037844387076, 1.000000000000000000, 0.8660254037844387076, 1.000000000000000000, 0.8660254037844387076, 1.000000000000000000, 0.8660254037844387076, 1.000000000000000000, 0.8660254037844387076, 1.000000000000000000, 0.8660254037844387076, 1.000000000000000000, 0.8660254037844387076, 1.000000000000000000, 0.8660254037844387076, 1.000000000000000000, 0.8660254037844387076, 1.000000000000000000, 0.8660254037844387076, 1.000000000000000000, 0.8660254037844387076, 1.000000000000000000, 0.8660254037844387076, 1.000000000000000000, 0.8660254037844387076, 1.000000000000000000, 0.8660254037844387076, 1.000000000000000000, 0.8660254037844387076, 1.000000000000000000, 0.8660254037844387076, 1.000000000000000000, 0.8660254037844387076, 1.000000000000000000, 0.8660254037844387076, 1.000000000000000000, 0.8660254037844387076, 1.000000000000000000, 0.8660254037844387076, 1.000000000000000000, 0.8660254037844387076, 1.000000000000000000, 0.8660254037844387076, 1.000000000000000000, 0.8660254037844387076, 1.000000000000000000, 0.8660254037844387076, 1.000000000000000000, 0.8660254037844387076, 1.000000000000000000, 0.8660254037844387076, 1.000000000000000000, 0.8660254037844387076, 1.000000000000000000, 0.8660254037844387076, 1.000000000000000000, 0.8660254037844387076, 1.000000000000000000, 0.8660254037844387076, 1.000000000000000000, 0.8660254037844387076, 1.000000000000000000, 0.8660254037844387076, 1.000000000000000000, 0.8660254037844387076, 1.000000000000000000, 0.8660254037844387076, 1.000000000000000000, 0.8660254037844387076, 1.000000000000000000, 0.8660254037844387076, 1.000000000000000000, 0.8660254037844387076, 1.000000000000000000, 0.8660254037844387076, 1.000000000000000000, 0.8660254037844387076, 1.000000000000000000, 0.8660254037844387076, 1.000000000000000000, 0.8660254037844387076, 1.000000000000000000, 0.8660254037844387076, 1.000000000000000000, 0.8660254037844387076, 1.000000000000000000, 0.8660254037844387076, 1.000000000000000000, 0.8660254037844387076, 1.000000000000000000, 0.8660254037844387076, 1.000000000000000000, 0.8660254037844387076, 1.000000000000000000, 0.8660254037844387076, 1.000000000000000000, 0.8660254037844387076, 1.000000000000000000, 0.8660254037844387076, 1.000000000000000000, 0.8660254037844387076, 1.000000000000000000, 0.8660254037844387076, 1.000000000000000000, 0.8660254037844387076, 1.000000000000000000, 0.8660254037844387076, 1.000000000000000000, 0.8660254037844387076, 1.000000000000000000, 0.8660254037844387076, 1.000000000000000000, 0.8660254037844387076, 1.000000000000000000, 0.8660254037844387076, 1.000000000000000000, 0.8660254037844387076, 1.000000000000000000, 0.8660254037844387076, 1.000000000000000000, 0.8660254037844387076, 1.000000000000000000, 0.8660254037844387076, 1.000000000000000000, 0.8660254037844387076, 1.000000000000000000, 0.8660254037844387076, 1.000000000000000000, 0.8660254037844387076, 1.000000000000000000, 0.8660254037844387076, 1.000000000000000000, 0.8660254037844387076, 1.000000000000000000, 0.8660254037844387076, 1.000000000000000000, 0.8660254037844387076, 1.000000000000000000, 0.8660254037844387076, 1.000000000000000000, 0.8660254037844387076, 1.000000000000000000, 0.8660254037844387076, 1.000000000000000000, 0.8660254037844387076, 1.000000000000000000, 0.8660254037844387076, 1.000000000000000000, 0.8660254037844387076, 1.000000000000000000, 0.8660254037844387076, 1.000000000000000000, 0.8660254037844387076, 1.000000000000000000, 0.8660254037844387076, 1.000000000000000000, 0.8660254037844387076, 1.000000000000000000, 0.8660254037844387076, 1.000000000000000000, 0.8660254037844387076, 1.000000000000000000, 0.8660254037844387076, 1.000000000000000000, 0.8660254037844387076, 1.000000000000000000, 0.8660254037844387076, 1.000000000000000000, 0.8660254037844387076, 1.000000000000000000, 0.8660254037844387076, 1.000000000000000000, 0.8660254037844387076, 1.000000000000000000, 0.8660254037844387076, 1.000000000000000000, 0.8660254037844387076, 1.000000000000000000, 0.8660254037844387076, 1.000000000000000000, 0.8660254037844387076, 1.000000000000000000, 0.8660254037844387076, 1.000000000000000000, 0.8660254037844387076, 1.000000000000000000, 0.8660254037844387076, 1.000000000000000000, 0.8660254037844387076, 1.000000000000000000, 0.8660254037844387076, 1.000000000000000000, 0.8660254037844387076, 1.000000000000000000, 0.8660254037844387076, 1.000000000000000000, 0.8660254037844387076, 1.000000000000000000, 0.8660254037844387076, 1.000000000000000000, 0.8660254037844387076, 1.000000000000000000, 0.8660254037844387076, 1.000000000000000000, 0.8660254037844387076, 1.000000000000000000, 0.8660254037844387076, 1.000000000000000000, 0.8660254037844387076, 1.000000000000000000, 0.8660254037844387076, 1.000000000000000000, 0.8660254037844387076, 1.000000000000000000, 0.8660254037844387076, 1.000000000000000000, 0.8660254037844387076, 1.000000000000000000, 0.8660254037844387076, 1.000000000000000000, 0.8660254037844387076, 1.000000000000000000, 0.8660254037844387076, 1.000000000000000000, 0.8660254037844387076, 1.000000000000000000, 0.8660254037844387076, 1.000000000000000000, 0.8660254037844387076, 1.000000000000000000, 0.8660254037844387076, 1.000000000000000000, 0.8660254037844387076, 1.000000000000000000, 0.8660254037844387076, 1.000000000000000000, 0.8660254037844387076, 1.000000000000000000, 0.8660254037844387076, 1.000000000000000000, 0.8660254037844387076, 1.000000000000000000, 0.8660254037844387076, 1.000000000000000000, 0.8660254037844387076, 1.000000000000000000, 0.8660254037844387076, 1.000000000000000000, 0.8660254037844387076, 1.000000000000000000, 0.8660254037844387076, 1.000000000000000000, 0.8660254037844387076, 1.000000000000000000, 0.8660254037844387076, 1.000000000000000000, 0.8660254037844387076, 1.000000000000000000, 0.8660254037844387076, 1.000000000000000000, 0.8660254037844387076, 1.000000000000000000, 0.8660254037844387076, 1.000000000000000000, 0.8660254037844387076, 1.000000000000000000, 0.8660254037844387076, 1.000000000000000000, 0.8660254037844387076, 1.000000000000000000, 0.8660254037844387076, 1.000000000000000000, 0.8660254037844387076, 1.000000000000000000, 0.8660254037844387076, 1.000000000000000000, 0.8660254037844387076, 1.000000000000000000, 0.8660254037844387076, 1.000000000000000000, 0.8660254037844387076, 1.000000000000000000, 0.8660254037844387076, 1.000000000000000000, 0.8660254037844387076, 1.000000000000000000, 0.8660254037844387076, 1.000000000000000000, 0.8660254037844387076, 1.000000000000000000, 0.8660254037844387076, 1.000000000000000000, 0.8660254037844387076, 1.000000000000000000, 0.8660254037844387076, 1.000000000000000000, 0.8660254037844387076, 1.000000000000000000, 0.8660254037844387076, 1.000000000000000000, 0.8660254037844387076, 1.000000000000000000, 0.8660254037844387076, 1.000000000000000000, 0.8660254037844387076, 1.000000000000000000, 0.8660254037844387076, 1.000000000000000000),
 ( 1.000000000000000000, 0.8660254037844387076, 1.000000000000000000, 0.8660254037844387076, 1.000000000000000000, 0.8660254037844387076, 1.000000000000000000, 0.8660254037844387076, 1.000000000000000000, 0.8660254037844387076, 1.000000000000000000, 0.8660254037844387076, 1.000000000000000000, 0.8660254037844387076, 1.000000000000000000, 0.8660254037844387076, 1.000000000000000000, 0.8660254037844387076, 1.000000000000000000, 0.8660254037844387076, 1.000000000000000000, 0.8660254037844387076, 1.000000000000000000, 0.8660254037844387076, 1.000000000000000000, 0.8660254037844387076, 1.000000000000000000, 0.8660254037844387076, 1.000000000000000000, 0.8660254037844387076, 1.000000000000000000, 0.8660254037844387076, 1.000000000000000000, 0.8660254037844387076, 1.000000000000000000, 0.8660254037844387076, 1.000000000000000000, 0.8660254037844387076, 1.000000000000000000, 0.8660254037844387076, 1.000000000000000000, 0.8660254037844387076, 1.000000000000000000, 0.8660254037844387076, 1.000000000000000000, 0.8660254037844387076, 1.000000000000000000, 0.8660254037844387076, 1.000000000000000000, 0.8660254037844387076, 1.000000000000000000, 0.8660254037844387076, 1.000000000000000000, 0.8660254037844387076, 1.000000000000000000, 0.8660254037844387076, 1.000000000000000000, 0.8660254037844387076, 1.000000000000000000, 0.8660254037844387076, 1.000000000000000000, 0.8660254037844387076, 1.000000000000000000, 0.8660254037844387076, 1.000000000000000000, 0.8660254037844387076, 1.000000000000000000, 0.8660254037844387076, 1.000000000000000000, 0.8660254037844387076, 1.000000000000000000, 0.8660254037844387076, 1.000000000000000000, 0.8660254037844387076, 1.000000000000000000, 0.8660254037844387076, 1.000000000000000000, 0.8660254037844387076, 1.000000000000000000, 0.8660254037844387076, 1.000000000000000000, 0.8660254037844387076, 1.000000000000000000, 0.8660254037844387076, 1.000000000000000000, 0.8660254037844387076, 1.000000000000000000, 0.8660254037844387076, 1.000000000000000000, 0.8660254037844387076, 1.000000000000000000, 0.8660254037844387076, 1.000000000000000000, 0.8660254037844387076, 1.000000000000000000, 0.8660254037844387076, 1.000000000000000000, 0.8660254037844387076, 1.000000000000000000, 0.8660254037844387076, 1.000000000000000000, 0.8660254037844387076, 1.000000000000000000, 0.8660254037844387076, 1.000000000000000000, 0.8660254037844387076, 1.000000000000000000, 0.8660254037844387076, 1.000000000000000000, 0.8660254037844387076, 1.000000000000000000, 0.8660254037844387076, 1.000000000000000000, 0.8660254037844387076, 1.000000000000000000, 0.8660254037844387076, 1.000000000000000000, 0.8660254037844387076, 1.000000000000000000, 0.8660254037844387076, 1.000000000000000000, 0.8660254037844387076, 1.000000000000000000, 0.8660254037844387076, 1.000000000000000000, 0.8660254037844387076, 1.000000000000000000, 0.8660254037844387076, 1.000000000000000000, 0.8660254037844387076, 1.000000000000000000, 0.8660254037844387076, 1.000000000000000000, 0.8660254037844387076, 1.000000000000000000, 0.8660254037844387076, 1.000000000000000000, 0.8660254037844387076, 1.000000000000000000, 0.8660254037844387076, 1.000000000000000000, 0.8660254037844387076, 1.000000000000000000, 0.8660254037844387076, 1.000000000000000000, 0.8660254037844387076, 1.000000000000000000, 0.8660254037844387076, 1.000000000000000000, 0.8660254037844387076, 1.000000000000000000, 0.8660254037844387076, 1.000000000000000000, 0.8660254037844387076, 1.000000000000000000, 0.8660254037844387076, 1.000000000000000000, 0.8660254037844387076, 1.000000000000000000, 0.8660254037844387076, 1.000000000000000000, 0.8660254037844387076, 1.000000000000000000, 0.8660254037844387076, 1.000000000000000000, 0.8660254037844387076, 1.000000000000000000, 0.8660254037844387076, 1.000000000000000000, 0.8660254037844387076, 1.000000000000000000, 0.8660254037844387076, 1.000000000000000000, 0.8660254037844387076, 1.000000000000000000, 0.8660254037844387076, 1.000000000000000000, 0.8660254037844387076, 1.000000000000000000, 0.8660254037844387076, 1.000000000000000000, 0.8660254037844387076, 1.000000000000000000, 0.8660254037844387076, 1.000000000000000000, 0.8660254037844387076, 1.000000000000000000, 0.8660254037844387076, 1.000000000000000000, 0.8660254037844387076, 1.000000000000000000, 0.8660254037844387076, 1.000000000000000000, 0.8660254037844387076, 1.000000000000000000, 0.8660254037844387076, 1.000000000000000000, 0.8660254037844387076, 1.000000000000000000, 0.8660254037844387076, 1.000000000000000000, 0.8660254037844387076, 1.000000000000000000, 0.8660254037844387076, 1.000000000000000000, 0.8660254037844387076, 1.000000000000000000, 0.8660254037844387076, 1.000000000000000000, 0.8660254037844387076, 1.000000000000000000, 0.8660254037844387076, 1.000000000000000000, 0.8660254037844387076, 1.000000000000000000, 0.8660254037844387076, 1.000000000000000000, 0.8660254037844387076, 1.000000000000000000, 0.8660254037844387076, 1.000000000000000000, 0.8660254037844387076, 1.000000000000000000, 0.8660254037844387076, 1.000000000000000000, 0.8660254037844387076, 1.000000000000000000, 0.8660254037844387076, 1.000000000000000000, 0.8660254037844387076, 1.000000000000000000, 0.8660254037844387076, 1.000000000000000000, 0.8660254037844387076, 1.000000000000000000, 0.8660254037844387076, 1.000000000000000000, 0.8660254037844387076, 1.000000000000000000, 0.8660254037844387076, 1.000000000000000000, 0.8660254037844387076, 1.000000000000000000, 0.8660254037844387076, 1.000000000000000000, 0.8660254037844387076, 1.000000000000000000, 0.8660254037844387076, 1.000000000000000000, 0.8660254037844387076, 1.000000000000000000, 0.8660254037844387076, 1.000000000000000000, 0.8660254037844387076, 1.000000000000000000, 0.8660254037844387076, 1.000000000000000000, 0.8660254037844387076, 1.000000000000000000, 0.8660254037844387076, 1.000000000000000000, 0.8660254037844387076, 1.000000000000000000, 0.8660254037844387076, 1.000000000000000000, 0.8660254037844387076, 1.000000000000000000, 0.8660254037844387076, 1.000000000000000000, 0.8660254037844387076, 1.000000000000000000, 0.8660254037844387076, 1.000000000000000000, 0.8660254037844387076, 1.000000000000000000, 0.8660254037844387076, 1.000000000000000000, 0.8660254037844387076, 1.000000000000000000, 0.8660254037844387076, 1.000000000000000000, 0.8660254037844387076, 1.000000000000000000, 0.8660254037844387076, 1.000000000000000000, 0.8660254037844387076, 1.000000000000000000, 0.8660254037844387076, 1.000000000000000000, 0.8660254037844387076, 1.000000000000000000, 0.8660254037844387076, 1.000000000000000000, 0.8660254037844387076, 1.000000000000000000, 0.8660254037844387076, 1.000000000000000000, 0.8660254037844387076, 1.000000000000000000, 0.8660254037844387076, 1.000000000000000000, 0.8660254037844387076, 1.000000000000000000, 0.8660254037844387076, 1.000000000000000000, 0.8660254037844387076, 1.000000000000000000, 0.8660254037844387076, 1.000000000000000000, 0.8660254037844387076, 1.000000000000000000, 0.8660254037844387076, 1.000000000000000000, 0.8660254037844387076, 1.000000000000000000, 0.8660254037844387076, 1.000000000000000000, 0.8660254037844387076, 1.000000000000000000, 0.8660254037844387076, 1.000000000000000000, 0.8660254037844387076, 1.000000000000000000, 0.8660254037844387076, 1.000000000000000000, 0.8660254037844387076, 1.000000000000000000, 0.8660254037844387076, 1.000000000000000000, 0.8660254037844387076, 1.000000000000000000, 0.8660254037844387076, 1.000000000000000000, 0.8660254037844387076, 1.000000000000000000, 0.8660254037844387076, 1.000000000000000000, 0.8660254037844387076, 1.000000000000000000, 0.8660254037844387076, 1.000000000000000000, 0.8660254037844387076, 1.000000000000000000, 0.8660254037844387076, 1.000000000000000000, 0.8660254037844387076, 1.000000000000000000, 0.8660254037844387076, 1.000000000000000000, 0.8660254037844387076, 1.000000000000000000, 0.8660254037844387076, 1.000000000000000000, 0.8660254037844387076, 1.000000000000000000, 0.8660254037844387076, 1.000000000000000000, 0.8660254037844387076, 1.000000000000000000, 0.8660254037844387076, 1.000000000000000000, 0.8660254037844387076, 1.000000000000000000, 0.8660254037844387076, 1.000000000000000000, 0.8660254037844387076, 1.000000000000000000, 0.8660254037844387076, 1.000000000000000000, 0.8660254037844387076, 1.000000000000000000, 0.8660254037844387076, 1.000000000000000000, 0.8660254037844387076, 1.000000000000000000, 0.8660254037844387076, 1.000000000000000000, 0.8660254037844387076, 1.000000000000000000, 0.8660254037844387076, 1.000000000000000000, 0.8660254037844387076, 1.000000000000000000, 0.8660254037844387076, 1.000000000000000000, 0.8660254037844387076, 1.000000000000000000, 0.8660254037844387076, 1.000000000000000000, 0.8660254037844387076, 1.000000000000000000, 0.8660254037844387076, 1.000000000000000000, 0.8660254037844387076, 1.000000000000000000, 0.8660254037844387076, 1.000000000000000000, 0.8660254037844387076, 1.000000000000000000, 0.8660254037844387076, 1.000000000000000000, 0.8660254037844387076, 1.000000000000000000, 0.8660254037844387076, 1.000000000000000000, 0.8660254037844387076, 1.000000000000000000, 0.8660254037844387076, 1.000000000000000000, 0.8660254037844387076, 1.000000000000000000, 0.8660254037844387076, 1.000000000000000000, 0.8660254037844387076, 1.000000000000000000, 0.8660254037844387076, 1.000000000000000000, 0.8660254037844387076, 1.000000000000000000, 0.8660254037844387076, 1.000000000000000000, 0.8660254037844387076, 1.000000000000000000, 0.8660254037844387076, 1.000000000000000000, 0.8660254037844387076, 1.000000000000000000, 0.8660254037844387076, 1.000000000000000000, 0.8660254037844387076, 1.000000000000000000, 0.8660254037844387076, 1.000000000000000000, 0.8660254037844387076, 1.000000000000000000, 0.8660254037844387076, 1.000000000000000000, 0.8660254037844387076, 1.000000000000000000, 0.8660254037844387076, 1.000000000000000000, 0.8660254037844387076, 1.000000000000000000, 0.8660254037844387076, 1.000000000000000000, 0.8660254037844387076, 1.000000000000000000, 0.8660254037844387076, 1.000000000000000000, 0.8660254037844387076, 1.000000000000000000, 0.8660254037844387076, 1.000000000000000000, 0.8660254037844387076, 1.000000000000000000, 0.8660254037844387076, 1.000000000000000000, 0.8660254037844387076, 1.000000000000000000, 0.8660254037844387076, 1.000000000000000000, 0.8660254037844387076, 1.000000000000000000, 0.8660254037844387076, 1.000000000000000000, 0.8660254037844387076, 1.000000000000000000, 0.8660254037844387076, 1.000000000000000000, 0.8660254037844387076, 1.000000000000000000, 0.8660254037844387076, 1.000000000000000000, 0.8660254037844387076, 1.000000000000000000, 0.8660254037844387076, 1.000000000000000000, 0.8660254037844387076, 1.000000000000000000, 0.8660254037844387076, 1.000000000000000000) ) ) 
 REPRESENTATION_ITEM ( '' )  SURFACE ( )  );
#4282 = CARTESIAN_POINT ( 'NONE',  ( 2.918323747256291956, -1.167012588333454781, -1.282868673017246941 ) ) ;
#4283 = CARTESIAN_POINT ( 'NONE',  ( 8.134310703387671364E-16, 2.000000000682804924, -1.225000000000021849 ) ) ;
#4284 = CARTESIAN_POINT ( 'NONE',  ( -5.015590482412729756, 4.816220082428420923, 0.000000000000000000 ) ) ;
#4285 = CARTESIAN_POINT ( 'NONE',  ( -4.462041952228944730, 7.259447140025469203, -1.082531754730549967 ) ) ;
#4286 = CARTESIAN_POINT ( 'NONE',  ( 5.215394836314163562, -0.2642288504575221464, 1.806346989861665087 ) ) ;
#4287 = CARTESIAN_POINT ( 'NONE',  ( 2.975390029205773779, -0.1970676810524821521, 1.951864085487287959 ) ) ;
#4288 = CARTESIAN_POINT ( 'NONE',  ( -1.225000000000014078, -0.2083333326505250049, -0.7072540797572977045 ) ) ;
#4289 = CARTESIAN_POINT ( 'NONE',  ( -7.492852449846775897, 11.89341162479659531, 0.000000000000000000 ) ) ;
#4290 = CARTESIAN_POINT ( 'NONE',  ( 7.637320603199683866, 7.804628880021436288, -0.7998128361456281477 ) ) ;
#4291 = EDGE_CURVE ( 'NONE', #12260, #30915, #53572, .T. ) ;
#4292 = CARTESIAN_POINT ( 'NONE',  ( 5.092489908381383934, -1.177591669451777179, 1.763244422785560150 ) ) ;
#4293 = CARTESIAN_POINT ( 'NONE',  ( 5.820193082016415609, 10.01225203898631655, 0.000000000000000000 ) ) ;
#4294 = CARTESIAN_POINT ( 'NONE',  ( -10.64723070543352712, 11.31619066596094392, 0.7998128361456462443 ) ) ;
#4295 = CARTESIAN_POINT ( 'NONE',  ( 2.254815949590884827, -0.5480598642870064818, -1.996355599893632649 ) ) ;
#4297 = CARTESIAN_POINT ( 'NONE',  ( 1.364683531249986537, -0.5322916663252452718, -0.7879004041258309554 ) ) ;
#4296 = CARTESIAN_POINT ( 'NONE',  ( -11.94980361058169116, 10.89999999999999858, 1.099999999999994982 ) ) ;
#4299 = ORIENTED_EDGE ( 'NONE', *, *, #14312, .F. ) ;
#4298 = CARTESIAN_POINT ( 'NONE',  ( 4.512477240926440203, -2.220771887297602110, -0.05487108470654011860 ) ) ;
#4300 = CARTESIAN_POINT ( 'NONE',  ( 1.952162490553134955, -2.103507816325803415, -0.9273050526804761384 ) ) ;
#4301 = CARTESIAN_POINT ( 'NONE',  ( 9.083599731475988648, 10.66024977721925104, 1.082531754730549967 ) ) ;
#4303 = CARTESIAN_POINT ( 'NONE',  ( 1.642778471875000035, -1.976041666188709689, -2.845375778867859751 ) ) ;
#4302 = CARTESIAN_POINT ( 'NONE',  ( 5.076602173674213070, 4.887400388900169368, 0.000000000000000000 ) ) ;
#4304 = CARTESIAN_POINT ( 'NONE',  ( -9.904322480959008246, 3.508507969777028279, 6.779889285468879478 ) ) ;
#4305 = FACE_BOUND ( 'NONE', #212026, .T. ) ;
#4306 = CARTESIAN_POINT ( 'NONE',  ( 3.463059065379545221, -1.560675823418774533, 1.104941681961457256 ) ) ;
#4307 = CARTESIAN_POINT ( 'NONE',  ( -0.5161058020549844638, 6.726351010739881175, -3.601801347653132090 ) ) ;
#4308 = CARTESIAN_POINT ( 'NONE',  ( 3.803458131734431813, -0.5007765277059565978, 1.650448229862747196 ) ) ;
#4309 = B_SPLINE_CURVE_WITH_KNOTS ( 'NONE', 3,
 ( #211172, #199174, #116946, #212239, #98511, #197065, #196018, #82243, #114817, #50820, #62797, #133174, #128959, #112694, #63872, #214334, #148334, #12975 ),
 .UNSPECIFIED., .F., .F.,
 ( 4, 2, 2, 2, 2, 2, 2, 2, 4 ),
 ( 0.000000000000000000, 0.0006562923895199564888, 0.001312584779039912978, 0.001968877168559869575, 0.002625169558079825955, 0.003281461947599781902, 0.003937754337119737415, 0.004594046726639694662, 0.005250339116159651043 ),
 .UNSPECIFIED. ) ;
#4310 = CARTESIAN_POINT ( 'NONE',  ( 2.149625371984189126, 1.976669504256656218, -0.3981124878784659815 ) ) ;
#4311 = CARTESIAN_POINT ( 'NONE',  ( 4.008600857689972763, -2.199693827605917917, 0.6672659128543911855 ) ) ;
#4312 = CARTESIAN_POINT ( 'NONE',  ( -3.147653791585729444, 8.999999999999998224, 2.419999999999999485 ) ) ;
#4313 = CARTESIAN_POINT ( 'NONE',  ( 6.516252164726425100, -0.9909202252585481707, -1.858390699035996407 ) ) ;
#4314 = CARTESIAN_POINT ( 'NONE',  ( -5.560252395380252288, 7.580323442733986283, 1.443375672974058777 ) ) ;
#4315 = VERTEX_POINT ( 'NONE', #187828 ) ;
#4316 = CARTESIAN_POINT ( 'NONE',  ( 5.184699891622216228, -0.2167559868061739725, -1.756304918635148704 ) ) ;
#4318 = CARTESIAN_POINT ( 'NONE',  ( 0.4633194693007875453, 0.2188196410306940398, -2.281803551658576179 ) ) ;
#4317 = CARTESIAN_POINT ( 'NONE',  ( 5.854088466050551887, 10.05179665369283981, 0.7998128361456341429 ) ) ;
#4319 = CARTESIAN_POINT ( 'NONE',  ( 6.714805130922314014, -0.1276373473727103192, 1.811824464382847832 ) ) ;
#4320 = CARTESIAN_POINT ( 'NONE',  ( -8.106849506328558164, 8.422688943663599659, 0.000000000000000000 ) ) ;
#4321 = CARTESIAN_POINT ( 'NONE',  ( 5.191441776010861986, -0.7909675746368142191, 2.043907961996515699 ) ) ;
#4322 = CARTESIAN_POINT ( 'NONE',  ( -5.340986169140711226, 5.195848383611072485, 0.000000000000000000 ) ) ;
#4323 = CARTESIAN_POINT ( 'NONE',  ( 0.6801582343749900117, -0.4114583329919083154, -1.178068619123855409 ) ) ;
#4324 = CARTESIAN_POINT ( 'NONE',  ( -0.1296875068448159751, 0.001480089298542403009, -1.826395826379861864 ) ) ;
#4325 = CARTESIAN_POINT ( 'NONE',  ( 0.2038950025188591975, -1.678810847859620869, -1.376375048264495859 ) ) ;
#4326 = CARTESIAN_POINT ( 'NONE',  ( 1.587125413319636635, 1.679225032509903404, 1.116207499648947943 ) ) ;
#4327 = AXIS2_PLACEMENT_3D ( 'NONE', #23364, #22282, #38574 ) ;
#4328 = CARTESIAN_POINT ( 'NONE',  ( 0.7499999999999885647, -0.7354166659838470288, 1.299038105676657340 ) ) ;
#4329 = CARTESIAN_POINT ( 'NONE',  ( 4.617753627809100259, -1.889021752119159459, 0.3773520080231194673 ) ) ;
#4330 = CARTESIAN_POINT ( 'NONE',  ( -1.402160292154681736E-14, 11.67187500034140157, 1.575800808251682339 ) ) ;
#4331 = CARTESIAN_POINT ( 'NONE',  ( 1.459560619642571000, -1.873223059428649639, 1.193793739728800762 ) ) ;
#4333 = ORIENTED_EDGE ( 'NONE', *, *, #126049, .T. ) ;
#4332 = CARTESIAN_POINT ( 'NONE',  ( 8.028399517586572998, 12.51821653715971472, -0.7998128361456352531 ) ) ;
#4335 = AXIS2_PLACEMENT_3D ( 'NONE', #96713, #117247, #46885 ) ;
#4334 = CARTESIAN_POINT ( 'NONE',  ( 4.175484721775176489, 3.976419294354625933, -0.06592222766770190756 ) ) ;
#4336 = CARTESIAN_POINT ( 'NONE',  ( -0.4437274321079128780, 2.826106777454868713, -1.950208266479945163 ) ) ;
#4338 = EDGE_CURVE ( 'NONE', #17872, #210292, #167413, .T. ) ;
#4337 = CARTESIAN_POINT ( 'NONE',  ( 3.728655938958122196, 4.308852335994623139, -1.199719254218446718 ) ) ;
#4339 = CARTESIAN_POINT ( 'NONE',  ( -3.475000000000000533, -2.450000000000000622, 0.000000000000000000 ) ) ;
#4340 = DIRECTION ( 'NONE',  ( 0.000000000000000000, -1.000000000000000000, 0.000000000000000000 ) ) ;
#4341 = CARTESIAN_POINT ( 'NONE',  ( 3.878220372009810291, -0.1751146298830832670, -1.731616844506628006 ) ) ;
#4342 = CARTESIAN_POINT ( 'NONE',  ( 2.312880826517309085, -1.518475810973318074, 1.242258525517292433 ) ) ;
#4344 = CARTESIAN_POINT ( 'NONE',  ( 0.6823417656249899377, 3.238541667008085323, -1.181850606188754593 ) ) ;
#4343 = CARTESIAN_POINT ( 'NONE',  ( 4.150767584078112193, 7.994312614733129152, 0.7998128361456321445 ) ) ;
#4345 = CARTESIAN_POINT ( 'NONE',  ( -5.899175937014327076, 6.007822909898694164, -0.1935691424272238670 ) ) ;
#4346 = CARTESIAN_POINT ( 'NONE',  ( -6.042630808230841359E-15, -1.968749999044084875, 3.474999999999999645 ) ) ;
#4347 = CARTESIAN_POINT ( 'NONE',  ( 0.3091261446717024630, -1.657722840873154135, 1.227268292441574538 ) ) ;
#4348 = CARTESIAN_POINT ( 'NONE',  ( -6.509886312855995172, 10.74661779830734254, -0.7998128361456291469 ) ) ;
#4349 = CARTESIAN_POINT ( 'NONE',  ( -4.568734577680887199, 6.353276312092901890, -1.443375672974051449 ) ) ;
#4350 = CARTESIAN_POINT ( 'NONE',  ( 5.278529876733943915, -0.4946281652532491524, -1.954780475499573900 ) ) ;
#4351 = CARTESIAN_POINT ( 'NONE',  ( 0.8665589547518313118, 1.117614298721156585, 1.967126077831014896 ) ) ;
#4353 = VERTEX_POINT ( 'NONE', #200857 ) ;
#4352 = CARTESIAN_POINT ( 'NONE',  ( -4.882907879216086933, 8.848476292394087395, -0.7998128361456281477 ) ) ;
#4355 = EDGE_CURVE ( 'NONE', #77820, #55444, #175748, .T. ) ;
#4354 = CARTESIAN_POINT ( 'NONE',  ( 0.7499999999999885647, 0.3479166673494848983, -1.299038105676652899 ) ) ;
#4356 = CARTESIAN_POINT ( 'NONE',  ( 1.686563950722594685, -0.2693046698774223535, -1.850923959389898288 ) ) ;
#4357 = CARTESIAN_POINT ( 'NONE',  ( -0.01748474828899664046, -1.733701077801694579, -0.04590633323625636919 ) ) ;
#4358 = CARTESIAN_POINT ( 'NONE',  ( 4.634432875810733599, 0.3748786239917039631, 2.159109584303263940 ) ) ;
#4359 = CARTESIAN_POINT ( 'NONE',  ( 5.948310197725324322, 2.304532173486303570, 0.1212388396696506970 ) ) ;
#4360 = CARTESIAN_POINT ( 'NONE',  ( 0.7431281084272289839, -1.767980789219452342, 1.058748425497215262 ) ) ;
#4361 = CARTESIAN_POINT ( 'NONE',  ( 3.820204237656314561, 1.844379349147889480, 0.6080220579995837538 ) ) ;
#4362 = CARTESIAN_POINT ( 'NONE',  ( -3.538314903042294457, 6.111489239315849531, 1.082531754730560403 ) ) ;
#4363 = CARTESIAN_POINT ( 'NONE',  ( 5.624238404463478780, 1.114819804898508515, -1.501858222471161408 ) ) ;
#4364 = CARTESIAN_POINT ( 'NONE',  ( -0.6801582343750161019, 0.6822916670080614310, 1.178068619123810334 ) ) ;
#4365 = CARTESIAN_POINT ( 'NONE',  ( 4.096327398540238640, -0.3419367296172080017, 1.987046374476949095 ) ) ;
#4366 = CARTESIAN_POINT ( 'NONE',  ( -3.917943204224921150, 5.594019709727598766, -1.443375672974051449 ) ) ;
#4367 = CARTESIAN_POINT ( 'NONE',  ( -4.796552484184649856, 8.818004674849227342, -0.7998128361456362523 ) ) ;
#4368 = CARTESIAN_POINT ( 'NONE',  ( 7.262363838414439776, 11.62450824479221900, 0.7998128361456462443 ) ) ;
#4370 = CARTESIAN_POINT ( 'NONE',  ( 7.720982897393571243, -5.907420853759296264, -7.834948825496923952 ) ) ;
#4369 = CARTESIAN_POINT ( 'NONE',  ( 2.473051018021198200, 0.08991741065280876855, -1.823594477012622228 ) ) ;
#4371 = CARTESIAN_POINT ( 'NONE',  ( -4.122561227007127016, 6.967349310553715647, 1.199719254218452935 ) ) ;
#4372 = DIRECTION ( 'NONE',  ( 1.000000000000000000, -0.000000000000000000, -0.000000000000000000 ) ) ;
#4373 = CARTESIAN_POINT ( 'NONE',  ( -10.36733242867369142, 5.031604590660524678, 7.295138277318285347 ) ) ;
#4374 = ORIENTED_EDGE ( 'NONE', *, *, #96704, .T. ) ;
#4375 = CARTESIAN_POINT ( 'NONE',  ( -5.221298554594238084, 8.145246509451649075, 1.082531754730549967 ) ) ;
#4376 = CARTESIAN_POINT ( 'NONE',  ( -6.775478006741569637, -7.217909409563595169, 6.775478006741592729 ) ) ;
#4377 = CARTESIAN_POINT ( 'NONE',  ( 2.969872605471133742, 6.602209919732136001, 0.2729278363745436531 ) ) ;
#4378 = CARTESIAN_POINT ( 'NONE',  ( 6.094400524283400067, -1.078572965507901715, 1.707356775630589851 ) ) ;
#4380 = ORIENTED_EDGE ( 'NONE', *, *, #59990, .T. ) ;
#4379 = CARTESIAN_POINT ( 'NONE',  ( 6.358078514681034576, 0.8530912398192547208, -2.051143523256500067 ) ) ;
#4381 = CARTESIAN_POINT ( 'NONE',  ( -6.099189001301292379, 8.209082816308541197, 1.599625672291263179 ) ) ;
#4382 = CARTESIAN_POINT ( 'NONE',  ( 5.681030059326015014, 6.586622143090519188, -1.199719254218445830 ) ) ;
#4383 = CARTESIAN_POINT ( 'NONE',  ( 5.823136237661057812, -0.05295972098229295016, 2.060385759621866431 ) ) ;
#4384 = CARTESIAN_POINT ( 'NONE',  ( 3.428361437285933455, -1.528740797599713153, -1.314997250469025936 ) ) ;
#4385 = EDGE_LOOP ( 'NONE', ( #39707, #165219, #127190, #169715 ) ) ;
#4386 = ORIENTED_EDGE ( 'NONE', *, *, #83840, .T. ) ;
#4387 = CARTESIAN_POINT ( 'NONE',  ( 10.51593585047793233, 11.11323312775290439, -3.554043120631340535 ) ) ;
#4388 = CARTESIAN_POINT ( 'NONE',  ( 2.679707916995359263, 6.278076336469897711, -0.7998128361456291469 ) ) ;
#4390 = ORIENTED_EDGE ( 'NONE', *, *, #129415, .F. ) ;
#4389 = CARTESIAN_POINT ( 'NONE',  ( -7.228432174741334038, 8.462200954400218578, -1.199719254218452047 ) ) ;
#4391 = CARTESIAN_POINT ( 'NONE',  ( 4.595358334023878832, 8.489709390108890474, -0.01759220550971198060 ) ) ;
#4392 = CARTESIAN_POINT ( 'NONE',  ( 3.954453749441131816, 1.458333106491338960, 1.392332789497241263 ) ) ;
#4393 = CARTESIAN_POINT ( 'NONE',  ( 3.890429890068654917, 1.554390554365025379, -0.9864425779082321988 ) ) ;
#4394 = CARTESIAN_POINT ( 'NONE',  ( 3.809456170543648046, 8.470288933811609411, 2.500000000000000444 ) ) ;
#4395 = CARTESIAN_POINT ( 'NONE',  ( 2.579137097422959712, -2.208767019342866345, -0.6684429575241066512 ) ) ;
#4396 = CARTESIAN_POINT ( 'NONE',  ( 4.411198876399872404, 6.239761003923544713, -1.599625672291273171 ) ) ;
#4397 = CARTESIAN_POINT ( 'NONE',  ( 4.798204600472657511, -2.160985683756014630, -0.05834674948757002932 ) ) ;
#4398 = CARTESIAN_POINT ( 'NONE',  ( 8.392660782059197189, 9.750191319612612872, 1.199719254218462483 ) ) ;
#4399 = CARTESIAN_POINT ( 'NONE',  ( 6.567912610837368881, -1.126952994821692533, 1.456688911285822119 ) ) ;
#4400 = CARTESIAN_POINT ( 'NONE',  ( -5.922214171070950606, 5.803671375871217286, -0.7998128361456291469 ) ) ;
#4401 = CARTESIAN_POINT ( 'NONE',  ( -4.911285141672522059, 4.693790260148114513, 0.3511878651327460243 ) ) ;
#4402 = CARTESIAN_POINT ( 'NONE',  ( 1.166320357434693644, 2.840374313856441013, 0.7750000000000117906 ) ) ;
#4403 = CIRCLE ( 'NONE', #77098, 0.07999999999999998779 ) ;
#4404 = CARTESIAN_POINT ( 'NONE',  ( 2.641296366799699147, -1.384790685969448099, -1.257831364775918503 ) ) ;
#4405 = CIRCLE ( 'NONE', #87472, 0.08000000000000040412 ) ;
#4406 = CARTESIAN_POINT ( 'NONE',  ( 0.4386656386161046917, 0.3326637607320662160, 1.942932543480476726 ) ) ;
#4407 = CARTESIAN_POINT ( 'NONE',  ( -1.001543065824772872E-14, 5.571875000341416140, 1.575800808251672791 ) ) ;
#4408 = CARTESIAN_POINT ( 'NONE',  ( 1.172829962703396456, -1.397616723802884708, 1.707921395779465890 ) ) ;
#4409 = ORIENTED_EDGE ( 'NONE', *, *, #182370, .F. ) ;
#4410 = CARTESIAN_POINT ( 'NONE',  ( 4.529832720297257254, 8.298905583739861314, 0.000000000000000000 ) ) ;
#4411 = CARTESIAN_POINT ( 'NONE',  ( 4.487912541323413329, 5.194651705420806564, 1.199719254218462483 ) ) ;
#4412 = CARTESIAN_POINT ( 'NONE',  ( -4.303823697334223652, 7.108545849276850959, -1.199719254218452047 ) ) ;
#4413 = CARTESIAN_POINT ( 'NONE',  ( 11.94980361723123785, 13.50238056585427060, 1.099999926404769290 ) ) ;
#4414 = CARTESIAN_POINT ( 'NONE',  ( 6.649300054797159909, -1.583302550941813491, -1.174460211130315512 ) ) ;
#4415 = CARTESIAN_POINT ( 'NONE',  ( 6.516287943725491694, -1.081378002916585368, -2.038673766938512877 ) ) ;
#4416 = CARTESIAN_POINT ( 'NONE',  ( 6.725070007137362360, -1.702231675683645973, -0.7527390810756880990 ) ) ;
#4417 = CARTESIAN_POINT ( 'NONE',  ( 4.276276908810595856, -1.056066993903046924, -1.771547272865436673 ) ) ;
#4418 = CARTESIAN_POINT ( 'NONE',  ( 6.507550544879468823, 6.694489845221929691, -0.7216878364870257245 ) ) ;
#4419 = VECTOR ( 'NONE', #202531, 1000.000000000000000 ) ;
#4420 = CARTESIAN_POINT ( 'NONE',  ( 6.690022453700429139, 6.769724048930809701, 0.7998128361456331437 ) ) ;
#4421 = ORIENTED_EDGE ( 'NONE', *, *, #70055, .F. ) ;
#4422 = CARTESIAN_POINT ( 'NONE',  ( 8.893785580440313865, 9.478430720042945623, 1.040834085586084257E-14 ) ) ;
#4423 = CARTESIAN_POINT ( 'NONE',  ( -1.364683531250012516, 3.801041667008087099, -0.7879004041258300672 ) ) ;
#4424 = CARTESIAN_POINT ( 'NONE',  ( 4.000000000000012434, 4.999999999999997335, 0.7500000000000006661 ) ) ;
#4425 = CARTESIAN_POINT ( 'NONE',  ( 5.490689023410166847, 5.508151403507724808, -0.7216878364870207285 ) ) ;
#4426 = CARTESIAN_POINT ( 'NONE',  ( 6.268071979561871565, -2.155543878041016992, 0.2595383615264702515 ) ) ;
#4428 = CARTESIAN_POINT ( 'NONE',  ( 5.196754805642953556, 1.508532920973480795, 1.055450849767838317 ) ) ;
#4427 = DIRECTION ( 'NONE',  ( 0.9885327375000381167, 0.000000000000000000, 0.1510067114093955609 ) ) ;
#4429 = ADVANCED_FACE ( 'NONE', ( #170516 ), #84039, .T. ) ;
#4430 = CARTESIAN_POINT ( 'NONE',  ( 5.374112064994988280, 6.309506852805883526, -1.073983825876674514 ) ) ;
#4431 = FACE_OUTER_BOUND ( 'NONE', #192626, .T. ) ;
#4432 = CARTESIAN_POINT ( 'NONE',  ( 0.3681424317822541425, -1.226883886190757611, 1.412057460252094554 ) ) ;
#4433 = CARTESIAN_POINT ( 'NONE',  ( -4.670247306389155639, 7.079074041166477649, 1.395957953274113983 ) ) ;
#4434 = CARTESIAN_POINT ( 'NONE',  ( -10.87798840695972302, -6.646059016331640201, 0.1412570932018041570 ) ) ;
#4435 = CARTESIAN_POINT ( 'NONE',  ( 5.494857653270467601, 7.581134149042087600, -1.337725346733337872 ) ) ;
#4436 = CARTESIAN_POINT ( 'NONE',  ( 0.8207898099904624711, 1.447681275506585541, -1.249484660484905030 ) ) ;
#4437 = CARTESIAN_POINT ( 'NONE',  ( 2.377515701973518691, 1.086635889927405341, 1.396898309679272865 ) ) ;
#4438 = CARTESIAN_POINT ( 'NONE',  ( -0.05814382529654647802, -1.176414490726215734, -1.508152472379259867 ) ) ;
#4440 = CARTESIAN_POINT ( 'NONE',  ( 4.640194291141960470, 0.7370120463812566136, 1.768359169405645304 ) ) ;
#4439 = CARTESIAN_POINT ( 'NONE',  ( -9.667127221743832877, 11.23706883257798772, 1.199719254218462483 ) ) ;
#4441 = CARTESIAN_POINT ( 'NONE',  ( -15.75000000000000000, 10.19999999999998153, 3.599999999999999201 ) ) ;
#4442 = CARTESIAN_POINT ( 'NONE',  ( 5.476995390384709061, 1.819097369218507732, 0.7554879866787550524 ) ) ;
#4443 = CARTESIAN_POINT ( 'NONE',  ( 6.099869210120771434, 1.395876734396967356, 1.460039163664628159 ) ) ;
#4444 = CARTESIAN_POINT ( 'NONE',  ( -1.628336349302364372, -1.162346226930493387, 1.455206426644551243 ) ) ;
#4445 = CARTESIAN_POINT ( 'NONE',  ( 3.889402362484274622, 1.354500474538382626, 1.290456140434749654 ) ) ;
#4447 = VERTEX_POINT ( 'NONE', #54637 ) ;
#4446 = CARTESIAN_POINT ( 'NONE',  ( 6.164645834669005175, -1.214467819493704415, 1.225147371335724156 ) ) ;
#4449 = CARTESIAN_POINT ( 'NONE',  ( 3.606105671554957759, 4.269840040644637291, -1.082531754730543083 ) ) ;
#4448 = CARTESIAN_POINT ( 'NONE',  ( 3.616033620774202983, -2.174319932014677548, 0.3768175846284789743 ) ) ;
#4450 = CARTESIAN_POINT ( 'NONE',  ( -1.201851678989727383E-14, 3.259375000341420581, -1.575800808251660134 ) ) ;
#4451 = CARTESIAN_POINT ( 'NONE',  ( 0.2915633711191143451, -1.886499572934543956, 0.8344948317597818965 ) ) ;
#4452 = CARTESIAN_POINT ( 'NONE',  ( 7.287671262545424966, 8.461036880179857889, -1.199719254218451159 ) ) ;
#4453 = CARTESIAN_POINT ( 'NONE',  ( -10.17947440576205054, 10.77047498301088346, 0.7998128361456462443 ) ) ;
#4454 = CARTESIAN_POINT ( 'NONE',  ( -3.518398841103404173, 15.44797950387303054, -11.43484029727943607 ) ) ;
#4455 = CARTESIAN_POINT ( 'NONE',  ( -3.419783357106924715, -0.02451629128698711024, -0.3994745426820112688 ) ) ;
#4456 = CARTESIAN_POINT ( 'NONE',  ( -4.866920030118153662, 7.975534482151904747, -1.006773929442051685 ) ) ;
#4457 = EDGE_LOOP ( 'NONE', ( #92481, #97816, #3438, #190730, #136190, #88897 ) ) ;
#4458 = CARTESIAN_POINT ( 'NONE',  ( 3.051297593704501043, 1.777051743073382761, -1.062048545217339823 ) ) ;
#4459 = CARTESIAN_POINT ( 'NONE',  ( 1.499999999999987121, 4.795833333333353821, -0.8660254037844323793 ) ) ;
#4460 = CARTESIAN_POINT ( 'NONE',  ( 4.822949958159288286, 6.649860922651058992, -1.599625672291256295 ) ) ;
#4461 = CARTESIAN_POINT ( 'NONE',  ( -6.502837976706968171, 6.831778935668112673, 0.5908271424688981144 ) ) ;
#4462 = CARTESIAN_POINT ( 'NONE',  ( 1.313155450441779726, 1.649776782055782709, -1.164742093282441937 ) ) ;
#4463 = LINE ( 'NONE', #184302, #7915 ) ;
#4465 = CARTESIAN_POINT ( 'NONE',  ( 8.107412671292031803, 11.44210330227398487, 1.082531754730557072 ) ) ;
#4464 = CARTESIAN_POINT ( 'NONE',  ( 0.07499057489264347731, 7.629137130509110243, -2.555503484197537922 ) ) ;
#4466 = CARTESIAN_POINT ( 'NONE',  ( 6.116564501996816894, 0.5879282371138266905, -1.928457050679150298 ) ) ;
#4467 = CARTESIAN_POINT ( 'NONE',  ( 5.700375016119385130, 1.281441245451527600, -1.424251128553160273 ) ) ;
#4468 = FACE_BOUND ( 'NONE', #29943, .T. ) ;
#4469 = CARTESIAN_POINT ( 'NONE',  ( 3.544632465004614374, -1.790652189326558563, 1.263247045326251872 ) ) ;
#4470 =( BOUNDED_CURVE ( )  B_SPLINE_CURVE ( 2, ( #155751, #19326, #53979 ),
 .UNSPECIFIED., .F., .T. ) 
 B_SPLINE_CURVE_WITH_KNOTS ( ( 3, 3 ),
 ( 0.4749999999999995892, 0.4816879153505086442 ),
 .UNSPECIFIED. ) 
 CURVE ( )  GEOMETRIC_REPRESENTATION_ITEM ( )  RATIONAL_B_SPLINE_CURVE ( ( 1.000000000000006217, 0.8924787089670062068, 0.9575398082074682016 ) ) 
 REPRESENTATION_ITEM ( '' )  );
#4471 = CARTESIAN_POINT ( 'NONE',  ( -0.7500000000000215383, 3.972916667349481123, 1.299038105676671107 ) ) ;
#4472 = CARTESIAN_POINT ( 'NONE',  ( 2.935702856749935918, -1.841876368404654629, 0.5141854427313449216 ) ) ;
#4473 = CARTESIAN_POINT ( 'NONE',  ( -3.906720819032141190, 7.709591388846142479, -0.7998128361456281477 ) ) ;
#4474 = CARTESIAN_POINT ( 'NONE',  ( 2.860407222358956503, 6.280966159486672140, 0.7216878364870338292 ) ) ;
#4476 = CARTESIAN_POINT ( 'NONE',  ( 0.9136856707930467447, -1.281379520587552889, -1.556895127150646374 ) ) ;
#4475 = CARTESIAN_POINT ( 'NONE',  ( 10.14031698345507060, 3.934660213246449434, -5.561808457406779205 ) ) ;
#4477 = CARTESIAN_POINT ( 'NONE',  ( -0.6823417656250003738, 10.96354166700806765, 1.181850606188754593 ) ) ;
#4479 = CARTESIAN_POINT ( 'NONE',  ( -4.847922445338252118, 7.813604065273374921, -1.199719254218453823 ) ) ;
#4478 = CARTESIAN_POINT ( 'NONE',  ( 6.480031355044912900, -2.148842909532014289, -0.4297212958329286736 ) ) ;
#4481 = ORIENTED_EDGE ( 'NONE', *, *, #22105, .F. ) ;
#4480 = CARTESIAN_POINT ( 'NONE',  ( 3.434305118180380756, 1.682496158873967529, 0.3786907865064632062 ) ) ;
#4482 = CARTESIAN_POINT ( 'NONE',  ( 0.1394461523057500818, 4.098109337479769465, -2.274588453029251500 ) ) ;
#4483 = CARTESIAN_POINT ( 'NONE',  ( 8.606728586576791074, 8.935604860628076906, 0.7998128361456462443 ) ) ;
#4484 = CARTESIAN_POINT ( 'NONE',  ( 3.499976210622149253, 7.235056012367825140, 0.7998128361456321445 ) ) ;
#4485 = CARTESIAN_POINT ( 'NONE',  ( -1.420000000000077423, 7.240846818246208905, 4.154462424328226433 ) ) ;
#4486 = CARTESIAN_POINT ( 'NONE',  ( 1.064813361795993618, 1.487921858168140377, -1.278797858372302088 ) ) ;
#4487 = DIRECTION ( 'NONE',  ( -1.224646799147343346E-16, 0.000000000000000000, -1.000000000000000000 ) ) ;
#4488 = CARTESIAN_POINT ( 'NONE',  ( 5.529027716274630855, 5.344953845275508542, 1.040834085586084257E-14 ) ) ;
#4489 = PLANE ( 'NONE',  #154520 ) ;
#4490 = ORIENTED_EDGE ( 'NONE', *, *, #99349, .T. ) ;
#4492 = CIRCLE ( 'NONE', #21638, 10.24999999999999822 ) ;
#4491 = CARTESIAN_POINT ( 'NONE',  ( -2.927345865710861577E-15, -6.948429295162506847, 9.261794192843273876 ) ) ;
#4493 = ORIENTED_EDGE ( 'NONE', *, *, #181245, .T. ) ;
#4494 = CARTESIAN_POINT ( 'NONE',  ( 4.459482644723921752, -1.403152132390030449, -1.145693287117461656 ) ) ;
#4495 = ORIENTED_EDGE ( 'NONE', *, *, #87710, .F. ) ;
#4496 = CARTESIAN_POINT ( 'NONE',  ( 9.134442807305049428, 11.67993591332117376, 1.599625672291281386 ) ) ;
#4497 = COLOUR_RGB ( '', 0.08235294, 0.09019608, 0.10196078) ;
#4498 = CARTESIAN_POINT ( 'NONE',  ( 3.088225128862704949, 6.824956093640315302, 0.7998128361456281477 ) ) ;
#4499 = CARTESIAN_POINT ( 'NONE',  ( 5.109926359719781708, -0.6467658019376655298, 1.692270648455761917 ) ) ;
#4500 = CARTESIAN_POINT ( 'NONE',  ( 7.987161891782087686, 8.490979426600148372, -0.7216878364870317197 ) ) ;
#4501 = CARTESIAN_POINT ( 'NONE',  ( 5.096651299933133039, 6.508523278119453082, -1.213691435513279293 ) ) ;
#4503 = CARTESIAN_POINT ( 'NONE',  ( -1.364683531250014514, 15.08854166700806587, -0.7879004041258335089 ) ) ;
#4502 = CARTESIAN_POINT ( 'NONE',  ( 5.195690723081275664, -1.315925274417349522, -1.316268238436297144 ) ) ;
#4504 = CARTESIAN_POINT ( 'NONE',  ( 2.460426067449926535, -1.833815074015308300, -0.5538200352182551800 ) ) ;
#4505 = CARTESIAN_POINT ( 'NONE',  ( -6.385081391588430577, 6.907945078588741517, 0.8473268098342846555 ) ) ;
#4506 = CARTESIAN_POINT ( 'NONE',  ( -10.45142907045522129, 5.144535043903895932, -5.216774619840575333 ) ) ;
#4507 = CARTESIAN_POINT ( 'NONE',  ( -0.7500000000000215383, 3.191666666666689967, 1.299038105676671107 ) ) ;
#4508 = CARTESIAN_POINT ( 'NONE',  ( -1.734723475976807094E-15, 2.999999999999988898, -6.938893903907228378E-15 ) ) ;
#4509 = CARTESIAN_POINT ( 'NONE',  ( 7.307481608085759639, 7.627742752295940676, 1.040834085586084257E-14 ) ) ;
#4510 = CARTESIAN_POINT ( 'NONE',  ( -4.386226389220933441, 5.076017861301227008, -1.199719254218446718 ) ) ;
#4511 =( NAMED_UNIT ( * ) SI_UNIT ( $, .STERADIAN. ) SOLID_ANGLE_UNIT ( ) );
#4512 = CARTESIAN_POINT ( 'NONE',  ( -6.448838341955544173, 7.552674816150118708, 1.199719254218452047 ) ) ;
#4513 = CARTESIAN_POINT ( 'NONE',  ( 1.324293675337850695, 2.015212547500934814, 0.5562262626958893730 ) ) ;
#4514 = CARTESIAN_POINT ( 'NONE',  ( 6.201928923608456046, 6.200281597156833691, 0.7998128361456352531 ) ) ;
#4515 = CARTESIAN_POINT ( 'NONE',  ( 6.282248997152713343, -1.030047846951231971, 1.627708832905690350 ) ) ;
#4516 = CARTESIAN_POINT ( 'NONE',  ( -5.416646063859567484, 6.278174148379618735, 1.199719254218450271 ) ) ;
#4517 = CARTESIAN_POINT ( 'NONE',  ( 2.203868028057700990, -1.825262823911228072, 0.04193083753635528516 ) ) ;
#4518 = CARTESIAN_POINT ( 'NONE',  ( 9.741349722503858999, 13.15934765701661391, 8.090281636115273400 ) ) ;
#4519 = CARTESIAN_POINT ( 'NONE',  ( 2.373185085050379506, -1.665764800640230803, -0.9392108107411781814 ) ) ;
#4520 = CARTESIAN_POINT ( 'NONE',  ( 1.803111746996020948, -1.665554870236161333, 1.050892442246372349 ) ) ;
#4521 = CARTESIAN_POINT ( 'NONE',  ( 3.491681510897004959, -1.939965067831977530, -0.09248793024771610749 ) ) ;
#4522 = ORIENTED_EDGE ( 'NONE', *, *, #24691, .F. ) ;
#4523 = CARTESIAN_POINT ( 'NONE',  ( -3.644109427023046521, 7.473487774827342278, 0.000000000000000000 ) ) ;
#4525 = CARTESIAN_POINT ( 'NONE',  ( 4.183913158364858553, 2.056144659531285779, -0.5182805708664262045 ) ) ;
#4524 = CARTESIAN_POINT ( 'NONE',  ( 7.075376061485196821, 9.347967719856493218, 1.599625672291268286 ) ) ;
#4526 = FACE_OUTER_BOUND ( 'NONE', #155740, .T. ) ;
#4527 = CARTESIAN_POINT ( 'NONE',  ( 8.235688245297327015, 11.69572115523387268, -1.199719254218446718 ) ) ;
#4528 = CARTESIAN_POINT ( 'NONE',  ( 6.006184860439112150, 6.084034629330242971, -0.5924424362405518174 ) ) ;
#4529 = DIRECTION ( 'NONE',  ( 1.000000000000000000, 1.725633230170963762E-31, 8.638326563840814399E-31 ) ) ;
#4530 = AXIS2_PLACEMENT_3D ( 'NONE', #162845, #130413, #147660 ) ;
#4531 = CARTESIAN_POINT ( 'NONE',  ( 6.550524494058025837, 7.671308660269694712, -1.199719254218452047 ) ) ;
#4532 = CARTESIAN_POINT ( 'NONE',  ( 0.4499999999999747535, 4.000000000000003553, -5.377642775528101993E-14 ) ) ;
#4533 = CARTESIAN_POINT ( 'NONE',  ( 3.932112477472641920, 0.9751300899686901058, -1.543267412809447681 ) ) ;
#4534 = CARTESIAN_POINT ( 'NONE',  ( 0.2036857628631080219, -1.599406074100502506, -1.314310892166506317 ) ) ;
#4535 = CARTESIAN_POINT ( 'NONE',  ( -9.869972641068651242, 11.57768483841065787, 1.082531754730558626 ) ) ;
#4536 = CARTESIAN_POINT ( 'NONE',  ( -4.785410049391000342, 8.260660143818395085, 0.8633373473483215710 ) ) ;
#4537 = CARTESIAN_POINT ( 'NONE',  ( 0.000000000000000000, -8.233137084989836652, 0.000000000000000000 ) ) ;
#4538 = CARTESIAN_POINT ( 'NONE',  ( 4.610133579271312954, -0.8000244862099057386, -1.691074300901610261 ) ) ;
#4539 = CARTESIAN_POINT ( 'NONE',  ( 8.749089199520284410, 9.101692242395490240, 0.7998128361456481317 ) ) ;
#4540 = CARTESIAN_POINT ( 'NONE',  ( 2.648949911425259263, -1.601578617359520340, 1.070393023584510050 ) ) ;
#4541 = CARTESIAN_POINT ( 'NONE',  ( 6.965691013979927959, -0.4331334938386353084, 1.920344510276908112 ) ) ;
#4542 = EDGE_CURVE ( 'NONE', #29585, #38980, #65003, .T. ) ;
#4543 = CARTESIAN_POINT ( 'NONE',  ( 4.864678189204997949, 4.569879397027603929, 0.7998128361456341429 ) ) ;
#4544 = CARTESIAN_POINT ( 'NONE',  ( -1.364683531250014514, 8.901041667008069425, -0.7879004041258335089 ) ) ;
#4545 = CARTESIAN_POINT ( 'NONE',  ( -6.925517538482230506, 6.974191971184389160, 0.7998128361456341429 ) ) ;
#4546 = CARTESIAN_POINT ( 'NONE',  ( 3.499976210622149253, 7.235056012367825140, 0.7998128361456321445 ) ) ;
#4547 = CARTESIAN_POINT ( 'NONE',  ( -4.787437638956927977, 7.639075441208117212, -1.082531754730549967 ) ) ;
#4548 = CIRCLE ( 'NONE', #18331, 0.07999999999999982125 ) ;
#4549 = AXIS2_PLACEMENT_3D ( 'NONE', #87469, #133041, #103722 ) ;
#4550 = CARTESIAN_POINT ( 'NONE',  ( 0.8084048693777341477, 1.257526981011043654, -1.703196666993979536 ) ) ;
#4551 = CARTESIAN_POINT ( 'NONE',  ( 8.191097360950562845, 12.70803068775103739, -0.7998128361456352531 ) ) ;
#4552 = CARTESIAN_POINT ( 'NONE',  ( -1.355131232792150309, 3.768605237513072304, -0.6431325189496899242 ) ) ;
#4553 = CARTESIAN_POINT ( 'NONE',  ( 6.684440181240522527, 1.196966437107028547, -1.688953195037292243 ) ) ;
#4555 = CARTESIAN_POINT ( 'NONE',  ( 4.414360472080629094, 7.100309700288360837, -1.094782333960819809 ) ) ;
#4554 = CARTESIAN_POINT ( 'NONE',  ( 0.8195642880178370948, 1.096917009463085790, -1.478703137254427924 ) ) ;
#4556 = CARTESIAN_POINT ( 'NONE',  ( 6.557281991921043662, -1.419039031320767474, 1.809608378690949149 ) ) ;
#4557 = CARTESIAN_POINT ( 'NONE',  ( 6.046573322014824114, 7.117052299514516456, -1.082531754730543083 ) ) ;
#4558 = CARTESIAN_POINT ( 'NONE',  ( 4.638297949650961982, 5.544340708415133712, -1.082531754730548412 ) ) ;
#4559 = CARTESIAN_POINT ( 'NONE',  ( 0.9906304909971673789, -0.5616109214932778482, -2.222291424677411698 ) ) ;
#4560 = CARTESIAN_POINT ( 'NONE',  ( 0.6125000000000037081, 0.3333333333333590720, 1.060881119635903147 ) ) ;
#4561 = CARTESIAN_POINT ( 'NONE',  ( -6.286140498591554326, 7.362860665558790707, 1.199719254218452047 ) ) ;
#4562 = CARTESIAN_POINT ( 'NONE',  ( 6.544875487120448199, -1.561333999131156780, -1.154546517916557269 ) ) ;
#4563 = VERTEX_POINT ( 'NONE', #5856 ) ;
#4565 = EDGE_CURVE ( 'NONE', #112384, #212524, #189638, .T. ) ;
#4564 = CARTESIAN_POINT ( 'NONE',  ( 8.934460041281305109, 10.48625347199211966, -1.082531754730543083 ) ) ;
#4566 = AXIS2_PLACEMENT_3D ( 'NONE', #192689, #160212, #195917 ) ;
#4567 = ORIENTED_EDGE ( 'NONE', *, *, #168015, .F. ) ;
#4568 = CARTESIAN_POINT ( 'NONE',  ( 6.187759705938407073, 1.828009178079874841, -0.5617473972939349691 ) ) ;
#4569 = DIRECTION ( 'NONE',  ( 0.5254827454987551771, 0.7071067811865540120, 0.4731467892558094412 ) ) ;
#4570 = CARTESIAN_POINT ( 'NONE',  ( -8.864333505236459132, 9.236143932397675727, 1.040834085586084257E-14 ) ) ;
#4571 = CARTESIAN_POINT ( 'NONE',  ( -10.37901820579008039, 4.889546506944066451, 5.358714317323078014 ) ) ;
#4573 = CARTESIAN_POINT ( 'NONE',  ( 1.182078593147641632, -1.725526258793514067, -0.3928099155053321745 ) ) ;
#4572 = CARTESIAN_POINT ( 'NONE',  ( 3.134800171978794125, -1.843606372480216082, 0.9858348089602610997 ) ) ;
#4574 = CARTESIAN_POINT ( 'NONE',  ( 6.592432824109000222, -0.4393352932590722792, 1.975308225066509049 ) ) ;
#4576 = CARTESIAN_POINT ( 'NONE',  ( 4.172042307184393728, -1.321354948109268346, 1.872925066384116377 ) ) ;
#4575 = CARTESIAN_POINT ( 'NONE',  ( 4.934241560730721510, 4.721313007132757811, 0.000000000000000000 ) ) ;
#4577 = CARTESIAN_POINT ( 'NONE',  ( 3.433312839113885850, 0.7810296162102482453, -1.555295924109141303 ) ) ;
#4578 = AXIS2_PLACEMENT_3D ( 'NONE', #160731, #176983, #30744 ) ;
#4579 = CARTESIAN_POINT ( 'NONE',  ( 10.55232363013785246, 11.20546574478267132, 0.000000000000000000 ) ) ;
#4580 = CARTESIAN_POINT ( 'NONE',  ( 4.875038752565570732, 7.845239757038595663, -1.199719254218452047 ) ) ;
#4581 = CARTESIAN_POINT ( 'NONE',  ( 3.760871765136180933, -1.731833850012770126, -0.08630056690941270703 ) ) ;
#4582 = CARTESIAN_POINT ( 'NONE',  ( 3.455704523497793001, 1.709784277118444162, 1.338028058695311273 ) ) ;
#4583 = CARTESIAN_POINT ( 'NONE',  ( 4.684505768721569652, 5.424010470718658716, -1.199719254218452047 ) ) ;
#4584 = CARTESIAN_POINT ( 'NONE',  ( 4.399625206644591557, -1.976670321813909892, 0.3981083777728141038 ) ) ;
#4585 = CARTESIAN_POINT ( 'NONE',  ( 2.125000000000001332, -2.052068128417950277, 1.216660472349556312E-13 ) ) ;
#4586 = CARTESIAN_POINT ( 'NONE',  ( 1.499999999999989120, 2.285416667349482012, 0.8660254037844524744 ) ) ;
#4587 = CARTESIAN_POINT ( 'NONE',  ( 1.448133341116746964, 1.924057924963176180, 0.09734726817032554602 ) ) ;
#4588 = CARTESIAN_POINT ( 'NONE',  ( -1.402160292154681736E-14, 9.093750000682799595, 1.732050807568881190 ) ) ;
#4589 = CARTESIAN_POINT ( 'NONE',  ( 4.939773707303276140, -2.109081064246129067, 0.6975513078685476875 ) ) ;
#4590 = VERTEX_POINT ( 'NONE', #141275 ) ;
#4591 = CARTESIAN_POINT ( 'NONE',  ( -0.2108831679770960255, 0.2438762813419328990, -1.931650693707862132 ) ) ;
#4592 = CARTESIAN_POINT ( 'NONE',  ( 1.499999999999987121, 1.795833333333355819, -0.8660254037844253849 ) ) ;
#4593 = CARTESIAN_POINT ( 'NONE',  ( 8.776205506747620788, 9.133327934160710981, -0.7998128361456221525 ) ) ;
#4594 = CARTESIAN_POINT ( 'NONE',  ( 4.270455198180219902, 6.965652916976816655, -1.082531754730548412 ) ) ;
#4595 = CARTESIAN_POINT ( 'NONE',  ( 1.642778471875000035, -1.276041666188710400, -2.845375778867859751 ) ) ;
#4596 = CARTESIAN_POINT ( 'NONE',  ( 1.014661930782149168, -2.221473418436111125, 0.005229513783167742333 ) ) ;
#4597 = CARTESIAN_POINT ( 'NONE',  ( 5.863715402168387492, -0.4781514528688200483, 1.902565108626977031 ) ) ;
#4598 = CARTESIAN_POINT ( 'NONE',  ( 7.754900677336718395, 11.99120852362745460, -0.7216878364870267237 ) ) ;
#4599 = CARTESIAN_POINT ( 'NONE',  ( -0.3866901564497973731, 3.102326550341738098, 2.027579305719746205 ) ) ;
#4600 = CARTESIAN_POINT ( 'NONE',  ( 6.538354595224527444, 2.236366790538524718, 0.3417416818044561877 ) ) ;
#4601 = CARTESIAN_POINT ( 'NONE',  ( -4.611181642423629157, 7.433443445252599702, 1.082531754730549967 ) ) ;
#4602 = CARTESIAN_POINT ( 'NONE',  ( 3.701677541426426910, -1.560128098810292130, -1.349382831327667454 ) ) ;
#4603 = CARTESIAN_POINT ( 'NONE',  ( -5.739179097286464248, 5.590130456455974617, -0.7998128361456221525 ) ) ;
#4605 = EDGE_CURVE ( 'NONE', #57181, #111140, #15100, .T. ) ;
#4604 = CARTESIAN_POINT ( 'NONE',  ( -1.201851678989727383E-14, 3.368750000682815049, -1.732050807568863648 ) ) ;
#4606 = CARTESIAN_POINT ( 'NONE',  ( 0.6823417656249899377, 4.988541667008086655, -1.181850606188754593 ) ) ;
#4607 = CARTESIAN_POINT ( 'NONE',  ( 4.657402308249613654, 0.4116239899518738810, -1.824517662812553009 ) ) ;
#4608 = CARTESIAN_POINT ( 'NONE',  ( 3.498401880895495086, -1.707742140280370746, 0.3003691301488361498 ) ) ;
#4609 = CARTESIAN_POINT ( 'NONE',  ( 3.632115859802576008, 0.2593814109021801984, 1.720877339435398667 ) ) ;
#4610 = CARTESIAN_POINT ( 'NONE',  ( 1.189493828671518427, 1.739998485882883861, 1.492566873345043010 ) ) ;
#4611 = CARTESIAN_POINT ( 'NONE',  ( -1.364683531250012516, 3.551041667008086211, -0.7879004041258300672 ) ) ;
#4612 = CARTESIAN_POINT ( 'NONE',  ( 4.071883345936186060, -1.202257327942996445, 1.710302118368298707 ) ) ;
#4613 = CARTESIAN_POINT ( 'NONE',  ( 0.3394786764520755784, 1.835982197492795898, 0.1384515631646099088 ) ) ;
#4614 = EDGE_CURVE ( 'NONE', #59123, #6715, #158549, .T. ) ;
#4615 = CARTESIAN_POINT ( 'NONE',  ( -0.1236583036082171405, 1.000000000000000888, 11.99936284241579898 ) ) ;
#4616 = SURFACE_SIDE_STYLE ('',( #120620 ) ) ;
#4617 = CARTESIAN_POINT ( 'NONE',  ( 1.248672897702383988, 1.986100274556975354, -0.3474695496914689818 ) ) ;
#4618 = CARTESIAN_POINT ( 'NONE',  ( 0.5686479265839607944, -2.064760635122906418, -0.7346842419702694915 ) ) ;
#4619 = FACE_BOUND ( 'NONE', #32942, .T. ) ;
#4620 = CARTESIAN_POINT ( 'NONE',  ( -7.181014916732457287, 11.52960116949655678, -0.7998128361456291469 ) ) ;
#4621 = CARTESIAN_POINT ( 'NONE',  ( 7.156006149914539982, 7.243095351188763686, 1.040834085586084257E-14 ) ) ;
#4622 = CARTESIAN_POINT ( 'NONE',  ( 2.403126630736720948, -0.3650820022202577730, -2.088671427859823293 ) ) ;
#4623 = CARTESIAN_POINT ( 'NONE',  ( 0.000000000000000000, 0.5000000000000004441, 0.000000000000000000 ) ) ;
#4624 = CARTESIAN_POINT ( 'NONE',  ( 5.918537399722813674, 1.222626809077583587, -1.356019982345892050 ) ) ;
#4625 = ORIENTED_EDGE ( 'NONE', *, *, #139916, .T. ) ;
#4626 = CARTESIAN_POINT ( 'NONE',  ( -5.932574734431526942, 9.079031735882207244, 1.199719254218454489 ) ) ;
#4627 =( NAMED_UNIT ( * ) SI_UNIT ( $, .STERADIAN. ) SOLID_ANGLE_UNIT ( ) );
#4628 = CARTESIAN_POINT ( 'NONE',  ( -3.285556943750000070, -1.246874999522043392, 0.000000000000000000 ) ) ;
#4629 = CARTESIAN_POINT ( 'NONE',  ( -5.696397096036042385, 9.797547045350714967, -0.7998128361456231517 ) ) ;
#4630 = CARTESIAN_POINT ( 'NONE',  ( 1.775654988352931563, 0.3410282263864356511, -1.990609417402624537 ) ) ;
#4631 = CARTESIAN_POINT ( 'NONE',  ( 6.668967514498191029, -2.014860697535350020, -0.9005387006749266954 ) ) ;
#4632 = CARTESIAN_POINT ( 'NONE',  ( 10.22692794340986921, 10.82583744360002243, 0.000000000000000000 ) ) ;
#4633 = CARTESIAN_POINT ( 'NONE',  ( 4.627703445648046809, 1.805782058207167529, -0.4492820238155226797 ) ) ;
#4634 = CARTESIAN_POINT ( 'NONE',  ( 10.06423010004587759, 10.63602329300870153, 0.000000000000000000 ) ) ;
#4635 = CARTESIAN_POINT ( 'NONE',  ( 0.08058608058607655278, -9.999999999999994671, 10.99970480893082225 ) ) ;
#4636 = ORIENTED_EDGE ( 'NONE', *, *, #3283, .T. ) ;
#4637 = ORIENTED_EDGE ( 'NONE', *, *, #35345, .F. ) ;
#4638 = CARTESIAN_POINT ( 'NONE',  ( -3.730464822054482710, 7.503959392372201442, 1.040834085586084257E-14 ) ) ;
#4639 = AXIS2_PLACEMENT_3D ( 'NONE', #184989, #4097, #134162 ) ;
#4640 = CARTESIAN_POINT ( 'NONE',  ( -6.984421689334302741, 11.30024240419870374, 0.000000000000000000 ) ) ;
#4641 = CARTESIAN_POINT ( 'NONE',  ( 4.811078068098579408, 1.589968679568127596, 0.8971634079883783475 ) ) ;
#4642 = CONICAL_SURFACE ( 'NONE', #35902, 1.376945625684933061, 0.7853981633974491672 ) ;
#4644 = CARTESIAN_POINT ( 'NONE',  ( -4.021356766390437265, 7.786759281977493785, -0.4705729632344165525 ) ) ;
#4643 = CARTESIAN_POINT ( 'NONE',  ( -7.208094944320834863, 8.438474185576302133, -1.199719254218452047 ) ) ;
#4645 = CARTESIAN_POINT ( 'NONE',  ( 5.207906507908255378, 7.834591108650524660, -1.266300940072472736 ) ) ;
#4646 = CARTESIAN_POINT ( 'NONE',  ( 1.264529683829066498, -1.734034291683920426, -0.006956266631255938158 ) ) ;
#4647 = CARTESIAN_POINT ( 'NONE',  ( 0.07555271646370392835, -1.686692104669092807, -0.4283695578703243245 ) ) ;
#4648 = CARTESIAN_POINT ( 'NONE',  ( 5.690114378391165850, -1.042650834883801947, 2.058788517775663962 ) ) ;
#4649 = CARTESIAN_POINT ( 'NONE',  ( 3.054329744828568227, 6.785411478933790264, 0.000000000000000000 ) ) ;
#4650 = CARTESIAN_POINT ( 'NONE',  ( 1.405620310220422109, -0.5036079032930698141, 1.998149085168912986 ) ) ;
#4651 = CARTESIAN_POINT ( 'NONE',  ( 6.491656622844908853, 6.468020902940851968, 0.7998128361456341429 ) ) ;
#4652 = CARTESIAN_POINT ( 'NONE',  ( 0.1458495181914116201, -0.1430550213798176262, -1.983920851313693223 ) ) ;
#4653 = DIRECTION ( 'NONE',  ( -0.6483454320283800199, 0.000000000000000000, 0.7613463080411786432 ) ) ;
#4654 = CARTESIAN_POINT ( 'NONE',  ( -5.749539660647037032, 8.865490816466966351, 1.199719254218454489 ) ) ;
#4655 = CARTESIAN_POINT ( 'NONE',  ( 0.2683544108190681898, -1.289511475198481305, 1.491327623740832387 ) ) ;
#4657 = CARTESIAN_POINT ( 'NONE',  ( -3.461074353238556167, 7.259946855412102273, 0.000000000000000000 ) ) ;
#4656 = CARTESIAN_POINT ( 'NONE',  ( 3.744317949583543470, 1.018843395500759197, -1.618198357137661469 ) ) ;
#4658 = CARTESIAN_POINT ( 'NONE',  ( 5.426482453889071245, 1.317083479513626587, -1.770629405693980640 ) ) ;
#4659 = CARTESIAN_POINT ( 'NONE',  ( 1.224999999999959233, 1.916666667349501196, 0.7072540797572717253 ) ) ;
#4660 = FACE_OUTER_BOUND ( 'NONE', #40687, .T. ) ;
#4661 = CARTESIAN_POINT ( 'NONE',  ( 5.194182247366881278, 5.232503174782402233, 0.7216878364870328300 ) ) ;
#4662 = CARTESIAN_POINT ( 'NONE',  ( -4.868786560638931782, 6.773613302202437403, 1.443375672974058777 ) ) ;
#4663 = CARTESIAN_POINT ( 'NONE',  ( 6.182307711929101224, 1.089732742074623006, 1.818925385317768928 ) ) ;
#4664 = ORIENTED_EDGE ( 'NONE', *, *, #12460, .T. ) ;
#4665 = CARTESIAN_POINT ( 'NONE',  ( 3.839178312322106823, 0.3354718084071331430, 2.282954970297036201 ) ) ;
#4666 = CARTESIAN_POINT ( 'NONE',  ( 3.807043925254738781, -1.605251362286563177, 1.127602784832412386 ) ) ;
#4667 = CARTESIAN_POINT ( 'NONE',  ( -5.123001941117347968, 7.070197912760590064, 1.599625672291263401 ) ) ;
#4668 = CARTESIAN_POINT ( 'NONE',  ( 1.199968502355329703, 0.8001272530510427083, -1.791371145023381128 ) ) ;
#4669 = CARTESIAN_POINT ( 'NONE',  ( 7.046081134561259951, 15.44736638506130610, 9.660548086161224290 ) ) ;
#4670 = CARTESIAN_POINT ( 'NONE',  ( -11.88168329227127096, 13.87999999999998479, 1.685799833707126050 ) ) ;
#4671 = VERTEX_POINT ( 'NONE', #73005 ) ;
#4672 = CARTESIAN_POINT ( 'NONE',  ( 6.245327377194020535, 0.3399632236478037917, -1.987496870419297013 ) ) ;
#4673 = CARTESIAN_POINT ( 'NONE',  ( -9.508345801885592863, 9.987491611821676329, 0.7998128361456462443 ) ) ;
#4674 = DIRECTION ( 'NONE',  ( -0.01538971728768980148, -0.9998815712882226370, 0.000000000000000000 ) ) ;
#4675 = CARTESIAN_POINT ( 'NONE',  ( 2.940461416894753377, -1.119856305176626821, 1.859859765203975890 ) ) ;
#4676 = CARTESIAN_POINT ( 'NONE',  ( 4.960304097753311048, 6.880383762169266504, 1.599625672291268286 ) ) ;
#4677 = CARTESIAN_POINT ( 'NONE',  ( 0.4047333657465709278, -2.105317319661216047, -0.2534319464195868843 ) ) ;
#4678 = CARTESIAN_POINT ( 'NONE',  ( -1.500000000000013101, 1.702083334016151417, 0.8660254037844403729 ) ) ;
#4679 = CARTESIAN_POINT ( 'NONE',  ( 10.56588178375152864, 11.22128359066528169, -0.7998128361456281477 ) ) ;
#4680 = CARTESIAN_POINT ( 'NONE',  ( 11.86687934130374522, 11.10951949616558565, -1.056332641424308827 ) ) ;
#4681 = CARTESIAN_POINT ( 'NONE',  ( 5.057296774772758852, 7.978757421411086348, 1.172581024337983724 ) ) ;
#4682 = CARTESIAN_POINT ( 'NONE',  ( 0.6146155864290882009, 1.423047967033652883, -1.490775708471054006 ) ) ;
#4684 = CARTESIAN_POINT ( 'NONE',  ( 6.727182134110202050, 7.629137130509070275, 2.410944104600750038 ) ) ;
#4683 = CARTESIAN_POINT ( 'NONE',  ( -9.561524646135538319, 12.17819805862340310, -1.599625672291263179 ) ) ;
#4685 = CARTESIAN_POINT ( 'NONE',  ( -1.364683531250000748, 1.509375000341421691, 0.000000000000000000 ) ) ;
#4686 = CARTESIAN_POINT ( 'NONE',  ( -4.218316008240990271E-13, -9.350066838357692589, -9.500000000000001776 ) ) ;
#4687 = CARTESIAN_POINT ( 'NONE',  ( 4.160738352132353768, 0.5130957772990808463, 1.842076966104645663 ) ) ;
#4688 = CARTESIAN_POINT ( 'NONE',  ( 5.851225812749518695, 8.984124660586543243, -1.199719254218452047 ) ) ;
#4689 = CARTESIAN_POINT ( 'NONE',  ( -4.277761160311629673, 4.949475094240346706, 1.199719254218462483 ) ) ;
#4690 = CARTESIAN_POINT ( 'NONE',  ( -0.0001156980946178872989, -0.8540272384012604912, 1.597593110781750925 ) ) ;
#4692 = CARTESIAN_POINT ( 'NONE',  ( 1.182675045768744271, 1.564012596108365072, -1.105954659444969401 ) ) ;
#4691 = CYLINDRICAL_SURFACE ( 'NONE', #142641, 0.07999999999999998779 ) ;
#4693 = CARTESIAN_POINT ( 'NONE',  ( 1.574760213118006735, 1.391939136705011348, -1.532762857463897843 ) ) ;
#4694 = CARTESIAN_POINT ( 'NONE',  ( -0.6823417656250246877, 0.6135416670080897639, 1.181850606188755259 ) ) ;
#4695 = CARTESIAN_POINT ( 'NONE',  ( 6.807498166657679484, -0.4075194142965676836, 1.832415718333743282 ) ) ;
#4696 = CARTESIAN_POINT ( 'NONE',  ( 2.982817717652554101, -0.1347461720548545627, -1.820777111243766733 ) ) ;
#4698 = CARTESIAN_POINT ( 'NONE',  ( 5.582388601459258304, 7.396495182493852738, 1.242574333668546638 ) ) ;
#4697 = CARTESIAN_POINT ( 'NONE',  ( 6.287735281038357549, 1.518688880046001444, 1.601449620450722700 ) ) ;
#4699 = CARTESIAN_POINT ( 'NONE',  ( 0.6823417656249882723, -0.07395833299191079124, -1.181850606188749264 ) ) ;
#4700 = CARTESIAN_POINT ( 'NONE',  ( 4.334473715658632820, -1.190102281996632261, 1.684540188307581010 ) ) ;
#4701 = CIRCLE ( 'NONE', #32417, 0.08000000000000016820 ) ;
#4703 = CARTESIAN_POINT ( 'NONE',  ( -7.250913225210214641, 7.353820272367037170, 0.7998128361456341429 ) ) ;
#4702 = CIRCLE ( 'NONE', #129312, 0.08000000000000020983 ) ;
#4704 = CARTESIAN_POINT ( 'NONE',  ( 7.076466111328892694, 10.34329533227067799, -1.199719254218441611 ) ) ;
#4705 = CARTESIAN_POINT ( 'NONE',  ( 6.933263157960373846, 7.629137130509066722, 2.546189081643289942 ) ) ;
#4706 = CARTESIAN_POINT ( 'NONE',  ( 4.981731378017507872, 7.899438143407371271, -1.199719254218452047 ) ) ;
#4708 = CARTESIAN_POINT ( 'NONE',  ( -1.201851678989727383E-14, 3.337500000000019007, -1.732050807568863648 ) ) ;
#4707 = CARTESIAN_POINT ( 'NONE',  ( 5.719784389160836646, -2.055351168476500234, 0.4581721925015455610 ) ) ;
#4709 = CARTESIAN_POINT ( 'NONE',  ( 6.074686117427479992, 1.393331124738606652, -1.531503843499823381 ) ) ;
#4711 = CARTESIAN_POINT ( 'NONE',  ( 1.364683531249986537, 1.176041667008082658, 0.7879004041258500513 ) ) ;
#4710 = AXIS2_PLACEMENT_3D ( 'NONE', #23898, #119350, #90004 ) ;
#4712 = CARTESIAN_POINT ( 'NONE',  ( 3.550220938608072085, 2.161773192003491495, 0.003901938047633223515 ) ) ;
#4713 = CARTESIAN_POINT ( 'NONE',  ( 4.301429021398018193, 1.803172560858562701, -0.9099306128727399079 ) ) ;
#4714 = CARTESIAN_POINT ( 'NONE',  ( 0.000000000000000000, 2.499999999999998668, -4.500000000000000000 ) ) ;
#4717 = CARTESIAN_POINT ( 'NONE',  ( 6.155038550924150087, 7.243595066575396757, 1.082531754730558626 ) ) ;
#4716 = CARTESIAN_POINT ( 'NONE',  ( 0.000000000000000000, -3.696874999522040017, -3.793834371823813001 ) ) ;
#4715 = PLANE ( 'NONE',  #59335 ) ;
#4718 = CARTESIAN_POINT ( 'NONE',  ( -4.471156797456668386, 8.438376373666578445, -0.7998128361456362523 ) ) ;
#4719 = CARTESIAN_POINT ( 'NONE',  ( 2.360564879530482330, -1.931125380751706810, -0.5807522007576990664 ) ) ;
#4720 = CARTESIAN_POINT ( 'NONE',  ( -9.203287345578106127, 9.631590079462940324, 0.7998128361456462443 ) ) ;
#4722 =( NAMED_UNIT ( * ) SI_UNIT ( $, .STERADIAN. ) SOLID_ANGLE_UNIT ( ) );
#4721 = CARTESIAN_POINT ( 'NONE',  ( -3.928111819657352566, 5.605883094398769195, 1.599625672291267398 ) ) ;
#4723 = CARTESIAN_POINT ( 'NONE',  ( 8.014278199453780616, 8.522615118883788199, 0.000000000000000000 ) ) ;
#4724 = CARTESIAN_POINT ( 'NONE',  ( 5.379139070037473935, -1.731557697741787916, -0.8120211572784155063 ) ) ;
#4725 = CARTESIAN_POINT ( 'NONE',  ( 6.938893903907228378E-15, 10.64264068711930733, 1.214306433183764966E-14 ) ) ;
#4727 = CARTESIAN_POINT ( 'NONE',  ( 4.235953958900400274, 2.015913684659226490, -0.05231418598541925924 ) ) ;
#4726 = CARTESIAN_POINT ( 'NONE',  ( -7.171900071504729191, 11.31104115015678779, -0.7216878364870267237 ) ) ;
#4728 = CARTESIAN_POINT ( 'NONE',  ( -1.201851678989727383E-14, 4.837500000000018119, -1.732050807568863648 ) ) ;
#4729 = CARTESIAN_POINT ( 'NONE',  ( -1.364683531250010295, 14.69270833367472839, 0.7879004041258445001 ) ) ;
#4730 = CARTESIAN_POINT ( 'NONE',  ( 6.071300242175304618, 0.1216566699881876934, -1.720563304769450630 ) ) ;
#4731 = CARTESIAN_POINT ( 'NONE',  ( 4.199993725183334803, 8.122019456014369254, -0.7998128361456362523 ) ) ;
#4733 = CARTESIAN_POINT ( 'NONE',  ( 7.614839552730775729, 8.913009562054615031, 1.199719254218452047 ) ) ;
#4732 = CARTESIAN_POINT ( 'NONE',  ( 9.734391104931955141, 10.45913716528321125, 0.7216878364870438212 ) ) ;
#4734 = CARTESIAN_POINT ( 'NONE',  ( -11.06825346762359885, 7.101010065767195734, 4.641007292122007577 ) ) ;
#4735 = CARTESIAN_POINT ( 'NONE',  ( 5.237510374101456812, -1.321932271818569093, -1.323673891312632245 ) ) ;
#4736 = CARTESIAN_POINT ( 'NONE',  ( 6.433844876963536130, -1.951739824409718160, 0.4931976252120565118 ) ) ;
#4737 = CARTESIAN_POINT ( 'NONE',  ( -9.579603127937250662, 7.849261790823902629, 0.08720040834116031536 ) ) ;
#4738 = CARTESIAN_POINT ( 'NONE',  ( -1.408440994509095656, 7.230285460703086642, -4.273713947604043994 ) ) ;
#4739 = EDGE_LOOP ( 'NONE', ( #128508, #164924 ) ) ;
#4740 = CARTESIAN_POINT ( 'NONE',  ( 1.001577623981730891, -1.966640429010723112, 0.4445266750975271353 ) ) ;
#4741 = CARTESIAN_POINT ( 'NONE',  ( 0.8963918696095014571, -1.767652434117328308, -0.3957652751337119024 ) ) ;
#4742 = CARTESIAN_POINT ( 'NONE',  ( 3.675669042636310557, 6.342012078834061484, -1.082531754730549967 ) ) ;
#4743 = DIRECTION ( 'NONE',  ( -7.387867266669436732E-31, 1.000000000000000000, 8.546850786086424434E-32 ) ) ;
#4744 = CARTESIAN_POINT ( 'NONE',  ( 6.588899466117086767, 10.63087377720454363, 1.040834085586084257E-14 ) ) ;
#4745 = EDGE_CURVE ( 'NONE', #42265, #62112, #156421, .T. ) ;
#4746 = CARTESIAN_POINT ( 'NONE',  ( 7.124973419181436007, 8.271222729588529887, -1.199719254218446718 ) ) ;
#4748 = CARTESIAN_POINT ( 'NONE',  ( 5.835529424904522422, 0.5513129833306378291, -1.834571867064521022 ) ) ;
#4747 = CARTESIAN_POINT ( 'NONE',  ( -4.283486466913726254, 7.084819080452935403, -1.199719254218452047 ) ) ;
#4749 = CARTESIAN_POINT ( 'NONE',  ( 4.517335436343452137, 8.499999999999996447, 0.7749999999999996891 ) ) ;
#4750 = B_SPLINE_CURVE_WITH_KNOTS ( 'NONE', 3,
 ( #36336, #102414, #20080, #70954 ),
 .UNSPECIFIED., .F., .F.,
 ( 4, 4 ),
 ( 0.000000000000000000, 0.0002909236271752618720 ),
 .UNSPECIFIED. ) ;
#4751 = CARTESIAN_POINT ( 'NONE',  ( -10.99915817693634246, -6.765468805240992367, 0.1539349733294695932 ) ) ;
#4753 = VERTEX_POINT ( 'NONE', #40541 ) ;
#4752 = CARTESIAN_POINT ( 'NONE',  ( 4.202664430556257713, 4.965825259479493603, 1.082531754730560403 ) ) ;
#4754 = CARTESIAN_POINT ( 'NONE',  ( -2.611917148927046295, 6.198987107056845858, 1.040834085586084257E-14 ) ) ;
#4755 = CARTESIAN_POINT ( 'NONE',  ( 3.415052781332720055, 1.953485055394106107, 0.9259690932504063277 ) ) ;
#4756 = CARTESIAN_POINT ( 'NONE',  ( -5.939880696562884310, 9.943961556049767836, 0.7216878364870267237 ) ) ;
#4757 = CARTESIAN_POINT ( 'NONE',  ( 6.292392690518195941, 8.434487120394948079, -1.443375672974078761 ) ) ;
#4758 = CARTESIAN_POINT ( 'NONE',  ( 0.8969213510382867405, -2.070190491330957006, -0.4589741369691033857 ) ) ;
#4759 = CARTESIAN_POINT ( 'NONE',  ( 5.438443955714742373, 1.798867289239113987, 0.3102399082220568816 ) ) ;
#4760 = CARTESIAN_POINT ( 'NONE',  ( 1.880087831454971603, -1.058004756265405799, 1.663231189906771990 ) ) ;
#4761 = CARTESIAN_POINT ( 'NONE',  ( 4.675980034926481288, 1.890745994642643479, -0.2862527531290667837 ) ) ;
#4762 = CARTESIAN_POINT ( 'NONE',  ( 0.000000000000000000, 13.49999999999999822, -1.500000000000000222 ) ) ;
#4763 = CARTESIAN_POINT ( 'NONE',  ( 4.844182406995376944, -0.9301426015250592316, 1.736093160643120914 ) ) ;
#4764 = CARTESIAN_POINT ( 'NONE',  ( 0.02324440041187331510, -1.194077796415137449, -1.532174088482601837 ) ) ;
#4765 = ORIENTED_EDGE ( 'NONE', *, *, #43078, .F. ) ;
#4766 = CARTESIAN_POINT ( 'NONE',  ( -4.797606254389363833, 6.690569611577942943, 1.599625672291263179 ) ) ;
#4767 = CARTESIAN_POINT ( 'NONE',  ( -5.157951095356222204, 4.982307464195829816, 0.000000000000000000 ) ) ;
#4769 = CARTESIAN_POINT ( 'NONE',  ( 6.170369307550823912, 7.331757292631694511, 1.082531754730549967 ) ) ;
#4768 = CARTESIAN_POINT ( 'NONE',  ( 8.229962938695207342, 9.560377169021284871, 1.199719254218462483 ) ) ;
#4771 = EDGE_LOOP ( 'NONE', ( #69677, #173344, #50516, #196043 ) ) ;
#4770 = CARTESIAN_POINT ( 'NONE',  ( 5.391234928627540945, -0.05113397888981999206, -1.911771334517261778 ) ) ;
#4772 = EDGE_CURVE ( 'NONE', #10129, #60515, #159749, .T. ) ;
#4773 = CARTESIAN_POINT ( 'NONE',  ( 0.9388347430083656686, 2.174419798330699649, 0.3756190385216377492 ) ) ;
#4774 = CARTESIAN_POINT ( 'NONE',  ( 7.834948825496932834, -5.907420853759296264, 7.720982897393583677 ) ) ;
#4775 = CARTESIAN_POINT ( 'NONE',  ( 6.481113961022470171, -1.841437297342415791, -0.8137991234780891370 ) ) ;
#4776 = CARTESIAN_POINT ( 'NONE',  ( -1.607015867998815128, 0.9165151389911810886, 1.199999999999999734 ) ) ;
#4777 = CARTESIAN_POINT ( 'NONE',  ( -0.07926568655891585991, 15.51719745866557432, 11.99972817042865181 ) ) ;
#4778 = CARTESIAN_POINT ( 'NONE',  ( -6.594971855056635412, -6.631671885544847989, -6.818239715405305823 ) ) ;
#4779 = CARTESIAN_POINT ( 'NONE',  ( 2.559107912120599071, 1.664280205102614429, -1.231313097332722872 ) ) ;
#4780 = CARTESIAN_POINT ( 'NONE',  ( -4.062639585589296942, 7.891496616496157301, 0.7998128361456341429 ) ) ;
#4781 = CARTESIAN_POINT ( 'NONE',  ( -4.634775730458505549, 8.344889633747440527, 0.3497604727749434872 ) ) ;
#4783 = CARTESIAN_POINT ( 'NONE',  ( 0.4972265960483426284, 1.796464302094663346, -1.202062886709959422 ) ) ;
#4782 = CARTESIAN_POINT ( 'NONE',  ( -5.427341564172148303, 5.226320001155936090, 0.000000000000000000 ) ) ;
#4784 = CARTESIAN_POINT ( 'NONE',  ( 0.000000000000000000, 9.719999999999982876, 0.000000000000000000 ) ) ;
#4785 = CARTESIAN_POINT ( 'NONE',  ( 0.000000000000000000, 14.48154074412737202, 0.000000000000000000 ) ) ;
#4786 = CARTESIAN_POINT ( 'NONE',  ( -4.865483722010302436, 4.987817560565853903, 0.6172052690934929364 ) ) ;
#4787 = CARTESIAN_POINT ( 'NONE',  ( -1.364683531250010295, 13.69270833367473195, 0.7879004041258445001 ) ) ;
#4789 = CARTESIAN_POINT ( 'NONE',  ( -5.601453741101424022, 6.564059448486966986, -1.199719254218453823 ) ) ;
#4788 = DIRECTION ( 'NONE',  ( 0.000000000000000000, 0.000000000000000000, -1.000000000000000000 ) ) ;
#4790 = CARTESIAN_POINT ( 'NONE',  ( 5.889268099914369614, -0.6330491082502353040, -1.614684210577774115 ) ) ;
#4791 = CARTESIAN_POINT ( 'NONE',  ( -4.600294193738529103, 4.261431402316699035, -0.7998128361456221525 ) ) ;
#4792 = CARTESIAN_POINT ( 'NONE',  ( 3.590741003927795827, 2.018730135711533258, 0.4582614309688318177 ) ) ;
#4793 = CARTESIAN_POINT ( 'NONE',  ( 4.745783977240443541, 2.094000167431044446, -0.3121058131653231538 ) ) ;
#4794 = CARTESIAN_POINT ( 'NONE',  ( 7.070740804726770357, 8.207951346058097286, 1.199719254218462483 ) ) ;
#4795 = CARTESIAN_POINT ( 'NONE',  ( -1.001543065824772872E-14, 4.321875000341417916, 1.575800808251672791 ) ) ;
#4796 = CARTESIAN_POINT ( 'NONE',  ( 2.342574202377019521, -1.930441307185966515, -0.3890957575964202886 ) ) ;
#4797 = CARTESIAN_POINT ( 'NONE',  ( 0.9492982845318720386, -1.727743609841876360, 0.8201845251225792222 ) ) ;
#4798 = CARTESIAN_POINT ( 'NONE',  ( 4.435649837374885607, 0.9824219174630977047, -2.071190651000577976 ) ) ;
#4799 = CARTESIAN_POINT ( 'NONE',  ( 2.086296903703276140, -1.790263230197926436, -0.3570169370194844483 ) ) ;
#4800 = CARTESIAN_POINT ( 'NONE',  ( 6.527324610336440180, 6.579909898339485252, 0.7998128361456331437 ) ) ;
#4802 = EDGE_CURVE ( 'NONE', #135251, #147625, #51264, .T. ) ;
#4801 = CARTESIAN_POINT ( 'NONE',  ( 6.304178240230120522, 6.457222156464352381, -0.7216878364870257245 ) ) ;
#4803 = CARTESIAN_POINT ( 'NONE',  ( -6.995117189646935962, 10.24838825697502109, 1.199719254218453823 ) ) ;
#4804 = CARTESIAN_POINT ( 'NONE',  ( 2.742442218595582570, 1.114876114576800248, -1.676130933394081923 ) ) ;
#4805 = CARTESIAN_POINT ( 'NONE',  ( 3.783995958019512607, -1.164969938643352299, -1.578273546942794647 ) ) ;
#4806 = CARTESIAN_POINT ( 'NONE',  ( -5.994676475536691029, 10.14553965476814845, 0.7998128361456481317 ) ) ;
#4807 = CARTESIAN_POINT ( 'NONE',  ( -4.466521540698216164, 7.298359999868178960, -1.199719254218452047 ) ) ;
#4808 = CARTESIAN_POINT ( 'NONE',  ( 0.07536363704233049743, 0.2309889609098912111, -2.177957698420322163 ) ) ;
#4810 = CARTESIAN_POINT ( 'NONE',  ( 4.574921169738827231, -0.001286399002502561879, -1.770032026507301515 ) ) ;
#4809 = CARTESIAN_POINT ( 'NONE',  ( 6.386679164125504293, 1.819714881846513199, -1.029135884875460372 ) ) ;
#4811 = CARTESIAN_POINT ( 'NONE',  ( 1.050790385995002740, 15.00000000000000355, 12.64745918785790302 ) ) ;
#4812 = VECTOR ( 'NONE', #172412, 1000.000000000000000 ) ;
#4813 = CARTESIAN_POINT ( 'NONE',  ( 1.254151665356119549, 0.8908215700371600043, 2.002402562943622844 ) ) ;
#4814 = CARTESIAN_POINT ( 'NONE',  ( 6.492160993672303704, -0.4719841783793111145, -1.675048763955745645 ) ) ;
#4815 = CARTESIAN_POINT ( 'NONE',  ( 7.263417608619159083, 9.497073181520933716, -1.599625672291262513 ) ) ;
#4816 = LINE ( 'NONE', #124042, #176034 ) ;
#4817 = CARTESIAN_POINT ( 'NONE',  ( 0.5624050986996537160, 1.909334820886617656, -1.279222687617764809 ) ) ;
#4819 = ADVANCED_FACE ( 'NONE', ( #193864 ), #44446, .F. ) ;
#4818 = CARTESIAN_POINT ( 'NONE',  ( 0.4510473619779230003, -1.854578567552306767, -1.167393260480112493 ) ) ;
#4820 = CARTESIAN_POINT ( 'NONE',  ( 6.520799197568460492, 1.728869810328565793, -0.1316537485448170952 ) ) ;
#4821 = CARTESIAN_POINT ( 'NONE',  ( 3.035963658818414235, -1.482449291622448095, -1.634993338104336891 ) ) ;
#4822 = B_SPLINE_CURVE_WITH_KNOTS ( 'NONE', 3,
 ( #135801, #115345, #99038, #50281, #83828, #68630, #84903, #82769, #152050, #148843, #100092, #150990, #182388, #184520 ),
 .UNSPECIFIED., .F., .F.,
 ( 4, 2, 2, 2, 2, 2, 4 ),
 ( -5.999999995607368656E-08, 0.0007641236830326251584, 0.001146215524548915496, 0.001528307366065205725, 0.002292491049097787267, 0.002674582890614078581, 0.003056674732130369894 ),
 .UNSPECIFIED. ) ;
#4823 = CARTESIAN_POINT ( 'NONE',  ( 6.619587810436369679, 0.3779085275587866777, -2.137903583376862038 ) ) ;
#4824 = CARTESIAN_POINT ( 'NONE',  ( -7.720982897393583677, -5.907420853759296264, 7.834948825496934610 ) ) ;
#4825 = CARTESIAN_POINT ( 'NONE',  ( 1.024788983299034451, 0.4191291695722613730, 2.075291419971446061 ) ) ;
#4826 = CARTESIAN_POINT ( 'NONE',  ( 2.906250000000002220, 1.895863743164021509, -0.7852924748301391977 ) ) ;
#4827 = CARTESIAN_POINT ( 'NONE',  ( 6.827182134110222123, -0.006956174471953178659, 2.188967759425272330 ) ) ;
#4828 = CARTESIAN_POINT ( 'NONE',  ( 5.965835030274156736, 1.897794126051439045, -0.3298099971670089281 ) ) ;
#4829 = VERTEX_POINT ( 'NONE', #157128 ) ;
#4831 = CARTESIAN_POINT ( 'NONE',  ( -1.402160292154681736E-14, -0.9906249996585834161, -1.575800808251665908 ) ) ;
#4830 = CARTESIAN_POINT ( 'NONE',  ( 1.119135019589584834, -0.04993059730015738523, 2.291989107133483028 ) ) ;
#4832 = CARTESIAN_POINT ( 'NONE',  ( 3.714044015139744914, 6.420469553383295391, 1.199719254218462483 ) ) ;
#4833 = CARTESIAN_POINT ( 'NONE',  ( 5.575427483717746213, 7.527751369135936343, 1.599625672291267398 ) ) ;
#4834 = CARTESIAN_POINT ( 'NONE',  ( 3.211816561499138523, 1.752256602034316213, 1.365123760953767418 ) ) ;
#4835 = CARTESIAN_POINT ( 'NONE',  ( -7.348156068926747331, 11.51667314714914347, 0.7216878364870458196 ) ) ;
#4836 = SURFACE_SIDE_STYLE ('',( #105612 ) ) ;
#4837 = CARTESIAN_POINT ( 'NONE',  ( 4.853455804012203778, 8.606189504748821051, 0.7216878364870438212 ) ) ;
#4838 = CARTESIAN_POINT ( 'NONE',  ( -8.310784975052682100, 10.71900177569337487, -1.443375672974058777 ) ) ;
#4839 = AXIS2_PLACEMENT_3D ( 'NONE', #21646, #153830, #53117 ) ;
#4840 = CARTESIAN_POINT ( 'NONE',  ( 6.861835142292147083, 7.178098218861903135, 0.7216878364870328300 ) ) ;
#4841 = CARTESIAN_POINT ( 'NONE',  ( 2.356092462967720458, 0.09613450340887133572, -2.014232768679749430 ) ) ;
#4843 = CARTESIAN_POINT ( 'NONE',  ( 6.320769014966518107, -1.461346085113580440, 1.455966316998691168 ) ) ;
#4842 = CARTESIAN_POINT ( 'NONE',  ( 8.586391356156291010, 8.911878091804165791, 0.7998128361456481317 ) ) ;
#4844 = CARTESIAN_POINT ( 'NONE',  ( 6.848276988234151652, 7.162280372460873679, -0.7216878364870317197 ) ) ;
#4845 = CIRCLE ( 'NONE', #198605, 0.07999999999999993228 ) ;
#4846 = CARTESIAN_POINT ( 'NONE',  ( 6.058121337783492599, -1.224224903413055010, 1.237393016278231617 ) ) ;
#4848 = EDGE_CURVE ( 'NONE', #183021, #118273, #2829, .T. ) ;
#4847 = FILL_AREA_STYLE ('',( #86143 ) ) ;
#4849 = CARTESIAN_POINT ( 'NONE',  ( 1.364683531249988757, 2.134375000341422357, 1.214306433183764966E-14 ) ) ;
#4850 = CARTESIAN_POINT ( 'NONE',  ( 0.8250501123308005003, -1.682963436248402056, 0.5476568922856797084 ) ) ;
#4851 = CARTESIAN_POINT ( 'NONE',  ( 0.3697678102792775756, -0.2496098759999023087, -2.000856779379902139 ) ) ;
#4852 = CARTESIAN_POINT ( 'NONE',  ( 0.3097736896383457839, 1.270387085892955792, -1.333027339516623888 ) ) ;
#4853 = CARTESIAN_POINT ( 'NONE',  ( 3.825942575589100780, 1.225831451615842393, -1.936910307245596652 ) ) ;
#4854 = CARTESIAN_POINT ( 'NONE',  ( 3.890429890068654917, 1.554390554365025379, -0.9864425779082321988 ) ) ;
#4855 = EDGE_CURVE ( 'NONE', #38245, #21699, #58544, .T. ) ;
#4856 = CARTESIAN_POINT ( 'NONE',  ( 7.248805684800777804, 11.60869039890961218, 1.040834085586084257E-14 ) ) ;
#4857 = CARTESIAN_POINT ( 'NONE',  ( 4.629811725094972630, -1.123643258228578024, -1.438734611599351565 ) ) ;
#4858 = CARTESIAN_POINT ( 'NONE',  ( 4.834611377684539413, 0.6298767044488963185, -1.915599524792414465 ) ) ;
#4859 = CARTESIAN_POINT ( 'NONE',  ( -8.045874094706015001, 11.47427131287732927, -1.199719254218446718 ) ) ;
#4861 = CARTESIAN_POINT ( 'NONE',  ( -6.149505192250180663, 9.332117270003974951, -1.199719254218452047 ) ) ;
#4860 = CARTESIAN_POINT ( 'NONE',  ( 3.960077240414155764, 2.245805352194740756, -0.2739276486512822184 ) ) ;
#4862 = CARTESIAN_POINT ( 'NONE',  ( 6.756868576547260474, -1.630415217921374671, 1.332730856581629375 ) ) ;
#4863 = CARTESIAN_POINT ( 'NONE',  ( 5.299301323368958094, 6.361497809228795930, -1.122821758042211959 ) ) ;
#4864 = CARTESIAN_POINT ( 'NONE',  ( 3.596198176508007105, 0.9334358170956689182, -1.848091447891623051 ) ) ;
#4865 = CARTESIAN_POINT ( 'NONE',  ( 9.541187415715040032, 12.15447128979948310, -1.599625672291262513 ) ) ;
#4866 = CARTESIAN_POINT ( 'NONE',  ( -0.6801582343750438575, 1.630208333674734611, -1.178068619123879834 ) ) ;
#4867 = CARTESIAN_POINT ( 'NONE',  ( 6.041668349913133618, -1.996727924239691587, 0.7141442534656232688 ) ) ;
#4868 = CONTEXT_DEPENDENT_SHAPE_REPRESENTATION ( #121285, #112998 ) ;
#4870 = CARTESIAN_POINT ( 'NONE',  ( 1.752441099931791868, 0.6037874858934308975, 1.829501483119711169 ) ) ;
#4869 = CARTESIAN_POINT ( 'NONE',  ( -8.992082194361570302, 11.51384853155376220, 1.599625672291269396 ) ) ;
#4871 = CARTESIAN_POINT ( 'NONE',  ( -4.911894908834722351, 4.738238661368090909, 0.4458799699701230246 ) ) ;
#4872 = CARTESIAN_POINT ( 'NONE',  ( 0.1507525579465497367, -0.4251589684514142653, -1.929747299214799483 ) ) ;
#4873 = CARTESIAN_POINT ( 'NONE',  ( 3.228249973385329596, 6.780392379009261283, -1.734723475976807094E-15 ) ) ;
#4874 = CARTESIAN_POINT ( 'NONE',  ( 5.490683550995299811, 6.230756917952954055, 0.9772120879164881702 ) ) ;
#4875 = DIRECTION ( 'NONE',  ( 0.000000000000000000, 0.000000000000000000, -1.000000000000000000 ) ) ;
#4876 = CARTESIAN_POINT ( 'NONE',  ( -2.930533758848195447, 6.570706485298192234, -0.7998128361456281477 ) ) ;
#4877 = CARTESIAN_POINT ( 'NONE',  ( 1.143189493912871280, 2.142763695547444058, 0.5857495978145771387 ) ) ;
#4878 = CARTESIAN_POINT ( 'NONE',  ( 3.469845758843297823, 2.055011051013386769, -0.4596899858253248872 ) ) ;
#4879 = CARTESIAN_POINT ( 'NONE',  ( -5.340986169140711226, 5.195848383611072485, 0.000000000000000000 ) ) ;
#4880 = CARTESIAN_POINT ( 'NONE',  ( 6.775324078527185989, 8.927630729746953264, -1.599625672291262513 ) ) ;
#4881 = CARTESIAN_POINT ( 'NONE',  ( 0.2560159283585193846, -1.860519322180047785, -0.05176575080893807551 ) ) ;
#4882 = CARTESIAN_POINT ( 'NONE',  ( 6.474182045725470402, 7.511966127223233869, -1.199719254218446718 ) ) ;
#4883 =( BOUNDED_CURVE ( )  B_SPLINE_CURVE ( 3, ( #122582, #187475, #188544, #172308 ),
 .UNSPECIFIED., .F., .T. ) 
 B_SPLINE_CURVE_WITH_KNOTS ( ( 4, 4 ),
 ( 3.141592653589828643, 4.712388980384858428 ),
 .UNSPECIFIED. ) 
 CURVE ( )  GEOMETRIC_REPRESENTATION_ITEM ( )  RATIONAL_B_SPLINE_CURVE ( ( 1.000000000000000000, 0.8047378541243335182, 0.8047378541243335182, 1.000000000000000000 ) ) 
 REPRESENTATION_ITEM ( '' )  );
#4884 = CARTESIAN_POINT ( 'NONE',  ( 3.486418057008484617, 7.219238166485217434, 1.040834085586084257E-14 ) ) ;
#4885 = CARTESIAN_POINT ( 'NONE',  ( -7.607533591043815768, 8.048079742405473525, 0.000000000000000000 ) ) ;
#4886 = CARTESIAN_POINT ( 'NONE',  ( -8.351459436338041442, 9.806086099558291025, -1.082531754730543971 ) ) ;
#4887 = CARTESIAN_POINT ( 'NONE',  ( 0.7211286721200690364, 1.601891702520108485, -1.389630591760198541 ) ) ;
#4888 = CARTESIAN_POINT ( 'NONE',  ( -7.099629715411508890, 8.311931418515415615, 1.199719254218452047 ) ) ;
#4890 = CARTESIAN_POINT ( 'NONE',  ( 4.404711838702720428, 0.5211615849865286476, 1.891323523724611766 ) ) ;
#4889 = CARTESIAN_POINT ( 'NONE',  ( -1.151774525698488676E-14, 0.6875000000000193179, -1.414508159514585417 ) ) ;
#4891 = CARTESIAN_POINT ( 'NONE',  ( 2.167066695894452888, -1.976221826324360498, -0.8764929760368763700 ) ) ;
#4892 = CARTESIAN_POINT ( 'NONE',  ( 1.716098596715152746, 1.718394358364897068, 0.6617865747741287219 ) ) ;
#4894 = CARTESIAN_POINT ( 'NONE',  ( -5.603170282960403092, 6.190551086330195574, -0.8764620106105174280 ) ) ;
#4893 = CARTESIAN_POINT ( 'NONE',  ( -1.572671215950735155E-14, -5.754340240174835586, -10.93220419382470610 ) ) ;
#4895 = CARTESIAN_POINT ( 'NONE',  ( 3.837644434229481316, 1.732183052659850286, 0.1680905250187741673 ) ) ;
#4896 = CARTESIAN_POINT ( 'NONE',  ( -1.280216254274686216, 4.017177813915858486, 0.4723901200327987882 ) ) ;
#4897 = CARTESIAN_POINT ( 'NONE',  ( 4.039966587192250103, 7.657118751792200584, 0.7216878364870298324 ) ) ;
#4898 = CARTESIAN_POINT ( 'NONE',  ( -11.21884318011362147, 9.005685702144777594, -2.479759622982018463 ) ) ;
#4899 = CARTESIAN_POINT ( 'NONE',  ( 0.8136072859011161951, -0.3160970183575459447, 2.138355382504661506 ) ) ;
#4900 = CARTESIAN_POINT ( 'NONE',  ( 3.884138610457484653, -0.1511163893381066714, 2.010518618204664154 ) ) ;
#4901 = DIRECTION ( 'NONE',  ( 0.000000000000000000, 0.000000000000000000, -1.000000000000000000 ) ) ;
#4902 = LINE ( 'NONE', #206335, #160144 ) ;
#4903 = CARTESIAN_POINT ( 'NONE',  ( 3.678557393866654923, -1.899675168901427513, -0.5269097987367215019 ) ) ;
#4904 = VECTOR ( 'NONE', #61668, 1000.000000000000000 ) ;
#4905 = CARTESIAN_POINT ( 'NONE',  ( 6.609000000000010644, 6.035875036286768136, 2.694900582964809388 ) ) ;
#4906 = CARTESIAN_POINT ( 'NONE',  ( 2.806119653986011819, 1.404935138194723265, -1.341025529631818980 ) ) ;
#4909 = ORIENTED_EDGE ( 'NONE', *, *, #72896, .F. ) ;
#4908 = CARTESIAN_POINT ( 'NONE',  ( -3.675669043080673770, 7.302381293653823491, 0.000000000000000000 ) ) ;
#4907 = CARTESIAN_POINT ( 'NONE',  ( 6.827182134110198142, 0.003888933837258023996, 1.810856214465889069 ) ) ;
#4910 = CARTESIAN_POINT ( 'NONE',  ( -5.112833325684916552, 7.058334528089422300, -1.443375672974066548 ) ) ;
#4911 = CARTESIAN_POINT ( 'NONE',  ( 6.073126464278658432, 6.050012061272033392, 0.000000000000000000 ) ) ;
#4912 = CARTESIAN_POINT ( 'NONE',  ( -3.820365424000704557, 7.679119771301277098, -0.7998128361456481317 ) ) ;
#4913 = CARTESIAN_POINT ( 'NONE',  ( -5.284646014276622950, 9.387447126623207794, -0.7998128361456362523 ) ) ;
#4914 = DIRECTION ( 'NONE',  ( 1.000000000000000000, -0.000000000000000000, -0.000000000000000000 ) ) ;
#4915 = CARTESIAN_POINT ( 'NONE',  ( 0.5345543961663907773, 1.132513062451316221, -1.893880525681296723 ) ) ;
#4916 = CARTESIAN_POINT ( 'NONE',  ( -5.608757509019071996, 5.629766575911039794, 0.4613631940431175416 ) ) ;
#4917 = CARTESIAN_POINT ( 'NONE',  ( 3.889464431383614862, -1.814284039448841979, 0.7467176931179178023 ) ) ;
#4918 = CARTESIAN_POINT ( 'NONE',  ( 6.286176778230493589, 10.48562334124426698, 0.7998128361456462443 ) ) ;
#4919 = CARTESIAN_POINT ( 'NONE',  ( 2.233046271152541618, 2.016033844848092560, 0.04667593304989729047 ) ) ;
#4920 = ORIENTED_EDGE ( 'NONE', *, *, #33691, .F. ) ;
#4921 = CARTESIAN_POINT ( 'NONE',  ( 2.606785607150950757, 1.995414689559615207, 0.7085744572869844271 ) ) ;
#4922 = CARTESIAN_POINT ( 'NONE',  ( -0.7500000000000215383, 1.722916667349486008, 1.299038105676659116 ) ) ;
#4924 = CARTESIAN_POINT ( 'NONE',  ( -4.720210035852093533, 8.658662141802762946, -0.7998128361456281477 ) ) ;
#4923 = PLANE ( 'NONE',  #80079 ) ;
#4925 = CARTESIAN_POINT ( 'NONE',  ( 3.345483972246702020, 1.841320589717788447, -0.001054884335952021917 ) ) ;
#4926 = ORIENTED_EDGE ( 'NONE', *, *, #204566, .F. ) ;
#4927 = EDGE_CURVE ( 'NONE', #71186, #103536, #77988, .T. ) ;
#4928 = CARTESIAN_POINT ( 'NONE',  ( -7.974166903131914452, 12.45494515362926435, -0.7998128361456281477 ) ) ;
#4929 = CARTESIAN_POINT ( 'NONE',  ( -1.500000000000079936, 7.240846818246208905, 4.154462424328226433 ) ) ;
#4930 = CARTESIAN_POINT ( 'NONE',  ( 4.412424163657523657, -2.120181911468725033, -0.04909571644767100895 ) ) ;
#4931 = CARTESIAN_POINT ( 'NONE',  ( 0.000000000000000000, 0.000000000000000000, 0.000000000000000000 ) ) ;
#4932 = CARTESIAN_POINT ( 'NONE',  ( 5.913327553854682783, 10.05063257947248800, -0.7998128361456291469 ) ) ;
#4933 = CARTESIAN_POINT ( 'NONE',  ( 4.745419391729821967, -1.590323190411299770, -1.310567541734160457 ) ) ;
#4935 = CARTESIAN_POINT ( 'NONE',  ( 2.788419073117563762, 1.577926727847511312, -0.9486480243563880643 ) ) ;
#4934 = CARTESIAN_POINT ( 'NONE',  ( -7.226659571283968297, 8.389856573708110332, 1.199719254218450271 ) ) ;
#4936 = CARTESIAN_POINT ( 'NONE',  ( 7.747594715205354809, 11.12627870345989756, -1.199719254218446718 ) ) ;
#4937 = SURFACE_STYLE_USAGE ( .BOTH. , #35333 ) ;
#4938 = DIRECTION ( 'NONE',  ( 0.000000000000000000, 0.000000000000000000, 1.000000000000000000 ) ) ;
#4939 = CARTESIAN_POINT ( 'NONE',  ( -1.499999999998184563, 8.627523663849279600, 2.580000000000257643 ) ) ;
#4940 =( BOUNDED_SURFACE ( )  B_SPLINE_SURFACE ( 3, 3, ( 
 ( #108628, #203899, #90197, #26230, #158386, #9982, #156261, #7842, #73930, #76060, #140023, #142159, #208175, #59808, #125963, #191919, #121699, #187663, #105387, #171426, #178909, #28375, #30524, #128106, #144313, #97663, #145378, #15301, #211376, #130222, #32637, #63002, #164773, #146423, #127033, #115020, #98714, #163721, #160510, #14227, #77117, #80322, #129173, #181017, #192992, #48900, #44646, #110760, #194064, #196216, #195150, #143240, #64079, #45717, #162656, #96604, #46784, #176759, #111836, #13183, #47857, #212437, #113969, #79261, #60874, #112898, #94469, #61947, #78187, #179966, #213494, #31588, #12113, #209229, #210311, #177839, #81389, #29453, #95543, #161594, #147473, #131272, #65116, #197260, #104045, #151735, #70435, #69375, #201505, #16363, #148531, #166912, #66164, #184203, #3305, #52090, #51025, #86716, #186337, #82441, #118217, #117146, #100827, #165839, #85648, #17425, #83508, #54224, #1175, #37972, #67239, #183150, #134441, #135483, #19575, #101904, #33697, #102972, #149591, #34753, #167969, #2233, #98, #136551, #68310, #53152, #119281, #152785, #185267, #133373, #132309, #199378, #99774, #36890, #49956, #18506, #202572, #198316, #120362, #169030, #116075, #182065, #20627, #84585, #4365, #150672, #200444, #35826, #106221, #5430, #123581, #157069, #205789, #204704, #25971, #125701, #21677, #57419, #56354, #40110, #105124, #24901, #171164, #22753, #207920, #154925, #191660, #6510, #122517, #73664, #8658, #173323, #41192, #187408, #42257, #88871, #188480, #107299, #155992, #43324, #75800, #7579, #74737, #91007, #140842, #206854, #59540, #72586, #58486, #124642, #190599, #138687, #55289, #172247, #139763, #23834, #189544, #108370, #174393, #92077, #158134, #89941, #170091, #87787, #9725, #141908, #121439, #153861, #71509, #137621, #203638, #39039, #47592, #29188, #162397, #64873, #95278, #197011, #178645, #159178, #147218, #131019, #195958, #192727, #46513, #109442, #112636, #161326, #213243, #10779, #81132, #76854, #142973, #160249, #13973, #12910, #175449, #96342, #11850, #194877, #62736, #177575, #208974, #77928, #45451, #80060, #30256, #146161, #111567, #93141, #78990, #60610, #94209, #110503, #145106, #128896, #126769, #212176, #27033, #144048, #63811, #113707, #44381, #211112, #176503, #28115, #129971, #179711, #210044, #31328, #61683, #127852, #193802, #97405, #163460, #15040, #1980, #180761, #98453, #117962, #49697, #183956, #132059, #51843, #149333, #35566, #17174, #65912, #68044, #913, #199117, #18243, #48647, #148280, #66980, #101647, #133118, #198069, #83248, #34506, #100579, #50760, #166652, #116890, #151479, #165580, #115825, #134181, #167714, #182889, #19317, #84327, #181812, #82187, #33444, #214279, #99521, #150413, #135239, #200190, #85393, #3049, #69118, #201253, #52893, #114764, #164518, #119027, #32388, #16103, #77556, #49338, #112266, #45089, #47221, #28817, #15738, #180395, #162027, #159879, #212879, #144742, #209671, #79691, #210752, #29889, #130655, #94902, #193446, #32017, #12543, #194505, #11484, #143678, #62375, #147906, #98101, #27745, #14674, #128537, #178279, #177203, #111198, #127475, #160952, #131690, #78617, #80769, #164152, #163093, #113338, #115457, #93840, #145803, #46153, #63447, #95974, #179344, #211810, #61314, #13618, #129601, #97041, #195586, #81824, #30966, #146858 ),
 ( #64511, #196646, #65545, #48286, #213922, #114398, #197694, #17858, #20000, #101260, #54650, #168404, #83942, #52516, #134865, #35184, #66596, #150033, #117586, #86085, #184635, #118649, #183577, #165206, #151105, #148957, #166267, #182501, #2670, #103406, #36252, #116511, #99153, #100201, #50391, #102331, #528, #67663, #153220, #33076, #21051, #152160, #4790, #181447, #3730, #87148, #69804, #135911, #16796, #82880, #167344, #132741, #200872, #201929, #68742, #1603, #37331, #136983, #198744, #53585, #133807, #51462, #34132, #119718, #199819, #18930, #70868, #85016, #203010, #185699, #169467, #24262, #107746, #124013, #206226, #138051, #207299, #55716, #6939, #57853, #106658, #76238, #26413, #172685, #173770, #189980, #41632, #25347, #158564, #187840, #91446, #157508, #9103, #39467, #5868, #121869, #90368, #73020, #156435, #75179, #141290, #58922, #125081, #40554, #10164, #142347, #8020, #74111, #71940, #140205, #171596, #105565, #191037, #23190, #42704, #174835, #89305, #139117, #155354, #120800, #104482, #188916, #205145, #56787, #170528, #208355, #122956, #204064, #108811, #92525, #186776, #38403, #22112, #88224, #154293, #176946, #27485, #112017, #28561, #62131, #165760, #127217, #11223, #1093, #44834, #12287, #43768, #109881, #94650, #183063, #133290, #59987, #49875, #160694, #144488, #209412, #77305, #159629, #61058, #166828, #143417, #115999, #67154, #198237, #82363, #150587, #126140, #178017, #193185, #95721, #78368, #148452, #29636, #93585, #110940, #84497, #132228, #22, #175893, #66085, #34677, #210495, #99690, #149509, #128291, #161773, #192102, #194253, #181987, #13366, #100746, #33619, #45897, #18423, #17345, #83427, #199296, #50941, #117066, #134357, #118136, #171075, #201422, #22671, #69288, #38955, #152700, #88783, #20549, #151650, #55205, #4282, #54140, #153772, #2150, #167885, #70353, #105038, #136469, #3220, #86634, #37885, #103963, #202488, #170005, #120276, #204621, #36805, #135399, #121351, #154840, #168947, #6425, #5340, #85561, #35743, #53061, #19486, #119195, #186250, #40025, #185181, #102888, #101817, #21593, #106137, #87698, #203552, #72499, #137534, #71423, #89857, #68226, #187326, #138599, #56273, #122432, #188389, #172160, #184122, #23753, #200362, #52010, #175368, #205701, #93058, #127765, #124558, #192644, #28029, #139679, #125618, #7493, #8573, #60521, #207833, #193720, #142890, #74653, #45363, #156985, #59460, #110419, #94127, #208890, #73577, #57336, #176422, #140758, #160165, #206769, #44297, #91993, #11765, #174309, #90920, #126682, #158053, #191577, #159096, #155908, #107216, #9638, #77839, #75716, #58403, #25883, #43240, #109357, #141830, #26950, #10697, #143961, #190516, #42173, #209956, #61593, #108289, #111480, #76767, #24818, #189464, #177487, #173240, #29101, #123500, #41107, #79969, #16012, #149241, #146072, #14947, #96251, #95185, #78895, #196920, #162304, #13889, #145018, #116800, #114678, #112542, #180671, #212085, #83161, #33352, #32297, #46424, #65819, #129881, #178553, #82098, #47505, #148190, #197978, #214192, #30163, #99434, #131966, #181722, #165487, #17084, #816, #66885, #182798, #183869, #104782, #8323, #125363, #10450, #142634, #176181, #77592, #93879, #39770, #105875, #189213, #205451, #197726, #99184, #112301, #178316, #29925, #96008, #79723, #211844, #63482 ),
 ( #196680, #179378, #47258, #14709, #52548, #185727, #69833, #201959, #135942, #104513, #133840, #37360, #103435, #169496, #117616, #166299, #183609, #184664, #85046, #36283, #21078, #87180, #4820, #70900, #102361, #22140, #88254, #20029, #137011, #83975, #203038, #101292, #151134, #120828, #134893, #186804, #154323, #66624, #198774, #50423, #182533, #34161, #100232, #150063, #68774, #92555, #89335, #157538, #27515, #9134, #206258, #43799, #121901, #192134, #55745, #187868, #56817, #58952, #140236, #93614, #207333, #122987, #91478, #173800, #74143, #105595, #188945, #156467, #125110, #75209, #141320, #8054, #204092, #190012, #39497, #205175, #6967, #41662, #142377, #191068, #155383, #138079, #139147, #73048, #42732, #171628, #106690, #109912, #71969, #60018, #108840, #175923, #5897, #174866, #126171, #26445, #158595, #23223, #40585, #172715, #24291, #90397, #57883, #124046, #107775, #10194, #25377, #76268, #208386, #210529, #30739, #113111, #13395, #44866, #128322, #95752, #146636, #162869, #96820, #161804, #143448, #129383, #127249, #144520, #160726, #195362, #81600, #14449, #94683, #77335, #78400, #28596, #80540, #193220, #45930, #131473, #11257, #213702, #212652, #197475, #32856, #64293, #65326, #130439, #196426, #159658, #209445, #79471, #61090, #179116, #48071, #46994, #194286, #15515, #115238, #110971, #114182, #112049, #29668, #12319, #180177, #62164, #178050, #49120, #145588, #181228, #211585, #63221, #31803, #97879, #163939, #147685, #176978, #185486, #33912, #199598, #36039, #84799, #54443, #4581, #150887, #151946, #102119, #19787, #168188, #136765, #166054, #69588, #135699, #85869, #17639, #198528, #99988, #2449, #51241, #68524, #201725, #3517, #53366, #119500, #18715, #202793, #120585, #134652, #200656, #50175, #52305, #149815, #83725, #37112, #167130, #103190, #118435, #169253, #186563, #184422, #98931, #20839, #148743, #164985, #16576, #86938, #182286, #153004, #82659, #70655, #311, #66383, #132531, #116295, #1387, #67448, #133593, #117367, #183364, #34968, #101040, #124855, #121658, #189762, #59767, #41414, #24054, #76021, #154078, #9945, #88007, #5645, #89092, #91228, #172466, #125926, #25125, #155146, #123802, #206007, #106443, #137838, #6728, #188701, #157288, #107521, #173551, #40337, #21897, #7800, #71726, #22974, #39253, #73892, #174617, #8878, #187626, #170309, #171383, #105346, #74957, #203860, #138908, #142124, #104262, #92308, #141067, #208137, #38191, #207074, #158352, #58705, #190819, #55505, #72807, #90157, #204928, #57642, #42480, #139986, #56579, #108589, #122738, #156223, #26193, #12078, #61907, #126996, #46742, #192955, #44607, #15262, #176723, #147429, #28335, #144276, #95505, #178871, #195106, #62960, #209195, #64037, #110723, #78145, #129130, #177797, #213453, #97622, #29414, #30482, #112855, #96566, #162613, #81349, #94432, #14190, #80282, #146381, #160471, #77077, #210269, #161552, #128069, #13140, #212394, #130182, #196175, #47816, #111792, #65076, #191884, #79216, #145335, #143205, #211336, #194025, #45675, #113928, #179924, #31547, #163680, #43545, #109667, #175669, #27257, #93365, #159401, #60835, #11000, #34751, #1171, #100824, #19572, #52087, #85646, #69372, #183147, #155726, #7310, #166909, #150669, #95, #2230, #99771, #116073, #135480, #18502, #201502, #84581, #101901, #73387 ),
 ( #68307, #89676, #164770, #23566, #98711, #16361, #165837, #167965, #134438, #139492, #35824, #17422, #200441, #118214, #184201, #148529, #83505, #199376, #151732, #3303, #53148, #51022, #32635, #119279, #82439, #33695, #49953, #185263, #39845, #105952, #198313, #181013, #182063, #132305, #171976, #66160, #149587, #48896, #115017, #67237, #133370, #28925, #78723, #126504, #45194, #44120, #176251, #205520, #123319, #141648, #40922, #158925, #192468, #26776, #25707, #61419, #161059, #57154, #92879, #91815, #75537, #140580, #60343, #206591, #58219, #95010, #190336, #12652, #41998, #157873, #109178, #110241, #208717, #76595, #8391, #77665, #124378, #9466, #142707, #191399, #189282, #111308, #43065, #27852, #93949, #159990, #11591, #143785, #107028, #108105, #209780, #127583, #193552, #174133, #90742, #207659, #175190, #59278, #10521, #177311, #173054, #24634, #156804, #125437, #74473, #34236, #130757, #32120, #96079, #98203, #195692, #211918, #165309, #212978, #82984, #64618, #197801, #100310, #196752, #17968, #214023, #194611, #182614, #166376, #16903, #13721, #81927, #144850, #148013, #48393, #210856, #46254, #116621, #112372, #178383, #47327, #49436, #114506, #62482, #131795, #113442, #15841, #164253, #180502, #29994, #179447, #80873, #115555, #65648, #181552, #146963, #128646, #33180, #162132, #129709, #145907, #99261, #66700, #149059, #79794, #63553, #31069, #97145, #636, #163198, #14781, #132847, #198851, #50499, #87261, #121980, #171705, #4900, #138160, #137089, #54759, #84055, #1714, #20106, #133920, #37438, #70978, #119826, #118752, #154399, #39574, #150142, #185805, #184736, #168507, #19042, #153326, #85121, #151207, #187946, #68849, #105677, #134969, #36364, #202033, #203117, #120908, #169574, #101372, #170636, #2778, #102439, #21157, #69910, #67769, #204168, #136020, #186880, #167448, #38513, #199927, #104591, #53695, #51572, #117698, #55824, #183689, #35295, #200977, #22221, #3837, #52624, #88334, #86193, #5978, #103515, #152264, #72049, #206334, #173877, #10268, #26521, #174939, #25451, #7046, #207406, #205253, #8136, #24367, #59025, #159733, #92630, #172796, #155463, #156544, #106767, #158671, #56895, #124125, #209522, #89414, #77410, #76343, #61163, #111047, #142451, #127325, #208459, #60092, #23303, #73122, #91558, #139222, #191144, #126251, #125183, #57960, #93690, #193295, #123070, #42810, #190087, #107851, #90479, #192210, #74220, #140316, #44940, #41740, #189024, #157614, #9211, #141396, #43872, #176000, #108917, #40665, #27592, #75282, #11331, #114257, #162945, #132596, #82738, #14525, #15586, #180253, #97955, #31877, #382, #29743, #147759, #213776, #164011, #95826, #62236, #178127, #80622, #129458, #146712, #65399, #81673, #131546, #197547, #96896, #66455, #198599, #212729, #64367, #128395, #130513, #13470, #161883, #49191, #30817, #115311, #196502, #181301, #50246, #48144, #177054, #32929, #12396, #28671, #94756, #99004, #165059, #16652, #148811, #160805, #78475, #144594, #210608, #194362, #46004, #195441, #112123, #79546, #145664, #211662, #63298, #47071, #113188, #179194, #53434, #88076, #84869, #153075, #202862, #100060, #85944, #182356, #183435, #20909, #168258, #154150, #103262, #35038, #5718, #117440, #19857, #70722, #54509, #169324, #33985, #17708, #136836, #101110, #120654, #167197, #4652, #52378 ),
 ( #184489, #18784, #134721, #152019, #3587, #118506, #69663, #36107, #104335, #150957, #2522, #87003, #186632, #68598, #38259, #119572, #199669, #149890, #200727, #133666, #51313, #135771, #71795, #102191, #185558, #170380, #201794, #37186, #21968, #116368, #166124, #137908, #203928, #83797, #1456, #67521, #140055, #72873, #75028, #56648, #43616, #208208, #189836, #187697, #26261, #172538, #23046, #107595, #24123, #57712, #158414, #122810, #6797, #59840, #40409, #7873, #39324, #105419, #90225, #175742, #125992, #55576, #42556, #156289, #206078, #205002, #138979, #155216, #188769, #159476, #106511, #73961, #207152, #41484, #11074, #27335, #173626, #108659, #58776, #190891, #124929, #93437, #123869, #92380, #10016, #174686, #25197, #91301, #157359, #8951, #141141, #76091, #142194, #191950, #109734, #77152, #143274, #121730, #171457, #89162, #96641, #160544, #162696, #45751, #61986, #15338, #63042, #147509, #129210, #47896, #164809, #46820, #82479, #64118, #44685, #98752, #16401, #81427, #78223, #146459, #209263, #212474, #112935, #60909, #110794, #181056, #176796, #28412, #111870, #114008, #178948, #127067, #196251, #177875, #80362, #14268, #30561, #94506, #29486, #145412, #180003, #130261, #97700, #211413, #193029, #163760, #12151, #194103, #210345, #213529, #197300, #48940, #144345, #128142, #95579, #161628, #13221, #79295, #100865, #38010, #116114, #170131, #3344, #182104, #1210, #69413, #67273, #201541, #185304, #133411, #51061, #150708, #18542, #168006, #135520, #184238, #35865, #103010, #43356, #153897, #123619, #122554, #7616, #22790, #157102, #88908, #154962, #125735, #72625, #109477, #138724, #40145, #205826, #74774, #91042, #24939, #105161, #26004, #6546, #8693, #206889, #73700, #203676, #57457, #55326, #204741, #56391, #189581, #9761, #42293, #188515, #5466, #106259, #171200, #108405, #121477, #139798, #59580, #187448, #191697, #92115, #175487, #87827, #75835, #39075, #107336, #63845, #114793, #159213, #177612, #143010, #112669, #146194, #162429, #61719, #97436, #197040, #93180, #195992, #111603, #95315, #11887, #47627, #77962, #144083, #131052, #161363, #48676, #12947, #145142, #113737, #31360, #163491, #15072, #81164, #213274, #27073, #60644, #35598, #150447, #136326, #86493, #2009, #19344, #167745, #85423, #151509, #4144, #33474, #3076, #69147, #52923, #165612, #49725, #17201, #68076, #50791, #134211, #119055, #185039, #102750, #168806, #200221, #70215, #53996, #51872, #20411, #83276, #152557, #180792, #32416, #98481, #164547, #82217, #204481, #173100, #58269, #122293, #124425, #155772, #21459, #120135, #186113, #24681, #55067, #7356, #37746, #87567, #71281, #121217, #154704, #187186, #72359, #188250, #106001, #38813, #104899, #39891, #23615, #89723, #184662, #52545, #167372, #198772, #67692, #35215, #152187, #153244, #83972, #117614, #100229, #99181, #82910, #18960, #166297, #17888, #148983, #120826, #183606, #116541, #102359, #150061, #87178, #37358, #85044, #16826, #69831, #1633, #66622, #151132, #133838, #101290, #201957, #199849, #50421, #103433, #2699, #68771, #558, #132769, #134891, #4817, #169494, #165233, #3756, #200898, #168431, #20027, #182531, #135939, #119747, #203036, #185725, #21076, #70898, #137009, #54677, #186802, #38431, #156465, #138077, #74141, #56815, #57881, #8051, #5895, #171626 ),
 ( #170555, #188943, #88251, #206256, #25375, #140234, #73046, #108838, #208385, #104511, #124043, #139145, #122985, #187866, #107773, #39495, #105593, #76266, #23220, #60016, #89333, #205173, #190010, #91476, #41660, #173798, #55743, #125108, #155381, #40582, #157537, #24289, #126169, #158593, #90395, #9132, #75207, #141318, #207330, #142375, #6965, #58950, #191066, #42730, #106688, #204090, #172713, #174864, #26443, #92553, #10192, #22138, #154321, #71967, #121899, #84529, #180964, #147418, #32586, #165790, #198263, #17373, #1123, #114964, #150618, #2179, #98663, #82392, #146369, #148481, #31537, #47805, #67185, #48850, #133322, #164718, #33644, #68255, #16307, #195094, #49906, #30471, #18452, #46731, #199325, #64026, #132256, #112843, #116028, #50, #178859, #96555, #166856, #162602, #14178, #97612, #99718, #66113, #80271, #182013, #163669, #83457, #149537, #50971, #212384, #15253, #131222, #117093, #183093, #34705, #197210, #130172, #100774, #196164, #179914, #113918, #81339, #213443, #65066, #69318, #52039, #53093, #3250, #137568, #167918, #20578, #106168, #200391, #188423, #203585, #172195, #7527, #55237, #40059, #187357, #105072, #134388, #118165, #70382, #184151, #87731, #121384, #170037, #168978, #204654, #89890, #35774, #21623, #86662, #4311, #135428, #38987, #201450, #119226, #23784, #185210, #155941, #36834, #152729, #37919, #171110, #22703, #5376, #151680, #6456, #102917, #136498, #71455, #120307, #101848, #19515, #186282, #88816, #154873, #72533, #138631, #85592, #202519, #56303, #122465, #54169, #103993, #153804, #74686, #191609, #60555, #76800, #159129, #90951, #160196, #8602, #174340, #10730, #59490, #95219, #193750, #125647, #126715, #142921, #208921, #192675, #111513, #140787, #44329, #110451, #176452, #206801, #173270, #58434, #43271, #25918, #109391, #28064, #94157, #11798, #77873, #207866, #177519, #161269, #175396, #93088, #24850, #143995, #124587, #190547, #209987, #61629, #127795, #45396, #73610, #139709, #205732, #189495, #41139, #107249, #108320, #92026, #9671, #75747, #164463, #34454, #16049, #213191, #50710, #128839, #199064, #62680, #46456, #63756, #65855, #147164, #100526, #214227, #129916, #82133, #180707, #64818, #112578, #195902, #163407, #132005, #148225, #198015, #14982, #211055, #196956, #178590, #212118, #13922, #48594, #149277, #49643, #162339, #30198, #47538, #96287, #115766, #80002, #113651, #116836, #78930, #66924, #181755, #182837, #12855, #33389, #133066, #99467, #165526, #179655, #31275, #130964, #97350, #17118, #83195, #114712, #858, #22454, #122210, #18190, #202267, #201204, #36583, #101594, #21382, #167662, #19263, #204400, #151426, #188172, #2999, #118978, #85345, #4065, #121139, #38736, #153556, #84275, #67992, #187102, #69068, #104818, #135188, #203334, #168728, #170864, #184957, #52843, #5127, #20330, #70135, #103742, #166601, #183906, #86416, #54987, #152483, #136247, #53918, #120055, #186030, #37666, #169793, #87491, #154624, #71202, #137318, #88566, #6204, #72273, #138382, #56053, #35517, #51795, #39806, #150362, #134134, #9429, #143747, #90706, #175152, #77625, #8354, #190298, #106991, #105912, #73348, #25668, #173016, #24597, #139451, #127543, #91775, #140540, #125395, #206554, #209742, #176211, #75499, #57117, #27813, #58182, #59236, #43027, #109139, #92841, #193514 ),
 ( #32079, #13684, #129671, #194573, #62443, #144811, #46219, #149019, #210818, #98167, #49397, #180463, #64579, #132807, #45155, #163158, #128606, #80835, #63519, #130720, #14743, #12613, #178348, #66660, #114463, #196711, #94972, #48352, #16865, #79754, #81888, #131754, #28888, #146925, #111269, #112336, #164215, #97106, #82945, #15802, #29956, #594, #177272, #99220, #147974, #161018, #78686, #213984, #165270, #65604, #197759, #96042, #162095, #195656, #145870, #212942, #115516, #181511, #211878, #33140, #47290, #113405, #179411, #31032, #68807, #133877, #53650, #199884, #51529, #22179, #183647, #154356, #35251, #151165, #102397, #185763, #201992, #69868, #1672, #70937, #117654, #85081, #135977, #184698, #5935, #104549, #36319, #37395, #119782, #103470, #169532, #88295, #101327, #21112, #87218, #153282, #167408, #84009, #19000, #168465, #2736, #20063, #4858, #137047, #203073, #54717, #118710, #72006, #198811, #86152, #152223, #150100, #3794, #134929, #200934, #120866, #52582, #186840, #38472, #170593, #50457, #116576, #182571, #34193, #100268, #166333, #17925, #67726, #7004, #75243, #159692, #141355, #124084, #175958, #39534, #109948, #187904, #105635, #188979, #191103, #57919, #11291, #125146, #40623, #9168, #91516, #206294, #23259, #106726, #74182, #42771, #207369, #58989, #140275, #121938, #107809, #171663, #123028, #139182, #173834, #60054, #108878, #73081, #55781, #56854, #205212, #174902, #89371, #24328, #27553, #190047, #155420, #25411, #172753, #90436, #156504, #157575, #126209, #26481, #8093, #41699, #92591, #158633, #10230, #76305, #142412, #93649, #204128, #192171, #208420, #138119, #43832, #212689, #131508, #130472, #48105, #165020, #209482, #13431, #127283, #30777, #64331, #113147, #112086, #147721, #32890, #143485, #179153, #178087, #161843, #12355, #146674, #78434, #210565, #115271, #62199, #98968, #128355, #29705, #195402, #196463, #80576, #162904, #94718, #163973, #194323, #95786, #14486, #63257, #61123, #197511, #129419, #114217, #180216, #31838, #97914, #181264, #45965, #15549, #81636, #213738, #79507, #177014, #211622, #47032, #96856, #65361, #49155, #193254, #44901, #111009, #28631, #160761, #120621, #2487, #118472, #182321, #184457, #67486, #83762, #37147, #84836, #169288, #150926, #69628, #186598, #68562, #104299, #85908, #66419, #54476, #38225, #103228, #100025, #168225, #16614, #19823, #134689, #82695, #132562, #202828, #198563, #50212, #133632, #135737, #200693, #148776, #3556, #199634, #102158, #36075, #52344, #116331, #51280, #167165, #201759, #151983, #53400, #119538, #17676, #35005, #185523, #20873, #18752, #86972, #153042, #4617, #117405, #149855, #70689, #136802, #183401, #346, #33950, #166088, #1423, #101077, #187661, #105384, #73928, #208172, #155183, #25164, #9979, #6766, #188737, #171424, #170347, #154113, #24090, #23011, #89128, #5683, #191916, #40376, #39289, #189800, #72840, #158384, #108624, #90195, #88042, #141105, #138945, #137876, #7838, #204966, #172505, #58742, #56613, #121696, #174653, #122777, #106478, #71760, #203896, #156258, #76057, #26227, #21932, #157323, #140020, #206046, #57682, #123839, #55542, #41451, #59804, #107559, #8915, #92344, #91266, #173594, #43582, #74996, #207116, #124894, #190857, #42518, #142156, #125960, #77113, #28372, #131270, #178906, #129169, #159437 ) ),
 .UNSPECIFIED., .T., .F., .T. ) 
 B_SPLINE_SURFACE_WITH_KNOTS ( ( 4, 3, 4 ),
 ( 4, 1, 1, 1, 1, 1, 1, 1, 1, 1, 1, 1, 1, 1, 1, 1, 1, 1, 1, 1, 1, 1, 1, 1, 1, 1, 1, 1, 1, 1, 1, 1, 1, 1, 1, 1, 1, 1, 1, 1, 1, 1, 1, 1, 1, 1, 1, 1, 1, 1, 1, 1, 1, 1, 1, 1, 1, 1, 1, 1, 1, 1, 1, 1, 1, 1, 1, 1, 1, 1, 1, 1, 1, 1, 1, 1, 1, 1, 1, 1, 1, 1, 1, 1, 1, 1, 1, 1, 1, 1, 1, 1, 1, 1, 1, 1, 1, 1, 1, 1, 1, 1, 1, 1, 1, 1, 1, 1, 1, 1, 1, 1, 1, 1, 1, 1, 1, 1, 1, 1, 1, 1, 1, 1, 1, 1, 1, 1, 1, 1, 1, 1, 1, 1, 1, 1, 1, 1, 1, 1, 1, 1, 1, 1, 1, 1, 1, 1, 1, 1, 1, 1, 1, 1, 1, 1, 1, 1, 1, 1, 1, 1, 1, 1, 1, 1, 1, 1, 1, 1, 1, 1, 1, 1, 1, 1, 1, 1, 1, 1, 1, 1, 1, 1, 1, 1, 1, 1, 1, 1, 1, 1, 1, 1, 1, 1, 1, 1, 1, 1, 1, 1, 1, 1, 1, 1, 1, 1, 1, 1, 1, 1, 1, 1, 1, 1, 1, 1, 1, 1, 1, 1, 1, 1, 1, 1, 1, 1, 1, 1, 1, 1, 1, 1, 1, 1, 1, 1, 1, 1, 1, 1, 1, 1, 1, 1, 1, 1, 1, 1, 1, 1, 1, 1, 1, 1, 1, 1, 1, 1, 1, 1, 1, 1, 1, 1, 1, 1, 1, 1, 1, 1, 1, 1, 1, 1, 1, 1, 1, 1, 1, 1, 1, 1, 1, 1, 1, 1, 1, 1, 1, 1, 1, 1, 1, 1, 1, 1, 1, 1, 1, 1, 1, 1, 1, 1, 1, 1, 1, 1, 1, 1, 1, 1, 1, 1, 1, 1, 1, 1, 1, 1, 1, 1, 1, 1, 1, 1, 1, 1, 1, 1, 1, 1, 1, 1, 1, 1, 1, 1, 1, 1, 1, 1, 1, 1, 1, 1, 1, 1, 1, 1, 1, 1, 1, 1, 1, 1, 1, 1, 1, 1, 1, 1, 1, 1, 1, 1, 1, 1, 1, 1, 1, 1, 1, 1, 1, 1, 1, 1, 1, 1, 1, 1, 4 ),
 ( 0.000000000000000000, 0.5000000000000000000, 1.000000000000000000 ),
 ( 0.000000000000000000, 0.002600033395298661284, 0.005208813367820810773, 0.007813200023264601363, 0.01041635779573905213, 0.01302082523971277370, 0.01562491580351430334, 0.01822918961192645723, 0.02083333155136493989, 0.02343746137460561707, 0.02604174567981391505, 0.02864576082122225614, 0.03125012338981237453, 0.03385410379569547823, 0.03645843966640821554, 0.03906250599122108869, 0.04166672065998115043, 0.04427093656960304907, 0.04687500111868234121, 0.04947933663890847350, 0.05208331727515622817, 0.05468767913406928638, 0.05729168951085979872, 0.05989597295159828499, 0.06250011041458469752, 0.06510424634142775169, 0.06770853038940542745, 0.07031253939703428768, 0.07291690072920921362, 0.07552088074063932621, 0.07812521459448035221, 0.08072927904253822395, 0.08333349217322323643, 0.08593770650149938628, 0.08854176936806532061, 0.09114610329512429221, 0.09375008230893774885, 0.09635444258075796797, 0.09895845137230636912, 0.1015627332241899466, 0.1041668691376404637, 0.1067710034717011397, 0.1093752859901425123, 0.1119792934252105548, 0.1145836532378000650, 0.1171876317139315254, 0.1197919640503514460, 0.1223960270027875247, 0.1250002386107842423, 0.1276044514713231270, 0.1302085128224930721, 0.1328128452953424854, 0.1354168228245230532, 0.1380211816480703679, 0.1406251889951717071, 0.1432294693974442978, 0.1458336039016293884, 0.1484377367829480265, 0.1510420179109137340, 0.1536460239143070949, 0.1562503823458506746, 0.1588543594276481397, 0.1614586903853630351, 0.1640627519827278502, 0.1666669622076225599, 0.1692711737400035832, 0.1718752337163205746, 0.1744795648736557347, 0.1770835410591554138, 0.1796878985729436218, 0.1822919046164021839, 0.1848961837081005144, 0.1875003169431251615, 0.1901044485118078553, 0.1927087283883223978, 0.1953127331008320255, 0.1979170902898210183, 0.2005210661182068033, 0.2031253958358791578, 0.2057294562186703923, 0.2083336651999991573, 0.2109378755437518183, 0.2135419342857080849, 0.2161462642661750033, 0.2187502392488957503, 0.2213545955913898966, 0.2239586004719608947, 0.2265628783920732026, 0.2291670104979939837, 0.2317711408940984485, 0.2343754196581391558, 0.2369794232205082452, 0.2395837793053874898, 0.2421877540212369617, 0.2447920826374832270, 0.2473961419461526701, 0.2500003498234057431, 0.2526045591180144934, 0.2552086167660569949, 0.2578129457082574683, 0.2604169196290564980, 0.2630212749386780513, 0.2656252787970727613, 0.2682295556845439854, 0.2708336868013750398, 0.2734378161649161920, 0.2760420939554183439, 0.2786460965083475960, 0.2812504516275206035, 0.2838544253716674404, 0.2864587530250631842, 0.2890628114000217685, 0.2916670183126490179, 0.2942712266975582858, 0.2968752833920936807, 0.2994796114345903981, 0.3020835844342854570, 0.3046879388494173613, 0.3072919418263086455, 0.3098962178200457829, 0.3125003480877632800, 0.3151044765587182606, 0.3177087535145803887, 0.3203127551987332566, 0.3229171094905676220, 0.3255210824038090589, 0.3281254092328941829, 0.3307294668145174810, 0.3333336729019333866, 0.3359378805165532667, 0.3385419363979534357, 0.3411462636792753078, 0.3437502358986498918, 0.3463545895576419231, 0.3489585917936692261, 0.3515628670325462446, 0.3541669965910940188, 0.3567711243094072171, 0.3593754005694961839, 0.3619794015255044517, 0.3645837551283364619, 0.3671877273514386752, 0.3697920534947228832, 0.3723961104233561858, 0.3750003158249449187, 0.3776045228086560845, 0.3802085780172632101, 0.3828129046759103926, 0.3854168762557192984, 0.3880212292968930887, 0.3906252309326675998, 0.3932295055555311003, 0.3958336345448258409, 0.3984377616504144459, 0.4010420373535708016, 0.4036460377220391638, 0.4062503907741795706, 0.4088543624478828686, 0.4114586880438503846, 0.4140627444598136697, 0.4166669493149349202, 0.4192711558070936761, 0.4218752104832254046, 0.4244795366576747386, 0.4270835077386489487, 0.4296878603003031483, 0.4322918614764136302, 0.4348961356220873986, 0.4375002641820237570, 0.4401043908147829753, 0.4427086660998260093, 0.4453126660213379551, 0.4479170186610768045, 0.4505209899261007900, 0.4531253151132156320, 0.4557293711568096706, 0.4583335756048029785, 0.4609377817447468106, 0.4635418360287018591, 0.4661461618574116450, 0.4687501325802634344, 0.4713544848006788190, 0.4739584856576960492, 0.4765627594649867738, 0.4791668877354426925, 0.4817710140352507997, 0.4843752890409837031, 0.4869792886561065681, 0.4895836410217184742, 0.4921876120187673176, 0.4947919369354787933, 0.4973959927469893683, 0.5000001969271801183, 0.5026044028542325792, 0.5052084568862954539, 0.5078127825077110025, 0.5104167530131399344, 0.5130211050305848453, 0.5156251057090676104, 0.5182293793167697116, 0.5208335074376115870, 0.5234376335443351458, 0.5260419084095501185, 0.5286459078588399141, 0.5312502600885893322, 0.5338542309583571566, 0.5364585557431046370, 0.5390626114628084276, 0.5416668155145124564, 0.5442710213679887721, 0.5468750752884355970, 0.5494794008409938924, 0.5520833712696913143, 0.5546877232224267651, 0.5572917238629264691, 0.5598959974098275394, 0.5625001255209155504, 0.5651042515744146844, 0.5677085264378984863, 0.5703125258619060611, 0.5729168780940517847, 0.5755208489772277725, 0.5781251737684461878, 0.5807292295366155432, 0.5833334335991446906, 0.5859376395183565345, 0.5885416934674594369, 0.5911460190895951872, 0.5937499895822500040, 0.5963543416085342885, 0.5989583423516006144, 0.6015626159764864145, 0.6041667442176794633, 0.6067708703578130747, 0.6093751453583519107, 0.6119791448976270587, 0.6145834972704286026, 0.6171874683077025470, 0.6197917932438269384, 0.6223958492007358734, 0.6250000534134032559, 0.6276042595376638555, 0.6302083136556971832, 0.6328126394858472059, 0.6354166101831504321, 0.6380209624212449526, 0.6406249634074311361, 0.6432292372490908683, 0.6458333657602520761, 0.6484374921268833969, 0.6510417674032679125, 0.6536457671983656459, 0.6562501198500874100, 0.6588540911821543222, 0.6614584164016259482, 0.6640624726875546946, 0.6666666771896793131, 0.6692708836583093346, 0.6718749380855545406, 0.6744792642621626477, 0.6770832353048136243, 0.6796875878929879988, 0.6822915892628557133, 0.6848958634600870177, 0.6874999923810890534, 0.6901041191140900866, 0.6927083948051209195, 0.6953123949966061312, 0.6979167480655225075, 0.7005207198330885010, 0.7031250454743595002, 0.7057291022295995031, 0.7083333071605121267, 0.7109375141128444486, 0.7135415689895947544, 0.7161458956511181917, 0.7187498671798290273, 0.7213542202563657524, 0.7239582221504904380, 0.7265624968421051655, 0.7291666263128349090, 0.7317707535520923123, 0.7343750297965853102, 0.7369790305250381035, 0.7395833841494394711, 0.7421873564932268685, 0.7447916826947649227, 0.7473957400596251688, 0.7499999455586733310, 0.7526041531340577073, 0.7552082086006238759, 0.7578125358855373195, 0.7604165080410384414, 0.7630208617442386654, 0.7656248643032155243, 0.7682291396280439555, 0.7708332697884082707, 0.7734373976738285750, 0.7760416746106194585, 0.7786456760166404756, 0.7812500303348380859, 0.7838540033955903041, 0.7864583302958847444, 0.7890623884106959807, 0.7916665946172487534, 0.7942708029550582527, 0.7968748591517740287, 0.7994791871985751364, 0.8020831601216208417, 0.8046875145898089166, 0.8072915179542569097, 0.8098957940511537501, 0.8124999250410844809, 0.8151040537125986418, 0.8177083314805486669, 0.8203123337047645292, 0.8229166888550945025, 0.8255206627735817149, 0.8281249905111484066, 0.8307290495162685806, 0.8333332565697225691, 0.8359374658093579047, 0.8385415228765847884, 0.8411458518237998616, 0.8437498256551729803, 0.8463541810267020127, 0.8489581853372698550, 0.8515624623451190089, 0.8541665943045783083, 0.8567707239021479237, 0.8593750026401490993, 0.8619790058232168484, 0.8645833619440471685, 0.8671873368610717447, 0.8697916655744575287, 0.8723957256102774505, 0.8749999336500613456, 0.8776041439309557601, 0.8802082020090884473, 0.8828125319952765393, 0.8854165068757942070, 0.8880208632890512765, 0.8906248686864229880, 0.8932291467441429988, 0.8958332798131283248, 0.8984374104767501867, 0.9010416903237299380, 0.9036456946063434748, 0.9062500518360779855, 0.9088540278924787108, 0.9114583577202677311, 0.9140624189272162914, 0.9166666280927961985, 0.9192708395544209043, 0.9218748987838942810, 0.9244792299476556341, 0.9270832060181642964, 0.9296875636115721209, 0.9322915702365133228, 0.9348958494830461596, 0.9374999838014769216, 0.9401041156712998115, 0.9427083967663798525, 0.9453124022892170908, 0.9479167607665550666, 0.9505207380999710631, 0.9531250691809918241, 0.9557291317261836783, 0.9583333421310490374, 0.9609375547886240820, 0.9635416155522130710, 0.9661459483928183101, 0.9687499245033458495, 0.9713542829945021051, 0.9739582954330652242, 0.9765625745907361432, 0.9791667024412501474, 0.9817708385604039245, 0.9843751096149007118, 0.9869791944699233266, 0.9895836584107432499, 0.9921868132917668337, 0.9947911946869415489, 0.9973999724172807335, 1.000000000000000000 ),
 .UNSPECIFIED. ) 
 GEOMETRIC_REPRESENTATION_ITEM ( )  RATIONAL_B_SPLINE_SURFACE ( (
 ( 1.000000000000000000, 1.000000000000000000, 1.000000000000000000, 0.9999999999999997780, 1.000000000000000000, 1.000000000000000000, 1.000000000000000000, 1.000000000000000222, 1.000000000000000000, 1.000000000000000000, 1.000000000000000222, 0.9999999999999997780, 1.000000000000000222, 1.000000000000000222, 1.000000000000000000, 1.000000000000000000, 1.000000000000000000, 0.9999999999999997780, 1.000000000000000222, 0.9999999999999996669, 1.000000000000000222, 1.000000000000000000, 1.000000000000000000, 0.9999999999999996669, 1.000000000000000444, 0.9999999999999996669, 1.000000000000000444, 1.000000000000000000, 1.000000000000000000, 0.9999999999999997780, 1.000000000000000222, 0.9999999999999994449, 1.000000000000000444, 1.000000000000000000, 1.000000000000000000, 1.000000000000000000, 1.000000000000000000, 1.000000000000000444, 0.9999999999999997780, 1.000000000000000000, 1.000000000000000000, 1.000000000000000000, 1.000000000000000000, 1.000000000000000000, 1.000000000000000000, 0.9999999999999997780, 1.000000000000000000, 1.000000000000000444, 0.9999999999999997780, 1.000000000000000444, 0.9999999999999997780, 0.9999999999999997780, 1.000000000000000000, 1.000000000000000222, 1.000000000000000000, 1.000000000000000000, 1.000000000000000000, 1.000000000000000000, 0.9999999999999997780, 1.000000000000000444, 0.9999999999999997780, 1.000000000000000000, 1.000000000000000222, 0.9999999999999997780, 1.000000000000000000, 1.000000000000000222, 0.9999999999999997780, 1.000000000000000222, 1.000000000000000000, 1.000000000000000222, 1.000000000000000000, 1.000000000000000222, 0.9999999999999997780, 1.000000000000000000, 1.000000000000000222, 1.000000000000000000, 1.000000000000000222, 0.9999999999999997780, 1.000000000000000222, 0.9999999999999997780, 1.000000000000000222, 0.9999999999999997780, 1.000000000000000222, 1.000000000000000222, 0.9999999999999997780, 1.000000000000000222, 1.000000000000000222, 0.9999999999999997780, 1.000000000000000222, 1.000000000000000000, 1.000000000000000000, 1.000000000000000222, 0.9999999999999996669, 1.000000000000000444, 0.9999999999999997780, 0.9999999999999997780, 1.000000000000000000, 1.000000000000000000, 1.000000000000000000, 0.9999999999999996669, 1.000000000000000444, 1.000000000000000000, 1.000000000000000222, 1.000000000000000000, 0.9999999999999997780, 1.000000000000000222, 0.9999999999999997780, 1.000000000000000222, 1.000000000000000000, 1.000000000000000000, 1.000000000000000222, 1.000000000000000000, 1.000000000000000222, 0.9999999999999994449, 1.000000000000000444, 1.000000000000000000, 0.9999999999999996669, 1.000000000000000222, 0.9999999999999997780, 1.000000000000000222, 0.9999999999999997780, 1.000000000000000000, 1.000000000000000000, 1.000000000000000000, 1.000000000000000000, 1.000000000000000000, 1.000000000000000444, 1.000000000000000000, 1.000000000000000000, 1.000000000000000222, 1.000000000000000000, 1.000000000000000000, 0.9999999999999997780, 1.000000000000000000, 1.000000000000000222, 1.000000000000000000, 1.000000000000000222, 0.9999999999999997780, 1.000000000000000000, 0.9999999999999997780, 0.9999999999999997780, 1.000000000000000222, 0.9999999999999997780, 1.000000000000000444, 0.9999999999999997780, 1.000000000000000000, 1.000000000000000222, 1.000000000000000000, 1.000000000000000000, 0.9999999999999997780, 1.000000000000000222, 1.000000000000000000, 1.000000000000000000, 1.000000000000000000, 1.000000000000000222, 0.9999999999999996669, 1.000000000000000222, 1.000000000000000222, 0.9999999999999996669, 1.000000000000000444, 0.9999999999999996669, 1.000000000000000000, 1.000000000000000222, 0.9999999999999996669, 1.000000000000000222, 1.000000000000000000, 1.000000000000000222, 1.000000000000000000, 1.000000000000000222, 0.9999999999999997780, 1.000000000000000444, 0.9999999999999997780, 0.9999999999999997780, 1.000000000000000222, 0.9999999999999996669, 1.000000000000000222, 1.000000000000000000, 1.000000000000000000, 1.000000000000000000, 0.9999999999999997780, 1.000000000000000222, 1.000000000000000222, 0.9999999999999997780, 1.000000000000000222, 0.9999999999999997780, 1.000000000000000222, 1.000000000000000000, 1.000000000000000444, 1.000000000000000000, 1.000000000000000222, 0.9999999999999996669, 1.000000000000000444, 0.9999999999999993339, 1.000000000000000444, 0.9999999999999997780, 1.000000000000000444, 0.9999999999999997780, 1.000000000000000000, 1.000000000000000000, 0.9999999999999997780, 1.000000000000000222, 0.9999999999999997780, 0.9999999999999996669, 1.000000000000000444, 1.000000000000000222, 1.000000000000000000, 0.9999999999999997780, 1.000000000000000222, 0.9999999999999996669, 1.000000000000000222, 0.9999999999999997780, 1.000000000000000222, 1.000000000000000000, 1.000000000000000000, 1.000000000000000000, 1.000000000000000000, 0.9999999999999997780, 1.000000000000000000, 1.000000000000000000, 0.9999999999999997780, 1.000000000000000000, 1.000000000000000000, 1.000000000000000000, 1.000000000000000222, 1.000000000000000000, 1.000000000000000444, 1.000000000000000222, 1.000000000000000000, 1.000000000000000000, 0.9999999999999997780, 1.000000000000000222, 1.000000000000000000, 1.000000000000000000, 1.000000000000000000, 0.9999999999999997780, 1.000000000000000222, 0.9999999999999997780, 1.000000000000000222, 1.000000000000000444, 0.9999999999999997780, 1.000000000000000222, 1.000000000000000000, 1.000000000000000000, 1.000000000000000000, 0.9999999999999997780, 1.000000000000000444, 0.9999999999999997780, 1.000000000000000222, 0.9999999999999997780, 1.000000000000000222, 0.9999999999999994449, 1.000000000000000222, 1.000000000000000000, 1.000000000000000222, 1.000000000000000000, 0.9999999999999997780, 1.000000000000000222, 1.000000000000000000, 0.9999999999999997780, 1.000000000000000444, 0.9999999999999996669, 1.000000000000000222, 1.000000000000000000, 1.000000000000000000, 1.000000000000000222, 0.9999999999999997780, 0.9999999999999997780, 1.000000000000000444, 1.000000000000000222, 1.000000000000000000, 0.9999999999999997780, 0.9999999999999997780, 1.000000000000000222, 1.000000000000000000, 1.000000000000000222, 1.000000000000000000, 0.9999999999999997780, 1.000000000000000000, 1.000000000000000000, 1.000000000000000000, 1.000000000000000222, 0.9999999999999997780, 1.000000000000000222, 1.000000000000000000, 1.000000000000000000, 1.000000000000000000, 0.9999999999999997780, 1.000000000000000000, 1.000000000000000222, 1.000000000000000222, 0.9999999999999996669, 1.000000000000000444, 0.9999999999999996669, 1.000000000000000222, 1.000000000000000000, 1.000000000000000222, 0.9999999999999997780, 1.000000000000000444, 1.000000000000000000, 1.000000000000000444, 0.9999999999999994449, 1.000000000000000222, 0.9999999999999997780, 0.9999999999999997780, 1.000000000000000000, 1.000000000000000222, 1.000000000000000000, 1.000000000000000000, 1.000000000000000000, 1.000000000000000222, 0.9999999999999996669, 1.000000000000000222, 1.000000000000000000, 0.9999999999999996669, 1.000000000000000444, 1.000000000000000000, 1.000000000000000000, 1.000000000000000000, 0.9999999999999996669, 1.000000000000000222, 1.000000000000000000, 1.000000000000000000, 1.000000000000000222, 0.9999999999999997780, 0.9999999999999997780, 1.000000000000000000, 1.000000000000000000, 1.000000000000000222, 0.9999999999999997780, 1.000000000000000222, 1.000000000000000000, 1.000000000000000000, 0.9999999999999996669, 1.000000000000000222, 1.000000000000000000, 1.000000000000000222, 1.000000000000000000, 1.000000000000000000, 1.000000000000000000, 0.9999999999999997780, 1.000000000000000222, 0.9999999999999996669, 1.000000000000000444, 1.000000000000000000, 0.9999999999999997780, 1.000000000000000000, 1.000000000000000222, 1.000000000000000222, 0.9999999999999996669, 1.000000000000000000, 1.000000000000000000, 0.9999999999999997780, 1.000000000000000222, 1.000000000000000000, 1.000000000000000222, 0.9999999999999996669, 1.000000000000000444, 1.000000000000000000, 1.000000000000000000, 1.000000000000000000, 1.000000000000000222, 1.000000000000000000, 0.9999999999999997780, 1.000000000000000444, 1.000000000000000000, 1.000000000000000444, 0.9999999999999997780, 1.000000000000000444, 1.000000000000000000, 1.000000000000000222, 1.000000000000000222, 1.000000000000000000, 0.9999999999999996669, 1.000000000000000000, 1.000000000000000000, 1.000000000000000000, 1.000000000000000000, 1.000000000000000222, 0.9999999999999996669, 1.000000000000000000, 1.000000000000000222, 0.9999999999999997780, 0.9999999999999997780, 1.000000000000000000, 1.000000000000000000, 1.000000000000000000, 1.000000000000000000),
 ( 0.3333333333333333703, 0.3333333333333333703, 0.3333333333333333703, 0.3333333333333333148, 0.3333333333333333703, 0.3333333333333333148, 0.3333333333333333703, 0.3333333333333334259, 0.3333333333333333703, 0.3333333333333333148, 0.3333333333333334259, 0.3333333333333332593, 0.3333333333333334259, 0.3333333333333333703, 0.3333333333333333703, 0.3333333333333332593, 0.3333333333333334259, 0.3333333333333333148, 0.3333333333333334259, 0.3333333333333333148, 0.3333333333333334259, 0.3333333333333334259, 0.3333333333333333148, 0.3333333333333333148, 0.3333333333333334814, 0.3333333333333332593, 0.3333333333333334259, 0.3333333333333334259, 0.3333333333333333703, 0.3333333333333333703, 0.3333333333333334814, 0.3333333333333332038, 0.3333333333333334814, 0.3333333333333333703, 0.3333333333333334259, 0.3333333333333333148, 0.3333333333333334259, 0.3333333333333334814, 0.3333333333333333703, 0.3333333333333332593, 0.3333333333333334259, 0.3333333333333333148, 0.3333333333333333148, 0.3333333333333333703, 0.3333333333333333703, 0.3333333333333334259, 0.3333333333333333148, 0.3333333333333335369, 0.3333333333333333148, 0.3333333333333334259, 0.3333333333333333703, 0.3333333333333332038, 0.3333333333333334259, 0.3333333333333334259, 0.3333333333333333148, 0.3333333333333334259, 0.3333333333333333703, 0.3333333333333333703, 0.3333333333333334259, 0.3333333333333334259, 0.3333333333333333703, 0.3333333333333334259, 0.3333333333333334259, 0.3333333333333333148, 0.3333333333333333703, 0.3333333333333333703, 0.3333333333333333148, 0.3333333333333334259, 0.3333333333333333148, 0.3333333333333334814, 0.3333333333333333703, 0.3333333333333334259, 0.3333333333333333148, 0.3333333333333333703, 0.3333333333333334259, 0.3333333333333333703, 0.3333333333333333703, 0.3333333333333333148, 0.3333333333333334259, 0.3333333333333333148, 0.3333333333333334259, 0.3333333333333333703, 0.3333333333333334259, 0.3333333333333334814, 0.3333333333333333148, 0.3333333333333334259, 0.3333333333333334259, 0.3333333333333333148, 0.3333333333333333703, 0.3333333333333333703, 0.3333333333333333148, 0.3333333333333334814, 0.3333333333333332593, 0.3333333333333334259, 0.3333333333333333703, 0.3333333333333333148, 0.3333333333333333703, 0.3333333333333333703, 0.3333333333333334259, 0.3333333333333333148, 0.3333333333333334259, 0.3333333333333333148, 0.3333333333333334814, 0.3333333333333333148, 0.3333333333333333148, 0.3333333333333334259, 0.3333333333333333148, 0.3333333333333333703, 0.3333333333333333703, 0.3333333333333334259, 0.3333333333333333703, 0.3333333333333334259, 0.3333333333333333703, 0.3333333333333332593, 0.3333333333333334259, 0.3333333333333333703, 0.3333333333333333148, 0.3333333333333334814, 0.3333333333333333148, 0.3333333333333334259, 0.3333333333333334259, 0.3333333333333333148, 0.3333333333333333703, 0.3333333333333334259, 0.3333333333333333703, 0.3333333333333333703, 0.3333333333333334259, 0.3333333333333333703, 0.3333333333333334259, 0.3333333333333333703, 0.3333333333333334259, 0.3333333333333333148, 0.3333333333333333703, 0.3333333333333333703, 0.3333333333333333703, 0.3333333333333333703, 0.3333333333333335369, 0.3333333333333332593, 0.3333333333333333703, 0.3333333333333333703, 0.3333333333333332593, 0.3333333333333333703, 0.3333333333333333703, 0.3333333333333334259, 0.3333333333333332593, 0.3333333333333333703, 0.3333333333333333703, 0.3333333333333333703, 0.3333333333333333703, 0.3333333333333333703, 0.3333333333333334259, 0.3333333333333333148, 0.3333333333333334259, 0.3333333333333333703, 0.3333333333333334814, 0.3333333333333332593, 0.3333333333333333703, 0.3333333333333334814, 0.3333333333333332038, 0.3333333333333334259, 0.3333333333333333148, 0.3333333333333333703, 0.3333333333333334814, 0.3333333333333332038, 0.3333333333333334259, 0.3333333333333333703, 0.3333333333333333703, 0.3333333333333333703, 0.3333333333333334259, 0.3333333333333333703, 0.3333333333333335369, 0.3333333333333333148, 0.3333333333333333148, 0.3333333333333334259, 0.3333333333333333148, 0.3333333333333333703, 0.3333333333333333703, 0.3333333333333334259, 0.3333333333333333148, 0.3333333333333334259, 0.3333333333333332593, 0.3333333333333334814, 0.3333333333333333703, 0.3333333333333333703, 0.3333333333333333703, 0.3333333333333333703, 0.3333333333333333703, 0.3333333333333334259, 0.3333333333333333703, 0.3333333333333334259, 0.3333333333333333148, 0.3333333333333335369, 0.3333333333333332038, 0.3333333333333335369, 0.3333333333333333148, 0.3333333333333334259, 0.3333333333333333703, 0.3333333333333333148, 0.3333333333333334259, 0.3333333333333333148, 0.3333333333333334259, 0.3333333333333332593, 0.3333333333333333148, 0.3333333333333334259, 0.3333333333333334814, 0.3333333333333333703, 0.3333333333333333703, 0.3333333333333334259, 0.3333333333333333148, 0.3333333333333333703, 0.3333333333333333148, 0.3333333333333334259, 0.3333333333333333148, 0.3333333333333333703, 0.3333333333333333703, 0.3333333333333334259, 0.3333333333333333148, 0.3333333333333334259, 0.3333333333333333703, 0.3333333333333333148, 0.3333333333333332593, 0.3333333333333334259, 0.3333333333333333148, 0.3333333333333334259, 0.3333333333333334259, 0.3333333333333334814, 0.3333333333333334259, 0.3333333333333333703, 0.3333333333333333703, 0.3333333333333333148, 0.3333333333333334259, 0.3333333333333333703, 0.3333333333333334259, 0.3333333333333333148, 0.3333333333333333703, 0.3333333333333333703, 0.3333333333333332593, 0.3333333333333334259, 0.3333333333333335369, 0.3333333333333333148, 0.3333333333333334814, 0.3333333333333333703, 0.3333333333333333148, 0.3333333333333334259, 0.3333333333333332593, 0.3333333333333334814, 0.3333333333333333148, 0.3333333333333333703, 0.3333333333333333148, 0.3333333333333334259, 0.3333333333333333148, 0.3333333333333334259, 0.3333333333333333148, 0.3333333333333333703, 0.3333333333333333703, 0.3333333333333333148, 0.3333333333333334259, 0.3333333333333333703, 0.3333333333333333703, 0.3333333333333335369, 0.3333333333333332038, 0.3333333333333334814, 0.3333333333333333148, 0.3333333333333334259, 0.3333333333333334259, 0.3333333333333333703, 0.3333333333333333148, 0.3333333333333334814, 0.3333333333333333703, 0.3333333333333333703, 0.3333333333333333703, 0.3333333333333333703, 0.3333333333333333703, 0.3333333333333334259, 0.3333333333333333703, 0.3333333333333334259, 0.3333333333333333148, 0.3333333333333333703, 0.3333333333333334259, 0.3333333333333334259, 0.3333333333333333703, 0.3333333333333333703, 0.3333333333333334259, 0.3333333333333333703, 0.3333333333333333148, 0.3333333333333333148, 0.3333333333333333703, 0.3333333333333333703, 0.3333333333333334259, 0.3333333333333334259, 0.3333333333333333703, 0.3333333333333333703, 0.3333333333333333703, 0.3333333333333333703, 0.3333333333333333703, 0.3333333333333333148, 0.3333333333333334259, 0.3333333333333334259, 0.3333333333333333703, 0.3333333333333335369, 0.3333333333333332038, 0.3333333333333334814, 0.3333333333333332593, 0.3333333333333333703, 0.3333333333333332593, 0.3333333333333334814, 0.3333333333333333148, 0.3333333333333333703, 0.3333333333333334259, 0.3333333333333334259, 0.3333333333333332593, 0.3333333333333334259, 0.3333333333333333148, 0.3333333333333333703, 0.3333333333333334259, 0.3333333333333334814, 0.3333333333333333148, 0.3333333333333334259, 0.3333333333333333148, 0.3333333333333334814, 0.3333333333333334259, 0.3333333333333333703, 0.3333333333333334259, 0.3333333333333332593, 0.3333333333333333148, 0.3333333333333333703, 0.3333333333333333703, 0.3333333333333334259, 0.3333333333333333703, 0.3333333333333334259, 0.3333333333333333703, 0.3333333333333334259, 0.3333333333333333148, 0.3333333333333333703, 0.3333333333333334259, 0.3333333333333334259, 0.3333333333333333703, 0.3333333333333333703, 0.3333333333333333703, 0.3333333333333333148, 0.3333333333333333703, 0.3333333333333333148, 0.3333333333333334259, 0.3333333333333334259, 0.3333333333333333148, 0.3333333333333333703, 0.3333333333333334259, 0.3333333333333333703, 0.3333333333333333148, 0.3333333333333333703, 0.3333333333333333148, 0.3333333333333333703, 0.3333333333333334259, 0.3333333333333333148, 0.3333333333333334259, 0.3333333333333332593, 0.3333333333333334814, 0.3333333333333334814, 0.3333333333333333148, 0.3333333333333333703, 0.3333333333333334814, 0.3333333333333333148, 0.3333333333333333703, 0.3333333333333334814, 0.3333333333333333703, 0.3333333333333334259, 0.3333333333333334259, 0.3333333333333334814, 0.3333333333333333703, 0.3333333333333333703, 0.3333333333333333703, 0.3333333333333333148, 0.3333333333333333148, 0.3333333333333333703, 0.3333333333333333703, 0.3333333333333333703, 0.3333333333333334259, 0.3333333333333334259, 0.3333333333333333148, 0.3333333333333333148, 0.3333333333333334814, 0.3333333333333333148, 0.3333333333333333148, 0.3333333333333333703, 0.3333333333333333703, 0.3333333333333333703, 0.3333333333333333703),
 ( 0.3333333333333333703, 0.3333333333333333703, 0.3333333333333333703, 0.3333333333333333148, 0.3333333333333333703, 0.3333333333333333148, 0.3333333333333333703, 0.3333333333333334259, 0.3333333333333333703, 0.3333333333333333148, 0.3333333333333334259, 0.3333333333333332593, 0.3333333333333334259, 0.3333333333333333703, 0.3333333333333333703, 0.3333333333333332593, 0.3333333333333334259, 0.3333333333333333148, 0.3333333333333334259, 0.3333333333333333148, 0.3333333333333334259, 0.3333333333333334259, 0.3333333333333333148, 0.3333333333333333148, 0.3333333333333334814, 0.3333333333333332593, 0.3333333333333334259, 0.3333333333333334259, 0.3333333333333333703, 0.3333333333333333703, 0.3333333333333334814, 0.3333333333333332038, 0.3333333333333334814, 0.3333333333333333703, 0.3333333333333334259, 0.3333333333333333148, 0.3333333333333334259, 0.3333333333333334814, 0.3333333333333333703, 0.3333333333333332593, 0.3333333333333334259, 0.3333333333333333148, 0.3333333333333333148, 0.3333333333333333703, 0.3333333333333333703, 0.3333333333333334259, 0.3333333333333333148, 0.3333333333333335369, 0.3333333333333333148, 0.3333333333333334259, 0.3333333333333333703, 0.3333333333333332038, 0.3333333333333334259, 0.3333333333333334259, 0.3333333333333333148, 0.3333333333333334259, 0.3333333333333333703, 0.3333333333333333703, 0.3333333333333334259, 0.3333333333333334259, 0.3333333333333333703, 0.3333333333333334259, 0.3333333333333334259, 0.3333333333333333148, 0.3333333333333333703, 0.3333333333333333703, 0.3333333333333333148, 0.3333333333333334259, 0.3333333333333333148, 0.3333333333333334814, 0.3333333333333333703, 0.3333333333333334259, 0.3333333333333333148, 0.3333333333333333703, 0.3333333333333334259, 0.3333333333333333703, 0.3333333333333333703, 0.3333333333333333148, 0.3333333333333334259, 0.3333333333333333148, 0.3333333333333334259, 0.3333333333333333703, 0.3333333333333334259, 0.3333333333333334814, 0.3333333333333333148, 0.3333333333333334259, 0.3333333333333334259, 0.3333333333333333148, 0.3333333333333333703, 0.3333333333333333703, 0.3333333333333333148, 0.3333333333333334814, 0.3333333333333332593, 0.3333333333333334259, 0.3333333333333333703, 0.3333333333333333148, 0.3333333333333333703, 0.3333333333333333703, 0.3333333333333334259, 0.3333333333333333148, 0.3333333333333334259, 0.3333333333333333148, 0.3333333333333334814, 0.3333333333333333148, 0.3333333333333333148, 0.3333333333333334259, 0.3333333333333333148, 0.3333333333333333703, 0.3333333333333333703, 0.3333333333333334259, 0.3333333333333333703, 0.3333333333333334259, 0.3333333333333333703, 0.3333333333333332593, 0.3333333333333334259, 0.3333333333333333703, 0.3333333333333333148, 0.3333333333333334814, 0.3333333333333333148, 0.3333333333333334259, 0.3333333333333334259, 0.3333333333333333148, 0.3333333333333333703, 0.3333333333333334259, 0.3333333333333333703, 0.3333333333333333703, 0.3333333333333334259, 0.3333333333333333703, 0.3333333333333334259, 0.3333333333333333703, 0.3333333333333334259, 0.3333333333333333148, 0.3333333333333333703, 0.3333333333333333703, 0.3333333333333333703, 0.3333333333333333703, 0.3333333333333335369, 0.3333333333333332593, 0.3333333333333333703, 0.3333333333333333703, 0.3333333333333332593, 0.3333333333333333703, 0.3333333333333333703, 0.3333333333333334259, 0.3333333333333332593, 0.3333333333333333703, 0.3333333333333333703, 0.3333333333333333703, 0.3333333333333333703, 0.3333333333333333703, 0.3333333333333334259, 0.3333333333333333148, 0.3333333333333334259, 0.3333333333333333703, 0.3333333333333334814, 0.3333333333333332593, 0.3333333333333333703, 0.3333333333333334814, 0.3333333333333332038, 0.3333333333333334259, 0.3333333333333333148, 0.3333333333333333703, 0.3333333333333334814, 0.3333333333333332038, 0.3333333333333334259, 0.3333333333333333703, 0.3333333333333333703, 0.3333333333333333703, 0.3333333333333334259, 0.3333333333333333703, 0.3333333333333335369, 0.3333333333333333148, 0.3333333333333333148, 0.3333333333333334259, 0.3333333333333333148, 0.3333333333333333703, 0.3333333333333333703, 0.3333333333333334259, 0.3333333333333333148, 0.3333333333333334259, 0.3333333333333332593, 0.3333333333333334814, 0.3333333333333333703, 0.3333333333333333703, 0.3333333333333333703, 0.3333333333333333703, 0.3333333333333333703, 0.3333333333333334259, 0.3333333333333333703, 0.3333333333333334259, 0.3333333333333333148, 0.3333333333333335369, 0.3333333333333332038, 0.3333333333333335369, 0.3333333333333333148, 0.3333333333333334259, 0.3333333333333333703, 0.3333333333333333148, 0.3333333333333334259, 0.3333333333333333148, 0.3333333333333334259, 0.3333333333333332593, 0.3333333333333333148, 0.3333333333333334259, 0.3333333333333334814, 0.3333333333333333703, 0.3333333333333333703, 0.3333333333333334259, 0.3333333333333333148, 0.3333333333333333703, 0.3333333333333333148, 0.3333333333333334259, 0.3333333333333333148, 0.3333333333333333703, 0.3333333333333333703, 0.3333333333333334259, 0.3333333333333333148, 0.3333333333333334259, 0.3333333333333333703, 0.3333333333333333148, 0.3333333333333332593, 0.3333333333333334259, 0.3333333333333333148, 0.3333333333333334259, 0.3333333333333334259, 0.3333333333333334814, 0.3333333333333334259, 0.3333333333333333703, 0.3333333333333333703, 0.3333333333333333148, 0.3333333333333334259, 0.3333333333333333703, 0.3333333333333334259, 0.3333333333333333148, 0.3333333333333333703, 0.3333333333333333703, 0.3333333333333332593, 0.3333333333333334259, 0.3333333333333335369, 0.3333333333333333148, 0.3333333333333334814, 0.3333333333333333703, 0.3333333333333333148, 0.3333333333333334259, 0.3333333333333332593, 0.3333333333333334814, 0.3333333333333333148, 0.3333333333333333703, 0.3333333333333333148, 0.3333333333333334259, 0.3333333333333333148, 0.3333333333333334259, 0.3333333333333333148, 0.3333333333333333703, 0.3333333333333333703, 0.3333333333333333148, 0.3333333333333334259, 0.3333333333333333703, 0.3333333333333333703, 0.3333333333333335369, 0.3333333333333332038, 0.3333333333333334814, 0.3333333333333333148, 0.3333333333333334259, 0.3333333333333334259, 0.3333333333333333703, 0.3333333333333333148, 0.3333333333333334814, 0.3333333333333333703, 0.3333333333333333703, 0.3333333333333333703, 0.3333333333333333703, 0.3333333333333333703, 0.3333333333333334259, 0.3333333333333333703, 0.3333333333333334259, 0.3333333333333333148, 0.3333333333333333703, 0.3333333333333334259, 0.3333333333333334259, 0.3333333333333333703, 0.3333333333333333703, 0.3333333333333334259, 0.3333333333333333703, 0.3333333333333333148, 0.3333333333333333148, 0.3333333333333333703, 0.3333333333333333703, 0.3333333333333334259, 0.3333333333333334259, 0.3333333333333333703, 0.3333333333333333703, 0.3333333333333333703, 0.3333333333333333703, 0.3333333333333333703, 0.3333333333333333148, 0.3333333333333334259, 0.3333333333333334259, 0.3333333333333333703, 0.3333333333333335369, 0.3333333333333332038, 0.3333333333333334814, 0.3333333333333332593, 0.3333333333333333703, 0.3333333333333332593, 0.3333333333333334814, 0.3333333333333333148, 0.3333333333333333703, 0.3333333333333334259, 0.3333333333333334259, 0.3333333333333332593, 0.3333333333333334259, 0.3333333333333333148, 0.3333333333333333703, 0.3333333333333334259, 0.3333333333333334814, 0.3333333333333333148, 0.3333333333333334259, 0.3333333333333333148, 0.3333333333333334814, 0.3333333333333334259, 0.3333333333333333703, 0.3333333333333334259, 0.3333333333333332593, 0.3333333333333333148, 0.3333333333333333703, 0.3333333333333333703, 0.3333333333333334259, 0.3333333333333333703, 0.3333333333333334259, 0.3333333333333333703, 0.3333333333333334259, 0.3333333333333333148, 0.3333333333333333703, 0.3333333333333334259, 0.3333333333333334259, 0.3333333333333333703, 0.3333333333333333703, 0.3333333333333333703, 0.3333333333333333148, 0.3333333333333333703, 0.3333333333333333148, 0.3333333333333334259, 0.3333333333333334259, 0.3333333333333333148, 0.3333333333333333703, 0.3333333333333334259, 0.3333333333333333703, 0.3333333333333333148, 0.3333333333333333703, 0.3333333333333333148, 0.3333333333333333703, 0.3333333333333334259, 0.3333333333333333148, 0.3333333333333334259, 0.3333333333333332593, 0.3333333333333334814, 0.3333333333333334814, 0.3333333333333333148, 0.3333333333333333703, 0.3333333333333334814, 0.3333333333333333148, 0.3333333333333333703, 0.3333333333333334814, 0.3333333333333333703, 0.3333333333333334259, 0.3333333333333334259, 0.3333333333333334814, 0.3333333333333333703, 0.3333333333333333703, 0.3333333333333333703, 0.3333333333333333148, 0.3333333333333333148, 0.3333333333333333703, 0.3333333333333333703, 0.3333333333333333703, 0.3333333333333334259, 0.3333333333333334259, 0.3333333333333333148, 0.3333333333333333148, 0.3333333333333334814, 0.3333333333333333148, 0.3333333333333333148, 0.3333333333333333703, 0.3333333333333333703, 0.3333333333333333703, 0.3333333333333333703),
 ( 1.000000000000000000, 1.000000000000000000, 1.000000000000000000, 0.9999999999999997780, 1.000000000000000000, 1.000000000000000000, 1.000000000000000000, 1.000000000000000222, 1.000000000000000000, 1.000000000000000000, 1.000000000000000222, 0.9999999999999997780, 1.000000000000000222, 1.000000000000000222, 1.000000000000000000, 1.000000000000000000, 1.000000000000000000, 0.9999999999999997780, 1.000000000000000222, 0.9999999999999996669, 1.000000000000000222, 1.000000000000000000, 1.000000000000000000, 0.9999999999999996669, 1.000000000000000444, 0.9999999999999996669, 1.000000000000000444, 1.000000000000000000, 1.000000000000000000, 0.9999999999999997780, 1.000000000000000222, 0.9999999999999994449, 1.000000000000000444, 1.000000000000000000, 1.000000000000000000, 1.000000000000000000, 1.000000000000000000, 1.000000000000000444, 0.9999999999999997780, 1.000000000000000000, 1.000000000000000000, 1.000000000000000000, 1.000000000000000000, 1.000000000000000000, 1.000000000000000000, 0.9999999999999997780, 1.000000000000000000, 1.000000000000000444, 0.9999999999999997780, 1.000000000000000444, 0.9999999999999997780, 0.9999999999999997780, 1.000000000000000000, 1.000000000000000222, 1.000000000000000000, 1.000000000000000000, 1.000000000000000000, 1.000000000000000000, 0.9999999999999997780, 1.000000000000000444, 0.9999999999999997780, 1.000000000000000000, 1.000000000000000222, 0.9999999999999997780, 1.000000000000000000, 1.000000000000000222, 0.9999999999999997780, 1.000000000000000222, 1.000000000000000000, 1.000000000000000222, 1.000000000000000000, 1.000000000000000222, 0.9999999999999997780, 1.000000000000000000, 1.000000000000000222, 1.000000000000000000, 1.000000000000000222, 0.9999999999999997780, 1.000000000000000222, 0.9999999999999997780, 1.000000000000000222, 0.9999999999999997780, 1.000000000000000222, 1.000000000000000222, 0.9999999999999997780, 1.000000000000000222, 1.000000000000000222, 0.9999999999999997780, 1.000000000000000222, 1.000000000000000000, 1.000000000000000000, 1.000000000000000222, 0.9999999999999996669, 1.000000000000000444, 0.9999999999999997780, 0.9999999999999997780, 1.000000000000000000, 1.000000000000000000, 1.000000000000000000, 0.9999999999999996669, 1.000000000000000444, 1.000000000000000000, 1.000000000000000222, 1.000000000000000000, 0.9999999999999997780, 1.000000000000000222, 0.9999999999999997780, 1.000000000000000222, 1.000000000000000000, 1.000000000000000000, 1.000000000000000222, 1.000000000000000000, 1.000000000000000222, 0.9999999999999994449, 1.000000000000000444, 1.000000000000000000, 0.9999999999999996669, 1.000000000000000222, 0.9999999999999997780, 1.000000000000000222, 0.9999999999999997780, 1.000000000000000000, 1.000000000000000000, 1.000000000000000000, 1.000000000000000000, 1.000000000000000000, 1.000000000000000444, 1.000000000000000000, 1.000000000000000000, 1.000000000000000222, 1.000000000000000000, 1.000000000000000000, 0.9999999999999997780, 1.000000000000000000, 1.000000000000000222, 1.000000000000000000, 1.000000000000000222, 0.9999999999999997780, 1.000000000000000000, 0.9999999999999997780, 0.9999999999999997780, 1.000000000000000222, 0.9999999999999997780, 1.000000000000000444, 0.9999999999999997780, 1.000000000000000000, 1.000000000000000222, 1.000000000000000000, 1.000000000000000000, 0.9999999999999997780, 1.000000000000000222, 1.000000000000000000, 1.000000000000000000, 1.000000000000000000, 1.000000000000000222, 0.9999999999999996669, 1.000000000000000222, 1.000000000000000222, 0.9999999999999996669, 1.000000000000000444, 0.9999999999999996669, 1.000000000000000000, 1.000000000000000222, 0.9999999999999996669, 1.000000000000000222, 1.000000000000000000, 1.000000000000000222, 1.000000000000000000, 1.000000000000000222, 0.9999999999999997780, 1.000000000000000444, 0.9999999999999997780, 0.9999999999999997780, 1.000000000000000222, 0.9999999999999996669, 1.000000000000000222, 1.000000000000000000, 1.000000000000000000, 1.000000000000000000, 0.9999999999999997780, 1.000000000000000222, 1.000000000000000222, 0.9999999999999997780, 1.000000000000000222, 0.9999999999999997780, 1.000000000000000222, 1.000000000000000000, 1.000000000000000444, 1.000000000000000000, 1.000000000000000222, 0.9999999999999996669, 1.000000000000000444, 0.9999999999999993339, 1.000000000000000444, 0.9999999999999997780, 1.000000000000000444, 0.9999999999999997780, 1.000000000000000000, 1.000000000000000000, 0.9999999999999997780, 1.000000000000000222, 0.9999999999999997780, 0.9999999999999996669, 1.000000000000000444, 1.000000000000000222, 1.000000000000000000, 0.9999999999999997780, 1.000000000000000222, 0.9999999999999996669, 1.000000000000000222, 0.9999999999999997780, 1.000000000000000222, 1.000000000000000000, 1.000000000000000000, 1.000000000000000000, 1.000000000000000000, 0.9999999999999997780, 1.000000000000000000, 1.000000000000000000, 0.9999999999999997780, 1.000000000000000000, 1.000000000000000000, 1.000000000000000000, 1.000000000000000222, 1.000000000000000000, 1.000000000000000444, 1.000000000000000222, 1.000000000000000000, 1.000000000000000000, 0.9999999999999997780, 1.000000000000000222, 1.000000000000000000, 1.000000000000000000, 1.000000000000000000, 0.9999999999999997780, 1.000000000000000222, 0.9999999999999997780, 1.000000000000000222, 1.000000000000000444, 0.9999999999999997780, 1.000000000000000222, 1.000000000000000000, 1.000000000000000000, 1.000000000000000000, 0.9999999999999997780, 1.000000000000000444, 0.9999999999999997780, 1.000000000000000222, 0.9999999999999997780, 1.000000000000000222, 0.9999999999999994449, 1.000000000000000222, 1.000000000000000000, 1.000000000000000222, 1.000000000000000000, 0.9999999999999997780, 1.000000000000000222, 1.000000000000000000, 0.9999999999999997780, 1.000000000000000444, 0.9999999999999996669, 1.000000000000000222, 1.000000000000000000, 1.000000000000000000, 1.000000000000000222, 0.9999999999999997780, 0.9999999999999997780, 1.000000000000000444, 1.000000000000000222, 1.000000000000000000, 0.9999999999999997780, 0.9999999999999997780, 1.000000000000000222, 1.000000000000000000, 1.000000000000000222, 1.000000000000000000, 0.9999999999999997780, 1.000000000000000000, 1.000000000000000000, 1.000000000000000000, 1.000000000000000222, 0.9999999999999997780, 1.000000000000000222, 1.000000000000000000, 1.000000000000000000, 1.000000000000000000, 0.9999999999999997780, 1.000000000000000000, 1.000000000000000222, 1.000000000000000222, 0.9999999999999996669, 1.000000000000000444, 0.9999999999999996669, 1.000000000000000222, 1.000000000000000000, 1.000000000000000222, 0.9999999999999997780, 1.000000000000000444, 1.000000000000000000, 1.000000000000000444, 0.9999999999999994449, 1.000000000000000222, 0.9999999999999997780, 0.9999999999999997780, 1.000000000000000000, 1.000000000000000222, 1.000000000000000000, 1.000000000000000000, 1.000000000000000000, 1.000000000000000222, 0.9999999999999996669, 1.000000000000000222, 1.000000000000000000, 0.9999999999999996669, 1.000000000000000444, 1.000000000000000000, 1.000000000000000000, 1.000000000000000000, 0.9999999999999996669, 1.000000000000000222, 1.000000000000000000, 1.000000000000000000, 1.000000000000000222, 0.9999999999999997780, 0.9999999999999997780, 1.000000000000000000, 1.000000000000000000, 1.000000000000000222, 0.9999999999999997780, 1.000000000000000222, 1.000000000000000000, 1.000000000000000000, 0.9999999999999996669, 1.000000000000000222, 1.000000000000000000, 1.000000000000000222, 1.000000000000000000, 1.000000000000000000, 1.000000000000000000, 0.9999999999999997780, 1.000000000000000222, 0.9999999999999996669, 1.000000000000000444, 1.000000000000000000, 0.9999999999999997780, 1.000000000000000000, 1.000000000000000222, 1.000000000000000222, 0.9999999999999996669, 1.000000000000000000, 1.000000000000000000, 0.9999999999999997780, 1.000000000000000222, 1.000000000000000000, 1.000000000000000222, 0.9999999999999996669, 1.000000000000000444, 1.000000000000000000, 1.000000000000000000, 1.000000000000000000, 1.000000000000000222, 1.000000000000000000, 0.9999999999999997780, 1.000000000000000444, 1.000000000000000000, 1.000000000000000444, 0.9999999999999997780, 1.000000000000000444, 1.000000000000000000, 1.000000000000000222, 1.000000000000000222, 1.000000000000000000, 0.9999999999999996669, 1.000000000000000000, 1.000000000000000000, 1.000000000000000000, 1.000000000000000000, 1.000000000000000222, 0.9999999999999996669, 1.000000000000000000, 1.000000000000000222, 0.9999999999999997780, 0.9999999999999997780, 1.000000000000000000, 1.000000000000000000, 1.000000000000000000, 1.000000000000000000),
 ( 0.3333333333333333703, 0.3333333333333333703, 0.3333333333333333703, 0.3333333333333333148, 0.3333333333333333703, 0.3333333333333333148, 0.3333333333333333703, 0.3333333333333334259, 0.3333333333333333703, 0.3333333333333333148, 0.3333333333333334259, 0.3333333333333332593, 0.3333333333333334259, 0.3333333333333333703, 0.3333333333333333703, 0.3333333333333332593, 0.3333333333333334259, 0.3333333333333333148, 0.3333333333333334259, 0.3333333333333333148, 0.3333333333333334259, 0.3333333333333334259, 0.3333333333333333148, 0.3333333333333333148, 0.3333333333333334814, 0.3333333333333332593, 0.3333333333333334259, 0.3333333333333334259, 0.3333333333333333703, 0.3333333333333333703, 0.3333333333333334814, 0.3333333333333332038, 0.3333333333333334814, 0.3333333333333333703, 0.3333333333333334259, 0.3333333333333333148, 0.3333333333333334259, 0.3333333333333334814, 0.3333333333333333703, 0.3333333333333332593, 0.3333333333333334259, 0.3333333333333333148, 0.3333333333333333148, 0.3333333333333333703, 0.3333333333333333703, 0.3333333333333334259, 0.3333333333333333148, 0.3333333333333335369, 0.3333333333333333148, 0.3333333333333334259, 0.3333333333333333703, 0.3333333333333332038, 0.3333333333333334259, 0.3333333333333334259, 0.3333333333333333148, 0.3333333333333334259, 0.3333333333333333703, 0.3333333333333333703, 0.3333333333333334259, 0.3333333333333334259, 0.3333333333333333703, 0.3333333333333334259, 0.3333333333333334259, 0.3333333333333333148, 0.3333333333333333703, 0.3333333333333333703, 0.3333333333333333148, 0.3333333333333334259, 0.3333333333333333148, 0.3333333333333334814, 0.3333333333333333703, 0.3333333333333334259, 0.3333333333333333148, 0.3333333333333333703, 0.3333333333333334259, 0.3333333333333333703, 0.3333333333333333703, 0.3333333333333333148, 0.3333333333333334259, 0.3333333333333333148, 0.3333333333333334259, 0.3333333333333333703, 0.3333333333333334259, 0.3333333333333334814, 0.3333333333333333148, 0.3333333333333334259, 0.3333333333333334259, 0.3333333333333333148, 0.3333333333333333703, 0.3333333333333333703, 0.3333333333333333148, 0.3333333333333334814, 0.3333333333333332593, 0.3333333333333334259, 0.3333333333333333703, 0.3333333333333333148, 0.3333333333333333703, 0.3333333333333333703, 0.3333333333333334259, 0.3333333333333333148, 0.3333333333333334259, 0.3333333333333333148, 0.3333333333333334814, 0.3333333333333333148, 0.3333333333333333148, 0.3333333333333334259, 0.3333333333333333148, 0.3333333333333333703, 0.3333333333333333703, 0.3333333333333334259, 0.3333333333333333703, 0.3333333333333334259, 0.3333333333333333703, 0.3333333333333332593, 0.3333333333333334259, 0.3333333333333333703, 0.3333333333333333148, 0.3333333333333334814, 0.3333333333333333148, 0.3333333333333334259, 0.3333333333333334259, 0.3333333333333333148, 0.3333333333333333703, 0.3333333333333334259, 0.3333333333333333703, 0.3333333333333333703, 0.3333333333333334259, 0.3333333333333333703, 0.3333333333333334259, 0.3333333333333333703, 0.3333333333333334259, 0.3333333333333333148, 0.3333333333333333703, 0.3333333333333333703, 0.3333333333333333703, 0.3333333333333333703, 0.3333333333333335369, 0.3333333333333332593, 0.3333333333333333703, 0.3333333333333333703, 0.3333333333333332593, 0.3333333333333333703, 0.3333333333333333703, 0.3333333333333334259, 0.3333333333333332593, 0.3333333333333333703, 0.3333333333333333703, 0.3333333333333333703, 0.3333333333333333703, 0.3333333333333333703, 0.3333333333333334259, 0.3333333333333333148, 0.3333333333333334259, 0.3333333333333333703, 0.3333333333333334814, 0.3333333333333332593, 0.3333333333333333703, 0.3333333333333334814, 0.3333333333333332038, 0.3333333333333334259, 0.3333333333333333148, 0.3333333333333333703, 0.3333333333333334814, 0.3333333333333332038, 0.3333333333333334259, 0.3333333333333333703, 0.3333333333333333703, 0.3333333333333333703, 0.3333333333333334259, 0.3333333333333333703, 0.3333333333333335369, 0.3333333333333333148, 0.3333333333333333148, 0.3333333333333334259, 0.3333333333333333148, 0.3333333333333333703, 0.3333333333333333703, 0.3333333333333334259, 0.3333333333333333148, 0.3333333333333334259, 0.3333333333333332593, 0.3333333333333334814, 0.3333333333333333703, 0.3333333333333333703, 0.3333333333333333703, 0.3333333333333333703, 0.3333333333333333703, 0.3333333333333334259, 0.3333333333333333703, 0.3333333333333334259, 0.3333333333333333148, 0.3333333333333335369, 0.3333333333333332038, 0.3333333333333335369, 0.3333333333333333148, 0.3333333333333334259, 0.3333333333333333703, 0.3333333333333333148, 0.3333333333333334259, 0.3333333333333333148, 0.3333333333333334259, 0.3333333333333332593, 0.3333333333333333148, 0.3333333333333334259, 0.3333333333333334814, 0.3333333333333333703, 0.3333333333333333703, 0.3333333333333334259, 0.3333333333333333148, 0.3333333333333333703, 0.3333333333333333148, 0.3333333333333334259, 0.3333333333333333148, 0.3333333333333333703, 0.3333333333333333703, 0.3333333333333334259, 0.3333333333333333148, 0.3333333333333334259, 0.3333333333333333703, 0.3333333333333333148, 0.3333333333333332593, 0.3333333333333334259, 0.3333333333333333148, 0.3333333333333334259, 0.3333333333333334259, 0.3333333333333334814, 0.3333333333333334259, 0.3333333333333333703, 0.3333333333333333703, 0.3333333333333333148, 0.3333333333333334259, 0.3333333333333333703, 0.3333333333333334259, 0.3333333333333333148, 0.3333333333333333703, 0.3333333333333333703, 0.3333333333333332593, 0.3333333333333334259, 0.3333333333333335369, 0.3333333333333333148, 0.3333333333333334814, 0.3333333333333333703, 0.3333333333333333148, 0.3333333333333334259, 0.3333333333333332593, 0.3333333333333334814, 0.3333333333333333148, 0.3333333333333333703, 0.3333333333333333148, 0.3333333333333334259, 0.3333333333333333148, 0.3333333333333334259, 0.3333333333333333148, 0.3333333333333333703, 0.3333333333333333703, 0.3333333333333333148, 0.3333333333333334259, 0.3333333333333333703, 0.3333333333333333703, 0.3333333333333335369, 0.3333333333333332038, 0.3333333333333334814, 0.3333333333333333148, 0.3333333333333334259, 0.3333333333333334259, 0.3333333333333333703, 0.3333333333333333148, 0.3333333333333334814, 0.3333333333333333703, 0.3333333333333333703, 0.3333333333333333703, 0.3333333333333333703, 0.3333333333333333703, 0.3333333333333334259, 0.3333333333333333703, 0.3333333333333334259, 0.3333333333333333148, 0.3333333333333333703, 0.3333333333333334259, 0.3333333333333334259, 0.3333333333333333703, 0.3333333333333333703, 0.3333333333333334259, 0.3333333333333333703, 0.3333333333333333148, 0.3333333333333333148, 0.3333333333333333703, 0.3333333333333333703, 0.3333333333333334259, 0.3333333333333334259, 0.3333333333333333703, 0.3333333333333333703, 0.3333333333333333703, 0.3333333333333333703, 0.3333333333333333703, 0.3333333333333333148, 0.3333333333333334259, 0.3333333333333334259, 0.3333333333333333703, 0.3333333333333335369, 0.3333333333333332038, 0.3333333333333334814, 0.3333333333333332593, 0.3333333333333333703, 0.3333333333333332593, 0.3333333333333334814, 0.3333333333333333148, 0.3333333333333333703, 0.3333333333333334259, 0.3333333333333334259, 0.3333333333333332593, 0.3333333333333334259, 0.3333333333333333148, 0.3333333333333333703, 0.3333333333333334259, 0.3333333333333334814, 0.3333333333333333148, 0.3333333333333334259, 0.3333333333333333148, 0.3333333333333334814, 0.3333333333333334259, 0.3333333333333333703, 0.3333333333333334259, 0.3333333333333332593, 0.3333333333333333148, 0.3333333333333333703, 0.3333333333333333703, 0.3333333333333334259, 0.3333333333333333703, 0.3333333333333334259, 0.3333333333333333703, 0.3333333333333334259, 0.3333333333333333148, 0.3333333333333333703, 0.3333333333333334259, 0.3333333333333334259, 0.3333333333333333703, 0.3333333333333333703, 0.3333333333333333703, 0.3333333333333333148, 0.3333333333333333703, 0.3333333333333333148, 0.3333333333333334259, 0.3333333333333334259, 0.3333333333333333148, 0.3333333333333333703, 0.3333333333333334259, 0.3333333333333333703, 0.3333333333333333148, 0.3333333333333333703, 0.3333333333333333148, 0.3333333333333333703, 0.3333333333333334259, 0.3333333333333333148, 0.3333333333333334259, 0.3333333333333332593, 0.3333333333333334814, 0.3333333333333334814, 0.3333333333333333148, 0.3333333333333333703, 0.3333333333333334814, 0.3333333333333333148, 0.3333333333333333703, 0.3333333333333334814, 0.3333333333333333703, 0.3333333333333334259, 0.3333333333333334259, 0.3333333333333334814, 0.3333333333333333703, 0.3333333333333333703, 0.3333333333333333703, 0.3333333333333333148, 0.3333333333333333148, 0.3333333333333333703, 0.3333333333333333703, 0.3333333333333333703, 0.3333333333333334259, 0.3333333333333334259, 0.3333333333333333148, 0.3333333333333333148, 0.3333333333333334814, 0.3333333333333333148, 0.3333333333333333148, 0.3333333333333333703, 0.3333333333333333703, 0.3333333333333333703, 0.3333333333333333703),
 ( 0.3333333333333333703, 0.3333333333333333703, 0.3333333333333333703, 0.3333333333333333148, 0.3333333333333333703, 0.3333333333333333148, 0.3333333333333333703, 0.3333333333333334259, 0.3333333333333333703, 0.3333333333333333148, 0.3333333333333334259, 0.3333333333333332593, 0.3333333333333334259, 0.3333333333333333703, 0.3333333333333333703, 0.3333333333333332593, 0.3333333333333334259, 0.3333333333333333148, 0.3333333333333334259, 0.3333333333333333148, 0.3333333333333334259, 0.3333333333333334259, 0.3333333333333333148, 0.3333333333333333148, 0.3333333333333334814, 0.3333333333333332593, 0.3333333333333334259, 0.3333333333333334259, 0.3333333333333333703, 0.3333333333333333703, 0.3333333333333334814, 0.3333333333333332038, 0.3333333333333334814, 0.3333333333333333703, 0.3333333333333334259, 0.3333333333333333148, 0.3333333333333334259, 0.3333333333333334814, 0.3333333333333333703, 0.3333333333333332593, 0.3333333333333334259, 0.3333333333333333148, 0.3333333333333333148, 0.3333333333333333703, 0.3333333333333333703, 0.3333333333333334259, 0.3333333333333333148, 0.3333333333333335369, 0.3333333333333333148, 0.3333333333333334259, 0.3333333333333333703, 0.3333333333333332038, 0.3333333333333334259, 0.3333333333333334259, 0.3333333333333333148, 0.3333333333333334259, 0.3333333333333333703, 0.3333333333333333703, 0.3333333333333334259, 0.3333333333333334259, 0.3333333333333333703, 0.3333333333333334259, 0.3333333333333334259, 0.3333333333333333148, 0.3333333333333333703, 0.3333333333333333703, 0.3333333333333333148, 0.3333333333333334259, 0.3333333333333333148, 0.3333333333333334814, 0.3333333333333333703, 0.3333333333333334259, 0.3333333333333333148, 0.3333333333333333703, 0.3333333333333334259, 0.3333333333333333703, 0.3333333333333333703, 0.3333333333333333148, 0.3333333333333334259, 0.3333333333333333148, 0.3333333333333334259, 0.3333333333333333703, 0.3333333333333334259, 0.3333333333333334814, 0.3333333333333333148, 0.3333333333333334259, 0.3333333333333334259, 0.3333333333333333148, 0.3333333333333333703, 0.3333333333333333703, 0.3333333333333333148, 0.3333333333333334814, 0.3333333333333332593, 0.3333333333333334259, 0.3333333333333333703, 0.3333333333333333148, 0.3333333333333333703, 0.3333333333333333703, 0.3333333333333334259, 0.3333333333333333148, 0.3333333333333334259, 0.3333333333333333148, 0.3333333333333334814, 0.3333333333333333148, 0.3333333333333333148, 0.3333333333333334259, 0.3333333333333333148, 0.3333333333333333703, 0.3333333333333333703, 0.3333333333333334259, 0.3333333333333333703, 0.3333333333333334259, 0.3333333333333333703, 0.3333333333333332593, 0.3333333333333334259, 0.3333333333333333703, 0.3333333333333333148, 0.3333333333333334814, 0.3333333333333333148, 0.3333333333333334259, 0.3333333333333334259, 0.3333333333333333148, 0.3333333333333333703, 0.3333333333333334259, 0.3333333333333333703, 0.3333333333333333703, 0.3333333333333334259, 0.3333333333333333703, 0.3333333333333334259, 0.3333333333333333703, 0.3333333333333334259, 0.3333333333333333148, 0.3333333333333333703, 0.3333333333333333703, 0.3333333333333333703, 0.3333333333333333703, 0.3333333333333335369, 0.3333333333333332593, 0.3333333333333333703, 0.3333333333333333703, 0.3333333333333332593, 0.3333333333333333703, 0.3333333333333333703, 0.3333333333333334259, 0.3333333333333332593, 0.3333333333333333703, 0.3333333333333333703, 0.3333333333333333703, 0.3333333333333333703, 0.3333333333333333703, 0.3333333333333334259, 0.3333333333333333148, 0.3333333333333334259, 0.3333333333333333703, 0.3333333333333334814, 0.3333333333333332593, 0.3333333333333333703, 0.3333333333333334814, 0.3333333333333332038, 0.3333333333333334259, 0.3333333333333333148, 0.3333333333333333703, 0.3333333333333334814, 0.3333333333333332038, 0.3333333333333334259, 0.3333333333333333703, 0.3333333333333333703, 0.3333333333333333703, 0.3333333333333334259, 0.3333333333333333703, 0.3333333333333335369, 0.3333333333333333148, 0.3333333333333333148, 0.3333333333333334259, 0.3333333333333333148, 0.3333333333333333703, 0.3333333333333333703, 0.3333333333333334259, 0.3333333333333333148, 0.3333333333333334259, 0.3333333333333332593, 0.3333333333333334814, 0.3333333333333333703, 0.3333333333333333703, 0.3333333333333333703, 0.3333333333333333703, 0.3333333333333333703, 0.3333333333333334259, 0.3333333333333333703, 0.3333333333333334259, 0.3333333333333333148, 0.3333333333333335369, 0.3333333333333332038, 0.3333333333333335369, 0.3333333333333333148, 0.3333333333333334259, 0.3333333333333333703, 0.3333333333333333148, 0.3333333333333334259, 0.3333333333333333148, 0.3333333333333334259, 0.3333333333333332593, 0.3333333333333333148, 0.3333333333333334259, 0.3333333333333334814, 0.3333333333333333703, 0.3333333333333333703, 0.3333333333333334259, 0.3333333333333333148, 0.3333333333333333703, 0.3333333333333333148, 0.3333333333333334259, 0.3333333333333333148, 0.3333333333333333703, 0.3333333333333333703, 0.3333333333333334259, 0.3333333333333333148, 0.3333333333333334259, 0.3333333333333333703, 0.3333333333333333148, 0.3333333333333332593, 0.3333333333333334259, 0.3333333333333333148, 0.3333333333333334259, 0.3333333333333334259, 0.3333333333333334814, 0.3333333333333334259, 0.3333333333333333703, 0.3333333333333333703, 0.3333333333333333148, 0.3333333333333334259, 0.3333333333333333703, 0.3333333333333334259, 0.3333333333333333148, 0.3333333333333333703, 0.3333333333333333703, 0.3333333333333332593, 0.3333333333333334259, 0.3333333333333335369, 0.3333333333333333148, 0.3333333333333334814, 0.3333333333333333703, 0.3333333333333333148, 0.3333333333333334259, 0.3333333333333332593, 0.3333333333333334814, 0.3333333333333333148, 0.3333333333333333703, 0.3333333333333333148, 0.3333333333333334259, 0.3333333333333333148, 0.3333333333333334259, 0.3333333333333333148, 0.3333333333333333703, 0.3333333333333333703, 0.3333333333333333148, 0.3333333333333334259, 0.3333333333333333703, 0.3333333333333333703, 0.3333333333333335369, 0.3333333333333332038, 0.3333333333333334814, 0.3333333333333333148, 0.3333333333333334259, 0.3333333333333334259, 0.3333333333333333703, 0.3333333333333333148, 0.3333333333333334814, 0.3333333333333333703, 0.3333333333333333703, 0.3333333333333333703, 0.3333333333333333703, 0.3333333333333333703, 0.3333333333333334259, 0.3333333333333333703, 0.3333333333333334259, 0.3333333333333333148, 0.3333333333333333703, 0.3333333333333334259, 0.3333333333333334259, 0.3333333333333333703, 0.3333333333333333703, 0.3333333333333334259, 0.3333333333333333703, 0.3333333333333333148, 0.3333333333333333148, 0.3333333333333333703, 0.3333333333333333703, 0.3333333333333334259, 0.3333333333333334259, 0.3333333333333333703, 0.3333333333333333703, 0.3333333333333333703, 0.3333333333333333703, 0.3333333333333333703, 0.3333333333333333148, 0.3333333333333334259, 0.3333333333333334259, 0.3333333333333333703, 0.3333333333333335369, 0.3333333333333332038, 0.3333333333333334814, 0.3333333333333332593, 0.3333333333333333703, 0.3333333333333332593, 0.3333333333333334814, 0.3333333333333333148, 0.3333333333333333703, 0.3333333333333334259, 0.3333333333333334259, 0.3333333333333332593, 0.3333333333333334259, 0.3333333333333333148, 0.3333333333333333703, 0.3333333333333334259, 0.3333333333333334814, 0.3333333333333333148, 0.3333333333333334259, 0.3333333333333333148, 0.3333333333333334814, 0.3333333333333334259, 0.3333333333333333703, 0.3333333333333334259, 0.3333333333333332593, 0.3333333333333333148, 0.3333333333333333703, 0.3333333333333333703, 0.3333333333333334259, 0.3333333333333333703, 0.3333333333333334259, 0.3333333333333333703, 0.3333333333333334259, 0.3333333333333333148, 0.3333333333333333703, 0.3333333333333334259, 0.3333333333333334259, 0.3333333333333333703, 0.3333333333333333703, 0.3333333333333333703, 0.3333333333333333148, 0.3333333333333333703, 0.3333333333333333148, 0.3333333333333334259, 0.3333333333333334259, 0.3333333333333333148, 0.3333333333333333703, 0.3333333333333334259, 0.3333333333333333703, 0.3333333333333333148, 0.3333333333333333703, 0.3333333333333333148, 0.3333333333333333703, 0.3333333333333334259, 0.3333333333333333148, 0.3333333333333334259, 0.3333333333333332593, 0.3333333333333334814, 0.3333333333333334814, 0.3333333333333333148, 0.3333333333333333703, 0.3333333333333334814, 0.3333333333333333148, 0.3333333333333333703, 0.3333333333333334814, 0.3333333333333333703, 0.3333333333333334259, 0.3333333333333334259, 0.3333333333333334814, 0.3333333333333333703, 0.3333333333333333703, 0.3333333333333333703, 0.3333333333333333148, 0.3333333333333333148, 0.3333333333333333703, 0.3333333333333333703, 0.3333333333333333703, 0.3333333333333334259, 0.3333333333333334259, 0.3333333333333333148, 0.3333333333333333148, 0.3333333333333334814, 0.3333333333333333148, 0.3333333333333333148, 0.3333333333333333703, 0.3333333333333333703, 0.3333333333333333703, 0.3333333333333333703),
 ( 1.000000000000000000, 1.000000000000000000, 1.000000000000000000, 0.9999999999999997780, 1.000000000000000000, 1.000000000000000000, 1.000000000000000000, 1.000000000000000222, 1.000000000000000000, 1.000000000000000000, 1.000000000000000222, 0.9999999999999997780, 1.000000000000000222, 1.000000000000000222, 1.000000000000000000, 1.000000000000000000, 1.000000000000000000, 0.9999999999999997780, 1.000000000000000222, 0.9999999999999996669, 1.000000000000000222, 1.000000000000000000, 1.000000000000000000, 0.9999999999999996669, 1.000000000000000444, 0.9999999999999996669, 1.000000000000000444, 1.000000000000000000, 1.000000000000000000, 0.9999999999999997780, 1.000000000000000222, 0.9999999999999994449, 1.000000000000000444, 1.000000000000000000, 1.000000000000000000, 1.000000000000000000, 1.000000000000000000, 1.000000000000000444, 0.9999999999999997780, 1.000000000000000000, 1.000000000000000000, 1.000000000000000000, 1.000000000000000000, 1.000000000000000000, 1.000000000000000000, 0.9999999999999997780, 1.000000000000000000, 1.000000000000000444, 0.9999999999999997780, 1.000000000000000444, 0.9999999999999997780, 0.9999999999999997780, 1.000000000000000000, 1.000000000000000222, 1.000000000000000000, 1.000000000000000000, 1.000000000000000000, 1.000000000000000000, 0.9999999999999997780, 1.000000000000000444, 0.9999999999999997780, 1.000000000000000000, 1.000000000000000222, 0.9999999999999997780, 1.000000000000000000, 1.000000000000000222, 0.9999999999999997780, 1.000000000000000222, 1.000000000000000000, 1.000000000000000222, 1.000000000000000000, 1.000000000000000222, 0.9999999999999997780, 1.000000000000000000, 1.000000000000000222, 1.000000000000000000, 1.000000000000000222, 0.9999999999999997780, 1.000000000000000222, 0.9999999999999997780, 1.000000000000000222, 0.9999999999999997780, 1.000000000000000222, 1.000000000000000222, 0.9999999999999997780, 1.000000000000000222, 1.000000000000000222, 0.9999999999999997780, 1.000000000000000222, 1.000000000000000000, 1.000000000000000000, 1.000000000000000222, 0.9999999999999996669, 1.000000000000000444, 0.9999999999999997780, 0.9999999999999997780, 1.000000000000000000, 1.000000000000000000, 1.000000000000000000, 0.9999999999999996669, 1.000000000000000444, 1.000000000000000000, 1.000000000000000222, 1.000000000000000000, 0.9999999999999997780, 1.000000000000000222, 0.9999999999999997780, 1.000000000000000222, 1.000000000000000000, 1.000000000000000000, 1.000000000000000222, 1.000000000000000000, 1.000000000000000222, 0.9999999999999994449, 1.000000000000000444, 1.000000000000000000, 0.9999999999999996669, 1.000000000000000222, 0.9999999999999997780, 1.000000000000000222, 0.9999999999999997780, 1.000000000000000000, 1.000000000000000000, 1.000000000000000000, 1.000000000000000000, 1.000000000000000000, 1.000000000000000444, 1.000000000000000000, 1.000000000000000000, 1.000000000000000222, 1.000000000000000000, 1.000000000000000000, 0.9999999999999997780, 1.000000000000000000, 1.000000000000000222, 1.000000000000000000, 1.000000000000000222, 0.9999999999999997780, 1.000000000000000000, 0.9999999999999997780, 0.9999999999999997780, 1.000000000000000222, 0.9999999999999997780, 1.000000000000000444, 0.9999999999999997780, 1.000000000000000000, 1.000000000000000222, 1.000000000000000000, 1.000000000000000000, 0.9999999999999997780, 1.000000000000000222, 1.000000000000000000, 1.000000000000000000, 1.000000000000000000, 1.000000000000000222, 0.9999999999999996669, 1.000000000000000222, 1.000000000000000222, 0.9999999999999996669, 1.000000000000000444, 0.9999999999999996669, 1.000000000000000000, 1.000000000000000222, 0.9999999999999996669, 1.000000000000000222, 1.000000000000000000, 1.000000000000000222, 1.000000000000000000, 1.000000000000000222, 0.9999999999999997780, 1.000000000000000444, 0.9999999999999997780, 0.9999999999999997780, 1.000000000000000222, 0.9999999999999996669, 1.000000000000000222, 1.000000000000000000, 1.000000000000000000, 1.000000000000000000, 0.9999999999999997780, 1.000000000000000222, 1.000000000000000222, 0.9999999999999997780, 1.000000000000000222, 0.9999999999999997780, 1.000000000000000222, 1.000000000000000000, 1.000000000000000444, 1.000000000000000000, 1.000000000000000222, 0.9999999999999996669, 1.000000000000000444, 0.9999999999999993339, 1.000000000000000444, 0.9999999999999997780, 1.000000000000000444, 0.9999999999999997780, 1.000000000000000000, 1.000000000000000000, 0.9999999999999997780, 1.000000000000000222, 0.9999999999999997780, 0.9999999999999996669, 1.000000000000000444, 1.000000000000000222, 1.000000000000000000, 0.9999999999999997780, 1.000000000000000222, 0.9999999999999996669, 1.000000000000000222, 0.9999999999999997780, 1.000000000000000222, 1.000000000000000000, 1.000000000000000000, 1.000000000000000000, 1.000000000000000000, 0.9999999999999997780, 1.000000000000000000, 1.000000000000000000, 0.9999999999999997780, 1.000000000000000000, 1.000000000000000000, 1.000000000000000000, 1.000000000000000222, 1.000000000000000000, 1.000000000000000444, 1.000000000000000222, 1.000000000000000000, 1.000000000000000000, 0.9999999999999997780, 1.000000000000000222, 1.000000000000000000, 1.000000000000000000, 1.000000000000000000, 0.9999999999999997780, 1.000000000000000222, 0.9999999999999997780, 1.000000000000000222, 1.000000000000000444, 0.9999999999999997780, 1.000000000000000222, 1.000000000000000000, 1.000000000000000000, 1.000000000000000000, 0.9999999999999997780, 1.000000000000000444, 0.9999999999999997780, 1.000000000000000222, 0.9999999999999997780, 1.000000000000000222, 0.9999999999999994449, 1.000000000000000222, 1.000000000000000000, 1.000000000000000222, 1.000000000000000000, 0.9999999999999997780, 1.000000000000000222, 1.000000000000000000, 0.9999999999999997780, 1.000000000000000444, 0.9999999999999996669, 1.000000000000000222, 1.000000000000000000, 1.000000000000000000, 1.000000000000000222, 0.9999999999999997780, 0.9999999999999997780, 1.000000000000000444, 1.000000000000000222, 1.000000000000000000, 0.9999999999999997780, 0.9999999999999997780, 1.000000000000000222, 1.000000000000000000, 1.000000000000000222, 1.000000000000000000, 0.9999999999999997780, 1.000000000000000000, 1.000000000000000000, 1.000000000000000000, 1.000000000000000222, 0.9999999999999997780, 1.000000000000000222, 1.000000000000000000, 1.000000000000000000, 1.000000000000000000, 0.9999999999999997780, 1.000000000000000000, 1.000000000000000222, 1.000000000000000222, 0.9999999999999996669, 1.000000000000000444, 0.9999999999999996669, 1.000000000000000222, 1.000000000000000000, 1.000000000000000222, 0.9999999999999997780, 1.000000000000000444, 1.000000000000000000, 1.000000000000000444, 0.9999999999999994449, 1.000000000000000222, 0.9999999999999997780, 0.9999999999999997780, 1.000000000000000000, 1.000000000000000222, 1.000000000000000000, 1.000000000000000000, 1.000000000000000000, 1.000000000000000222, 0.9999999999999996669, 1.000000000000000222, 1.000000000000000000, 0.9999999999999996669, 1.000000000000000444, 1.000000000000000000, 1.000000000000000000, 1.000000000000000000, 0.9999999999999996669, 1.000000000000000222, 1.000000000000000000, 1.000000000000000000, 1.000000000000000222, 0.9999999999999997780, 0.9999999999999997780, 1.000000000000000000, 1.000000000000000000, 1.000000000000000222, 0.9999999999999997780, 1.000000000000000222, 1.000000000000000000, 1.000000000000000000, 0.9999999999999996669, 1.000000000000000222, 1.000000000000000000, 1.000000000000000222, 1.000000000000000000, 1.000000000000000000, 1.000000000000000000, 0.9999999999999997780, 1.000000000000000222, 0.9999999999999996669, 1.000000000000000444, 1.000000000000000000, 0.9999999999999997780, 1.000000000000000000, 1.000000000000000222, 1.000000000000000222, 0.9999999999999996669, 1.000000000000000000, 1.000000000000000000, 0.9999999999999997780, 1.000000000000000222, 1.000000000000000000, 1.000000000000000222, 0.9999999999999996669, 1.000000000000000444, 1.000000000000000000, 1.000000000000000000, 1.000000000000000000, 1.000000000000000222, 1.000000000000000000, 0.9999999999999997780, 1.000000000000000444, 1.000000000000000000, 1.000000000000000444, 0.9999999999999997780, 1.000000000000000444, 1.000000000000000000, 1.000000000000000222, 1.000000000000000222, 1.000000000000000000, 0.9999999999999996669, 1.000000000000000000, 1.000000000000000000, 1.000000000000000000, 1.000000000000000000, 1.000000000000000222, 0.9999999999999996669, 1.000000000000000000, 1.000000000000000222, 0.9999999999999997780, 0.9999999999999997780, 1.000000000000000000, 1.000000000000000000, 1.000000000000000000, 1.000000000000000000) ) ) 
 REPRESENTATION_ITEM ( '' )  SURFACE ( )  );
#4941 = CARTESIAN_POINT ( 'NONE',  ( 2.192262590105994668, -0.9421081357594159877, 1.995820444975453745 ) ) ;
#4942 = CARTESIAN_POINT ( 'NONE',  ( 4.235799883310053637, -1.556133899351975103, -1.642472060615452589 ) ) ;
#4943 = CARTESIAN_POINT ( 'NONE',  ( -6.887178846062116833, 9.058127958537705027, -1.443375672974059665 ) ) ;
#4944 = CARTESIAN_POINT ( 'NONE',  ( 3.796947700133224135, -0.1831754980210500150, -1.802320314001674806 ) ) ;
#4945 = CARTESIAN_POINT ( 'NONE',  ( 4.030425823177123057, 0.5166280748541264289, 1.844641390986961671 ) ) ;
#4946 = CARTESIAN_POINT ( 'NONE',  ( 0.6823417656249917140, 4.405208333674755394, 1.181850606188765695 ) ) ;
#4947 = CARTESIAN_POINT ( 'NONE',  ( 3.819176294577591779, -0.1464417209034867828, 1.966092509880690065 ) ) ;
#4948 = CARTESIAN_POINT ( 'NONE',  ( 0.6219390430294257088, -1.027834010343916749, -1.629101698904901863 ) ) ;
#4949 = CARTESIAN_POINT ( 'NONE',  ( 5.207814216083940018, -1.861544245658670604, 0.1842191830812092979 ) ) ;
#4950 = CARTESIAN_POINT ( 'NONE',  ( 3.159088808783340419, -1.747439373373047333, 1.507377025801335702 ) ) ;
#4951 = CARTESIAN_POINT ( 'NONE',  ( 4.351900876113290018, -0.7134228844126557778, 1.719084262507431182 ) ) ;
#4952 = CARTESIAN_POINT ( 'NONE',  ( 0.09916492693107491208, -9.920000000000095852, 9.499482423651659957 ) ) ;
#4953 = CLOSED_SHELL ( 'NONE', ( #198823, #171874, #825, #2469, #197741, #47697, #205413, #23197, #90561, #130667, #13106, #154164, #153476, #166301, #75225, #119571, #52703, #143729, #195068, #161161, #126757, #47786, #65725, #174690, #143847, #18503, #204388, #101033, #122550, #30052, #10413, #172137, #207688, #84503, #29165, #150410, #141036, #5117, #4819, #68995, #99839, #26329, #6086, #132105, #19712, #123390, #62771, #210940, #171934, #209739, #197319, #116928, #181368, #46215, #138304, #178206, #142040, #28362, #61359, #44869, #213826, #86494, #16855, #187300, #196987, #43023, #199535, #35756, #61310, #210611, #60406, #68147, #123510, #56246, #208109, #58868, #69918, #92443, #15911, #20778, #133964, #210996, #148626, #204370, #8727, #7986, #142207, #169369, #81246, #155525, #142497, #163536, #179890, #78945, #54584, #94614, #28852, #9276, #133817, #74015, #124376, #37654, #174784, #210032, #154511, #146239, #144646, #38233, #140053, #141252, #86624, #128257, #90630, #144786, #11620, #146903, #200229, #192889, #131589, #2324, #108393, #104607, #205436, #64327, #112460, #121265, #19638, #25767, #80358, #104194, #113853, #151358, #86956, #137, #119208, #195211, #118228, #156600, #210578, #154061, #27655, #175607, #29382, #41806, #20517, #94911, #108688, #143589, #118366, #107722, #173726, #111324, #31661, #61863, #198603, #35667, #134368, #190241, #104712, #11185, #40373, #193838, #205563, #120359, #105962, #189169, #134276, #10673, #57150, #172933, #49558, #23348, #13844, #89786, #197363, #159829 ) ) ;
#4954 = CARTESIAN_POINT ( 'NONE',  ( 11.01272219801454888, 3.870433085555837316, -3.737564583532788642 ) ) ;
#4956 = CARTESIAN_POINT ( 'NONE',  ( 1.823018060162405085, 1.965545597939293954, 0.7568914254860066304 ) ) ;
#4955 = CARTESIAN_POINT ( 'NONE',  ( -3.077337680177623103, 6.534051693608437184, 0.7216878364870317197 ) ) ;
#4957 = CARTESIAN_POINT ( 'NONE',  ( 2.833290915131624566, 6.249330467721451399, -0.7216878364870267237 ) ) ;
#4959 = CARTESIAN_POINT ( 'NONE',  ( 8.283668668269706714, 8.766627655843896250, 1.040834085586084257E-14 ) ) ;
#4958 = CARTESIAN_POINT ( 'NONE',  ( 0.6823417656249917140, 5.655208333674749177, 1.181850606188765695 ) ) ;
#4960 = CARTESIAN_POINT ( 'NONE',  ( 3.234745892528373634, 1.342314639517484087, -1.641720766639111817 ) ) ;
#4961 = FACE_OUTER_BOUND ( 'NONE', #116639, .T. ) ;
#4962 = CARTESIAN_POINT ( 'NONE',  ( 0.8088602503539430444, -0.4949860548154049189, -1.958043583812353550 ) ) ;
#4963 = CARTESIAN_POINT ( 'NONE',  ( 1.364683531249986537, 0.6135416670080880985, 0.7879004041258500513 ) ) ;
#4964 = CARTESIAN_POINT ( 'NONE',  ( -4.311129659465605002, 4.131998812239033647, 0.7216878364870317197 ) ) ;
#4965 = CARTESIAN_POINT ( 'NONE',  ( 4.822949958159288286, 6.649860922651058992, -1.599625672291256295 ) ) ;
#4966 = ORIENTED_EDGE ( 'NONE', *, *, #114112, .F. ) ;
#4967 = CARTESIAN_POINT ( 'NONE',  ( 2.495597164219889308, 1.669172397749154380, 1.373402732410613725 ) ) ;
#4968 = FACE_OUTER_BOUND ( 'NONE', #66297, .T. ) ;
#4971 = CARTESIAN_POINT ( 'NONE',  ( 3.307826292054301121, 4.882216645528547616, -1.443375672974057666 ) ) ;
#4970 = CARTESIAN_POINT ( 'NONE',  ( 6.825078400183592464, 1.263193418084729958, 2.069194724180785538 ) ) ;
#4969 = CARTESIAN_POINT ( 'NONE',  ( 3.739016502318667445, 7.584212696005614873, 0.7998128361456271485 ) ) ;
#4972 = DIRECTION ( 'NONE',  ( 1.276756478318932585E-15, -1.000000000000000000, 1.665334536937738262E-16 ) ) ;
#4973 = CARTESIAN_POINT ( 'NONE',  ( 6.069546051295945155, 1.394081536189460069, 1.457239770841619597 ) ) ;
#4974 = CARTESIAN_POINT ( 'NONE',  ( -7.537970219518066450, 11.73812298950569044, -0.7216878364870267237 ) ) ;
#4975 = CARTESIAN_POINT ( 'NONE',  ( 0.1170720436180875679, -0.1011795954627830590, 2.189343785608413917 ) ) ;
#4976 = DIRECTION ( 'NONE',  ( 0.000000000000000000, 1.000000000000000000, 0.000000000000000000 ) ) ;
#4978 = CARTESIAN_POINT ( 'NONE',  ( -1.364683531250010740, 12.13020833367473195, 0.7879004041258445001 ) ) ;
#4977 = CARTESIAN_POINT ( 'NONE',  ( 6.772347375734490527, -1.334533509509854943, 1.701269717329929820 ) ) ;
#4979 = CARTESIAN_POINT ( 'NONE',  ( -7.971304249830880373, 11.38727316052296601, 1.199719254218453823 ) ) ;
#4980 = B_SPLINE_CURVE_WITH_KNOTS ( 'NONE', 3,
 ( #104074, #204735, #20656, #38002, #186367, #205819, #87819 ),
 .UNSPECIFIED., .F., .F.,
 ( 4, 3, 4 ),
 ( 6.324901595874412133E-18, 3.303462137167311185E-05, 4.225156140141500603E-05 ),
 .UNSPECIFIED. ) ;
#4981 = CARTESIAN_POINT ( 'NONE',  ( -4.568734577680875653, 8.274014740695587733, -0.7216878364870257245 ) ) ;
#4982 = CARTESIAN_POINT ( 'NONE',  ( -0.6823417656250212460, 1.613541667008083769, 1.181850606188755259 ) ) ;
#4983 = LINE ( 'NONE', #107935, #196145 ) ;
#4984 = EDGE_CURVE ( 'NONE', #179126, #141384, #144052, .T. ) ;
#4985 = CARTESIAN_POINT ( 'NONE',  ( -1.402160292154681736E-14, 9.562499999999998224, 1.732050807568881190 ) ) ;
#4986 = CARTESIAN_POINT ( 'NONE',  ( 2.596001052779199014, -1.720239769356088688, -0.1272231981628013098 ) ) ;
#4987 = CARTESIAN_POINT ( 'NONE',  ( 4.746236293235721604, 7.694970221153795364, 1.199719254218451159 ) ) ;
#4988 = CARTESIAN_POINT ( 'NONE',  ( 1.932500037753889455, 0.1674293521093522530, 1.761778154814014119 ) ) ;
#4989 = CARTESIAN_POINT ( 'NONE',  ( 2.842442125518374496, 1.116481279481882805, -1.674925767759533723 ) ) ;
#4990 = CARTESIAN_POINT ( 'NONE',  ( 5.403435775159438847, 1.801252639416499379, 1.274624607731331905 ) ) ;
#4991 = ORIENTED_EDGE ( 'NONE', *, *, #160078, .T. ) ;
#4992 = CARTESIAN_POINT ( 'NONE',  ( 4.676038720085195166, 1.997217120926295442, -0.3003719491122060492 ) ) ;
#4993 = CARTESIAN_POINT ( 'NONE',  ( -5.749539660647037032, 8.865490816466966351, 1.199719254218454489 ) ) ;
#4995 = CARTESIAN_POINT ( 'NONE',  ( 3.497672881252233967, -1.986097994744703721, 0.3474890017408845955 ) ) ;
#4994 = CARTESIAN_POINT ( 'NONE',  ( 4.758503674095369007, 2.114844282287762667, 0.1552407789479764433 ) ) ;
#4997 = ORIENTED_EDGE ( 'NONE', *, *, #104111, .F. ) ;
#4996 = CARTESIAN_POINT ( 'NONE',  ( 4.552869461240817373, 0.3164949366275445208, 1.783561479213832346 ) ) ;
#4998 = CARTESIAN_POINT ( 'NONE',  ( 4.766573523656222555, 7.718696989977711809, 1.199719254218452047 ) ) ;
#4999 = EDGE_CURVE ( 'NONE', #50747, #93524, #187783, .T. ) ;
#5000 = ORIENTED_EDGE ( 'NONE', *, *, #203502, .F. ) ;
#5001 = CARTESIAN_POINT ( 'NONE',  ( 0.9537216069140028729, 1.868711056098860235, -0.08788249432020722729 ) ) ;
#5002 = EDGE_CURVE ( 'NONE', #213175, #71915, #22342, .T. ) ;
#5003 = AXIS2_PLACEMENT_3D ( 'NONE', #41374, #207035, #158314 ) ;
#5004 = CARTESIAN_POINT ( 'NONE',  ( -10.91927143613604301, -9.998067526917992609, 0.1131244342389375046 ) ) ;
#5005 = CARTESIAN_POINT ( 'NONE',  ( 5.936161223257452768, -1.012099431654609472, -1.502142840615662944 ) ) ;
#5006 = DIRECTION ( 'NONE',  ( -0.000000000000000000, -1.000000000000000000, -0.000000000000000000 ) ) ;
#5007 = CARTESIAN_POINT ( 'NONE',  ( -11.27976636440881641, 5.060096319113082330, -5.788224378391188196 ) ) ;
#5008 = DIRECTION ( 'NONE',  ( 0.3085202182251676195, 0.000000000000000000, -0.9512177852344304574 ) ) ;
#5009 = AXIS2_PLACEMENT_3D ( 'NONE', #84193, #213107, #67910 ) ;
#5010 = CARTESIAN_POINT ( 'NONE',  ( 0.6823417656249882723, 2.988541667008084879, -1.181850606188754593 ) ) ;
#5011 = FACE_OUTER_BOUND ( 'NONE', #54886, .T. ) ;
#5012 = B_SPLINE_CURVE_WITH_KNOTS ( 'NONE', 3,
 ( #205696, #87693, #55201, #187322, #71419 ),
 .UNSPECIFIED., .F., .F.,
 ( 4, 1, 4 ),
 ( 0.003096135707997031087, 0.003151720136792417887, 0.003207304565587804253 ),
 .UNSPECIFIED. ) ;
#5013 = CARTESIAN_POINT ( 'NONE',  ( 7.051649292883499953, 7.399548061218447437, -0.7216878364870317197 ) ) ;
#5014 = CARTESIAN_POINT ( 'NONE',  ( 1.557006721180295150, 1.605793932651664813, -1.126831546849601740 ) ) ;
#5015 = CARTESIAN_POINT ( 'NONE',  ( -3.689227196694341515, 7.318199139536432973, -0.7216878364870458196 ) ) ;
#5016 = CARTESIAN_POINT ( 'NONE',  ( -5.315678745009726924, 8.359319748223434487, -1.199719254218453823 ) ) ;
#5017 = CARTESIAN_POINT ( 'NONE',  ( 4.113620189327307664, 1.705085180707970771, 1.260635662952174663 ) ) ;
#5019 = FILL_AREA_STYLE ('',( #166486 ) ) ;
#5018 = CARTESIAN_POINT ( 'NONE',  ( -5.800227658267527175, 5.731630120925694349, -0.5022995730114099278 ) ) ;
#5020 = CARTESIAN_POINT ( 'NONE',  ( 5.870382883074816149, -1.252475921811508019, 1.522319303672705848 ) ) ;
#5021 = CARTESIAN_POINT ( 'NONE',  ( -1.201851678989727383E-14, 1.071875000341418138, 1.575800808251672791 ) ) ;
#5022 = CARTESIAN_POINT ( 'NONE',  ( 0.9318904303841836212, -1.963229875443720074, 0.4450799344311164862 ) ) ;
#5023 = EDGE_LOOP ( 'NONE', ( #156828, #125984, #201892, #90334 ) ) ;
#5024 = CARTESIAN_POINT ( 'NONE',  ( 0.7732552308061869661, 1.865071980587120315, -1.002124039132473055 ) ) ;
#5025 = CARTESIAN_POINT ( 'NONE',  ( 11.99989096720821991, 6.571554264009413338, 0.5037914602360314964 ) ) ;
#5026 = CARTESIAN_POINT ( 'NONE',  ( 2.365759603224312446, -0.4558734232973959966, 2.019384234097781228 ) ) ;
#5027 = CARTESIAN_POINT ( 'NONE',  ( 4.716257332707354699, 6.595662536282280719, -1.599625672291269396 ) ) ;
#5028 = CARTESIAN_POINT ( 'NONE',  ( 4.712340909201580885, 7.655425606447271214, -1.199719254218452047 ) ) ;
#5029 = ORIENTED_EDGE ( 'NONE', *, *, #163609, .T. ) ;
#5031 = CARTESIAN_POINT ( 'NONE',  ( 3.994848817520957773, 7.812407387083109001, 1.040834085586084257E-14 ) ) ;
#5030 = CARTESIAN_POINT ( 'NONE',  ( 5.261704619121490900, 1.029696775897260830, 1.819396322279245304 ) ) ;
#5034 = ORIENTED_EDGE ( 'NONE', *, *, #97813, .T. ) ;
#5033 = CARTESIAN_POINT ( 'NONE',  ( 1.471055694106305101, -1.553634009935511484, -0.9311844293155254748 ) ) ;
#5032 = CARTESIAN_POINT ( 'NONE',  ( 3.451995160207482538, 1.825762228170943136, 0.001041782061617091849 ) ) ;
#5035 = CARTESIAN_POINT ( 'NONE',  ( 6.287735281038357549, 1.518688880046001444, 1.601449620450722700 ) ) ;
#5036 = CARTESIAN_POINT ( 'NONE',  ( 6.827182134110222123, -0.006956174471953178659, 2.188967759425272330 ) ) ;
#5037 = CARTESIAN_POINT ( 'NONE',  ( 4.331241739176756589, 0.1049304944579672605, 2.204394592675275710 ) ) ;
#5038 = CARTESIAN_POINT ( 'NONE',  ( -1.364683531250010740, 9.692708333674737275, 0.7879004041258445001 ) ) ;
#5039 = ORIENTED_EDGE ( 'NONE', *, *, #19138, .T. ) ;
#5040 = CARTESIAN_POINT ( 'NONE',  ( 3.176317266091326807, 0.8619891151622931513, 1.707069686517001195 ) ) ;
#5041 = CARTESIAN_POINT ( 'NONE',  ( -3.623053363349869382, 5.249981562040033189, 1.599625672291267398 ) ) ;
#5042 = CARTESIAN_POINT ( 'NONE',  ( 7.639129486296027061, 10.99973593639901814, 1.199719254218460707 ) ) ;
#5043 = CARTESIAN_POINT ( 'NONE',  ( 6.039524589772497620, 1.914416561877980261, -0.7887839105886890190 ) ) ;
#5044 = STYLED_ITEM ( 'NONE', ( #7200 ), #90432 ) ;
#5045 = CARTESIAN_POINT ( 'NONE',  ( -9.345718720454772921, 15.44302540324981976, 7.452154232107743859 ) ) ;
#5046 = CARTESIAN_POINT ( 'NONE',  ( 5.759372899636661991, 2.159370146098410714, -0.3733810082120898044 ) ) ;
#5047 = DIRECTION ( 'NONE',  ( -1.276756478318932585E-15, 1.000000000000000000, -1.665334536937738262E-16 ) ) ;
#5048 = CARTESIAN_POINT ( 'NONE',  ( -8.771960149507961546, 15.44694760938148548, -8.173204598701103052 ) ) ;
#5049 = DIRECTION ( 'NONE',  ( -5.551115123125766062E-17, 0.000000000000000000, 1.000000000000000000 ) ) ;
#5050 = CARTESIAN_POINT ( 'NONE',  ( 3.848780967690919930, -1.530814235938406709, 1.074699354247290017 ) ) ;
#5051 = CARTESIAN_POINT ( 'NONE',  ( 1.642778471875000035, -1.013541666188708223, -2.845375778867859751 ) ) ;
#5052 = CARTESIAN_POINT ( 'NONE',  ( 4.258669648468303315, 7.982548666606043675, 0.7216878364870509266 ) ) ;
#5054 = CARTESIAN_POINT ( 'NONE',  ( -6.399085315970132193, 10.40942393536641397, -0.7216878364870278340 ) ) ;
#5053 = AXIS2_PLACEMENT_3D ( 'NONE', #95542, #28374, #127032 ) ;
#5055 = CARTESIAN_POINT ( 'NONE',  ( 4.736594563127852098, 6.619389305106191834, -1.599625672291273171 ) ) ;
#5056 = CARTESIAN_POINT ( 'NONE',  ( 0.5495732465782035003, 1.455460699200894270, 1.326940832280040450 ) ) ;
#5057 = CARTESIAN_POINT ( 'NONE',  ( 0.7379079170338509464, 2.013986002441462198, -0.1017714793793283723 ) ) ;
#5058 = CARTESIAN_POINT ( 'NONE',  ( -9.459838494033043332, 12.05956421450382088, 1.599625672291281386 ) ) ;
#5059 = CARTESIAN_POINT ( 'NONE',  ( 7.506374323821472849, 8.786466794993730289, -1.199719254218452047 ) ) ;
#5060 = DIRECTION ( 'NONE',  ( -1.224646799147353207E-16, 0.000000000000000000, 1.000000000000000000 ) ) ;
#5061 = CARTESIAN_POINT ( 'NONE',  ( 1.605704095283020605, -2.174604996184846595, 0.2706701637196773369 ) ) ;
#5062 = CARTESIAN_POINT ( 'NONE',  ( 5.760330229460346452, 0.7440287100829170441, 1.667389206893993725 ) ) ;
#5063 = CARTESIAN_POINT ( 'NONE',  ( -4.135400547368138113, 4.783387712472935149, 1.199719254218462483 ) ) ;
#5064 = CARTESIAN_POINT ( 'NONE',  ( 6.102578539926878598, 7.252668063737060855, -1.082531754730548412 ) ) ;
#5066 = EDGE_CURVE ( 'NONE', #139477, #45585, #136576, .T. ) ;
#5065 = CARTESIAN_POINT ( 'NONE',  ( 8.550388431712704573, 13.12720360364021133, 0.000000000000000000 ) ) ;
#5067 = CARTESIAN_POINT ( 'NONE',  ( 5.203632029546647608, 4.965325544092860532, 1.040834085586084257E-14 ) ) ;
#5068 = CARTESIAN_POINT ( 'NONE',  ( 4.065465959251388206, 5.836405933916976707, -1.599625672291269396 ) ) ;
#5069 = ORIENTED_EDGE ( 'NONE', *, *, #8140, .T. ) ;
#5071 = CARTESIAN_POINT ( 'NONE',  ( 0.2232913631893228001, 1.752491241892171647, 0.9904617665423065542 ) ) ;
#5070 = CARTESIAN_POINT ( 'NONE',  ( 4.054132754448328768, -1.361571661076573792, 1.239656203754435193 ) ) ;
#5072 = CARTESIAN_POINT ( 'NONE',  ( 1.704906730629534684, -1.665072001576539007, -1.584524786048894240 ) ) ;
#5074 = CARTESIAN_POINT ( 'NONE',  ( 0.3735836145450521228, -1.826584228078181660, 0.3550381321636967846 ) ) ;
#5073 = CARTESIAN_POINT ( 'NONE',  ( 4.528060117284244512, 4.385084346360807572, 0.7216878364870317197 ) ) ;
#5075 = CARTESIAN_POINT ( 'NONE',  ( -3.581325132304157943, 7.329963087663487364, -0.7998128361456281477 ) ) ;
#5076 = CARTESIAN_POINT ( 'NONE',  ( -1.992711204631002198E-15, 2.999999999999989342, 1.224999999999989875 ) ) ;
#5077 = CARTESIAN_POINT ( 'NONE',  ( 4.078302138561982204, 0.9061299177482335931, 1.684124486321957104 ) ) ;
#5078 = CARTESIAN_POINT ( 'NONE',  ( -8.622095623286845978, 12.14652976288826913, 1.199719254218462483 ) ) ;
#5079 = CARTESIAN_POINT ( 'NONE',  ( 5.925280661667059690, 7.134359284303951831, -1.114000666120490868 ) ) ;
#5080 = CARTESIAN_POINT ( 'NONE',  ( -5.790741006812557323, 9.769965251341050205, 0.000000000000000000 ) ) ;
#5082 = CARTESIAN_POINT ( 'NONE',  ( 0.9713206009373563932, 1.803875226702996049, -0.4951341686536685494 ) ) ;
#5081 = CARTESIAN_POINT ( 'NONE',  ( 2.437156881564545685, -1.551092155746801815, -1.402114238623404896 ) ) ;
#5083 = CARTESIAN_POINT ( 'NONE',  ( 2.425157474508771838, 0.8594973679685766754, 1.823840639232063854 ) ) ;
#5084 = CARTESIAN_POINT ( 'NONE',  ( 9.246297574839983824, 9.889694713509232571, 0.7216878364870438212 ) ) ;
#5085 = CARTESIAN_POINT ( 'NONE',  ( -1.364683531249997417, 3.571875000341423245, 1.214306433183764966E-14 ) ) ;
#5086 = CARTESIAN_POINT ( 'NONE',  ( 2.753125985903591477, 1.731854804227653366, -0.1727350219371779905 ) ) ;
#5087 = CARTESIAN_POINT ( 'NONE',  ( 5.820528018968444961, 5.685037531751635953, 0.7998128361456341429 ) ) ;
#5089 = CARTESIAN_POINT ( 'NONE',  ( 0.3993783336448741283, 2.892526381812567493, -2.025045271722654583 ) ) ;
#5088 = DIRECTION ( 'NONE',  ( -0.000000000000000000, 1.000000000000000000, 0.000000000000000000 ) ) ;
#5090 = CARTESIAN_POINT ( 'NONE',  ( 3.685938805993322909, -0.8483273805379875077, 1.501759545097125059 ) ) ;
#5091 = CARTESIAN_POINT ( 'NONE',  ( 3.439196427729715566, -1.660734982795486481, -1.430121640581414111 ) ) ;
#5092 = CARTESIAN_POINT ( 'NONE',  ( 6.481111342790009999, -0.1036386110354891726, -2.204582208980155222 ) ) ;
#5093 = CARTESIAN_POINT ( 'NONE',  ( 6.983263157960362122, 6.035089925019382129, 2.648702789725385198 ) ) ;
#5094 = CARTESIAN_POINT ( 'NONE',  ( 3.766621525425926098, -0.8750874339106663458, -1.987059052243181689 ) ) ;
#5095 = CARTESIAN_POINT ( 'NONE',  ( 1.734698295210383767, 0.1775668987445792879, 1.817036636966688823 ) ) ;
#5096 = DIRECTION ( 'NONE',  ( 1.000000000000000000, 0.000000000000000000, 0.000000000000000000 ) ) ;
#5097 = CARTESIAN_POINT ( 'NONE',  ( 4.364542673910889015, -2.054697287276555873, -0.5108639600793271063 ) ) ;
#5098 = VERTEX_POINT ( 'NONE', #149389 ) ;
#5100 = CARTESIAN_POINT ( 'NONE',  ( -1.402160292154681736E-14, 2.259375000341416140, -1.575800808251660134 ) ) ;
#5099 = CARTESIAN_POINT ( 'NONE',  ( 5.302359097629713247, 1.737542498810572322, -1.495360377712177113 ) ) ;
#5101 = CARTESIAN_POINT ( 'NONE',  ( 6.620655732516672387, 6.040129668214249570, 2.321170174800915031 ) ) ;
#5102 = CARTESIAN_POINT ( 'NONE',  ( 2.205172540517054802, 5.724451730578533848, 1.040834085586084257E-14 ) ) ;
#5103 = CARTESIAN_POINT ( 'NONE',  ( 0.5926325054007793858, -1.174586488569592690, 1.765252418913294319 ) ) ;
#5104 = CARTESIAN_POINT ( 'NONE',  ( -4.934804725694231564, 5.819988937140460727, -1.082531754730544860 ) ) ;
#5105 = DIRECTION ( 'NONE',  ( 0.7592566023653005702, 0.6507913734559639396, 0.000000000000000000 ) ) ;
#5106 = AXIS2_PLACEMENT_3D ( 'NONE', #189443, #41086, #77818 ) ;
#5107 = CARTESIAN_POINT ( 'NONE',  ( -4.067082893975237035, 7.688754443039000464, 1.040834085586084257E-14 ) ) ;
#5108 = CARTESIAN_POINT ( 'NONE',  ( -10.99953061226852746, -9.919996481109292219, 0.1022074249660880618 ) ) ;
#5109 = ORIENTED_EDGE ( 'NONE', *, *, #29662, .T. ) ;
#5110 = CARTESIAN_POINT ( 'NONE',  ( 4.922500090287251773, -1.427935867408920645, -1.423962988533589158 ) ) ;
#5112 = CARTESIAN_POINT ( 'NONE',  ( 3.239185349552040183, -0.1472093337855179818, -2.057344904835652688 ) ) ;
#5111 = CARTESIAN_POINT ( 'NONE',  ( 4.137209430464448445, 7.978494768850520558, 1.040834085586084257E-14 ) ) ;
#5114 = CARTESIAN_POINT ( 'NONE',  ( -0.1411974294641837879, -0.0004739540254219963859, -1.900147702309516795 ) ) ;
#5113 = CARTESIAN_POINT ( 'NONE',  ( 6.180537922983273091, 8.303989891604203422, -1.599625672291281386 ) ) ;
#5115 = CARTESIAN_POINT ( 'NONE',  ( 7.700104897918568447, 7.948153567185284096, 0.000000000000000000 ) ) ;
#5117 = ADVANCED_FACE ( 'NONE', ( #213302 ), #31385, .F. ) ;
#5116 = CARTESIAN_POINT ( 'NONE',  ( 1.001543065824772753E-15, -2.121874999522043836, 3.793834371823811669 ) ) ;
#5118 =( LENGTH_UNIT ( ) NAMED_UNIT ( * ) SI_UNIT ( .MILLI., .METRE. ) );
#5119 = CARTESIAN_POINT ( 'NONE',  ( 6.615165563918417924, -2.126712762998611783, 0.5283135293715838232 ) ) ;
#5120 = CARTESIAN_POINT ( 'NONE',  ( 4.166638809851969327, 1.319227567334404494, 1.525044649537968589 ) ) ;
#5121 = CARTESIAN_POINT ( 'NONE',  ( 3.790429961727882713, 1.553415782126759792, -0.9881970032953185656 ) ) ;
#5122 = EDGE_CURVE ( 'NONE', #118628, #193157, #4309, .T. ) ;
#5123 = CARTESIAN_POINT ( 'NONE',  ( 5.494078562035752178, 7.432844293840273231, -1.599625672291262513 ) ) ;
#5124 =( NAMED_UNIT ( * ) PLANE_ANGLE_UNIT ( ) SI_UNIT ( $, .RADIAN. ) );
#5125 = CARTESIAN_POINT ( 'NONE',  ( 1.078623681775535914, -0.03615993657634165859, -1.724571457899269911 ) ) ;
#5126 = CARTESIAN_POINT ( 'NONE',  ( -2.117044542028253318, 5.621635732341564662, -0.7998128361456281477 ) ) ;
#5127 = CARTESIAN_POINT ( 'NONE',  ( 0.8624555810839064085, -0.06381188527813246025, -2.297968782114163222 ) ) ;
#5128 = CARTESIAN_POINT ( 'NONE',  ( -5.117312914154178216, 8.057616602233474978, -1.199719254218452047 ) ) ;
#5129 = CARTESIAN_POINT ( 'NONE',  ( 0.4041009963523278237, -0.6015683965250936405, 2.180870993196832419 ) ) ;
#5130 = CARTESIAN_POINT ( 'NONE',  ( 2.649164382713434573, -1.750592827090621917, 1.170555837024005008 ) ) ;
#5131 = CARTESIAN_POINT ( 'NONE',  ( -5.659602779061863487, 5.567567761852417085, 0.7998128361456281477 ) ) ;
#5132 = CARTESIAN_POINT ( 'NONE',  ( 5.777746017718023097, 9.892454120646377191, 0.7998128361456462443 ) ) ;
#5133 = CARTESIAN_POINT ( 'NONE',  ( 4.855228407025239612, 8.678533884922511987, 0.000000000000000000 ) ) ;
#5134 = CARTESIAN_POINT ( 'NONE',  ( -7.335124800193271177, 8.516399340768996851, -1.199719254218452935 ) ) ;
#5135 = CARTESIAN_POINT ( 'NONE',  ( 6.765155463094759014, 7.955398130774449683, 1.082531754730558626 ) ) ;
#5136 = CARTESIAN_POINT ( 'NONE',  ( 4.765179230921094522, 7.000095391635957398, 1.399907146243694722 ) ) ;
#5137 = CARTESIAN_POINT ( 'NONE',  ( -4.249591082879585535, 7.045274465746411252, 1.199719254218464037 ) ) ;
#5138 = CARTESIAN_POINT ( 'NONE',  ( 3.709420277874009297, 1.875127481890274561, -1.190789481685197604 ) ) ;
#5139 = CARTESIAN_POINT ( 'NONE',  ( 2.379091696419192381, 2.003018898301941686, -0.8894332929959417600 ) ) ;
#5140 = CARTESIAN_POINT ( 'NONE',  ( -6.226218857173722476, 8.287007971501239467, 1.599625672291283607 ) ) ;
#5141 = EDGE_CURVE ( 'NONE', #176704, #206450, #9819, .T. ) ;
#5142 = CARTESIAN_POINT ( 'NONE',  ( -5.646044625448194410, 5.551749915969804938, 0.000000000000000000 ) ) ;
#5143 = CARTESIAN_POINT ( 'NONE',  ( 5.547302793442128177, 1.730978599593002043, -0.9233319674036490898 ) ) ;
#5144 = CARTESIAN_POINT ( 'NONE',  ( 1.364683531249988535, 1.613541667008084879, 0.7879004041258500513 ) ) ;
#5145 = CARTESIAN_POINT ( 'NONE',  ( 6.610000000000006537, 7.629137130509094256, 2.600000000000001421 ) ) ;
#5146 = CARTESIAN_POINT ( 'NONE',  ( -4.555176424511596878, 7.297827681030051750, 1.082531754730560403 ) ) ;
#5147 = CARTESIAN_POINT ( 'NONE',  ( 4.957343421279006179, -1.817532610912236724, 1.092287347377165485 ) ) ;
#5148 = CARTESIAN_POINT ( 'NONE',  ( -3.474632506852224356, 7.275764701294714420, -0.7998128361456481317 ) ) ;
#5149 = ORIENTED_EDGE ( 'NONE', *, *, #164009, .T. ) ;
#5151 = CARTESIAN_POINT ( 'NONE',  ( 5.331013795412237855, 0.1550192300789655642, 2.156197635354038411 ) ) ;
#5150 = CARTESIAN_POINT ( 'NONE',  ( -6.346625304972878467, 7.537389289624049304, 1.082531754730548412 ) ) ;
#5152 = CARTESIAN_POINT ( 'NONE',  ( 6.830610463186557624, 6.863467050006115677, 1.040834085586084257E-14 ) ) ;
#5153 = CARTESIAN_POINT ( 'NONE',  ( 5.284640796330933199, 1.621094592300664106, -0.8731043043393661440 ) ) ;
#5154 = UNCERTAINTY_MEASURE_WITH_UNIT (LENGTH_MEASURE( 1.000000000000000082E-05 ), #1434, 'distance_accuracy_value', 'NONE');
#5155 = CARTESIAN_POINT ( 'NONE',  ( -5.911504460181634002, 6.000493611234613667, 0.05175081109743372154 ) ) ;
#5156 = CARTESIAN_POINT ( 'NONE',  ( 1.364683531249988535, 1.926041667008086211, 0.7879004041258500513 ) ) ;
#5157 = CARTESIAN_POINT ( 'NONE',  ( 6.369106938980155341, 1.663098657370492672, -0.5127371055620026929 ) ) ;
#5158 = DIRECTION ( 'NONE',  ( -5.578564026256490882E-16, -1.000000000000000000, -9.066213480720158442E-32 ) ) ;
#5159 = CARTESIAN_POINT ( 'NONE',  ( -0.4963857527936129665, 7.354535952643655783, 1.939768365030048125 ) ) ;
#5160 = CARTESIAN_POINT ( 'NONE',  ( -0.3282377607281405374, 1.801335450315361131, 1.224999999999994982 ) ) ;
#5161 = EDGE_CURVE ( 'NONE', #214101, #184826, #67037, .T. ) ;
#5162 = CARTESIAN_POINT ( 'NONE',  ( 3.731458613173586514, -1.998165266068991253, 0.8252760040215676440 ) ) ;
#5163 = AXIS2_PLACEMENT_3D ( 'NONE', #101028, #113373, #44052 ) ;
#5164 = CARTESIAN_POINT ( 'NONE',  ( -5.610376637956639101, 5.439860920571172542, 0.000000000000000000 ) ) ;
#5165 = EDGE_CURVE ( 'NONE', #213528, #98728, #14689, .T. ) ;
#5166 = CARTESIAN_POINT ( 'NONE',  ( -7.985389288324710400, 8.418635045908049008, -0.7216878364870267237 ) ) ;
#5167 = CARTESIAN_POINT ( 'NONE',  ( 3.520547545725543515, 1.372905562624787024, -1.669742455111824286 ) ) ;
#5168 = CARTESIAN_POINT ( 'NONE',  ( 4.798096821016461178, -1.970857504970180862, -0.05141287852120436652 ) ) ;
#5169 = CARTESIAN_POINT ( 'NONE',  ( 3.848775019297555389, -0.8554209813324518130, 1.508043379464953260 ) ) ;
#5170 = CIRCLE ( 'NONE', #77857, 9.636568542494918788 ) ;
#5171 = CARTESIAN_POINT ( 'NONE',  ( 0.3631484714031462668, 0.2087870660046411420, -2.181583536649676525 ) ) ;
#5172 = CARTESIAN_POINT ( 'NONE',  ( 2.661487998672926292, -2.007448288467659214, -1.137923995292255741 ) ) ;
#5173 = CARTESIAN_POINT ( 'NONE',  ( 3.286453515990275243, -2.029689310919643219, -0.3557144749045982879 ) ) ;
#5174 = CARTESIAN_POINT ( 'NONE',  ( 5.917518263527802524, -1.082453682572570797, -1.612232301441741233 ) ) ;
#5175 = CARTESIAN_POINT ( 'NONE',  ( -7.171900071504729191, 11.31104115015678779, -0.7216878364870267237 ) ) ;
#5176 = CARTESIAN_POINT ( 'NONE',  ( -4.444040490229335560, 8.406740681901359480, 0.7998128361456352531 ) ) ;
#5177 = CYLINDRICAL_SURFACE ( 'NONE', #54262, 9.999999999999998224 ) ;
#5178 = CARTESIAN_POINT ( 'NONE',  ( 0.3868239129443627466, 2.972657967446813654, -11.65375889120575792 ) ) ;
#5179 = CARTESIAN_POINT ( 'NONE',  ( -6.277061933002790362, 8.346324893301817482, 1.443375672974078761 ) ) ;
#5180 = CARTESIAN_POINT ( 'NONE',  ( 3.575398329460587554, 0.05639400328332971890, -2.206221599391814170 ) ) ;
#5181 = CARTESIAN_POINT ( 'NONE',  ( 3.285556943749998737, -2.792708332855373676, -1.896917185911906500 ) ) ;
#5182 = ORIENTED_EDGE ( 'NONE', *, *, #52572, .T. ) ;
#5183 = CARTESIAN_POINT ( 'NONE',  ( 0.9712807694385624524, -0.2802886605943204490, 1.839611564956656453 ) ) ;
#5184 = CARTESIAN_POINT ( 'NONE',  ( -0.1290005225502675879, 2.860092606084875033, -2.662085506130333457 ) ) ;
#5185 = CARTESIAN_POINT ( 'NONE',  ( -0.7500000000000215383, 5.222916667349482012, 1.299038105676671107 ) ) ;
#5186 = PRESENTATION_STYLE_ASSIGNMENT (( #8411 ) ) ;
#5188 = CARTESIAN_POINT ( 'NONE',  ( 6.825078400183574701, 2.043583509370741069, 2.350167621585138367 ) ) ;
#5187 = CARTESIAN_POINT ( 'NONE',  ( -6.586110727467836767, 6.776993156853382771, -0.3129968654442937814 ) ) ;
#5189 = CARTESIAN_POINT ( 'NONE',  ( 6.580030785786400216, -1.806642183828395920, -0.3538341520857649081 ) ) ;
#5190 = ORIENTED_EDGE ( 'NONE', *, *, #154855, .F. ) ;
#5191 = CARTESIAN_POINT ( 'NONE',  ( 3.362233863015654300, 0.9250742651227459312, 1.841665905919416035 ) ) ;
#5192 = CARTESIAN_POINT ( 'NONE',  ( -1.360316468750046859, 0.6197916670081009549, -0.7853790794159322131 ) ) ;
#5193 = CARTESIAN_POINT ( 'NONE',  ( -4.394814349124112951, 8.279033840620114049, -0.7998128361456281477 ) ) ;
#5194 = FACE_BOUND ( 'NONE', #61549, .T. ) ;
#5195 =( NAMED_UNIT ( * ) SI_UNIT ( $, .STERADIAN. ) SOLID_ANGLE_UNIT ( ) );
#5196 = CARTESIAN_POINT ( 'NONE',  ( 4.708759422647839976, 4.387974169377582001, -0.7998128361456211532 ) ) ;
#5197 = CARTESIAN_POINT ( 'NONE',  ( 1.428666007085793277, 1.985871523383303749, 0.5506756191897729247 ) ) ;
#5199 = CARTESIAN_POINT ( 'NONE',  ( 1.364683531249996529, 12.71354166700806232, 0.7879004041258405033 ) ) ;
#5198 = CARTESIAN_POINT ( 'NONE',  ( 3.834746474454188013E-15, 12.56250000000000178, 1.500000000000001554 ) ) ;
#5200 = CARTESIAN_POINT ( 'NONE',  ( 5.849453209292126310, 8.911780279894442103, 1.199719254218462483 ) ) ;
#5201 = SURFACE_STYLE_FILL_AREA ( #185033 ) ;
#5202 = EDGE_CURVE ( 'NONE', #60255, #183115, #50764, .T. ) ;
#5203 = CIRCLE ( 'NONE', #147041, 12.00000000000000178 ) ;
#5204 = CARTESIAN_POINT ( 'NONE',  ( 5.479209177496175087, -0.05098606815037013545, -2.206463706674952618 ) ) ;
#5205 = CARTESIAN_POINT ( 'NONE',  ( 0.6323695665565836066, 1.111747700424435159, -1.853661729306683936 ) ) ;
#5206 = CARTESIAN_POINT ( 'NONE',  ( -3.958617665510266725, 7.562211676496538360, -0.7216878364870267237 ) ) ;
#5207 = CARTESIAN_POINT ( 'NONE',  ( 0.2511858651975951151, 0.1928294586405615574, -2.007256720055437871 ) ) ;
#5208 = CARTESIAN_POINT ( 'NONE',  ( -0.4365953560983779069, -5.836144560139977955, -10.35465518852990385 ) ) ;
#5209 = CARTESIAN_POINT ( 'NONE',  ( 1.899821779672239419, 8.994870868756308369, -0.7749999999999996891 ) ) ;
#5210 = CARTESIAN_POINT ( 'NONE',  ( 2.360033908006432757, 0.7977434165707707470, 1.692156362554583460 ) ) ;
#5211 = MECHANICAL_DESIGN_GEOMETRIC_PRESENTATION_REPRESENTATION (  '', ( #64005 ), #147052 ) ;
#5212 = CARTESIAN_POINT ( 'NONE',  ( 3.134000194803722383, 2.016708403948695771, -0.004836970814638129855 ) ) ;
#5214 = CARTESIAN_POINT ( 'NONE',  ( 2.280903940472752467, 5.594607745005274246, -0.6109567437776646237 ) ) ;
#5213 = CARTESIAN_POINT ( 'NONE',  ( -1.364683531250014514, 0.7385416670080887647, -0.7879004041258289570 ) ) ;
#5216 = CARTESIAN_POINT ( 'NONE',  ( 5.092451870646586443, -2.090052423365583500, -0.2586305528886819194 ) ) ;
#5215 = CARTESIAN_POINT ( 'NONE',  ( -7.330154606482786050, 11.70359747420527619, 0.000000000000000000 ) ) ;
#5217 = CARTESIAN_POINT ( 'NONE',  ( 7.202405917357655341, 9.425892875049191488, 1.599625672291281386 ) ) ;
#5219 = CARTESIAN_POINT ( 'NONE',  ( -8.552495972122143186, 8.872333477097637200, 0.7998128361456462443 ) ) ;
#5218 = CARTESIAN_POINT ( 'NONE',  ( 5.574337433874081427, 6.532423756721743580, -1.199719254218452047 ) ) ;
#5220 = CARTESIAN_POINT ( 'NONE',  ( 0.5773502691896124084, -2.500000000000002220, -0.9999999999999991118 ) ) ;
#5221 = CARTESIAN_POINT ( 'NONE',  ( 4.043226763451240657, 0.1031935428237283348, 2.017299519520795670 ) ) ;
#5222 = CARTESIAN_POINT ( 'NONE',  ( -1.364683531249997417, 4.509375000341424133, 1.214306433183764966E-14 ) ) ;
#5223 = AXIS2_PLACEMENT_3D ( 'NONE', #188377, #207821, #58390 ) ;
#5224 = CARTESIAN_POINT ( 'NONE',  ( 6.760222218534770455, -2.062298699534569124, 0.04672293413533928907 ) ) ;
#5225 = CARTESIAN_POINT ( 'NONE',  ( 9.083599731475988648, 10.66024977721925104, 1.082531754730549967 ) ) ;
#5226 = CARTESIAN_POINT ( 'NONE',  ( 5.255217470067075070, -1.823004960263453489, -1.161262906855420329 ) ) ;
#5227 = CARTESIAN_POINT ( 'NONE',  ( 5.580062740476173566, 8.667767742934335828, 1.199719254218451159 ) ) ;
#5228 = CARTESIAN_POINT ( 'NONE',  ( -1.402160292154681736E-14, -0.6156249996585817508, 1.575800808251672791 ) ) ;
#5229 = CARTESIAN_POINT ( 'NONE',  ( 5.559725510055676168, 8.644040974110419384, 1.199719254218451159 ) ) ;
#5230 = CARTESIAN_POINT ( 'NONE',  ( 8.744645890689993095, 9.304434415334227992, -0.7216878364870197293 ) ) ;
#5232 = DIRECTION ( 'NONE',  ( 0.000000000000000000, -1.000000000000000000, 0.000000000000000000 ) ) ;
#5231 = CARTESIAN_POINT ( 'NONE',  ( 2.928372970691155430, 1.159507463759208878, 1.835456099276617570 ) ) ;
#5234 = CARTESIAN_POINT ( 'NONE',  ( 2.032514702046281485, -1.644074058028240692, 0.8291662819630771786 ) ) ;
#5233 = CARTESIAN_POINT ( 'NONE',  ( -4.880572111239580124, 7.677455982212699759, 1.082531754730560403 ) ) ;
#5235 = CARTESIAN_POINT ( 'NONE',  ( -1.364683531250012516, 2.988541667008091096, -0.7879004041258289570 ) ) ;
#5236 = CARTESIAN_POINT ( 'NONE',  ( 3.157961424266928052, 0.9873743524775533409, 1.956624655947765357 ) ) ;
#5237 = CARTESIAN_POINT ( 'NONE',  ( 6.983263157960363010, -0.009046620988246899253, 2.153544821522495489 ) ) ;
#5238 = CARTESIAN_POINT ( 'NONE',  ( 3.696369045748033155, -2.259781416529721643, -0.1137371904085457408 ) ) ;
#5239 = CARTESIAN_POINT ( 'NONE',  ( -6.742482464697739708, 6.760651051769146491, 0.7998128361456341429 ) ) ;
#5240 = FACE_OUTER_BOUND ( 'NONE', #185647, .T. ) ;
#5241 = CARTESIAN_POINT ( 'NONE',  ( 6.093313910611117379, 7.014445836765536235, -0.9825430356366869900 ) ) ;
#5242 = CARTESIAN_POINT ( 'NONE',  ( 1.500000000000001332, 14.12499999999999822, 0.000000000000000000 ) ) ;
#5243 = CARTESIAN_POINT ( 'NONE',  ( 6.224601922449876312, 6.434659462379210382, 0.000000000000000000 ) ) ;
#5244 = CARTESIAN_POINT ( 'NONE',  ( 5.624192029756354572, 1.053330351427090639, -1.421934073773284180 ) ) ;
#5245 = B_SPLINE_CURVE_WITH_KNOTS ( 'NONE', 3,
 ( #15324, #153623, #169858, #51049, #47881, #116099 ),
 .UNSPECIFIED., .F., .F.,
 ( 4, 2, 4 ),
 ( 0.000000000000000000, 0.002403937268455933786, 0.004807874536911865837 ),
 .UNSPECIFIED. ) ;
#5246 = CARTESIAN_POINT ( 'NONE',  ( 3.404942666290892817, -0.3948933297331903014, -1.973820178108119272 ) ) ;
#5247 = CARTESIAN_POINT ( 'NONE',  ( 6.774270308322468459, 11.05506579301824743, 0.7998128361456462443 ) ) ;
#5248 = CARTESIAN_POINT ( 'NONE',  ( 1.729655969393493642, -1.983145177596838948, 0.7090631796887718608 ) ) ;
#5249 = CARTESIAN_POINT ( 'NONE',  ( 1.364683531249996529, 11.71354166700806587, 0.7879004041258405033 ) ) ;
#5250 = CARTESIAN_POINT ( 'NONE',  ( 1.855843448759408210, -0.6666243292093411155, 1.853429361541816700 ) ) ;
#5251 = CARTESIAN_POINT ( 'NONE',  ( -4.496464221587651799, 5.274905009054215554, 1.199719254218452935 ) ) ;
#5253 = EDGE_LOOP ( 'NONE', ( #32865, #102273, #31606, #108392, #176513 ) ) ;
#5252 = CARTESIAN_POINT ( 'NONE',  ( 5.642768253578701376, 1.748184277621564808, 0.4749025624241067223 ) ) ;
#5254 = CARTESIAN_POINT ( 'NONE',  ( 6.317736394288135493, 8.393778431468064127, 1.443375672974076540 ) ) ;
#5255 = EDGE_CURVE ( 'NONE', #20303, #8789, #204233, .T. ) ;
#5256 = CARTESIAN_POINT ( 'NONE',  ( 0.3910932212915787520, 3.280071935319364584, -1.963192794826990495 ) ) ;
#5257 = CARTESIAN_POINT ( 'NONE',  ( 5.348468966913380029, 0.5439794105128460400, 1.789823788735760646 ) ) ;
#5258 = AXIS2_PLACEMENT_3D ( 'NONE', #56140, #70223, #39899 ) ;
#5259 = CARTESIAN_POINT ( 'NONE',  ( 5.137584473783054051, 1.933663220787355419, -0.7400441640052904946 ) ) ;
#5260 = CARTESIAN_POINT ( 'NONE',  ( -0.6125000000000175859, 2.541666666666664298, 1.060881119635903147 ) ) ;
#5261 = CARTESIAN_POINT ( 'NONE',  ( -5.777182852754558340, 5.912670547734647286, 0.000000000000000000 ) ) ;
#5262 = CARTESIAN_POINT ( 'NONE',  ( -4.124095526617549778E-13, -0.9769569599453676867, 3.449959810851647823 ) ) ;
#5263 = CARTESIAN_POINT ( 'NONE',  ( 1.499999999999989120, 0.5250000000000185629, 0.000000000000000000 ) ) ;
#5264 = CARTESIAN_POINT ( 'NONE',  ( 7.588813295347141441, 9.876701482703580837, -1.599625672291262513 ) ) ;
#5265 = CARTESIAN_POINT ( 'NONE',  ( -9.450196763925152510, 10.98398329845622001, -1.199719254218441611 ) ) ;
#5266 = CARTESIAN_POINT ( 'NONE',  ( 5.722423353419669567, 8.833855124701747386, 1.199719254218451159 ) ) ;
#5267 = CARTESIAN_POINT ( 'NONE',  ( -1.364683531250000748, -0.7406249996585803075, 0.000000000000000000 ) ) ;
#5268 = CARTESIAN_POINT ( 'NONE',  ( -1.500000000000001332, 1.400000000000019229, 0.000000000000000000 ) ) ;
#5270 = CARTESIAN_POINT ( 'NONE',  ( 4.904298879841284098, 6.744767997946721216, 1.599625672291267398 ) ) ;
#5269 = CARTESIAN_POINT ( 'NONE',  ( 4.685966490639408732, -1.205361723144786845, -1.547842780461285761 ) ) ;
#5271 = CARTESIAN_POINT ( 'NONE',  ( 2.179064334209149578, -0.9478932651061505732, -1.779355105811925020 ) ) ;
#5272 = CARTESIAN_POINT ( 'NONE',  ( 2.448326871961825191, -1.317826014703428639, 1.390694818219958107 ) ) ;
#5273 = EDGE_CURVE ( 'NONE', #36822, #70481, #131023, .T. ) ;
#5274 = DIRECTION ( 'NONE',  ( 0.000000000000000000, 1.000000000000000000, 0.000000000000000000 ) ) ;
#5275 = CARTESIAN_POINT ( 'NONE',  ( 0.5565083568685527116, -1.583368386835169783, 1.515454571103365344 ) ) ;
#5276 = CARTESIAN_POINT ( 'NONE',  ( 6.639320575229251453, 0.008029245381881157731, 1.796863947021019925 ) ) ;
#5277 = CARTESIAN_POINT ( 'NONE',  ( 2.565516880305099612, 1.835255434019352094, -0.3607447438512822457 ) ) ;
#5278 = CARTESIAN_POINT ( 'NONE',  ( -1.201851678989727383E-14, 5.196875000341422357, -1.575800808251660134 ) ) ;
#5279 = CARTESIAN_POINT ( 'NONE',  ( 4.043230579294037952, 0.1031557717955585846, 2.010702285795034072 ) ) ;
#5280 = CARTESIAN_POINT ( 'NONE',  ( -7.914208982075130905, 10.25632978388623684, -1.599625672291263179 ) ) ;
#5282 = CARTESIAN_POINT ( 'NONE',  ( 4.200857891667449273, 1.936436120981197773, 0.8564517604346032487 ) ) ;
#5281 = CARTESIAN_POINT ( 'NONE',  ( -6.399085315970155285, 6.567947078161039620, -0.7216878364870278340 ) ) ;
#5283 = CARTESIAN_POINT ( 'NONE',  ( 5.898901817742318698, 0.4001337562283372451, 2.031160294743330486 ) ) ;
#5285 = CARTESIAN_POINT ( 'NONE',  ( 11.88156762547254175, 13.87999991545966516, 1.686557021358693786 ) ) ;
#5284 = CARTESIAN_POINT ( 'NONE',  ( 1.259447021655529797, 2.059213905598542116, -0.3608319165549890295 ) ) ;
#5287 = ORIENTED_EDGE ( 'NONE', *, *, #128928, .T. ) ;
#5286 = CARTESIAN_POINT ( 'NONE',  ( 5.913091143547532624, 1.611232972626057247, 0.8583240166551919792 ) ) ;
#5288 = CARTESIAN_POINT ( 'NONE',  ( 8.450809820019639318, 8.753699632978056755, -0.7998128361456291469 ) ) ;
#5289 = DIRECTION ( 'NONE',  ( 0.000000000000000000, 1.000000000000000000, 0.000000000000000000 ) ) ;
#5290 = SURFACE_SIDE_STYLE ('',( #7441 ) ) ;
#5291 = CARTESIAN_POINT ( 'NONE',  ( -10.40865662669954084, 4.028931174475638421, 7.242212795919873436 ) ) ;
#5292 = CARTESIAN_POINT ( 'NONE',  ( 7.917598520256366790, 8.339545816494993602, 1.040834085586084257E-14 ) ) ;
#5293 = CARTESIAN_POINT ( 'NONE',  ( -1.364683531250014514, 13.15104166700806410, -0.7879004041258335089 ) ) ;
#5294 = CARTESIAN_POINT ( 'NONE',  ( 0.9612203838427415548, -1.427409828940959136, -1.115214234437786223 ) ) ;
#5295 = CARTESIAN_POINT ( 'NONE',  ( -6.984421689334302741, 11.30024240419870374, 0.000000000000000000 ) ) ;
#5296 = CARTESIAN_POINT ( 'NONE',  ( 6.681470773436232413, 6.689470745297396270, -0.7998128361456281477 ) ) ;
#5297 = CARTESIAN_POINT ( 'NONE',  ( 0.4635785636673696586, -6.836568542494932288, 10.85353573482940703 ) ) ;
#5298 = CARTESIAN_POINT ( 'NONE',  ( -1.500000000000015099, 12.26041666734946212, -0.8660254037844309360 ) ) ;
#5299 = CARTESIAN_POINT ( 'NONE',  ( 2.737856954955798727, 5.281584649835344258, 1.199719254218452047 ) ) ;
#5300 = EDGE_LOOP ( 'NONE', ( #79413, #9856, #93170, #114096 ) ) ;
#5301 = CARTESIAN_POINT ( 'NONE',  ( -0.1411974294642202310, -0.0004739540254597266757, -1.900147702309512132 ) ) ;
#5302 = CARTESIAN_POINT ( 'NONE',  ( 0.4168467196605326053, -0.7183999135813923242, -1.995210048009891102 ) ) ;
#5303 = CARTESIAN_POINT ( 'NONE',  ( 2.007420792093927986E-08, -6.938893903907228378E-15, -1.225000000000033396 ) ) ;
#5304 = CARTESIAN_POINT ( 'NONE',  ( -0.1394461523061326647, 2.860155921427895542, -2.768185420354400073 ) ) ;
#5305 = CARTESIAN_POINT ( 'NONE',  ( -4.609409038966234995, 7.361099064560491456, -1.082531754730549967 ) ) ;
#5306 = CIRCLE ( 'NONE', #119525, 10.86343145750506878 ) ;
#5307 = CARTESIAN_POINT ( 'NONE',  ( 9.490344339885973923, 12.09515436799890331, -1.443375672974057666 ) ) ;
#5308 = CARTESIAN_POINT ( 'NONE',  ( 3.537912347765668208, 1.245987026601946157, 1.525231921242198307 ) ) ;
#5309 = CARTESIAN_POINT ( 'NONE',  ( 4.323842328482737862, 0.8596156136044874607, -1.824127480631778653 ) ) ;
#5310 = CARTESIAN_POINT ( 'NONE',  ( -7.043624497499477499, 8.176315654292865887, 1.199719254218450271 ) ) ;
#5311 = CARTESIAN_POINT ( 'NONE',  ( 1.124100812432970948E-16, 2.999999999999975131, -2.025000000000006573 ) ) ;
#5312 = CARTESIAN_POINT ( 'NONE',  ( 4.839868765920234850, 2.185429510258177110, 0.1630863781024796955 ) ) ;
#5313 = DIRECTION ( 'NONE',  ( 0.000000000000000000, 0.000000000000000000, -1.000000000000000000 ) ) ;
#5314 = CARTESIAN_POINT ( 'NONE',  ( 2.590742828618552984, -0.3275076452619613554, -1.898194946008352035 ) ) ;
#5315 = CARTESIAN_POINT ( 'NONE',  ( -6.496328159242330536, 10.73079995242472862, 0.000000000000000000 ) ) ;
#5316 = CARTESIAN_POINT ( 'NONE',  ( -0.1298852118744256712, 0.2531197755418754247, -1.761387242530809250 ) ) ;
#5317 = CARTESIAN_POINT ( 'NONE',  ( 0.3818278861203865393, 2.057605126571937060, -0.7983354260262252033 ) ) ;
#5319 = EDGE_CURVE ( 'NONE', #74967, #176780, #106660, .T. ) ;
#5318 = CARTESIAN_POINT ( 'NONE',  ( -0.6823417656250039265, 12.81770833367473017, -1.181850606188755259 ) ) ;
#5320 = ORIENTED_EDGE ( 'NONE', *, *, #70130, .T. ) ;
#5321 = CARTESIAN_POINT ( 'NONE',  ( 4.177320726786311056, 5.966903162707725805, -1.443375672974068769 ) ) ;
#5322 = EDGE_LOOP ( 'NONE', ( #668, #88355, #119854, #35076 ) ) ;
#5323 = CARTESIAN_POINT ( 'NONE',  ( 5.207841159657320418, 0.6216970817616838119, -1.868779976745947202 ) ) ;
#5324 = ORIENTED_EDGE ( 'NONE', *, *, #193355, .T. ) ;
#5326 = CARTESIAN_POINT ( 'NONE',  ( 3.686192936682455734, 1.120187844794858556, 1.672449120617898410 ) ) ;
#5325 = CARTESIAN_POINT ( 'NONE',  ( 0.01113493735188827126, -1.904398801838134148, 0.3797647843634504583 ) ) ;
#5327 = CARTESIAN_POINT ( 'NONE',  ( 5.378365493435281586, -0.3450152841970657858, 2.272265683862843666 ) ) ;
#5328 = CARTESIAN_POINT ( 'NONE',  ( 3.414761196407948063, -1.412042937968212231, 1.212274210779472394 ) ) ;
#5329 = CARTESIAN_POINT ( 'NONE',  ( 5.580062740476173566, 8.667767742934335828, 1.199719254218451159 ) ) ;
#5330 = FACE_BOUND ( 'NONE', #144187, .T. ) ;
#5331 = CARTESIAN_POINT ( 'NONE',  ( -7.881367368245678406, 8.089350105908421185, 0.7998128361456602331 ) ) ;
#5332 = CARTESIAN_POINT ( 'NONE',  ( -5.817857314039913241, 5.960124085900898372, 0.000000000000000000 ) ) ;
#5333 = CARTESIAN_POINT ( 'NONE',  ( 5.530836773642837656, -1.889722758269284375, 0.8948517497979097124 ) ) ;
#5334 = CARTESIAN_POINT ( 'NONE',  ( 5.748293942514166588, 7.729428904398431222, -1.443375672974057666 ) ) ;
#5335 = ORIENTED_EDGE ( 'NONE', *, *, #197116, .T. ) ;
#5336 = FACE_OUTER_BOUND ( 'NONE', #168055, .T. ) ;
#5337 = DIRECTION ( 'NONE',  ( 0.5994789404140788980, 1.518179186858609835E-15, -0.8003905296791143931 ) ) ;
#5338 = CARTESIAN_POINT ( 'NONE',  ( 0.5920835508136900183, -1.811502216344462735, -0.2265648652611390590 ) ) ;
#5339 = CARTESIAN_POINT ( 'NONE',  ( -4.843287188579803448, 6.673587691474970107, -1.599625672291256295 ) ) ;
#5340 = CARTESIAN_POINT ( 'NONE',  ( 2.531537987306311965, -1.440582175967281886, 0.9650062983845784093 ) ) ;
#5341 = CARTESIAN_POINT ( 'NONE',  ( -0.5000000000000143219, 3.949999999999981526, 0.4999999999999553690 ) ) ;
#5342 = CARTESIAN_POINT ( 'NONE',  ( -6.126860945727902852, 6.002842251083519542, -0.2255282439200041456 ) ) ;
#5344 = CARTESIAN_POINT ( 'NONE',  ( -6.287230548435221777, 8.358188277972981695, -1.599625672291263179 ) ) ;
#5343 = AXIS2_PLACEMENT_3D ( 'NONE', #191787, #206976, #175571 ) ;
#5345 = CARTESIAN_POINT ( 'NONE',  ( -5.913158477246164502, 5.999510931274985026, -0.08576477159101922321 ) ) ;
#5346 = CARTESIAN_POINT ( 'NONE',  ( 0.6376584384039893916, 1.932990051301992418, -0.7417924570976216492 ) ) ;
#5347 = CARTESIAN_POINT ( 'NONE',  ( 5.971303284387838417, 0.1295235881030691594, -1.821162830480331563 ) ) ;
#5348 = CARTESIAN_POINT ( 'NONE',  ( 3.045700443693433179, 1.383923128670875746, 1.390673908496591782 ) ) ;
#5349 = CARTESIAN_POINT ( 'NONE',  ( 1.224999999999979661, -0.8124999993172135060, -2.602085213965210642E-14 ) ) ;
#5350 = CARTESIAN_POINT ( 'NONE',  ( -9.667127221743832877, 11.23706883257798772, 1.199719254218462483 ) ) ;
#5351 = CARTESIAN_POINT ( 'NONE',  ( 5.926885707468349196, 10.06645042535509660, 1.040834085586084257E-14 ) ) ;
#5352 = CARTESIAN_POINT ( 'NONE',  ( 3.721430941620011534, 1.819509361161365524, 1.088713516244857571 ) ) ;
#5353 = CARTESIAN_POINT ( 'NONE',  ( 6.827182134110199918, 2.946470958711099541, 2.641117900019366527 ) ) ;
#5354 = CARTESIAN_POINT ( 'NONE',  ( -9.646789991323334590, 11.21334206375407305, 1.199719254218462483 ) ) ;
#5355 = CIRCLE ( 'NONE', #209464, 0.08000000000000015432 ) ;
#5356 = CARTESIAN_POINT ( 'NONE',  ( 1.305626334525695986, -1.629615561912756805, -1.276682400165381148 ) ) ;
#5358 = CARTESIAN_POINT ( 'NONE',  ( 1.499999999999993117, 14.63541666734946567, 0.8660254037844409281 ) ) ;
#5357 = CARTESIAN_POINT ( 'NONE',  ( 6.827182134110200806, 1.288579688585177685, 1.926502426867699347 ) ) ;
#5360 = ORIENTED_EDGE ( 'NONE', *, *, #184823, .T. ) ;
#5359 = CARTESIAN_POINT ( 'NONE',  ( 4.494933454782477078, -2.154585855983886411, -0.5399016382821394400 ) ) ;
#5361 = CARTESIAN_POINT ( 'NONE',  ( 1.495234749544295250, -2.280609600776092094, 0.2875172478875551163 ) ) ;
#5363 = CARTESIAN_POINT ( 'NONE',  ( 0.5144084716053355377, 0.7454083195421266073, 1.814826383214888983 ) ) ;
#5362 = CARTESIAN_POINT ( 'NONE',  ( 8.242994207428692377, 12.56065097540143327, -0.7216878364870328300 ) ) ;
#5365 = CARTESIAN_POINT ( 'NONE',  ( -1.737500000000000266, -0.7583333333333330817, -3.009438278150923907 ) ) ;
#5364 = CARTESIAN_POINT ( 'NONE',  ( 7.363486825997814123, 7.763358516518489516, 0.000000000000000000 ) ) ;
#5366 = EDGE_CURVE ( 'NONE', #10766, #101960, #196600, .T. ) ;
#5367 = DIRECTION ( 'NONE',  ( -0.000000000000000000, -1.000000000000000000, 0.000000000000000000 ) ) ;
#5368 = DIRECTION ( 'NONE',  ( 0.000000000000000000, 0.000000000000000000, 1.000000000000000000 ) ) ;
#5369 = ORIENTED_EDGE ( 'NONE', *, *, #11637, .F. ) ;
#5371 = CARTESIAN_POINT ( 'NONE',  ( 1.408343819019456176E-15, 0.7999999999999951594, 11.50000000000000000 ) ) ;
#5370 = CIRCLE ( 'NONE', #33087, 10.91999999999999105 ) ;
#5372 = CARTESIAN_POINT ( 'NONE',  ( 3.480628297764537304, -1.280852673386581264, 1.420289963180096260 ) ) ;
#5373 = DIRECTION ( 'NONE',  ( -1.124869321039521280E-29, -7.437565543542506798E-15, -1.000000000000000000 ) ) ;
#5374 = CARTESIAN_POINT ( 'NONE',  ( 3.715580044805122384, -1.699234090967314259, 0.2946211727567394911 ) ) ;
#5375 = CARTESIAN_POINT ( 'NONE',  ( 2.395720570290179374, -1.993893129684479293, 0.3006499569925198956 ) ) ;
#5376 = CARTESIAN_POINT ( 'NONE',  ( 3.780169564947546856, 1.941421826978003251, -1.230584599089700637 ) ) ;
#5377 = CARTESIAN_POINT ( 'NONE',  ( 3.392113076582465858, -0.9204767452889413004, 2.066876591271109120 ) ) ;
#5378 = CARTESIAN_POINT ( 'NONE',  ( 0.1357705729100426029, -2.015811560716780360, 0.8986578214904348272 ) ) ;
#5379 = CARTESIAN_POINT ( 'NONE',  ( -4.326460416536637155, 8.061637896019123062, 0.000000000000000000 ) ) ;
#5380 = ORIENTED_EDGE ( 'NONE', *, *, #64826, .F. ) ;
#5381 = CARTESIAN_POINT ( 'NONE',  ( 4.657331418887999064, 0.3884847549131437705, -1.726375946583807774 ) ) ;
#5382 = EDGE_CURVE ( 'NONE', #18903, #170487, #159341, .T. ) ;
#5384 = CARTESIAN_POINT ( 'NONE',  ( 0.9555020568867471642, 0.4423240407584581035, -2.249030425913514541 ) ) ;
#5383 = CARTESIAN_POINT ( 'NONE',  ( 5.515134625708930649, 9.656350506627580543, 0.000000000000000000 ) ) ;
#5385 = CARTESIAN_POINT ( 'NONE',  ( 5.753808258465379133, 0.7501079416377672837, 1.681592913607635964 ) ) ;
#5386 = CARTESIAN_POINT ( 'NONE',  ( -3.704402285031864306, 5.344888637335695414, -1.599625672291256295 ) ) ;
#5387 = CARTESIAN_POINT ( 'NONE',  ( 5.648420989521034663, -1.729380818958951460, 1.345873388983606533 ) ) ;
#5388 = CARTESIAN_POINT ( 'NONE',  ( -4.359828915246279024, 7.244161613499399799, -1.199719254218455378 ) ) ;
#5389 = CARTESIAN_POINT ( 'NONE',  ( 7.065207446497155708, 9.336104335703744539, 0.000000000000000000 ) ) ;
#5390 = CARTESIAN_POINT ( 'NONE',  ( -8.799907370706367971, 15.46908217234898153, 8.208919216386629358 ) ) ;
#5391 = CARTESIAN_POINT ( 'NONE',  ( 5.564915762860970894, 1.570151797963925455, -1.349580972669261580 ) ) ;
#5392 = CARTESIAN_POINT ( 'NONE',  ( 1.464077725791514517, -1.074659653367866952, 1.706114136832518779 ) ) ;
#5393 = CARTESIAN_POINT ( 'NONE',  ( 0.7499999999999867883, -0.6520833326505159899, -1.299038105676652899 ) ) ;
#5394 = CARTESIAN_POINT ( 'NONE',  ( 4.740804336882096237, 0.3310356755545171836, 1.897698676112127725 ) ) ;
#5395 = CARTESIAN_POINT ( 'NONE',  ( -0.6823417656250003738, 10.90104166700806765, 1.181850606188754593 ) ) ;
#5396 = CARTESIAN_POINT ( 'NONE',  ( 1.072868727471010253, 0.9067168766181363804, 2.028134479351159314 ) ) ;
#5398 = VERTEX_POINT ( 'NONE', #94559 ) ;
#5397 = DIRECTION ( 'NONE',  ( -1.000000000000000000, 0.000000000000000000, 0.000000000000000000 ) ) ;
#5400 = DIRECTION ( 'NONE',  ( 0.000000000000000000, 3.252606517456504467E-14, -1.000000000000000000 ) ) ;
#5399 = CARTESIAN_POINT ( 'NONE',  ( 1.483013432599449732, 7.294277089886982424, -4.259227663826814059 ) ) ;
#5401 = CARTESIAN_POINT ( 'NONE',  ( -3.633221978782290140, 6.222214161012547429, -1.082531754730549967 ) ) ;
#5402 = CARTESIAN_POINT ( 'NONE',  ( 3.785751206713845018, 5.439795712631356750, 1.599625672291267398 ) ) ;
#5403 = LINE ( 'NONE', #55263, #76976 ) ;
#5404 = DIRECTION ( 'NONE',  ( 1.000000000000000000, 0.000000000000000000, 0.000000000000000000 ) ) ;
#5405 = CARTESIAN_POINT ( 'NONE',  ( 4.352889007613729433, 0.3757914745146764823, -1.699215345876355476 ) ) ;
#5406 = CARTESIAN_POINT ( 'NONE',  ( 2.330453122711079850, -1.209328770571056921, 1.544706564130463811 ) ) ;
#5408 = CARTESIAN_POINT ( 'NONE',  ( -1.364683531250012516, 2.801041667008090652, -0.7879004041258289570 ) ) ;
#5407 = CARTESIAN_POINT ( 'NONE',  ( 4.798696304233017074, 7.685897223992134819, -1.199719254218452047 ) ) ;
#5409 = CARTESIAN_POINT ( 'NONE',  ( -4.361599125657974696, 7.193191237876310318, 1.033186747995703758 ) ) ;
#5410 = CARTESIAN_POINT ( 'NONE',  ( 4.371348721082305211, 3.994328350884451151, -0.09103173162486978554 ) ) ;
#5411 = CARTESIAN_POINT ( 'NONE',  ( 6.619590441841329387, 0.3365870006281460047, -1.932621868259084330 ) ) ;
#5412 = CARTESIAN_POINT ( 'NONE',  ( -8.616370316684697883, 10.01118577667568132, -1.199719254218446718 ) ) ;
#5413 = ADVANCED_FACE ( 'NONE', ( #11130 ), #44741, .F. ) ;
#5414 = CARTESIAN_POINT ( 'NONE',  ( -3.267151830768946663, 6.755501535964989479, -0.7216878364870257245 ) ) ;
#5415 = CARTESIAN_POINT ( 'NONE',  ( 5.032435514249763209, 0.5899841883351600869, 1.928258608204669766 ) ) ;
#5416 = CARTESIAN_POINT ( 'NONE',  ( 0.7786449305766733886, -1.254482527970951056, 1.882701536962180677 ) ) ;
#5418 = ORIENTED_EDGE ( 'NONE', *, *, #51505, .F. ) ;
#5417 = CARTESIAN_POINT ( 'NONE',  ( -6.175902666224832416, 7.163973517805802160, -1.199719254218446718 ) ) ;
#5419 = CARTESIAN_POINT ( 'NONE',  ( -0.6823417656249969321, 5.467708333674756283, -1.181850606188749264 ) ) ;
#5420 = CARTESIAN_POINT ( 'NONE',  ( 1.739302498465819191, -1.351291084634953066, -1.293660915597586003 ) ) ;
#5421 = CARTESIAN_POINT ( 'NONE',  ( -0.1405533004718754753, 0.003749010675345095921, -1.720146753850458010 ) ) ;
#5423 = CARTESIAN_POINT ( 'NONE',  ( 4.370767597569780172, -0.0006098066561242150270, -2.191739723162715592 ) ) ;
#5422 = CARTESIAN_POINT ( 'NONE',  ( 0.6801582343749987825, 1.557291667008103841, -1.178068619123876282 ) ) ;
#5424 = CARTESIAN_POINT ( 'NONE',  ( 5.579250153011313884, -0.04958841179729735205, -2.307219497322360535 ) ) ;
#5425 = CARTESIAN_POINT ( 'NONE',  ( 0.6728171419645075924, -1.940266777691628919, -0.6950667680841491336 ) ) ;
#5426 = CARTESIAN_POINT ( 'NONE',  ( 2.888542945859973177, 1.665235949713929076, -0.9988640340363763581 ) ) ;
#5427 = CARTESIAN_POINT ( 'NONE',  ( -5.870317324592821073, 6.911420302522161663, -1.082531754730543083 ) ) ;
#5428 = CARTESIAN_POINT ( 'NONE',  ( 0.7144793466747193511, 13.35177634501765453, -1.205057194458958314 ) ) ;
#5429 = CARTESIAN_POINT ( 'NONE',  ( -0.6801582343750247617, 0.09895833367471601472, -1.178068619123872729 ) ) ;
#5430 = CARTESIAN_POINT ( 'NONE',  ( 4.008435526009396455, -1.928752077057366732, 0.5880193435906443389 ) ) ;
#5431 = CARTESIAN_POINT ( 'NONE',  ( -4.907688418022547516, 4.827984030555475314, 1.214306433183764966E-14 ) ) ;
#5432 = CARTESIAN_POINT ( 'NONE',  ( -6.577640801285370209, 7.702944352034914566, -1.199719254218452047 ) ) ;
#5433 = CARTESIAN_POINT ( 'NONE',  ( 9.745613490124728884, 10.26430391476735338, 0.7998128361456462443 ) ) ;
#5435 = CARTESIAN_POINT ( 'NONE',  ( 7.720982915750170150, -5.743759731405705615, -7.834948807407336346 ) ) ;
#5434 = CARTESIAN_POINT ( 'NONE',  ( 0.9612317138737861422, 0.3586375672061762887, -1.789940867121169843 ) ) ;
#5436 = CARTESIAN_POINT ( 'NONE',  ( -4.936050443827081580, 7.916420063510339666, 1.199719254218452935 ) ) ;
#5437 = DIRECTION ( 'NONE',  ( 8.638326563840814399E-31, 0.000000000000000000, 1.000000000000000000 ) ) ;
#5438 = CARTESIAN_POINT ( 'NONE',  ( -10.77299012366456310, 5.423410747438590640, 6.621146351739780833 ) ) ;
#5439 = ORIENTED_EDGE ( 'NONE', *, *, #188097, .F. ) ;
#5440 = CARTESIAN_POINT ( 'NONE',  ( 6.543830163797104582, 0.7912256320986108538, -1.903158165889913045 ) ) ;
#5441 = CARTESIAN_POINT ( 'NONE',  ( -7.892254816486440561, 8.380254505421877553, 0.000000000000000000 ) ) ;
#5442 = CARTESIAN_POINT ( 'NONE',  ( 6.902509602688803980, 9.146290184594002781, -1.443375672974064550 ) ) ;
#5443 = CARTESIAN_POINT ( 'NONE',  ( -2.819205876637805641, 5.376491725131008259, -1.199719254218446718 ) ) ;
#5444 = CARTESIAN_POINT ( 'NONE',  ( -10.13202086811422475, 10.71511252242175161, -0.7998128361456291469 ) ) ;
#5445 = CARTESIAN_POINT ( 'NONE',  ( 5.338538087541965460, 1.201400599988803108, -1.623342581396812090 ) ) ;
#5447 = VERTEX_POINT ( 'NONE', #144402 ) ;
#5446 = CARTESIAN_POINT ( 'NONE',  ( 5.953820247260992460, -1.607154219335062528, -1.533616513404257198 ) ) ;
#5448 = CARTESIAN_POINT ( 'NONE',  ( -3.169574050544739841, 6.919863168935977527, -0.7998128361456481317 ) ) ;
#5449 = CARTESIAN_POINT ( 'NONE',  ( 6.226218857173709154, 8.287007971501239467, 1.599625672291281386 ) ) ;
#5450 = CARTESIAN_POINT ( 'NONE',  ( 5.207911835226475716, -2.051185258288893198, 0.1996322284415520676 ) ) ;
#5451 = CARTESIAN_POINT ( 'NONE',  ( 4.254529844270301453, 1.955172953530256219, -0.4926405443339901269 ) ) ;
#5452 = ORIENTED_EDGE ( 'NONE', *, *, #138983, .T. ) ;
#5453 = DIRECTION ( 'NONE',  ( -1.000000000000000000, 5.782411586589355667E-16, 0.000000000000000000 ) ) ;
#5454 = CARTESIAN_POINT ( 'NONE',  ( 2.706824224222692088, 6.309712028235118453, 0.7998128361456362523 ) ) ;
#5456 = EDGE_LOOP ( 'NONE', ( #57254, #59418, #188811, #140618 ) ) ;
#5455 = CARTESIAN_POINT ( 'NONE',  ( -5.935437387732586778, 10.14670372898850381, -0.7998128361456362523 ) ) ;
#5457 = CARTESIAN_POINT ( 'NONE',  ( 4.749341595749815070, 8.305088035112140332, 0.7662636247844747395 ) ) ;
#5458 = CARTESIAN_POINT ( 'NONE',  ( 4.446638634790680555, 1.314796391739967207, 1.528506369862133285 ) ) ;
#5459 = CARTESIAN_POINT ( 'NONE',  ( 3.749809578975582536, 0.6641696684822319119, 1.717346325712478583 ) ) ;
#5460 = CARTESIAN_POINT ( 'NONE',  ( 4.370663978927085580, 5.060324124126027279, -1.009771797811724214 ) ) ;
#5461 = CARTESIAN_POINT ( 'NONE',  ( 2.069360784497351613, -2.110879405061675929, -0.9329422106417961658 ) ) ;
#5462 = CARTESIAN_POINT ( 'NONE',  ( 6.481679955784983349, 9.719654494127929922, -1.199719254218452047 ) ) ;
#5463 = CARTESIAN_POINT ( 'NONE',  ( 3.972077263441410100, 1.197190051160206936, 1.799587594625361220 ) ) ;
#5464 = CARTESIAN_POINT ( 'NONE',  ( 7.747594715205354809, 11.12627870345989756, -1.199719254218446718 ) ) ;
#5465 = CARTESIAN_POINT ( 'NONE',  ( -5.870844209917351009, 6.808071985447069707, -1.199719254218446718 ) ) ;
#5466 = CARTESIAN_POINT ( 'NONE',  ( 3.198860821731682513, -1.541234334381531568, -1.705209785003541700 ) ) ;
#5467 = CARTESIAN_POINT ( 'NONE',  ( -9.568429106564499520, 15.10400138847699303, -7.242208005537321469 ) ) ;
#5468 = CARTESIAN_POINT ( 'NONE',  ( 3.742823004191514212E-13, -7.217909409572238033, -9.581972888692755319 ) ) ;
#5469 = CARTESIAN_POINT ( 'NONE',  ( 2.571000202304725590, 0.09389976206976291540, -1.868427151830873267 ) ) ;
#5470 =( BOUNDED_CURVE ( )  B_SPLINE_CURVE ( 3, ( #69422, #100873, #2278, #134487 ),
 .UNSPECIFIED., .F., .T. ) 
 B_SPLINE_CURVE_WITH_KNOTS ( ( 4, 4 ),
 ( 0.000000000000000000, 0.5000000000000018874 ),
 .UNSPECIFIED. ) 
 CURVE ( )  GEOMETRIC_REPRESENTATION_ITEM ( )  RATIONAL_B_SPLINE_CURVE ( ( 1.000000000000000000, 0.3333333333333308723, 0.3333333333333333703, 1.000000000000002442 ) ) 
 REPRESENTATION_ITEM ( '' )  );
#5471 = CARTESIAN_POINT ( 'NONE',  ( 6.543826718160733691, 0.7548084958455666404, -1.821436488709103019 ) ) ;
#5472 = AXIS2_PLACEMENT_3D ( 'NONE', #139402, #59195, #174049 ) ;
#5474 = CARTESIAN_POINT ( 'NONE',  ( -7.747558435566414659, 8.003516027774422170, -0.7998128361456362523 ) ) ;
#5473 = CARTESIAN_POINT ( 'NONE',  ( -1.364683531249997417, 4.509375000341424133, 1.214306433183764966E-14 ) ) ;
#5475 = CARTESIAN_POINT ( 'NONE',  ( 2.104404934925046877, -2.206339196854599116, 0.05594281105186085790 ) ) ;
#5476 = ORIENTED_EDGE ( 'NONE', *, *, #125755, .T. ) ;
#5477 = CARTESIAN_POINT ( 'NONE',  ( 0.000000000000000000, 13.49999999999999822, -1.500000000000000222 ) ) ;
#5478 = CARTESIAN_POINT ( 'NONE',  ( 3.167801447087334576, 6.847518788243868393, -0.7998128361456291469 ) ) ;
#5479 = CARTESIAN_POINT ( 'NONE',  ( -5.447678794592645701, 5.250046769979851646, 0.000000000000000000 ) ) ;
#5480 = CARTESIAN_POINT ( 'NONE',  ( -1.038038101541534383E-14, -8.644755361503008828, -10.68216772480108823 ) ) ;
#5481 = CARTESIAN_POINT ( 'NONE',  ( 6.332890595682218127, 0.1930081403669886009, 1.961983401381848457 ) ) ;
#5482 = CARTESIAN_POINT ( 'NONE',  ( 5.162836451262333703, -1.674513216643868985, 1.588141549981958001 ) ) ;
#5483 = CARTESIAN_POINT ( 'NONE',  ( 0.7659737006216191801, -1.952758744216346765, 0.1886366088557633325 ) ) ;
#5484 = CARTESIAN_POINT ( 'NONE',  ( 3.643474114467046387, 1.866637444603681528, -0.8776443792693452428 ) ) ;
#5485 = CARTESIAN_POINT ( 'NONE',  ( 6.805829924380118356, 7.042482454639357847, 0.7216878364870317197 ) ) ;
#5486 = CARTESIAN_POINT ( 'NONE',  ( 7.126746022638799971, 8.343567110280638133, 1.199719254218452047 ) ) ;
#5487 = CARTESIAN_POINT ( 'NONE',  ( 7.253248993186724114, 9.485209796849769504, 1.443375672974076540 ) ) ;
#5488 = CARTESIAN_POINT ( 'NONE',  ( -0.6823417656249969321, 4.030208333674754506, -1.181850606188749264 ) ) ;
#5489 = CARTESIAN_POINT ( 'NONE',  ( -3.447813423226582241, 14.52993373270244248, 11.50294194160398753 ) ) ;
#5490 = CARTESIAN_POINT ( 'NONE',  ( 4.406036734316882253, 6.163462161501577441, -1.443375672974051449 ) ) ;
#5491 = CARTESIAN_POINT ( 'NONE',  ( 6.127409529368080143, 0.1660417618732710210, -2.164901972331951363 ) ) ;
#5493 = CARTESIAN_POINT ( 'NONE',  ( 4.739718475747470627, 1.836682745182907972, 0.1304020654292817605 ) ) ;
#5492 = DIRECTION ( 'NONE',  ( 0.000000000000000000, 0.000000000000000000, -1.000000000000000000 ) ) ;
#5494 = CARTESIAN_POINT ( 'NONE',  ( 4.161361007603033180, 7.399433999391101580, -0.7812420967184935394 ) ) ;
#5495 = CARTESIAN_POINT ( 'NONE',  ( 6.251546423958431298, 2.185849743821382862, -0.1592787069685035195 ) ) ;
#5496 = CARTESIAN_POINT ( 'NONE',  ( -11.86239285000045918, 9.719999999999982876, 1.812080536912751061 ) ) ;
#5497 = CARTESIAN_POINT ( 'NONE',  ( -4.201283080389795366, 7.561618497949153195, 0.9685097419542560981 ) ) ;
#5498 = CARTESIAN_POINT ( 'NONE',  ( -0.3706017150059756071, 3.173913102025869737, -2.032929028842745733 ) ) ;
#5499 = CARTESIAN_POINT ( 'NONE',  ( 6.564609147483420060, 6.793222102749934876, 0.3624652974001541517 ) ) ;
#5500 = CARTESIAN_POINT ( 'NONE',  ( 11.86145016429273369, 13.50587408513255383, 1.099999999999996758 ) ) ;
#5501 = CARTESIAN_POINT ( 'NONE',  ( 2.043481384864866524, 0.6806142739823103360, -1.633949198972502570 ) ) ;
#5502 = VECTOR ( 'NONE', #213164, 1000.000000000000000 ) ;
#5503 = CARTESIAN_POINT ( 'NONE',  ( 6.516276865632868898, -2.012592099345715813, 0.05177761937730576691 ) ) ;
#5505 = CARTESIAN_POINT ( 'NONE',  ( 3.937047882288559286, -1.594636078160330150, -1.061121380078999143 ) ) ;
#5504 = CARTESIAN_POINT ( 'NONE',  ( -9.022061154889962964, 12.61315621642528129, -1.199719254218446718 ) ) ;
#5506 = DIRECTION ( 'NONE',  ( 0.000000000000000000, 1.000000000000000000, 0.000000000000000000 ) ) ;
#5507 = CARTESIAN_POINT ( 'NONE',  ( 5.547300264688804994, 1.737891114709901208, -0.9267001309954668864 ) ) ;
#5508 = CARTESIAN_POINT ( 'NONE',  ( 0.1762450972803019933, 2.096614079038420897, -0.3174041833761130360 ) ) ;
#5509 = CARTESIAN_POINT ( 'NONE',  ( 3.344469905398727239, 0.4532862802011444758, 1.814783984445811127 ) ) ;
#5511 = ORIENTED_EDGE ( 'NONE', *, *, #96073, .T. ) ;
#5510 = CARTESIAN_POINT ( 'NONE',  ( 6.516207646108923335, -0.8203346053292108753, -1.517322292280029350 ) ) ;
#5513 = CARTESIAN_POINT ( 'NONE',  ( 4.365362273920252889, 4.195270195769483124, 0.7216878364870317197 ) ) ;
#5512 = CARTESIAN_POINT ( 'NONE',  ( 3.158999515626020216, -1.670948785577108797, 1.441709373268922123 ) ) ;
#5514 = EDGE_CURVE ( 'NONE', #6079, #59123, #30565, .T. ) ;
#5515 = CARTESIAN_POINT ( 'NONE',  ( -1.364683531250012516, 3.092708333674755838, 0.7879004041258379498 ) ) ;
#5516 = CARTESIAN_POINT ( 'NONE',  ( 1.082570677935968062, 1.230128212588364356, -1.655568962787755005 ) ) ;
#5517 = CARTESIAN_POINT ( 'NONE',  ( 7.450369105909416589, 8.650851030771185890, -1.199719254218441611 ) ) ;
#5518 = CARTESIAN_POINT ( 'NONE',  ( 11.80235830595197655, 11.29999999999998117, 1.696088231482818065 ) ) ;
#5519 = DIRECTION ( 'NONE',  ( -0.000000000000000000, -1.000000000000000000, -0.000000000000000000 ) ) ;
#5520 = CARTESIAN_POINT ( 'NONE',  ( -3.419492857000915986, -0.02754147205532485668, -0.3393126727284642152 ) ) ;
#5521 = CARTESIAN_POINT ( 'NONE',  ( -7.503460210123537699, -6.893136966056810699, -8.043985462411194831 ) ) ;
#5522 = CARTESIAN_POINT ( 'NONE',  ( 3.490741092712910998, 2.019281663078629219, 0.4563312328872348722 ) ) ;
#5523 = CARTESIAN_POINT ( 'NONE',  ( 1.499999999999989120, 5.004166666666691299, 0.8660254037844524744 ) ) ;
#5524 = CARTESIAN_POINT ( 'NONE',  ( 4.741601036477289810, 6.554953847355395880, 1.599625672291267398 ) ) ;
#5525 = CARTESIAN_POINT ( 'NONE',  ( -6.387810837761664473, 6.908839790476999809, 0.8166356711787735589 ) ) ;
#5526 = CARTESIAN_POINT ( 'NONE',  ( 1.383469627199322538, 0.1461868815116218467, -2.014428406654201531 ) ) ;
#5527 = CARTESIAN_POINT ( 'NONE',  ( 0.6823417656249899377, 2.905208333674754062, 1.181850606188765695 ) ) ;
#5528 = CARTESIAN_POINT ( 'NONE',  ( 1.364683531249988535, 3.655208333674750509, -0.7879004041258239610 ) ) ;
#5529 = AXIS2_PLACEMENT_3D ( 'NONE', #173864, #210596, #141386 ) ;
#5531 = CARTESIAN_POINT ( 'NONE',  ( 10.39874063200158893, 11.23421161353111586, 0.000000000000000000 ) ) ;
#5530 = CARTESIAN_POINT ( 'NONE',  ( 0.1745949693968693039, 6.948552162806741705, -2.350360486623141121 ) ) ;
#5532 = CARTESIAN_POINT ( 'NONE',  ( 6.046249930811113060, 1.863882344683247094, -0.7690052245405626374 ) ) ;
#5533 = CARTESIAN_POINT ( 'NONE',  ( 6.174997428096934193, 1.663181612469267101, -0.9506077395253130780 ) ) ;
#5534 = CARTESIAN_POINT ( 'NONE',  ( -1.500000000000039524, 7.128742170989512239, -10.89107411574799045 ) ) ;
#5535 = CARTESIAN_POINT ( 'NONE',  ( 3.825867475279482566, 1.171244075711602051, -1.852137614134836907 ) ) ;
#5536 = CARTESIAN_POINT ( 'NONE',  ( -1.201851678989727383E-14, 2.243750000682818158, 1.732050807568877637 ) ) ;
#5537 = CARTESIAN_POINT ( 'NONE',  ( 2.601700882821424976, 1.355260107747566334, 1.349524769375435973 ) ) ;
#5538 = CARTESIAN_POINT ( 'NONE',  ( -5.530836599371015794, 8.540060901653093950, 1.199719254218452047 ) ) ;
#5539 = CARTESIAN_POINT ( 'NONE',  ( 5.463572716182834910, 5.476515711742504067, 0.7216878364870317197 ) ) ;
#5541 = CARTESIAN_POINT ( 'NONE',  ( 0.8961114988408731552, -0.9091644883451601711, -1.799914091915676639 ) ) ;
#5540 = FILL_AREA_STYLE ('',( #20737 ) ) ;
#5542 = CARTESIAN_POINT ( 'NONE',  ( -1.364683531250010295, 10.44270833367473017, 0.7879004041258445001 ) ) ;
#5544 = CARTESIAN_POINT ( 'NONE',  ( -5.257529707049291900, 9.355811434857983500, 0.7998128361456291469 ) ) ;
#5543 = CARTESIAN_POINT ( 'NONE',  ( 6.304242050522723240, 1.625252681175231029, -1.470355468214133543 ) ) ;
#5546 = ORIENTED_EDGE ( 'NONE', *, *, #102930, .T. ) ;
#5545 = CARTESIAN_POINT ( 'NONE',  ( 3.223388876545678183, -1.662537434388009938, 0.4588695312727729125 ) ) ;
#5547 = CARTESIAN_POINT ( 'NONE',  ( 7.039708073993665494, 9.236078724457858158, 1.599625672291281386 ) ) ;
#5548 = CARTESIAN_POINT ( 'NONE',  ( 4.147904930777053245, 6.926640621626830807, -1.199719254218452047 ) ) ;
#5549 = DIRECTION ( 'NONE',  ( 1.000000000000000000, 0.000000000000000000, 0.000000000000000000 ) ) ;
#5550 = CARTESIAN_POINT ( 'NONE',  ( 0.6077679335219284829, 0.6189715888181289705, -1.861716921216026055 ) ) ;
#5551 = DIRECTION ( 'NONE',  ( 0.000000000000000000, 1.000000000000000000, 0.000000000000000000 ) ) ;
#5552 = CARTESIAN_POINT ( 'NONE',  ( 4.599240423533799138, 6.388866465587984322, 1.599625672291267398 ) ) ;
#5553 = CARTESIAN_POINT ( 'NONE',  ( -1.734935157289736685, -1.374772708486751593, 1.500000000000001332 ) ) ;
#5554 = VERTEX_POINT ( 'NONE', #31681 ) ;
#5556 =( BOUNDED_CURVE ( )  B_SPLINE_CURVE ( 2, ( #9884, #108526, #26132, #124797, #56515, #92244, #158293, #10936, #143139 ),
 .UNSPECIFIED., .F., .T. ) 
 B_SPLINE_CURVE_WITH_KNOTS ( ( 3, 2, 2, 2, 3 ),
 ( 0.7232142857142856984, 0.7261904761904761640, 0.7321428571428570953, 0.7380952380952381375, 0.7410714285714286031 ),
 .UNSPECIFIED. ) 
 CURVE ( )  GEOMETRIC_REPRESENTATION_ITEM ( )  RATIONAL_B_SPLINE_CURVE ( ( 0.9330127018922194093, 0.9330127018922194093, 1.000000000000000000, 0.8660254037844387076, 1.000000000000000000, 0.8660254037844387076, 1.000000000000000000, 0.9330127018922194093, 0.9330127018922194093 ) ) 
 REPRESENTATION_ITEM ( '' )  );
#5555 = DIRECTION ( 'NONE',  ( 0.000000000000000000, 1.000000000000000000, 0.000000000000000000 ) ) ;
#5557 = ORIENTED_EDGE ( 'NONE', *, *, #174069, .T. ) ;
#5558 = CARTESIAN_POINT ( 'NONE',  ( 3.721195823539941827, 1.555462818066039254, 0.9281401003491447366 ) ) ;
#5559 = VERTEX_POINT ( 'NONE', #210403 ) ;
#5560 = CARTESIAN_POINT ( 'NONE',  ( 10.22692794340986921, 10.82583744360002243, 0.000000000000000000 ) ) ;
#5562 = EDGE_CURVE ( 'NONE', #151754, #8301, #113631, .T. ) ;
#5561 = CARTESIAN_POINT ( 'NONE',  ( 4.248501033035879004, 6.049946853332221153, -1.599625672291273171 ) ) ;
#5563 = CARTESIAN_POINT ( 'NONE',  ( 4.600164522386200439, -0.8494929878282222457, 1.599918020626096782 ) ) ;
#5564 = CARTESIAN_POINT ( 'NONE',  ( 0.4355862708379926174, -6.583980363595115293, 9.606148981167594414 ) ) ;
#5565 = CARTESIAN_POINT ( 'NONE',  ( 5.095443103064356549, 4.909381473188671130, 0.08826871305007774615 ) ) ;
#5566 = CARTESIAN_POINT ( 'NONE',  ( 5.421662447778366811, 6.277071961296246450, 1.037714289653376198 ) ) ;
#5568 = CARTESIAN_POINT ( 'NONE',  ( -0.6823417656250039265, 14.31770833367473195, -1.181850606188755259 ) ) ;
#5567 = CARTESIAN_POINT ( 'NONE',  ( 4.879284944527097601, -0.09183316818502919310, 1.858928597182760711 ) ) ;
#5569 = CARTESIAN_POINT ( 'NONE',  ( 2.759290930233889494, 1.818065234828979637, -0.6036251144310407213 ) ) ;
#5570 = SURFACE_STYLE_USAGE ( .BOTH. , #189686 ) ;
#5571 = CARTESIAN_POINT ( 'NONE',  ( -11.04433755984576848, 5.142917986253679352, 4.203129294766247526 ) ) ;
#5572 = CARTESIAN_POINT ( 'NONE',  ( 1.084637062511528693, 3.242628807292008197, 1.105835307554807301 ) ) ;
#5573 = CARTESIAN_POINT ( 'NONE',  ( 6.925078400183569904, 6.033938712579569597, 2.739235483740619426 ) ) ;
#5574 = CARTESIAN_POINT ( 'NONE',  ( 7.632877294813741109, 8.007371053478589573, 1.040834085586084257E-14 ) ) ;
#5575 = CARTESIAN_POINT ( 'NONE',  ( -3.090368948911150770, 5.692848642783215674, 1.199719254218462483 ) ) ;
#5576 = CARTESIAN_POINT ( 'NONE',  ( 0.07536363704235826688, -0.001874865094115066300, -2.144269471569634877 ) ) ;
#5577 = CARTESIAN_POINT ( 'NONE',  ( 1.183663948672460942, -0.9384196385337481017, 1.868258235111931898 ) ) ;
#5578 = CARTESIAN_POINT ( 'NONE',  ( 6.066347387471824781, 6.042103138330730872, -0.7998128361456481317 ) ) ;
#5579 = CARTESIAN_POINT ( 'NONE',  ( 6.247092716751994068, -1.627016005604764670, 1.031123616215999794 ) ) ;
#5580 = CARTESIAN_POINT ( 'NONE',  ( -4.229253852459088137, 7.021547696922494808, 1.199719254218464037 ) ) ;
#5581 = CARTESIAN_POINT ( 'NONE',  ( 2.555444900642935391, 0.4891320457309326075, -1.758753460580727790 ) ) ;
#5582 = CARTESIAN_POINT ( 'NONE',  ( 11.73212044392280262, 8.686627382477217552, -4.360314433000339385 ) ) ;
#5583 = CARTESIAN_POINT ( 'NONE',  ( 1.740342883905017013, 1.098329146349947827, -1.565357986077076990 ) ) ;
#5584 = CARTESIAN_POINT ( 'NONE',  ( 2.137097444212227693, -0.09349721708603592196, -1.967446466973846952 ) ) ;
#5585 = CARTESIAN_POINT ( 'NONE',  ( 3.966302600639686204, -1.813262256789631266, -0.6959421042645166366 ) ) ;
#5586 = AXIS2_PLACEMENT_3D ( 'NONE', #127407, #77494, #94839 ) ;
#5587 = VERTEX_POINT ( 'NONE', #46877 ) ;
#5588 = CARTESIAN_POINT ( 'NONE',  ( -1.201851678989727383E-14, 3.243750000682814161, 1.732050807568877637 ) ) ;
#5589 = CARTESIAN_POINT ( 'NONE',  ( -5.842637852846353397, 5.781108681267656202, 0.7998128361456281477 ) ) ;
#5591 = CARTESIAN_POINT ( 'NONE',  ( 4.359710196644346780, -1.641147893522959089, -1.343014508298406628 ) ) ;
#5590 = CARTESIAN_POINT ( 'NONE',  ( 4.004454267989866700, 5.765225627445230927, 1.599625672291262513 ) ) ;
#5592 = CARTESIAN_POINT ( 'NONE',  ( 0.4356160240586420263, -9.063431457505059186, -9.626717610576610795 ) ) ;
#5593 = CARTESIAN_POINT ( 'NONE',  ( 9.073431116043567002, 11.60875560684942265, -1.599625672291262513 ) ) ;
#5594 = CARTESIAN_POINT ( 'NONE',  ( -6.473091995881817162, 6.516638514809040217, 0.7998128361456281477 ) ) ;
#5595 = ORIENTED_EDGE ( 'NONE', *, *, #99713, .F. ) ;
#5596 = CARTESIAN_POINT ( 'NONE',  ( 6.658989722967328717, 7.797851427330578566, 1.199719254218452935 ) ) ;
#5597 = FACE_OUTER_BOUND ( 'NONE', #187539, .T. ) ;
#5598 = CARTESIAN_POINT ( 'NONE',  ( 4.213378774425760476, -0.3099129147984269195, 1.799030153321119263 ) ) ;
#5599 = CARTESIAN_POINT ( 'NONE',  ( 0.000000000000000000, 13.49999999999999822, 0.000000000000000000 ) ) ;
#5600 = CARTESIAN_POINT ( 'NONE',  ( -9.815740026613960723, 11.51441345488021106, -1.082531754730539753 ) ) ;
#5601 = CARTESIAN_POINT ( 'NONE',  ( -4.586114404036374381, 8.497146329035404122, -0.08355658565369419866 ) ) ;
#5602 = LINE ( 'NONE', #35998, #143466 ) ;
#5603 = CARTESIAN_POINT ( 'NONE',  ( 4.188257260935820625, -1.850246793840780279, -0.2747695030091561463 ) ) ;
#5604 = CARTESIAN_POINT ( 'NONE',  ( 8.320953590485093088, 10.73086516036454618, 1.599625672291281386 ) ) ;
#5605 = CARTESIAN_POINT ( 'NONE',  ( 2.543477943364984117, -1.427709268621931260, -1.293647605089723429 ) ) ;
#5606 = CARTESIAN_POINT ( 'NONE',  ( 6.491066726104213203, 0.1889763263339637456, 1.952597990788194959 ) ) ;
#5607 = CARTESIAN_POINT ( 'NONE',  ( 1.364683531249997417, 8.546875000341403350, 2.602085213965210642E-15 ) ) ;
#5608 = CARTESIAN_POINT ( 'NONE',  ( -6.847031270101295419, 7.946956888995021728, -1.199719254218446718 ) ) ;
#5609 = CARTESIAN_POINT ( 'NONE',  ( 3.714044015139744914, 6.420469553383295391, 1.199719254218462483 ) ) ;
#5610 = CARTESIAN_POINT ( 'NONE',  ( -5.275531169048909952, 7.248148678680751189, -1.443375672974066548 ) ) ;
#5611 = AXIS2_PLACEMENT_3D ( 'NONE', #38582, #22291, #88404 ) ;
#5612 = CARTESIAN_POINT ( 'NONE',  ( 1.159931391799984279, 1.264437666799199889, 1.698043086552150749 ) ) ;
#5613 = VECTOR ( 'NONE', #152995, 1000.000000000000000 ) ;
#5614 = CARTESIAN_POINT ( 'NONE',  ( 10.40318394038753702, 11.03146944007395724, -0.7998128361456281477 ) ) ;
#5616 = ORIENTED_EDGE ( 'NONE', *, *, #174895, .T. ) ;
#5615 = FACE_OUTER_BOUND ( 'NONE', #172724, .T. ) ;
#5617 = CARTESIAN_POINT ( 'NONE',  ( 4.786024367859083029, -1.269482053145968514, -1.635305934682528717 ) ) ;
#5619 = CARTESIAN_POINT ( 'NONE',  ( 1.364683531249986537, 2.717708333674754062, -0.7879004041258239610 ) ) ;
#5618 = CARTESIAN_POINT ( 'NONE',  ( 0.2218712608162629052, 1.761692264604281633, 0.5354471447000588302 ) ) ;
#5620 = ORIENTED_EDGE ( 'NONE', *, *, #66894, .F. ) ;
#5621 = CARTESIAN_POINT ( 'NONE',  ( 5.485083606918717436, -2.298851034700015727, -0.002838145216723860897 ) ) ;
#5622 = CARTESIAN_POINT ( 'NONE',  ( 7.158341918335438869, 7.453746447587225710, -0.7216878364870257245 ) ) ;
#5623 = CARTESIAN_POINT ( 'NONE',  ( 4.041739190649647817, 6.769093918182960579, -1.082531754730548412 ) ) ;
#5624 = CARTESIAN_POINT ( 'NONE',  ( 0.9379084653730703769, 0.9244841788896654977, -2.097747560502453812 ) ) ;
#5625 = CARTESIAN_POINT ( 'NONE',  ( 7.636191794455520210, -6.027819618361872855, -7.636191794455548632 ) ) ;
#5626 = CARTESIAN_POINT ( 'NONE',  ( -5.586841817283045408, 8.675676665875643678, 1.199719254218454489 ) ) ;
#5627 = CARTESIAN_POINT ( 'NONE',  ( 4.628815217244971691, -1.774851831708891714, 0.7884768782448601243 ) ) ;
#5628 = VERTEX_POINT ( 'NONE', #45808 ) ;
#5629 = CARTESIAN_POINT ( 'NONE',  ( 8.744645890689993095, 9.304434415334227992, -0.7216878364870197293 ) ) ;
#5630 = ORIENTED_EDGE ( 'NONE', *, *, #14825, .T. ) ;
#5631 = CARTESIAN_POINT ( 'NONE',  ( 6.433860211133586304, -1.853236450885078712, 0.4715264990977630077 ) ) ;
#5632 = CARTESIAN_POINT ( 'NONE',  ( 5.665250009225348826, 1.861346387706263261, -0.7762253298396750711 ) ) ;
#5634 = CARTESIAN_POINT ( 'NONE',  ( 11.07123604129543359, 12.30000000000000249, 0.8055550039003240848 ) ) ;
#5633 = CARTESIAN_POINT ( 'NONE',  ( -9.352427035328430449, 9.805586384171650849, 1.040834085586084257E-14 ) ) ;
#5635 = CARTESIAN_POINT ( 'NONE',  ( 1.642778471875001811, -2.530208332855374387, 2.845375778867859751 ) ) ;
#5637 = CARTESIAN_POINT ( 'NONE',  ( 1.234804682044550850, -1.602240143502192238, 0.7520855130052228610 ) ) ;
#5636 = CARTESIAN_POINT ( 'NONE',  ( 3.205106881211945868, -0.4073652088906943858, 2.050380944992454602 ) ) ;
#5638 = CARTESIAN_POINT ( 'NONE',  ( -11.48243876534946217, 13.87999999999998302, 3.199999999999997957 ) ) ;
#5639 = ADVANCED_FACE ( 'NONE', ( #29543 ), #18874, .T. ) ;
#5641 = CARTESIAN_POINT ( 'NONE',  ( 3.679849949768813744, -1.130634651955428671, 1.993948080406320766 ) ) ;
#5640 = CARTESIAN_POINT ( 'NONE',  ( 3.627688620108284745, 6.389997935838436227, 1.199719254218452047 ) ) ;
#5642 = CARTESIAN_POINT ( 'NONE',  ( 2.659766076405935653, -1.200293992427956757, 1.260412480424155435 ) ) ;
#5643 = CARTESIAN_POINT ( 'NONE',  ( 4.379447312414087357, 5.068108938359919158, -1.199719254218452047 ) ) ;
#5644 = CARTESIAN_POINT ( 'NONE',  ( -2.675383846940428967, -0.4458684588859937459, -0.1127173061977598811 ) ) ;
#5645 = CARTESIAN_POINT ( 'NONE',  ( 2.565452462605917638, 1.394811117528846900, -1.029664540377094761 ) ) ;
#5646 = CARTESIAN_POINT ( 'NONE',  ( 2.735037655519993560, -2.077075009683257090, -0.6322084445426826571 ) ) ;
#5647 = CARTESIAN_POINT ( 'NONE',  ( 4.497554271431305040, 6.270232621468402989, -1.599625672291256295 ) ) ;
#5648 = CARTESIAN_POINT ( 'NONE',  ( 5.120327457147888950, 1.987497208294352280, 0.3399611521368098854 ) ) ;
#5650 = AXIS2_PLACEMENT_3D ( 'NONE', #135606, #134562, #118340 ) ;
#5649 = CARTESIAN_POINT ( 'NONE',  ( 2.687500000000001332, -1.451031289061010421, 1.451031289061227136 ) ) ;
#5651 = CARTESIAN_POINT ( 'NONE',  ( -1.499999999999997780, 3.431250000682818602, 1.214306433183764966E-14 ) ) ;
#5652 = CARTESIAN_POINT ( 'NONE',  ( 0.7098319175448050133, -1.917404841279496397, 0.1857973779731073583 ) ) ;
#5653 = CARTESIAN_POINT ( 'NONE',  ( 1.364683531249996529, 15.21354166700806587, 0.7879004041258405033 ) ) ;
#5654 = CARTESIAN_POINT ( 'NONE',  ( 4.342156631555553759, -1.367984123109561301, -1.750111109629876260 ) ) ;
#5655 = ORIENTED_EDGE ( 'NONE', *, *, #51928, .T. ) ;
#5656 = CARTESIAN_POINT ( 'NONE',  ( -0.1110810684432960160, 0.2482034880273851774, -1.831546034005934853 ) ) ;
#5657 = CARTESIAN_POINT ( 'NONE',  ( -1.500000000000001332, -0.09999999999997510880, 0.000000000000000000 ) ) ;
#5658 = CARTESIAN_POINT ( 'NONE',  ( 6.642605195691581699, 9.837124264027149678, 1.199719254218462483 ) ) ;
#5659 = CARTESIAN_POINT ( 'NONE',  ( 6.168596704093459060, 7.259412911939593371, -1.082531754730543083 ) ) ;
#5660 = CARTESIAN_POINT ( 'NONE',  ( 1.642778471875000035, -1.626041666188710044, -2.845375778867859751 ) ) ;
#5661 = CARTESIAN_POINT ( 'NONE',  ( 1.084998894000373637, -1.405142754555653628, 1.720412613360406295 ) ) ;
#5663 = CARTESIAN_POINT ( 'NONE',  ( 5.951606347324344348, 1.484592722905058171, 1.282605414028796353 ) ) ;
#5662 = VECTOR ( 'NONE', #18240, 1000.000000000000000 ) ;
#5664 = CARTESIAN_POINT ( 'NONE',  ( 10.07334494527360569, 10.85458331234846696, 0.000000000000000000 ) ) ;
#5665 = CARTESIAN_POINT ( 'NONE',  ( -1.273593037966616048, 3.712960547652722987, -0.4852599168373451510 ) ) ;
#5666 = CARTESIAN_POINT ( 'NONE',  ( 0.3687372981288695728, -1.412185959430117821, 1.636573055046482983 ) ) ;
#5667 = CARTESIAN_POINT ( 'NONE',  ( -5.234856708652269042, 7.200695141551334721, 1.443375672974058777 ) ) ;
#5668 = CARTESIAN_POINT ( 'NONE',  ( 3.385269252200762580, 0.04793456357342047724, 2.062272590435239028 ) ) ;
#5669 = CARTESIAN_POINT ( 'NONE',  ( -5.915435094264120508, 5.795762452929912101, 0.000000000000000000 ) ) ;
#5670 = ADVANCED_FACE ( 'NONE', ( #74704 ), #73631, .T. ) ;
#5671 = CARTESIAN_POINT ( 'NONE',  ( 1.499999999999987121, 2.327083334016154303, -0.8660254037844262731 ) ) ;
#5672 = CARTESIAN_POINT ( 'NONE',  ( 1.364683531249986537, -1.136458332991912235, 0.7879004041258500513 ) ) ;
#5673 = CARTESIAN_POINT ( 'NONE',  ( 5.079306140367803479, 1.745876537259077432, -0.6719496041647440299 ) ) ;
#5674 = CARTESIAN_POINT ( 'NONE',  ( 3.726996057929339745, 1.726255173046949309, 0.1649803145151728934 ) ) ;
#5675 = CARTESIAN_POINT ( 'NONE',  ( 3.772797691900576567, 1.637269354731695881, -0.5906731273508105673 ) ) ;
#5676 = CARTESIAN_POINT ( 'NONE',  ( 1.259778491951433654, 2.257442302724984806, -0.3979086512072607107 ) ) ;
#5677 = CARTESIAN_POINT ( 'NONE',  ( 0.6823417656249917140, 4.155208333674755394, 1.181850606188765695 ) ) ;
#5678 = CARTESIAN_POINT ( 'NONE',  ( 4.933190498422773018, -1.479524406611672394, -1.477502780037798447 ) ) ;
#5679 = CARTESIAN_POINT ( 'NONE',  ( 6.667919370488161412, -1.192936252400189190, 1.533121312111614065 ) ) ;
#5680 = AXIS2_PLACEMENT_3D ( 'NONE', #105900, #24587, #126455 ) ;
#5682 = ORIENTED_EDGE ( 'NONE', *, *, #30234, .F. ) ;
#5681 = CARTESIAN_POINT ( 'NONE',  ( 0.3553982319964839043, -6.532648833121156962, 9.473247973006321487 ) ) ;
#5683 = CARTESIAN_POINT ( 'NONE',  ( 0.7916389524552720491, 1.525042296397002284, -1.319230309296010928 ) ) ;
#5684 = CARTESIAN_POINT ( 'NONE',  ( 0.7562902151678205787, 0.8540304730459827853, -1.941197329821432227 ) ) ;
#5685 = CARTESIAN_POINT ( 'NONE',  ( -5.204170427930421283E-15, -8.763419982614969683, 10.56339547890107688 ) ) ;
#5686 = CARTESIAN_POINT ( 'NONE',  ( 9.220166054920730048, 13.21238179712012517, -9.025879716107306550 ) ) ;
#5687 = CARTESIAN_POINT ( 'NONE',  ( -7.018317073368468328, 11.33978701890523233, -0.7998128361456291469 ) ) ;
#5688 = CARTESIAN_POINT ( 'NONE',  ( 5.307127064745490230, 8.279066444590018392, -1.199719254218452935 ) ) ;
#5689 = CARTESIAN_POINT ( 'NONE',  ( 2.139458383197485603, 0.002846582261652879763, 2.120667954922689002 ) ) ;
#5690 = DIRECTION ( 'NONE',  ( 0.000000000000000000, 1.000000000000000000, 0.000000000000000000 ) ) ;
#5691 = CARTESIAN_POINT ( 'NONE',  ( 4.353998665852670591, 1.825246345946249571, -0.04724550102237072557 ) ) ;
#5692 = ORIENTED_EDGE ( 'NONE', *, *, #107653, .F. ) ;
#5693 = CARTESIAN_POINT ( 'NONE',  ( -6.794571259104023930, 7.956029886156682274, 1.199719254218452047 ) ) ;
#5694 = CARTESIAN_POINT ( 'NONE',  ( -0.01138762994425885841, -7.792108994756149265, -9.500479199177400247 ) ) ;
#5695 = CARTESIAN_POINT ( 'NONE',  ( 6.821160681006781523, 9.051383109298340557, 1.443375672974063439 ) ) ;
#5696 = CARTESIAN_POINT ( 'NONE',  ( 0.000000000000000000, -0.2843749995220433702, -3.793834371823813001 ) ) ;
#5697 = CARTESIAN_POINT ( 'NONE',  ( -8.030507057996002729, 8.263346410617135263, 1.040834085586084257E-14 ) ) ;
#5698 = CARTESIAN_POINT ( 'NONE',  ( 1.881123716185427286, -1.848401041775033171, -0.8146170886813360879 ) ) ;
#5699 = CARTESIAN_POINT ( 'NONE',  ( 5.104599427727727345, -0.7392731805347593221, -2.079399364341961487 ) ) ;
#5700 = CARTESIAN_POINT ( 'NONE',  ( -5.320648938720212051, 5.172121614787156929, 0.000000000000000000 ) ) ;
#5701 = CARTESIAN_POINT ( 'NONE',  ( 4.047575586610673071, 1.345269348194571668, 1.286062638920927537 ) ) ;
#5702 = CARTESIAN_POINT ( 'NONE',  ( 7.716561984472250835, 12.15440608185967086, 1.040834085586084257E-14 ) ) ;
#5703 = CARTESIAN_POINT ( 'NONE',  ( 5.885648082108199119, 6.999582529615296700, 1.082531754730549967 ) ) ;
#5704 = EDGE_LOOP ( 'NONE', ( #210630, #106119, #15688, #178224 ) ) ;
#5705 = CARTESIAN_POINT ( 'NONE',  ( -4.765854690403601879, 5.518917546014321829, 1.199719254218462483 ) ) ;
#5706 = CARTESIAN_POINT ( 'NONE',  ( -8.350932551013499960, 11.83017284523606172, -1.199719254218446718 ) ) ;
#5707 = CARTESIAN_POINT ( 'NONE',  ( 4.600122369450095228, -1.825375079466069694, -0.04201004182294298950 ) ) ;
#5709 = CARTESIAN_POINT ( 'NONE',  ( -4.002915605954192380, 7.811702849818844108, -0.3674259761444337302 ) ) ;
#5708 = CARTESIAN_POINT ( 'NONE',  ( -4.625266680917477835, 5.425174544939014964, -1.199719254218453823 ) ) ;
#5710 = CARTESIAN_POINT ( 'NONE',  ( 5.300918301777743480, 7.749796750553542779, -1.302405036909856761 ) ) ;
#5711 = CARTESIAN_POINT ( 'NONE',  ( 0.5437846328400409712, 1.620832503561630666, -0.6162787013818531445 ) ) ;
#5712 = CARTESIAN_POINT ( 'NONE',  ( 0.6557207866510657013, -1.263530833501663952, 1.197007909421362370 ) ) ;
#5713 = CARTESIAN_POINT ( 'NONE',  ( 5.918676688095830585, 1.554283316268306292, -1.705954940095489203 ) ) ;
#5714 = CARTESIAN_POINT ( 'NONE',  ( 5.123001941117305336, 7.070197912760590064, 1.599625672291268286 ) ) ;
#5715 = CARTESIAN_POINT ( 'NONE',  ( 1.827488212121135769, -1.941439008138484246, 0.6915448510415463934 ) ) ;
#5716 = CARTESIAN_POINT ( 'NONE',  ( 6.993308306550549247, 7.053281200597435685, 1.040834085586084257E-14 ) ) ;
#5717 = EDGE_CURVE ( 'NONE', #200740, #3699, #112531, .T. ) ;
#5718 = CARTESIAN_POINT ( 'NONE',  ( 0.3509351863830567075, -0.9528684895154272416, 1.776737725368633614 ) ) ;
#5719 = CARTESIAN_POINT ( 'NONE',  ( 5.905025204062885003, 4.805319369733568102, 2.500000000000011102 ) ) ;
#5720 = CARTESIAN_POINT ( 'NONE',  ( -7.123883369337781879, 7.275895117174344229, 0.7998128361456341429 ) ) ;
#5721 = CARTESIAN_POINT ( 'NONE',  ( 5.647288160985431738, -1.475499438119257878, -1.149758287351684949 ) ) ;
#5723 = CARTESIAN_POINT ( 'NONE',  ( -3.902768115887413014, 5.646591783325653147, -1.599625672291283607 ) ) ;
#5722 = CARTESIAN_POINT ( 'NONE',  ( 3.269685606991072468, 0.4601866041431811327, -1.856093204100267124 ) ) ;
#5724 = CARTESIAN_POINT ( 'NONE',  ( 5.268293329372571776, 1.085216321637239023, 1.921556908365213312 ) ) ;
#5725 = CARTESIAN_POINT ( 'NONE',  ( -1.225000000000038058, 1.333333334016162386, 0.7072540797572777205 ) ) ;
#5726 = CARTESIAN_POINT ( 'NONE',  ( 4.692530564105613422, 7.528350520548263702, -1.082531754730548412 ) ) ;
#5727 = CARTESIAN_POINT ( 'NONE',  ( 5.546694241322223107, 5.643767167730274537, -0.7216878364870458196 ) ) ;
#5728 = CARTESIAN_POINT ( 'NONE',  ( -5.112833325684920993, 6.097965313788082931, -1.082531754730549967 ) ) ;
#5729 = CARTESIAN_POINT ( 'NONE',  ( 5.813165546740090228, 1.733599321496303691, -1.220823391460408303 ) ) ;
#5730 = CARTESIAN_POINT ( 'NONE',  ( 1.993646994336109257, 2.007229749184535450, -1.138263614794749801 ) ) ;
#5731 = CARTESIAN_POINT ( 'NONE',  ( 3.683996026499200660, -1.166640140252427793, -1.577160851978461009 ) ) ;
#5732 = CARTESIAN_POINT ( 'NONE',  ( 7.019253602638882761, -7.126685749119995528, 7.019253602638860556 ) ) ;
#5733 = CARTESIAN_POINT ( 'NONE',  ( 0.7956631384608278124, -1.383255022760669251, -1.391342014947573924 ) ) ;
#5734 = PLANE ( 'NONE',  #209870 ) ;
#5735 = CARTESIAN_POINT ( 'NONE',  ( 5.174371902270911150, 6.065797303184739420, 1.199719254218452047 ) ) ;
#5736 = ORIENTED_EDGE ( 'NONE', *, *, #67524, .T. ) ;
#5737 = CARTESIAN_POINT ( 'NONE',  ( 6.262907710099243630, -0.1037740067610822270, -2.014008436551452785 ) ) ;
#5738 =( BOUNDED_SURFACE ( )  B_SPLINE_SURFACE ( 1, 2, ( 
 ( #81026, #99416, #83145, #798, #64770, #15996, #197961, #133011, #49590, #165470, #130912, #116782, #101542, #182779, #17066, #34397, #18132, #134080, #200088, #117860, #183852, #35464, #39750, #85288, #208365, #126149, #201149, #154573, #151374, #153503, #204342, #6149, #92533, #38683, #175902, #5073, #71148, #169739, #26421, #2943, #137265, #21328, #86360, #168672, #174844, #192112, #37609, #202212, #203285, #105855, #158573, #185976, #59996, #87435, #20276, #188119, #69015, #4010, #10172, #53866, #54932, #142355, #76246, #43776, #72219, #109889, #135132, #138326, #119999, #56000, #121084, #52787, #118926, #184906, #88511, #36530, #152431, #122151, #102617, #187051, #104762, #170811, #22402, #70080, #136194, #103690, #61067, #147663, #46972, #209422, #144498, #143426, #110949, #146613, #211564, #63198, #195340, #113088, #127226, #159637, #162848, #179094, #112026, #77313, #196404, #161783, #30716, #93593, #45908, #212631, #15492, #114162, #145565, #12297, #14426, #78377, #176956, #193195, #178028, #27493, #44843, #28572, #31781, #94660, #131452, #130417, #81580, #210505, #29646, #95731, #129362, #64272, #96799, #160703, #11234, #62140, #128300, #194262, #13374, #79448, #80516, #48049, #180155, #97853, #163916, #115214, #213680, #65303, #197453, #49094, #199575, #136742, #181204, #149790, #3496, #70631, #51219, #1364, #66361, #54419, #202769, #148720, #103165, #183340, #119478, #67426, #32832, #98909, #134631, #290, #169226, #168166, #167108, #133569, #20818, #86914, #164961, #118412, #68503, #16553, #132507, #152982, #4557, #50150, #85846, #82636, #198506, #116274, #185466, #182263, #150864, #184397, #36017, #33888, #117343, #34945, #102096, #101017, #18695, #99966, #19764, #166031, #151923, #84777, #52283, #2426, #200635, #69566, #17616, #37086, #135676, #201701, #53344, #83702, #21874, #122715, #156198, #170286, #92284, #157263, #104240, #74933, #186538, #87981, #38167, #71703, #40311, #141043, #190796, #5622, #139960, #124829, #42456, #137815, #188677, #121633, #154055, #203834, #55480, #106418, #187602, #171358, #39229, #90131, #108564, #205983, #174592, #75996, #73865, #158329, #25100, #138883, #58682, #204901, #26166, #173527, #9922, #57619, #105321, #7774, #123776, #56555, #189736, #6706, #22952, #89066, #172441, #41388, #155124, #142101, #24028, #8854, #72783, #120560, #208114, #207050, #107499, #91202, #210243, #78120, #95481, #96543, #13114, #60809, #191860, #159377, #125902, #93341, #160445, #44584, #12052, #176697, #175647, #126970, #61879, #147405, #110697, #109644, #28310, #195079, #14164, #59743, #179901, #97598, #27233, #129105, #43521, #128044, #178846, #46717, #64012, #79192, #10976, #193999, #45648, #144250, #212371, #77049, #111765, #177772, #192928, #143179, #146358, #163657, #29387, #94406, #161529, #80259, #130160, #145307, #31524, #211312, #209171, #162590, #62937, #112830, #196152, #30457, #47792, #113906, #15239, #81326, #134377, #119216, #65054, #200381, #33634, #118155, #1112, #131210, #185199, #180951, #2166, #213431, #39, #52029, #167906, #67173, #18441, #149526, #117083, #36824, #32574, #184139, #98650, #102905, #84518, #164707, #116017, #114951, #82380, #35763, #183082, #34694, #166845, #150606, #16295, #197198, #101838, #68243, #83446, #48837, #19504, #133308, #85580, #148471, #17362, #151670, #201440, #3241, #100763, #198253, #69307, #49893, #66103, #132245, #199313, #182003, #99707, #165779, #135419, #50959, #168964, #53081, #20568, #86651, #4301, #54159, #70372, #103983, #72522, #173260, #8592, #37907, #172183, #157006, #74674, #170026, #154862, #153793, #136487, #120298, #202509, #6444, #186271, #203574, #21612, #122452, #140777, #23773, #206792, #108309, #106157, #190538, #57357, #171099, #90940, #22690, #58424, #205722, #124577, #89878, #137556, #40048, #155930, #88803, #7515, #38975, #87720, #5362, #138618, #73597, #71444, #42194, #204641, #41127, #55225, #152719, #107239, #174329, #121371, #187346, #56292, #25905, #105061, #188411, #189484, #139699, #123520, #24841, #191599, #179643, #195887, #59481, #13910, #94147, #30186, #192664, #92015, #9661, #45387 ),
 ( #175386, #211043, #158073, #125638, #113638, #96276, #75737, #61616, #29121, #161257, #26972, #110440, #44318, #12844, #176442, #11787, #43261, #95208, #47525, #78918, #77861, #177509, #143984, #209975, #127786, #142911, #162326, #60545, #126703, #145040, #141850, #207855, #160186, #193741, #109379, #79992, #62669, #111503, #28054, #146096, #212107, #93077, #128828, #194810, #159119, #10720, #63744, #129903, #76789, #46446, #208911, #112567, #178578, #183892, #118965, #844, #182823, #100512, #180693, #49628, #198002, #166587, #131993, #165512, #196943, #34439, #201189, #18176, #17104, #116821, #83182, #149265, #66909, #82120, #101581, #214215, #65844, #84263, #31263, #147152, #33374, #133049, #81066, #2987, #67977, #14969, #200129, #97337, #213177, #163395, #48583, #199051, #51782, #167649, #130953, #50697, #35504, #19250, #114699, #99455, #32318, #64806, #98386, #164450, #150348, #16037, #148213, #115753, #1918, #85330, #134120, #151413, #52828, #117899, #69054, #135174, #181744, #123273, #203322, #106979, #23518, #173004, #56040, #169779, #72259, #204384, #54973, #122196, #71188, #20317, #4050, #170849, #138367, #36570, #40874, #187089, #73334, #87476, #184943, #139437, #189235, #21368, #86403, #121125, #140528, #102656, #153542, #7258, #74428, #38723, #5111, #70120, #58170, #206540, #152470, #24585, #104804, #90692, #137305, #168713, #136231, #188158, #202254, #53905, #120040, #186014, #156754, #37650, #154611, #39791, #105898, #103728, #22439, #88550, #6190, #8343, #171922, #89624, #155676, #205472, #57104, #28873, #193503, #128594, #77613, #211865, #192416, #44071, #208664, #62431, #124328, #110190, #60295, #125383, #207606, #210806, #162081, #76543, #26727, #176200, #144799, #78673, #10469, #29945, #126453, #59225, #12601, #190288, #43014, #194560, #92829, #27801, #178336, #46205, #13670, #45144, #96030, #41945, #111256, #158873, #94958, #93899, #108058, #79742, #91765, #127531, #174083, #191349, #177259, #112321, #159938, #143736, #11543, #209730, #145859, #157821, #161006, #9417, #25655, #61373, #75488, #142654, #141599, #109127, #175141, #33127, #99207, #16849, #82932, #97093, #195642, #198795, #149005, #147960, #113390, #17910, #197747, #581, #129658, #81876, #182556, #51514, #150085, #181499, #48340, #50444, #114451, #146912, #163146, #213973, #63504, #14730, #80822, #67713, #212930, #167394, #166321, #117639, #32067, #65593, #131742, #165256, #100252, #66647, #64566, #47278, #130709, #179399, #196700, #164203, #180450, #98156, #34180, #31019, #15790, #85066, #1656, #151152, #132792, #116563, #83996, #133864, #49385, #115504, #183631, #199871, #35238, #101313, #18985, #172737, #154342, #137032, #88277, #203059, #120852, #38456, #53635, #73068, #185748, #37381, #204114, #90419, #118699, #4842, #104533, #52568, #188964, #39519, #200920, #171648, #68793, #184685, #134913, #168451, #54702, #23245, #139167, #102384, #22162, #6988, #205198, #20050, #70921, #3779, #36305, #86138, #152209, #186826, #69853, #119768, #135963, #170579, #56839, #5920, #123012, #24313, #71992, #40606, #121924, #21099, #155405, #87202, #106711, #55766, #2721, #138104, #201979, #187891, #105619, #153267, #89357, #103456, #169518, #190032, #142397, #43818, #8077, #12340, #158617, #44887, #58974, #156488, #110993, #160745, #141340, #57903, #174886, #112069, #74165, #125129, #193240, #45949, #26466, #191087, #41685, #29688, #178070, #124067, #78420, #10214, #94704, #42756, #140258, #206280, #109933, #107796, #144542, #143469, #208405, #108860, #210549, #62185, #173821, #93633, #175942, #25399, #91499, #128342, #194308, #157560, #76288, #60039, #92575, #9153, #75230, #126192, #192155, #207354, #27538, #28614, #159675, #11277, #77356, #209466, #176998, #61109, #127269, #4332, #180201, #179137, #201471, #186303, #14470, #102938, #212672, #97899, #152750, #119247, #136520, #19537, #70401, #161828, #85614, #130458, #3271, #163958, #13415, #202538, #63241, #98953, #95771, #96840, #151702, #53114, #15536, #115256, #31823, #213723, #54187, #129403, #69338, #195383, #120327, #181249, #47015, #64313, #211605, #30760, #135449, #65346, #131493 ) ),
 .UNSPECIFIED., .F., .F., .T. ) 
 B_SPLINE_SURFACE_WITH_KNOTS ( ( 2, 2 ),
 ( 3, 2, 2, 2, 2, 2, 2, 2, 2, 2, 2, 2, 2, 2, 2, 2, 2, 2, 2, 2, 2, 2, 2, 2, 2, 2, 2, 2, 2, 2, 2, 2, 2, 2, 2, 2, 2, 2, 2, 2, 2, 2, 2, 2, 2, 2, 2, 2, 2, 2, 2, 2, 2, 2, 2, 2, 2, 2, 2, 2, 2, 2, 2, 2, 2, 2, 2, 2, 2, 2, 2, 2, 2, 2, 2, 2, 2, 2, 2, 2, 2, 2, 2, 2, 2, 2, 2, 2, 2, 2, 2, 2, 2, 2, 2, 2, 2, 2, 2, 2, 2, 2, 2, 2, 2, 2, 2, 2, 2, 2, 2, 2, 2, 2, 2, 2, 2, 2, 2, 2, 2, 2, 2, 2, 2, 2, 2, 2, 2, 2, 2, 2, 2, 2, 2, 2, 2, 2, 2, 2, 2, 2, 2, 2, 2, 2, 2, 2, 2, 2, 2, 2, 2, 2, 2, 2, 2, 2, 2, 2, 2, 2, 2, 2, 2, 2, 2, 2, 2, 2, 2, 2, 2, 2, 2, 2, 2, 2, 2, 2, 2, 2, 2, 2, 2, 2, 2, 2, 2, 2, 2, 2, 2, 2, 2, 2, 2, 2, 2, 2, 2, 2, 2, 2, 2, 2, 2, 2, 2, 2, 2, 2, 2, 2, 2, 2, 2, 2, 2, 2, 2, 2, 2, 2, 2, 2, 2, 2, 2, 2, 2, 2, 2, 2, 2, 2, 2, 2, 2, 2, 3 ),
 ( 0.000000000000000000, 1.000000000000000000 ),
 ( 0.000000000000000000, 0.004166666666666666609, 0.008333333333333333218, 0.01250000000000000069, 0.01666666666666666644, 0.02083333333333333218, 0.02500000000000000139, 0.02916666666666666713, 0.03333333333333333287, 0.03749999999999999861, 0.04166666666666666435, 0.04583333333333333010, 0.05000000000000000278, 0.05416666666666666852, 0.05833333333333333426, 0.06250000000000000000, 0.06666666666666666574, 0.07083333333333333148, 0.07499999999999999722, 0.07916666666666666297, 0.08333333333333332871, 0.08749999999999999445, 0.09166666666666666019, 0.09583333333333333981, 0.1000000000000000056, 0.1041666666666666713, 0.1083333333333333370, 0.1125000000000000028, 0.1166666666666666685, 0.1208333333333333343, 0.1250000000000000000, 0.1291666666666666796, 0.1333333333333333315, 0.1375000000000000111, 0.1416666666666666630, 0.1458333333333333426, 0.1499999999999999944, 0.1541666666666666741, 0.1583333333333333259, 0.1625000000000000056, 0.1666666666666666574, 0.1708333333333333370, 0.1749999999999999889, 0.1791666666666666685, 0.1833333333333333204, 0.1875000000000000000, 0.1916666666666666796, 0.1958333333333333315, 0.2000000000000000111, 0.2041666666666666630, 0.2083333333333333426, 0.2124999999999999944, 0.2166666666666666741, 0.2208333333333333259, 0.2250000000000000056, 0.2291666666666666574, 0.2333333333333333370, 0.2374999999999999889, 0.2416666666666666685, 0.2458333333333333204, 0.2500000000000000000, 0.2541666666666666519, 0.2583333333333333592, 0.2625000000000000111, 0.2666666666666666630, 0.2708333333333333148, 0.2750000000000000222, 0.2791666666666666741, 0.2833333333333333259, 0.2874999999999999778, 0.2916666666666666852, 0.2958333333333333370, 0.2999999999999999889, 0.3041666666666666408, 0.3083333333333333481, 0.3125000000000000000, 0.3166666666666666519, 0.3208333333333333592, 0.3250000000000000111, 0.3291666666666666630, 0.3333333333333333148, 0.3375000000000000222, 0.3416666666666666741, 0.3458333333333333259, 0.3499999999999999778, 0.3541666666666666852, 0.3583333333333333370, 0.3624999999999999889, 0.3666666666666666408, 0.3708333333333333481, 0.3750000000000000000, 0.3791666666666666519, 0.3833333333333333592, 0.3875000000000000111, 0.3916666666666666630, 0.3958333333333333148, 0.4000000000000000222, 0.4041666666666666741, 0.4083333333333333259, 0.4124999999999999778, 0.4166666666666666852, 0.4208333333333333370, 0.4249999999999999889, 0.4291666666666666408, 0.4333333333333333481, 0.4375000000000000000, 0.4416666666666666519, 0.4458333333333333592, 0.4500000000000000111, 0.4541666666666666630, 0.4583333333333333148, 0.4625000000000000222, 0.4666666666666666741, 0.4708333333333333259, 0.4749999999999999778, 0.4791666666666666852, 0.4833333333333333370, 0.4874999999999999889, 0.4916666666666666408, 0.4958333333333333481, 0.5000000000000000000, 0.5041666666666666519, 0.5083333333333333037, 0.5124999999999999556, 0.5166666666666667185, 0.5208333333333333703, 0.5250000000000000222, 0.5291666666666666741, 0.5333333333333333259, 0.5374999999999999778, 0.5416666666666666297, 0.5458333333333332815, 0.5500000000000000444, 0.5541666666666666963, 0.5583333333333333481, 0.5625000000000000000, 0.5666666666666666519, 0.5708333333333333037, 0.5749999999999999556, 0.5791666666666667185, 0.5833333333333333703, 0.5875000000000000222, 0.5916666666666666741, 0.5958333333333333259, 0.5999999999999999778, 0.6041666666666666297, 0.6083333333333332815, 0.6125000000000000444, 0.6166666666666666963, 0.6208333333333333481, 0.6250000000000000000, 0.6291666666666666519, 0.6333333333333333037, 0.6374999999999999556, 0.6416666666666667185, 0.6458333333333333703, 0.6500000000000000222, 0.6541666666666666741, 0.6583333333333333259, 0.6624999999999999778, 0.6666666666666666297, 0.6708333333333332815, 0.6750000000000000444, 0.6791666666666666963, 0.6833333333333333481, 0.6875000000000000000, 0.6916666666666666519, 0.6958333333333333037, 0.6999999999999999556, 0.7041666666666667185, 0.7083333333333333703, 0.7125000000000000222, 0.7166666666666666741, 0.7208333333333333259, 0.7249999999999999778, 0.7291666666666666297, 0.7333333333333332815, 0.7375000000000000444, 0.7416666666666666963, 0.7458333333333333481, 0.7500000000000000000, 0.7541666666666666519, 0.7583333333333333037, 0.7624999999999999556, 0.7666666666666667185, 0.7708333333333333703, 0.7750000000000000222, 0.7791666666666666741, 0.7833333333333333259, 0.7874999999999999778, 0.7916666666666666297, 0.7958333333333332815, 0.8000000000000000444, 0.8041666666666666963, 0.8083333333333333481, 0.8125000000000000000, 0.8166666666666666519, 0.8208333333333333037, 0.8249999999999999556, 0.8291666666666667185, 0.8333333333333333703, 0.8375000000000000222, 0.8416666666666666741, 0.8458333333333333259, 0.8499999999999999778, 0.8541666666666666297, 0.8583333333333332815, 0.8625000000000000444, 0.8666666666666666963, 0.8708333333333333481, 0.8750000000000000000, 0.8791666666666666519, 0.8833333333333333037, 0.8874999999999999556, 0.8916666666666667185, 0.8958333333333333703, 0.9000000000000000222, 0.9041666666666666741, 0.9083333333333333259, 0.9124999999999999778, 0.9166666666666666297, 0.9208333333333332815, 0.9250000000000000444, 0.9291666666666666963, 0.9333333333333333481, 0.9375000000000000000, 0.9416666666666666519, 0.9458333333333333037, 0.9499999999999999556, 0.9541666666666667185, 0.9583333333333333703, 0.9625000000000000222, 0.9666666666666666741, 0.9708333333333333259, 0.9749999999999999778, 0.9791666666666666297, 0.9833333333333332815, 0.9875000000000000444, 0.9916666666666666963, 0.9958333333333333481, 1.000000000000000000 ),
 .UNSPECIFIED. ) 
 GEOMETRIC_REPRESENTATION_ITEM ( )  RATIONAL_B_SPLINE_SURFACE ( (
 ( 1.000000000000000000, 0.8660254037844387076, 1.000000000000000000, 0.8660254037844387076, 1.000000000000000000, 0.8660254037844387076, 1.000000000000000000, 0.8660254037844387076, 1.000000000000000000, 0.8660254037844387076, 1.000000000000000000, 0.8660254037844387076, 1.000000000000000000, 0.8660254037844387076, 1.000000000000000000, 0.8660254037844387076, 1.000000000000000000, 0.8660254037844387076, 1.000000000000000000, 0.8660254037844387076, 1.000000000000000000, 0.8660254037844387076, 1.000000000000000000, 0.8660254037844387076, 1.000000000000000000, 0.8660254037844387076, 1.000000000000000000, 0.8660254037844387076, 1.000000000000000000, 0.8660254037844387076, 1.000000000000000000, 0.8660254037844387076, 1.000000000000000000, 0.8660254037844387076, 1.000000000000000000, 0.8660254037844387076, 1.000000000000000000, 0.8660254037844387076, 1.000000000000000000, 0.8660254037844387076, 1.000000000000000000, 0.8660254037844387076, 1.000000000000000000, 0.8660254037844387076, 1.000000000000000000, 0.8660254037844387076, 1.000000000000000000, 0.8660254037844387076, 1.000000000000000000, 0.8660254037844387076, 1.000000000000000000, 0.8660254037844387076, 1.000000000000000000, 0.8660254037844387076, 1.000000000000000000, 0.8660254037844387076, 1.000000000000000000, 0.8660254037844387076, 1.000000000000000000, 0.8660254037844387076, 1.000000000000000000, 0.8660254037844387076, 1.000000000000000000, 0.8660254037844387076, 1.000000000000000000, 0.8660254037844387076, 1.000000000000000000, 0.8660254037844387076, 1.000000000000000000, 0.8660254037844387076, 1.000000000000000000, 0.8660254037844387076, 1.000000000000000000, 0.8660254037844387076, 1.000000000000000000, 0.8660254037844387076, 1.000000000000000000, 0.8660254037844387076, 1.000000000000000000, 0.8660254037844387076, 1.000000000000000000, 0.8660254037844387076, 1.000000000000000000, 0.8660254037844387076, 1.000000000000000000, 0.8660254037844387076, 1.000000000000000000, 0.8660254037844387076, 1.000000000000000000, 0.8660254037844387076, 1.000000000000000000, 0.8660254037844387076, 1.000000000000000000, 0.8660254037844387076, 1.000000000000000000, 0.8660254037844387076, 1.000000000000000000, 0.8660254037844387076, 1.000000000000000000, 0.8660254037844387076, 1.000000000000000000, 0.8660254037844387076, 1.000000000000000000, 0.8660254037844387076, 1.000000000000000000, 0.8660254037844387076, 1.000000000000000000, 0.8660254037844387076, 1.000000000000000000, 0.8660254037844387076, 1.000000000000000000, 0.8660254037844387076, 1.000000000000000000, 0.8660254037844387076, 1.000000000000000000, 0.8660254037844387076, 1.000000000000000000, 0.8660254037844387076, 1.000000000000000000, 0.8660254037844387076, 1.000000000000000000, 0.8660254037844387076, 1.000000000000000000, 0.8660254037844387076, 1.000000000000000000, 0.8660254037844387076, 1.000000000000000000, 0.8660254037844387076, 1.000000000000000000, 0.8660254037844387076, 1.000000000000000000, 0.8660254037844387076, 1.000000000000000000, 0.8660254037844387076, 1.000000000000000000, 0.8660254037844387076, 1.000000000000000000, 0.8660254037844387076, 1.000000000000000000, 0.8660254037844387076, 1.000000000000000000, 0.8660254037844387076, 1.000000000000000000, 0.8660254037844387076, 1.000000000000000000, 0.8660254037844387076, 1.000000000000000000, 0.8660254037844387076, 1.000000000000000000, 0.8660254037844387076, 1.000000000000000000, 0.8660254037844387076, 1.000000000000000000, 0.8660254037844387076, 1.000000000000000000, 0.8660254037844387076, 1.000000000000000000, 0.8660254037844387076, 1.000000000000000000, 0.8660254037844387076, 1.000000000000000000, 0.8660254037844387076, 1.000000000000000000, 0.8660254037844387076, 1.000000000000000000, 0.8660254037844387076, 1.000000000000000000, 0.8660254037844387076, 1.000000000000000000, 0.8660254037844387076, 1.000000000000000000, 0.8660254037844387076, 1.000000000000000000, 0.8660254037844387076, 1.000000000000000000, 0.8660254037844387076, 1.000000000000000000, 0.8660254037844387076, 1.000000000000000000, 0.8660254037844387076, 1.000000000000000000, 0.8660254037844387076, 1.000000000000000000, 0.8660254037844387076, 1.000000000000000000, 0.8660254037844387076, 1.000000000000000000, 0.8660254037844387076, 1.000000000000000000, 0.8660254037844387076, 1.000000000000000000, 0.8660254037844387076, 1.000000000000000000, 0.8660254037844387076, 1.000000000000000000, 0.8660254037844387076, 1.000000000000000000, 0.8660254037844387076, 1.000000000000000000, 0.8660254037844387076, 1.000000000000000000, 0.8660254037844387076, 1.000000000000000000, 0.8660254037844387076, 1.000000000000000000, 0.8660254037844387076, 1.000000000000000000, 0.8660254037844387076, 1.000000000000000000, 0.8660254037844387076, 1.000000000000000000, 0.8660254037844387076, 1.000000000000000000, 0.8660254037844387076, 1.000000000000000000, 0.8660254037844387076, 1.000000000000000000, 0.8660254037844387076, 1.000000000000000000, 0.8660254037844387076, 1.000000000000000000, 0.8660254037844387076, 1.000000000000000000, 0.8660254037844387076, 1.000000000000000000, 0.8660254037844387076, 1.000000000000000000, 0.8660254037844387076, 1.000000000000000000, 0.8660254037844387076, 1.000000000000000000, 0.8660254037844387076, 1.000000000000000000, 0.8660254037844387076, 1.000000000000000000, 0.8660254037844387076, 1.000000000000000000, 0.8660254037844387076, 1.000000000000000000, 0.8660254037844387076, 1.000000000000000000, 0.8660254037844387076, 1.000000000000000000, 0.8660254037844387076, 1.000000000000000000, 0.8660254037844387076, 1.000000000000000000, 0.8660254037844387076, 1.000000000000000000, 0.8660254037844387076, 1.000000000000000000, 0.8660254037844387076, 1.000000000000000000, 0.8660254037844387076, 1.000000000000000000, 0.8660254037844387076, 1.000000000000000000, 0.8660254037844387076, 1.000000000000000000, 0.8660254037844387076, 1.000000000000000000, 0.8660254037844387076, 1.000000000000000000, 0.8660254037844387076, 1.000000000000000000, 0.8660254037844387076, 1.000000000000000000, 0.8660254037844387076, 1.000000000000000000, 0.8660254037844387076, 1.000000000000000000, 0.8660254037844387076, 1.000000000000000000, 0.8660254037844387076, 1.000000000000000000, 0.8660254037844387076, 1.000000000000000000, 0.8660254037844387076, 1.000000000000000000, 0.8660254037844387076, 1.000000000000000000, 0.8660254037844387076, 1.000000000000000000, 0.8660254037844387076, 1.000000000000000000, 0.8660254037844387076, 1.000000000000000000, 0.8660254037844387076, 1.000000000000000000, 0.8660254037844387076, 1.000000000000000000, 0.8660254037844387076, 1.000000000000000000, 0.8660254037844387076, 1.000000000000000000, 0.8660254037844387076, 1.000000000000000000, 0.8660254037844387076, 1.000000000000000000, 0.8660254037844387076, 1.000000000000000000, 0.8660254037844387076, 1.000000000000000000, 0.8660254037844387076, 1.000000000000000000, 0.8660254037844387076, 1.000000000000000000, 0.8660254037844387076, 1.000000000000000000, 0.8660254037844387076, 1.000000000000000000, 0.8660254037844387076, 1.000000000000000000, 0.8660254037844387076, 1.000000000000000000, 0.8660254037844387076, 1.000000000000000000, 0.8660254037844387076, 1.000000000000000000, 0.8660254037844387076, 1.000000000000000000, 0.8660254037844387076, 1.000000000000000000, 0.8660254037844387076, 1.000000000000000000, 0.8660254037844387076, 1.000000000000000000, 0.8660254037844387076, 1.000000000000000000, 0.8660254037844387076, 1.000000000000000000, 0.8660254037844387076, 1.000000000000000000, 0.8660254037844387076, 1.000000000000000000, 0.8660254037844387076, 1.000000000000000000, 0.8660254037844387076, 1.000000000000000000, 0.8660254037844387076, 1.000000000000000000, 0.8660254037844387076, 1.000000000000000000, 0.8660254037844387076, 1.000000000000000000, 0.8660254037844387076, 1.000000000000000000, 0.8660254037844387076, 1.000000000000000000, 0.8660254037844387076, 1.000000000000000000, 0.8660254037844387076, 1.000000000000000000, 0.8660254037844387076, 1.000000000000000000, 0.8660254037844387076, 1.000000000000000000, 0.8660254037844387076, 1.000000000000000000, 0.8660254037844387076, 1.000000000000000000, 0.8660254037844387076, 1.000000000000000000, 0.8660254037844387076, 1.000000000000000000, 0.8660254037844387076, 1.000000000000000000, 0.8660254037844387076, 1.000000000000000000, 0.8660254037844387076, 1.000000000000000000, 0.8660254037844387076, 1.000000000000000000, 0.8660254037844387076, 1.000000000000000000, 0.8660254037844387076, 1.000000000000000000, 0.8660254037844387076, 1.000000000000000000, 0.8660254037844387076, 1.000000000000000000, 0.8660254037844387076, 1.000000000000000000, 0.8660254037844387076, 1.000000000000000000, 0.8660254037844387076, 1.000000000000000000, 0.8660254037844387076, 1.000000000000000000, 0.8660254037844387076, 1.000000000000000000, 0.8660254037844387076, 1.000000000000000000, 0.8660254037844387076, 1.000000000000000000, 0.8660254037844387076, 1.000000000000000000, 0.8660254037844387076, 1.000000000000000000, 0.8660254037844387076, 1.000000000000000000, 0.8660254037844387076, 1.000000000000000000, 0.8660254037844387076, 1.000000000000000000, 0.8660254037844387076, 1.000000000000000000, 0.8660254037844387076, 1.000000000000000000, 0.8660254037844387076, 1.000000000000000000, 0.8660254037844387076, 1.000000000000000000, 0.8660254037844387076, 1.000000000000000000, 0.8660254037844387076, 1.000000000000000000, 0.8660254037844387076, 1.000000000000000000, 0.8660254037844387076, 1.000000000000000000, 0.8660254037844387076, 1.000000000000000000, 0.8660254037844387076, 1.000000000000000000, 0.8660254037844387076, 1.000000000000000000, 0.8660254037844387076, 1.000000000000000000, 0.8660254037844387076, 1.000000000000000000, 0.8660254037844387076, 1.000000000000000000, 0.8660254037844387076, 1.000000000000000000, 0.8660254037844387076, 1.000000000000000000, 0.8660254037844387076, 1.000000000000000000, 0.8660254037844387076, 1.000000000000000000, 0.8660254037844387076, 1.000000000000000000, 0.8660254037844387076, 1.000000000000000000, 0.8660254037844387076, 1.000000000000000000, 0.8660254037844387076, 1.000000000000000000, 0.8660254037844387076, 1.000000000000000000, 0.8660254037844387076, 1.000000000000000000, 0.8660254037844387076, 1.000000000000000000, 0.8660254037844387076, 1.000000000000000000, 0.8660254037844387076, 1.000000000000000000, 0.8660254037844387076, 1.000000000000000000, 0.8660254037844387076, 1.000000000000000000, 0.8660254037844387076, 1.000000000000000000, 0.8660254037844387076, 1.000000000000000000, 0.8660254037844387076, 1.000000000000000000, 0.8660254037844387076, 1.000000000000000000, 0.8660254037844387076, 1.000000000000000000, 0.8660254037844387076, 1.000000000000000000, 0.8660254037844387076, 1.000000000000000000, 0.8660254037844387076, 1.000000000000000000, 0.8660254037844387076, 1.000000000000000000),
 ( 1.000000000000000000, 0.8660254037844387076, 1.000000000000000000, 0.8660254037844387076, 1.000000000000000000, 0.8660254037844387076, 1.000000000000000000, 0.8660254037844387076, 1.000000000000000000, 0.8660254037844387076, 1.000000000000000000, 0.8660254037844387076, 1.000000000000000000, 0.8660254037844387076, 1.000000000000000000, 0.8660254037844387076, 1.000000000000000000, 0.8660254037844387076, 1.000000000000000000, 0.8660254037844387076, 1.000000000000000000, 0.8660254037844387076, 1.000000000000000000, 0.8660254037844387076, 1.000000000000000000, 0.8660254037844387076, 1.000000000000000000, 0.8660254037844387076, 1.000000000000000000, 0.8660254037844387076, 1.000000000000000000, 0.8660254037844387076, 1.000000000000000000, 0.8660254037844387076, 1.000000000000000000, 0.8660254037844387076, 1.000000000000000000, 0.8660254037844387076, 1.000000000000000000, 0.8660254037844387076, 1.000000000000000000, 0.8660254037844387076, 1.000000000000000000, 0.8660254037844387076, 1.000000000000000000, 0.8660254037844387076, 1.000000000000000000, 0.8660254037844387076, 1.000000000000000000, 0.8660254037844387076, 1.000000000000000000, 0.8660254037844387076, 1.000000000000000000, 0.8660254037844387076, 1.000000000000000000, 0.8660254037844387076, 1.000000000000000000, 0.8660254037844387076, 1.000000000000000000, 0.8660254037844387076, 1.000000000000000000, 0.8660254037844387076, 1.000000000000000000, 0.8660254037844387076, 1.000000000000000000, 0.8660254037844387076, 1.000000000000000000, 0.8660254037844387076, 1.000000000000000000, 0.8660254037844387076, 1.000000000000000000, 0.8660254037844387076, 1.000000000000000000, 0.8660254037844387076, 1.000000000000000000, 0.8660254037844387076, 1.000000000000000000, 0.8660254037844387076, 1.000000000000000000, 0.8660254037844387076, 1.000000000000000000, 0.8660254037844387076, 1.000000000000000000, 0.8660254037844387076, 1.000000000000000000, 0.8660254037844387076, 1.000000000000000000, 0.8660254037844387076, 1.000000000000000000, 0.8660254037844387076, 1.000000000000000000, 0.8660254037844387076, 1.000000000000000000, 0.8660254037844387076, 1.000000000000000000, 0.8660254037844387076, 1.000000000000000000, 0.8660254037844387076, 1.000000000000000000, 0.8660254037844387076, 1.000000000000000000, 0.8660254037844387076, 1.000000000000000000, 0.8660254037844387076, 1.000000000000000000, 0.8660254037844387076, 1.000000000000000000, 0.8660254037844387076, 1.000000000000000000, 0.8660254037844387076, 1.000000000000000000, 0.8660254037844387076, 1.000000000000000000, 0.8660254037844387076, 1.000000000000000000, 0.8660254037844387076, 1.000000000000000000, 0.8660254037844387076, 1.000000000000000000, 0.8660254037844387076, 1.000000000000000000, 0.8660254037844387076, 1.000000000000000000, 0.8660254037844387076, 1.000000000000000000, 0.8660254037844387076, 1.000000000000000000, 0.8660254037844387076, 1.000000000000000000, 0.8660254037844387076, 1.000000000000000000, 0.8660254037844387076, 1.000000000000000000, 0.8660254037844387076, 1.000000000000000000, 0.8660254037844387076, 1.000000000000000000, 0.8660254037844387076, 1.000000000000000000, 0.8660254037844387076, 1.000000000000000000, 0.8660254037844387076, 1.000000000000000000, 0.8660254037844387076, 1.000000000000000000, 0.8660254037844387076, 1.000000000000000000, 0.8660254037844387076, 1.000000000000000000, 0.8660254037844387076, 1.000000000000000000, 0.8660254037844387076, 1.000000000000000000, 0.8660254037844387076, 1.000000000000000000, 0.8660254037844387076, 1.000000000000000000, 0.8660254037844387076, 1.000000000000000000, 0.8660254037844387076, 1.000000000000000000, 0.8660254037844387076, 1.000000000000000000, 0.8660254037844387076, 1.000000000000000000, 0.8660254037844387076, 1.000000000000000000, 0.8660254037844387076, 1.000000000000000000, 0.8660254037844387076, 1.000000000000000000, 0.8660254037844387076, 1.000000000000000000, 0.8660254037844387076, 1.000000000000000000, 0.8660254037844387076, 1.000000000000000000, 0.8660254037844387076, 1.000000000000000000, 0.8660254037844387076, 1.000000000000000000, 0.8660254037844387076, 1.000000000000000000, 0.8660254037844387076, 1.000000000000000000, 0.8660254037844387076, 1.000000000000000000, 0.8660254037844387076, 1.000000000000000000, 0.8660254037844387076, 1.000000000000000000, 0.8660254037844387076, 1.000000000000000000, 0.8660254037844387076, 1.000000000000000000, 0.8660254037844387076, 1.000000000000000000, 0.8660254037844387076, 1.000000000000000000, 0.8660254037844387076, 1.000000000000000000, 0.8660254037844387076, 1.000000000000000000, 0.8660254037844387076, 1.000000000000000000, 0.8660254037844387076, 1.000000000000000000, 0.8660254037844387076, 1.000000000000000000, 0.8660254037844387076, 1.000000000000000000, 0.8660254037844387076, 1.000000000000000000, 0.8660254037844387076, 1.000000000000000000, 0.8660254037844387076, 1.000000000000000000, 0.8660254037844387076, 1.000000000000000000, 0.8660254037844387076, 1.000000000000000000, 0.8660254037844387076, 1.000000000000000000, 0.8660254037844387076, 1.000000000000000000, 0.8660254037844387076, 1.000000000000000000, 0.8660254037844387076, 1.000000000000000000, 0.8660254037844387076, 1.000000000000000000, 0.8660254037844387076, 1.000000000000000000, 0.8660254037844387076, 1.000000000000000000, 0.8660254037844387076, 1.000000000000000000, 0.8660254037844387076, 1.000000000000000000, 0.8660254037844387076, 1.000000000000000000, 0.8660254037844387076, 1.000000000000000000, 0.8660254037844387076, 1.000000000000000000, 0.8660254037844387076, 1.000000000000000000, 0.8660254037844387076, 1.000000000000000000, 0.8660254037844387076, 1.000000000000000000, 0.8660254037844387076, 1.000000000000000000, 0.8660254037844387076, 1.000000000000000000, 0.8660254037844387076, 1.000000000000000000, 0.8660254037844387076, 1.000000000000000000, 0.8660254037844387076, 1.000000000000000000, 0.8660254037844387076, 1.000000000000000000, 0.8660254037844387076, 1.000000000000000000, 0.8660254037844387076, 1.000000000000000000, 0.8660254037844387076, 1.000000000000000000, 0.8660254037844387076, 1.000000000000000000, 0.8660254037844387076, 1.000000000000000000, 0.8660254037844387076, 1.000000000000000000, 0.8660254037844387076, 1.000000000000000000, 0.8660254037844387076, 1.000000000000000000, 0.8660254037844387076, 1.000000000000000000, 0.8660254037844387076, 1.000000000000000000, 0.8660254037844387076, 1.000000000000000000, 0.8660254037844387076, 1.000000000000000000, 0.8660254037844387076, 1.000000000000000000, 0.8660254037844387076, 1.000000000000000000, 0.8660254037844387076, 1.000000000000000000, 0.8660254037844387076, 1.000000000000000000, 0.8660254037844387076, 1.000000000000000000, 0.8660254037844387076, 1.000000000000000000, 0.8660254037844387076, 1.000000000000000000, 0.8660254037844387076, 1.000000000000000000, 0.8660254037844387076, 1.000000000000000000, 0.8660254037844387076, 1.000000000000000000, 0.8660254037844387076, 1.000000000000000000, 0.8660254037844387076, 1.000000000000000000, 0.8660254037844387076, 1.000000000000000000, 0.8660254037844387076, 1.000000000000000000, 0.8660254037844387076, 1.000000000000000000, 0.8660254037844387076, 1.000000000000000000, 0.8660254037844387076, 1.000000000000000000, 0.8660254037844387076, 1.000000000000000000, 0.8660254037844387076, 1.000000000000000000, 0.8660254037844387076, 1.000000000000000000, 0.8660254037844387076, 1.000000000000000000, 0.8660254037844387076, 1.000000000000000000, 0.8660254037844387076, 1.000000000000000000, 0.8660254037844387076, 1.000000000000000000, 0.8660254037844387076, 1.000000000000000000, 0.8660254037844387076, 1.000000000000000000, 0.8660254037844387076, 1.000000000000000000, 0.8660254037844387076, 1.000000000000000000, 0.8660254037844387076, 1.000000000000000000, 0.8660254037844387076, 1.000000000000000000, 0.8660254037844387076, 1.000000000000000000, 0.8660254037844387076, 1.000000000000000000, 0.8660254037844387076, 1.000000000000000000, 0.8660254037844387076, 1.000000000000000000, 0.8660254037844387076, 1.000000000000000000, 0.8660254037844387076, 1.000000000000000000, 0.8660254037844387076, 1.000000000000000000, 0.8660254037844387076, 1.000000000000000000, 0.8660254037844387076, 1.000000000000000000, 0.8660254037844387076, 1.000000000000000000, 0.8660254037844387076, 1.000000000000000000, 0.8660254037844387076, 1.000000000000000000, 0.8660254037844387076, 1.000000000000000000, 0.8660254037844387076, 1.000000000000000000, 0.8660254037844387076, 1.000000000000000000, 0.8660254037844387076, 1.000000000000000000, 0.8660254037844387076, 1.000000000000000000, 0.8660254037844387076, 1.000000000000000000, 0.8660254037844387076, 1.000000000000000000, 0.8660254037844387076, 1.000000000000000000, 0.8660254037844387076, 1.000000000000000000, 0.8660254037844387076, 1.000000000000000000, 0.8660254037844387076, 1.000000000000000000, 0.8660254037844387076, 1.000000000000000000, 0.8660254037844387076, 1.000000000000000000, 0.8660254037844387076, 1.000000000000000000, 0.8660254037844387076, 1.000000000000000000, 0.8660254037844387076, 1.000000000000000000, 0.8660254037844387076, 1.000000000000000000, 0.8660254037844387076, 1.000000000000000000, 0.8660254037844387076, 1.000000000000000000, 0.8660254037844387076, 1.000000000000000000, 0.8660254037844387076, 1.000000000000000000, 0.8660254037844387076, 1.000000000000000000, 0.8660254037844387076, 1.000000000000000000, 0.8660254037844387076, 1.000000000000000000, 0.8660254037844387076, 1.000000000000000000, 0.8660254037844387076, 1.000000000000000000, 0.8660254037844387076, 1.000000000000000000, 0.8660254037844387076, 1.000000000000000000, 0.8660254037844387076, 1.000000000000000000, 0.8660254037844387076, 1.000000000000000000, 0.8660254037844387076, 1.000000000000000000, 0.8660254037844387076, 1.000000000000000000, 0.8660254037844387076, 1.000000000000000000, 0.8660254037844387076, 1.000000000000000000, 0.8660254037844387076, 1.000000000000000000, 0.8660254037844387076, 1.000000000000000000, 0.8660254037844387076, 1.000000000000000000, 0.8660254037844387076, 1.000000000000000000, 0.8660254037844387076, 1.000000000000000000, 0.8660254037844387076, 1.000000000000000000, 0.8660254037844387076, 1.000000000000000000, 0.8660254037844387076, 1.000000000000000000, 0.8660254037844387076, 1.000000000000000000, 0.8660254037844387076, 1.000000000000000000, 0.8660254037844387076, 1.000000000000000000, 0.8660254037844387076, 1.000000000000000000, 0.8660254037844387076, 1.000000000000000000, 0.8660254037844387076, 1.000000000000000000, 0.8660254037844387076, 1.000000000000000000, 0.8660254037844387076, 1.000000000000000000, 0.8660254037844387076, 1.000000000000000000, 0.8660254037844387076, 1.000000000000000000, 0.8660254037844387076, 1.000000000000000000, 0.8660254037844387076, 1.000000000000000000, 0.8660254037844387076, 1.000000000000000000) ) ) 
 REPRESENTATION_ITEM ( '' )  SURFACE ( )  );
#5739 = CARTESIAN_POINT ( 'NONE',  ( -8.299562589859897699, 12.83457345481192036, -0.7998128361456281477 ) ) ;
#5740 = CARTESIAN_POINT ( 'NONE',  ( 0.3043191165176574176, 1.600368420507289668, 0.9101283655772866021 ) ) ;
#5742 = PRESENTATION_LAYER_ASSIGNMENT (  '', '', ( #147580 ) ) ;
#5741 = CARTESIAN_POINT ( 'NONE',  ( 3.432658224824499893, -1.297079494776206543, 1.740850151316934991 ) ) ;
#5743 = CARTESIAN_POINT ( 'NONE',  ( 0.000000000000000000, 18.91999999999999815, 0.000000000000000000 ) ) ;
#5744 = CARTESIAN_POINT ( 'NONE',  ( 0.8793290508635929204, -1.919567575575848339, -0.9014759086384205311 ) ) ;
#5745 = CARTESIAN_POINT ( 'NONE',  ( 1.499999999999987121, 1.535416667349486453, 0.8660254037844524744 ) ) ;
#5746 = CARTESIAN_POINT ( 'NONE',  ( 9.836604141914616406, 11.43479190611061647, 1.199719254218452047 ) ) ;
#5747 = FACE_OUTER_BOUND ( 'NONE', #1493, .T. ) ;
#5748 = CARTESIAN_POINT ( 'NONE',  ( 5.669760509565840323, 7.437725440679550992, 1.325564871123290356 ) ) ;
#5749 = CARTESIAN_POINT ( 'NONE',  ( 0.5267265402719328860, 1.971218143044730420, 0.6008300406652696823 ) ) ;
#5751 = CARTESIAN_POINT ( 'NONE',  ( 0.4461838333974484927, 2.877219473291486640, 1.949594826320268481 ) ) ;
#5750 = CYLINDRICAL_SURFACE ( 'NONE', #104934, 0.08000000000000020983 ) ;
#5752 = CARTESIAN_POINT ( 'NONE',  ( 1.364683531249988757, 0.3843750003414206362, 0.000000000000000000 ) ) ;
#5753 = CARTESIAN_POINT ( 'NONE',  ( 0.000000000000000000, 5.999999999999998224, 0.000000000000000000 ) ) ;
#5754 = VERTEX_POINT ( 'NONE', #139730 ) ;
#5755 = CARTESIAN_POINT ( 'NONE',  ( 3.352119889487484183, 0.8575151890419380196, -1.709291564166728783 ) ) ;
#5756 = CARTESIAN_POINT ( 'NONE',  ( 5.770295338139614927, -1.120113875738535825, 1.370259874377998788 ) ) ;
#5757 = CARTESIAN_POINT ( 'NONE',  ( 6.710359684120930091, 6.793450817754725257, 0.7998128361456352531 ) ) ;
#5758 = CARTESIAN_POINT ( 'NONE',  ( -3.741160322367112379, 6.452105245148518797, 1.199719254218464037 ) ) ;
#5759 = CARTESIAN_POINT ( 'NONE',  ( 0.7206316775285178666, 1.371080193274256676, -1.184091668402836639 ) ) ;
#5761 = CARTESIAN_POINT ( 'NONE',  ( 0.6201578395632812990, 1.887877179178775400, 0.3243255173654129297 ) ) ;
#5760 = CARTESIAN_POINT ( 'NONE',  ( 1.579999999999985860, -1.099999999999982991, -2.579999999999990301 ) ) ;
#5762 = CARTESIAN_POINT ( 'NONE',  ( 1.996617168637443429, 2.047528291220417351, 0.3059219562495316125 ) ) ;
#5763 = CARTESIAN_POINT ( 'NONE',  ( -0.6823417656250003738, -0.2197916663252488800, -1.181850606188749264 ) ) ;
#5764 = CARTESIAN_POINT ( 'NONE',  ( 6.420764531294745225, 1.746252128813120086, 0.6712297951826234899 ) ) ;
#5765 = CARTESIAN_POINT ( 'NONE',  ( 3.193790821891542731, -0.7392406677243367197, 1.669511829839696260 ) ) ;
#5767 = CARTESIAN_POINT ( 'NONE',  ( 6.307155384238837037, 6.868572428096745064, 0.7081091520576547893 ) ) ;
#5766 = CARTESIAN_POINT ( 'NONE',  ( 0.5929126122562259349, -2.290994082922478636, -0.2767204673215419852 ) ) ;
#5768 = EDGE_CURVE ( 'NONE', #191630, #187511, #12121, .T. ) ;
#5769 = CARTESIAN_POINT ( 'NONE',  ( 0.6823417656249882723, 0.9260416670080831025, -1.181850606188749264 ) ) ;
#5770 = AXIS2_PLACEMENT_3D ( 'NONE', #198618, #116383, #196517 ) ;
#5771 = CARTESIAN_POINT ( 'NONE',  ( 4.668458352237446540, -0.8791470107305986437, -1.866060610730088332 ) ) ;
#5772 = CARTESIAN_POINT ( 'NONE',  ( -7.063961727919978451, 8.200042423116789436, 1.199719254218450271 ) ) ;
#5773 = CARTESIAN_POINT ( 'NONE',  ( 7.130698725783555680, 10.40656671580112658, 1.199719254218460707 ) ) ;
#5774 = CARTESIAN_POINT ( 'NONE',  ( 4.436542580169809291, 6.199052314996659874, 1.599625672291267175 ) ) ;
#5775 = CARTESIAN_POINT ( 'NONE',  ( 0.1753634416057497925, 0.0001173177735149660839, -2.144164757042037017 ) ) ;
#5776 = AXIS2_PLACEMENT_3D ( 'NONE', #186216, #103926, #18384 ) ;
#5777 = CARTESIAN_POINT ( 'NONE',  ( 6.355931484454268698, -0.7012994977402075003, 1.948090369817329526 ) ) ;
#5778 = CARTESIAN_POINT ( 'NONE',  ( -0.6823417656250212460, 1.613541667008083769, 1.181850606188755259 ) ) ;
#5779 = CARTESIAN_POINT ( 'NONE',  ( 3.602937629199114422, 1.706465849011789881, -1.326752773236601124 ) ) ;
#5780 = CARTESIAN_POINT ( 'NONE',  ( 4.143226661672769318, 0.1011831993794048007, 2.017277399227022094 ) ) ;
#5781 = CARTESIAN_POINT ( 'NONE',  ( 6.620655732516651071, 4.689394895873098434, 2.736297475404291024 ) ) ;
#5782 = ADVANCED_FACE ( 'NONE', ( #190567 ), #108992, .T. ) ;
#5785 = CARTESIAN_POINT ( 'NONE',  ( 7.022760382198770301, 8.255937203062467589, -1.082531754730543083 ) ) ;
#5784 = CARTESIAN_POINT ( 'NONE',  ( 3.285556943750000514, -3.813541666188710710, 1.896917185911906500 ) ) ;
#5783 = DIRECTION ( 'NONE',  ( 0.000000000000000000, 0.000000000000000000, -1.000000000000000000 ) ) ;
#5786 = CARTESIAN_POINT ( 'NONE',  ( -6.954406449166956605, 7.078172043641714595, -0.7998128361456362523 ) ) ;
#5787 = CARTESIAN_POINT ( 'NONE',  ( 2.325407997918966796, -1.497503195670712328, -1.350734289967000512 ) ) ;
#5788 = CARTESIAN_POINT ( 'NONE',  ( -6.744291347794091784, 9.955758108146730123, -1.199719254218440723 ) ) ;
#5790 = CARTESIAN_POINT ( 'NONE',  ( -4.199533704925234368, 7.510932310329544670, -0.9222493318717175370 ) ) ;
#5789 = CARTESIAN_POINT ( 'NONE',  ( -4.711622075948912247, 5.455646162483875017, -1.199719254218446718 ) ) ;
#5791 = CARTESIAN_POINT ( 'NONE',  ( -3.746784212325278141, 7.355493017976345804, 0.6363135798663853704 ) ) ;
#5792 = CARTESIAN_POINT ( 'NONE',  ( 5.906500813101931868, -1.903809282439900219, -0.1807861040028224398 ) ) ;
#5793 = DIRECTION ( 'NONE',  ( 0.7408284471490504952, 0.000000000000000000, -0.6716942845482061220 ) ) ;
#5794 = CARTESIAN_POINT ( 'NONE',  ( 5.382223794500827552, 7.302347065049529462, -1.443375672974051449 ) ) ;
#5796 = CARTESIAN_POINT ( 'NONE',  ( 4.007435537932837910, -1.928747227692016564, 0.5880391185724976877 ) ) ;
#5795 = CARTESIAN_POINT ( 'NONE',  ( -7.904040366642703930, 10.24446639921506552, 1.443375672974090751 ) ) ;
#5797 = CARTESIAN_POINT ( 'NONE',  ( -1.201851678989727383E-14, 5.087500000000019007, -1.732050807568863648 ) ) ;
#5798 = CARTESIAN_POINT ( 'NONE',  ( -8.012344526598182026E-15, 14.60937500034139980, -1.575800808251669460 ) ) ;
#5799 = CARTESIAN_POINT ( 'NONE',  ( 6.510786919798099426, 1.273903079158642981, -1.162983891536113479 ) ) ;
#5800 = CARTESIAN_POINT ( 'NONE',  ( 6.384963997392946844, 6.413822516572072807, 0.7998128361456352531 ) ) ;
#5802 = DIRECTION ( 'NONE',  ( -3.330669073875479482E-16, 3.330669073875479482E-16, 1.000000000000000000 ) ) ;
#5801 = CARTESIAN_POINT ( 'NONE',  ( 9.897088948295946764, 10.64895131587453569, 0.7216878364870438212 ) ) ;
#5803 = CARTESIAN_POINT ( 'NONE',  ( 10.99916818177027622, -10.00038292658552486, -0.1458870414463221132 ) ) ;
#5804 = CARTESIAN_POINT ( 'NONE',  ( 4.956247902659736582, 0.7144662795386286236, 1.728917671469521800 ) ) ;
#5805 = CARTESIAN_POINT ( 'NONE',  ( 0.06508986333318785011, -1.615617207129100397, 1.200762793324720690 ) ) ;
#5806 = FACE_BOUND ( 'NONE', #190877, .T. ) ;
#5807 = AXIS2_PLACEMENT_3D ( 'NONE', #106904, #86320, #6112 ) ;
#5808 = CARTESIAN_POINT ( 'NONE',  ( 2.623957243734816647, 2.031168598393529034, -0.3995267358143372860 ) ) ;
#5809 = CARTESIAN_POINT ( 'NONE',  ( 0.4350533259329415481, -9.438199013093635514, -9.251577493846877331 ) ) ;
#5810 = ORIENTED_EDGE ( 'NONE', *, *, #123967, .T. ) ;
#5811 = CARTESIAN_POINT ( 'NONE',  ( 4.913904330310220558, 4.697586238308844919, 0.000000000000000000 ) ) ;
#5813 = ADVANCED_FACE ( 'NONE', ( #155960 ), #129697, .T. ) ;
#5812 = CARTESIAN_POINT ( 'NONE',  ( 0.5621253344089729431, -1.117812357707391069, 1.678020072846800659 ) ) ;
#5814 = CARTESIAN_POINT ( 'NONE',  ( 1.564434226245875026, 0.5705330181091838870, 1.719429346978663897 ) ) ;
#5815 = CARTESIAN_POINT ( 'NONE',  ( 5.370438244344566847, 5.438135171256338829, 0.000000000000000000 ) ) ;
#5816 = FACE_BOUND ( 'NONE', #9308, .T. ) ;
#5817 = AXIS2_PLACEMENT_3D ( 'NONE', #186095, #38795, #87549 ) ;
#5818 = CARTESIAN_POINT ( 'NONE',  ( 8.554831740098663317, 9.082984572977682802, 0.7216878364870458196 ) ) ;
#5819 = CARTESIAN_POINT ( 'NONE',  ( 6.252281394196331554, 10.44607872653774372, 1.040834085586084257E-14 ) ) ;
#5821 = CARTESIAN_POINT ( 'NONE',  ( 6.099236069963973605, -0.2290726985337887822, 1.901777391499546166 ) ) ;
#5820 = CARTESIAN_POINT ( 'NONE',  ( -5.961834861707238531, 7.978559976790334574, -1.599625672291263179 ) ) ;
#5822 = CARTESIAN_POINT ( 'NONE',  ( -11.44800751630026880, 13.79999999999998295, 3.302956944461236777 ) ) ;
#5823 = DIRECTION ( 'NONE',  ( 1.000000000000000000, -3.135042426464105837E-15, 0.000000000000000000 ) ) ;
#5824 = B_SPLINE_CURVE_WITH_KNOTS ( 'NONE', 3,
 ( #7897, #90247, #89187, #73985, #139004, #57736, #140080, #205026, #77174, #155238, #174713, #56672, #209287, #121752, #40433, #107618, #8978, #92401, #206103, #173649, #39348, #25223, #91326, #157386, #75052, #43644, #141166, #190916, #207175, #124954 ),
 .UNSPECIFIED., .F., .F.,
 ( 4, 2, 2, 2, 2, 2, 2, 2, 2, 2, 2, 2, 2, 2, 4 ),
 ( 0.3904182756812821231, 0.3921283039710705687, 0.3938383322608589587, 0.3972583888404358499, 0.4040985019995896321, 0.4177787283178971967, 0.4451391809545123257, 0.4999364453639513206, 0.5547656701200603946, 0.5821739285757332460, 0.5958780578035696163, 0.6027301224174878014, 0.6061561547244469494, 0.6078691708779264680, 0.6095821870314059865 ),
 .UNSPECIFIED. ) ;
#5825 = EDGE_CURVE ( 'NONE', #57442, #6079, #12173, .T. ) ;
#5826 = CARTESIAN_POINT ( 'NONE',  ( -10.99979681685432631, -6.306104522322589112, -0.07019693227476625497 ) ) ;
#5828 = EDGE_LOOP ( 'NONE', ( #152679, #100768, #3675, #154947 ) ) ;
#5827 = CARTESIAN_POINT ( 'NONE',  ( 4.148431816101584957, 6.823292304551739740, -1.082531754730548412 ) ) ;
#5829 = CARTESIAN_POINT ( 'NONE',  ( -3.785751206713858785, 5.439795712631356750, 1.599625672291267398 ) ) ;
#5830 = CARTESIAN_POINT ( 'NONE',  ( -7.321039761699444703, 10.52466824108257804, 1.082531754730549967 ) ) ;
#5831 = CIRCLE ( 'NONE', #113094, 0.08000000000000014044 ) ;
#5832 = CARTESIAN_POINT ( 'NONE',  ( 2.958072429731005926, 2.151414462573512765, -0.2105227563667099733 ) ) ;
#5833 = EDGE_CURVE ( 'NONE', #17518, #146015, #43134, .T. ) ;
#5834 = CARTESIAN_POINT ( 'NONE',  ( -5.478903473698241378, 9.406154796041011679, -0.7216878364870338292 ) ) ;
#5835 = CARTESIAN_POINT ( 'NONE',  ( 6.888951449519509218, 7.209733910627123876, -0.7216878364870317197 ) ) ;
#5836 = CARTESIAN_POINT ( 'NONE',  ( 0.5453776912951785460, 0.1620316879334358084, 2.114494688702214020 ) ) ;
#5837 = CARTESIAN_POINT ( 'NONE',  ( 5.579063851370913873, -0.04688903583028104782, -1.825137680102270288 ) ) ;
#5838 = CARTESIAN_POINT ( 'NONE',  ( 1.704304553464238703, -0.7057161435466070554, -1.840894384558971808 ) ) ;
#5839 = CARTESIAN_POINT ( 'NONE',  ( 4.465046277278037934, -1.532637281380120564, 1.143568071694904598 ) ) ;
#5840 = ORIENTED_EDGE ( 'NONE', *, *, #84110, .T. ) ;
#5841 = CARTESIAN_POINT ( 'NONE',  ( -11.33772465723282785, 10.09131699265171278, -3.600000000000076472 ) ) ;
#5842 = CARTESIAN_POINT ( 'NONE',  ( 4.492606276566666779, 1.931098607525572497, 0.3863565733641035616 ) ) ;
#5843 = CARTESIAN_POINT ( 'NONE',  ( 0.2693405865131668353, 1.117251289913205881, 1.588187351064213715 ) ) ;
#5844 = ORIENTED_EDGE ( 'NONE', *, *, #102451, .F. ) ;
#5845 = CARTESIAN_POINT ( 'NONE',  ( -4.960304097753355457, 6.880383762169266504, 1.599625672291263179 ) ) ;
#5847 = CARTESIAN_POINT ( 'NONE',  ( -0.3788956605886329987, 3.049042541176487209, 0.4283520265745272004 ) ) ;
#5846 = CARTESIAN_POINT ( 'NONE',  ( -3.634467696915153034, 6.397906858779740524, 1.199719254218452935 ) ) ;
#5849 = CARTESIAN_POINT ( 'NONE',  ( 5.519577934094851202, 8.493239118869080784, 1.082531754730547524 ) ) ;
#5848 = CARTESIAN_POINT ( 'NONE',  ( 6.435316467980822353, 10.65961964595298817, 1.040834085586084257E-14 ) ) ;
#5851 = ORIENTED_EDGE ( 'NONE', *, *, #91556, .F. ) ;
#5850 = CARTESIAN_POINT ( 'NONE',  ( 5.039673278062164918, -1.814583965733532978, 0.6035816954967700987 ) ) ;
#5852 = CARTESIAN_POINT ( 'NONE',  ( 0.7103623821160671703, -2.195938746145317477, 0.2182302698266261887 ) ) ;
#5853 = CARTESIAN_POINT ( 'NONE',  ( 5.830732115328919996, 1.350214353519451960, -1.493314199452821178 ) ) ;
#5854 = CARTESIAN_POINT ( 'NONE',  ( 0.07680821025394035662, 2.052785608010514018, -2.228496998325917744 ) ) ;
#5855 = DIRECTION ( 'NONE',  ( -0.000000000000000000, 1.000000000000000000, -0.000000000000000000 ) ) ;
#5856 = CARTESIAN_POINT ( 'NONE',  ( -10.62873463776380234, 9.799999999999982947, 3.199999999999997957 ) ) ;
#5857 = CARTESIAN_POINT ( 'NONE',  ( 3.525891238081062085, 2.020528833579691597, -0.4508363271973143127 ) ) ;
#5858 = CARTESIAN_POINT ( 'NONE',  ( -6.898401231254901234, 6.942556279419168419, -0.7998128361456291469 ) ) ;
#5859 = CARTESIAN_POINT ( 'NONE',  ( -4.640257700270903563, 8.337993449908045918, -0.3781808898682629261 ) ) ;
#5861 = CARTESIAN_POINT ( 'NONE',  ( 0.4620835240300471547, 2.137967531602209981, -0.3185850937674692407 ) ) ;
#5860 = CARTESIAN_POINT ( 'NONE',  ( -2.605138072120212200, 6.191078184115536232, -0.7998128361456281477 ) ) ;
#5862 =( NAMED_UNIT ( * ) PLANE_ANGLE_UNIT ( ) SI_UNIT ( $, .RADIAN. ) );
#5863 = CARTESIAN_POINT ( 'NONE',  ( 5.289089323106923146, 6.303597310780433283, -1.082531754730548412 ) ) ;
#5864 = CARTESIAN_POINT ( 'NONE',  ( -4.812789021178021542, 5.101776157678782120, 0.9029685044427698815 ) ) ;
#5865 = CARTESIAN_POINT ( 'NONE',  ( -8.012344526598182026E-15, 12.85937500034139802, -1.575800808251669460 ) ) ;
#5867 = CARTESIAN_POINT ( 'NONE',  ( -6.479871072688648148, 6.524547437750345402, 0.000000000000000000 ) ) ;
#5866 = CARTESIAN_POINT ( 'NONE',  ( 6.825078400183548055, 2.475450427997231362, 2.140471860334830279 ) ) ;
#5868 = CARTESIAN_POINT ( 'NONE',  ( 4.975145882941295561, -1.721944285756441984, -0.2046304421847028043 ) ) ;
#5869 = CARTESIAN_POINT ( 'NONE',  ( -3.066115294984855133, 6.728884944124295053, 0.7998128361456341429 ) ) ;
#5870 = CARTESIAN_POINT ( 'NONE',  ( 2.079047829753433163, 1.930162853665925216, 0.7490395704240898622 ) ) ;
#5871 = CARTESIAN_POINT ( 'NONE',  ( 4.376635333690025220, -0.4654363970535125294, -2.065280895323940324 ) ) ;
#5872 = CARTESIAN_POINT ( 'NONE',  ( 8.450809820019639318, 8.753699632978056755, -0.7998128361456291469 ) ) ;
#5873 = CARTESIAN_POINT ( 'NONE',  ( -1.364683531250010740, 4.030208333674752730, 0.7879004041258379498 ) ) ;
#5874 = CARTESIAN_POINT ( 'NONE',  ( 1.920693274676561924, -1.396391452584997417, 1.389085034315578060 ) ) ;
#5875 = CARTESIAN_POINT ( 'NONE',  ( 0.4043728756845180183, -1.898191424145349471, -0.2318213773434482650 ) ) ;
#5876 = CARTESIAN_POINT ( 'NONE',  ( 5.349693066923443041, 2.289838395228523282, -0.1081633463214677210 ) ) ;
#5877 = CARTESIAN_POINT ( 'NONE',  ( 2.209345402013741300, -0.4006574107652469130, 1.781019818369505847 ) ) ;
#5878 = CARTESIAN_POINT ( 'NONE',  ( 5.123001941117305336, 7.070197912760590064, 1.599625672291268286 ) ) ;
#5879 = CARTESIAN_POINT ( 'NONE',  ( 6.277061933002788585, 6.425586464699131639, 0.7216878364870317197 ) ) ;
#5880 = CARTESIAN_POINT ( 'NONE',  ( -6.886651960737580680, 10.12184548991413457, -1.199719254218440723 ) ) ;
#5881 = CARTESIAN_POINT ( 'NONE',  ( 3.199479786217104493, 1.818179288054132536, -0.8647478076822049387 ) ) ;
#5882 = CARTESIAN_POINT ( 'NONE',  ( 3.520314338623427020, 0.8779579967637550775, 1.754372790864023646 ) ) ;
#5883 = CARTESIAN_POINT ( 'NONE',  ( -6.997979842947967377, 11.31606025008131233, -0.7998128361456291469 ) ) ;
#5884 =( GEOMETRIC_REPRESENTATION_CONTEXT ( 3 ) GLOBAL_UNCERTAINTY_ASSIGNED_CONTEXT ( ( #116588 ) ) GLOBAL_UNIT_ASSIGNED_CONTEXT ( ( #15813, #115528, #82956 ) ) REPRESENTATION_CONTEXT ( 'NONE', 'WORKASPACE' ) );
#5885 = CARTESIAN_POINT ( 'NONE',  ( -4.412288926243578935, 7.235088616337731260, 1.199719254218464037 ) ) ;
#5886 = FACE_OUTER_BOUND ( 'NONE', #3059, .T. ) ;
#5888 = CARTESIAN_POINT ( 'NONE',  ( 4.311239457809501907, -0.3017279273445966914, 1.743759454612598070 ) ) ;
#5887 = CARTESIAN_POINT ( 'NONE',  ( 5.736299646367586824, 0.4068676293152873602, 2.050479918790772960 ) ) ;
#5889 = DIRECTION ( 'NONE',  ( -0.000000000000000000, -1.000000000000000000, -0.000000000000000000 ) ) ;
#5890 = EDGE_CURVE ( 'NONE', #194295, #36526, #196032, .T. ) ;
#5891 = CARTESIAN_POINT ( 'NONE',  ( 0.2698121887318750689, 1.265274936352598134, 1.789097752032620114 ) ) ;
#5892 = CARTESIAN_POINT ( 'NONE',  ( 0.2393033055489251493, 1.735545043620636996, 0.1309560527960016429 ) ) ;
#5893 = CARTESIAN_POINT ( 'NONE',  ( 6.317209508963599340, 9.457495962844502557, 1.199719254218462483 ) ) ;
#5894 = CARTESIAN_POINT ( 'NONE',  ( 0.1333692844072559003, 2.872395615372814515, -2.542035612928101873 ) ) ;
#5895 = CARTESIAN_POINT ( 'NONE',  ( 0.1464030204712711281, -0.1495716826577230818, -2.263613701224455710 ) ) ;
#5896 = PLANE ( 'NONE',  #184540 ) ;
#5897 = CARTESIAN_POINT ( 'NONE',  ( 5.290307710256559659, -1.645723771949607173, 0.5459688634881465497 ) ) ;
#5898 = CARTESIAN_POINT ( 'NONE',  ( 1.998912159191484905, -0.5904864226158462737, -2.126349760018491963 ) ) ;
#5899 = CARTESIAN_POINT ( 'NONE',  ( 0.4269466478069834925, -1.418992435970769739, 1.643201522047117669 ) ) ;
#5900 = DIRECTION ( 'NONE',  ( 1.000000000000000000, 0.000000000000000000, 0.000000000000000000 ) ) ;
#5901 = CARTESIAN_POINT ( 'NONE',  ( 0.8489989883206483512, -1.916807839401615476, -0.8996751459469201073 ) ) ;
#5902 = CARTESIAN_POINT ( 'NONE',  ( 4.437500000000002665, 1.451031289060936480, -1.451031289061293528 ) ) ;
#5903 = CARTESIAN_POINT ( 'NONE',  ( -0.2871295479482242619, 7.105992221059546310, -1.980474574527449239 ) ) ;
#5904 = CARTESIAN_POINT ( 'NONE',  ( 4.190394698586521471, -1.905300493120251515, -0.2835615876582204820 ) ) ;
#5905 = CARTESIAN_POINT ( 'NONE',  ( 0.9794852244889130644, -2.010350447809361896, -0.9450808295136583492 ) ) ;
#5906 = ORIENTED_EDGE ( 'NONE', *, *, #198196, .F. ) ;
#5908 = CARTESIAN_POINT ( 'NONE',  ( -0.6823417656250246877, -1.136458332991911790, 1.181850606188755259 ) ) ;
#5907 = CARTESIAN_POINT ( 'NONE',  ( 1.347684858569838440, 0.6597076516901092536, -2.195415608770342253 ) ) ;
#5909 = CARTESIAN_POINT ( 'NONE',  ( 6.159481859310094620, 6.080483678816896109, 1.040834085586084257E-14 ) ) ;
#5910 = CARTESIAN_POINT ( 'NONE',  ( 6.277588818327314080, 7.282607361925381717, 1.199719254218462483 ) ) ;
#5911 = CARTESIAN_POINT ( 'NONE',  ( 3.809420206217276395, 1.876102094647231988, -1.189034995700769981 ) ) ;
#5912 = CARTESIAN_POINT ( 'NONE',  ( -8.866669273657352690, 9.446795028796142191, 0.7216878364870438212 ) ) ;
#5913 = SURFACE_SIDE_STYLE ('',( #172731 ) ) ;
#5914 = CARTESIAN_POINT ( 'NONE',  ( 6.968527767744104651, 8.192665819532020777, 1.082531754730558626 ) ) ;
#5915 = CARTESIAN_POINT ( 'NONE',  ( -7.659993601596710278, 10.92011438762942355, -1.082531754730543083 ) ) ;
#5916 = CARTESIAN_POINT ( 'NONE',  ( 5.966997003790217136, 8.054858819212300958, -1.443375672974078761 ) ) ;
#5918 = ORIENTED_EDGE ( 'NONE', *, *, #36887, .T. ) ;
#5917 = AXIS2_PLACEMENT_3D ( 'NONE', #126327, #75364, #27672 ) ;
#5919 = CARTESIAN_POINT ( 'NONE',  ( 1.494767762416524093, -2.000856930885573259, 0.2496086726550551249 ) ) ;
#5921 = CARTESIAN_POINT ( 'NONE',  ( 6.689892334039674537, -1.344252178338888992, -1.564594595144116695 ) ) ;
#5920 = CARTESIAN_POINT ( 'NONE',  ( 6.889514614038635187, 11.18951748302043114, -0.7998128361456291469 ) ) ;
#5922 = FILL_AREA_STYLE_COLOUR ( '', #102666 ) ;
#5923 = CARTESIAN_POINT ( 'NONE',  ( 5.356880090730850696, 9.263794182579101033, 0.7216878364870317197 ) ) ;
#5924 = CARTESIAN_POINT ( 'NONE',  ( 6.374529642495492254, -0.09526421964337064563, -1.737987611564382862 ) ) ;
#5925 = CARTESIAN_POINT ( 'NONE',  ( -3.380278471875000523, -0.05468749976102194044, 0.000000000000000000 ) ) ;
#5926 = CARTESIAN_POINT ( 'NONE',  ( -1.364683531250000748, 2.009375000341421913, 1.214306433183764966E-14 ) ) ;
#5927 = CARTESIAN_POINT ( 'NONE',  ( 1.334804486018669856, -1.602990312956679597, 0.7502176981645010123 ) ) ;
#5928 = CARTESIAN_POINT ( 'NONE',  ( 6.592404480832670721, -0.3601991968599608795, 1.702173051257379832 ) ) ;
#5929 = CARTESIAN_POINT ( 'NONE',  ( 6.251467208264422482, 1.735085017428819931, -0.1376019381845137446 ) ) ;
#5930 = CARTESIAN_POINT ( 'NONE',  ( 3.878722286802076535, -0.2252994024176681598, -2.281293266731793778 ) ) ;
#5931 = CARTESIAN_POINT ( 'NONE',  ( 3.310337721246572773, 1.664907390794263531, 0.7863323413084821745 ) ) ;
#5932 = CARTESIAN_POINT ( 'NONE',  ( 9.094822116668764167, 9.505047312402055582, 0.7998128361456462443 ) ) ;
#5933 = CARTESIAN_POINT ( 'NONE',  ( 9.412522317677918693, 11.54714845510762267, -7.460155439063340665 ) ) ;
#5934 = CARTESIAN_POINT ( 'NONE',  ( 4.700122295916242088, -1.825221593135372578, -0.04401369772454033491 ) ) ;
#5935 = CARTESIAN_POINT ( 'NONE',  ( 5.151017605526480025, 0.9962996879465220168, 1.753031629501592192 ) ) ;
#5936 = CARTESIAN_POINT ( 'NONE',  ( -10.34217224912604571, 10.96028913360221502, 0.7998128361456462443 ) ) ;
#5938 = CARTESIAN_POINT ( 'NONE',  ( -7.608060475923978494, 8.905100639113307182, 1.199719254218452047 ) ) ;
#5937 = CARTESIAN_POINT ( 'NONE',  ( 3.010884265427976825, 1.639692042162781194, -1.559206548184206564 ) ) ;
#5939 = CARTESIAN_POINT ( 'NONE',  ( 5.544006925699364707, 0.8563935509715396854, -1.924162301928746821 ) ) ;
#5940 = CARTESIAN_POINT ( 'NONE',  ( 9.663580702207960726, 13.51594383518721365, 8.187698013202092895 ) ) ;
#5941 = CARTESIAN_POINT ( 'NONE',  ( 3.771986465066007099, -2.040223509676724500, 0.3510349978646867264 ) ) ;
#5942 = CARTESIAN_POINT ( 'NONE',  ( 9.028840231696797503, 12.62106513936658203, -1.199719254218446718 ) ) ;
#5943 = CARTESIAN_POINT ( 'NONE',  ( -1.360316468750018659, 2.401041667008069425, -0.7853790794159061228 ) ) ;
#5944 = CARTESIAN_POINT ( 'NONE',  ( 5.373730994130428762, 0.4134100146411868737, -2.079626175754036410 ) ) ;
#5945 = CONTEXT_DEPENDENT_SHAPE_REPRESENTATION ( #87995, #209683 ) ;
#5947 = CARTESIAN_POINT ( 'NONE',  ( 0.9086680563264810662, 1.459560178543020559, -1.257504221390127519 ) ) ;
#5946 = CARTESIAN_POINT ( 'NONE',  ( -9.854078719034067291, 10.39084668182823634, 0.7998128361456462443 ) ) ;
#5948 = CARTESIAN_POINT ( 'NONE',  ( 0.000000000000000000, 0.4330127018922214077, 0.000000000000000000 ) ) ;
#5949 = CARTESIAN_POINT ( 'NONE',  ( 0.3792734414799744380, -0.1002090192285705339, 1.967142940827655284 ) ) ;
#5950 = CARTESIAN_POINT ( 'NONE',  ( 3.879041346841291649, 7.539648981374564407, 1.040834085586084257E-14 ) ) ;
#5951 = CARTESIAN_POINT ( 'NONE',  ( 5.378845419373885051, 6.306261619127770501, 1.070519943709395960 ) ) ;
#5952 = DIRECTION ( 'NONE',  ( 0.000000000000000000, 0.000000000000000000, -1.000000000000000000 ) ) ;
#5953 = CARTESIAN_POINT ( 'NONE',  ( -3.066115294984855133, 6.728884944124295053, 0.7998128361456341429 ) ) ;
#5954 = CARTESIAN_POINT ( 'NONE',  ( 0.9849990780092006126, -1.403669121040777457, 1.721781922543249799 ) ) ;
#5955 = CARTESIAN_POINT ( 'NONE',  ( 2.784315802839703036, -1.083654668052931536, 1.805616322045165312 ) ) ;
#5956 = CARTESIAN_POINT ( 'NONE',  ( -6.050681693448748177, 10.28115541899069463, 0.7998128361456291469 ) ) ;
#5957 = CARTESIAN_POINT ( 'NONE',  ( 7.610204295972345712, 7.772993188256215547, 0.7998128361456341429 ) ) ;
#5958 = CARTESIAN_POINT ( 'NONE',  ( 1.047037934171668905, 1.643801913826014482, -0.8725737860223039544 ) ) ;
#5959 = CARTESIAN_POINT ( 'NONE',  ( 5.587931867126699537, 9.671004278289832001, -0.7998128361456291469 ) ) ;
#5960 = CARTESIAN_POINT ( 'NONE',  ( 11.96535697748077887, 9.847373329355470162, 0.9148528286454596925 ) ) ;
#5961 = CARTESIAN_POINT ( 'NONE',  ( -6.617788377246196951, 7.853746207276256719, -1.082531754730549967 ) ) ;
#5963 = CARTESIAN_POINT ( 'NONE',  ( -7.809133291791416909, 11.09411069285655493, 1.082531754730549967 ) ) ;
#5962 = AXIS2_PLACEMENT_3D ( 'NONE', #45770, #62003, #127084 ) ;
#5964 = CARTESIAN_POINT ( 'NONE',  ( 0.7914572142167939361, -0.05789999323873443182, -2.119991495365561640 ) ) ;
#5965 = CARTESIAN_POINT ( 'NONE',  ( -7.425025402139490360, 8.691559719698066289, 1.199719254218452047 ) ) ;
#5967 = CARTESIAN_POINT ( 'NONE',  ( 3.262109210011232108, -1.959739898415867154, 0.09363895518171151677 ) ) ;
#5966 = CARTESIAN_POINT ( 'NONE',  ( -1.151774525698488676E-14, 0.4375000000000101030, -1.414508159514601626 ) ) ;
#5968 = CARTESIAN_POINT ( 'NONE',  ( 1.745224485312408813, -1.826185749030174499, 1.156423465944363294 ) ) ;
#5969 = CARTESIAN_POINT ( 'NONE',  ( 1.927068723821170559, -1.203646435588998198, -1.393412863611859454 ) ) ;
#5971 = CARTESIAN_POINT ( 'NONE',  ( -5.796211742468360129, 6.069872997065163922, -0.5622600474686073602 ) ) ;
#5970 = CARTESIAN_POINT ( 'NONE',  ( -4.984557751679625781, 5.844347460828191565, 1.199719254218452935 ) ) ;
#5972 = CARTESIAN_POINT ( 'NONE',  ( 3.661793474361102252, -1.167423004587186952, 1.290856655984705670 ) ) ;
#5973 = CARTESIAN_POINT ( 'NONE',  ( 4.934804725694211136, 6.780358151441803649, -1.443375672974051449 ) ) ;
#5974 = CARTESIAN_POINT ( 'NONE',  ( -11.15881748666195072, 6.758040191959135079, 5.811769976250384495 ) ) ;
#5975 = AXIS2_PLACEMENT_3D ( 'NONE', #125796, #123675, #208014 ) ;
#5976 = CARTESIAN_POINT ( 'NONE',  ( 0.6905621207787122628, -2.145541755201633372, -0.2633910710312590275 ) ) ;
#5977 = ADVANCED_FACE ( 'NONE', ( #194125 ), #211187, .F. ) ;
#5978 = CARTESIAN_POINT ( 'NONE',  ( 2.882185300971401798, -0.2004049647258976941, 2.006138917898095730 ) ) ;
#5979 = CARTESIAN_POINT ( 'NONE',  ( 6.825078400183577365, 2.023440267519378999, 2.448151054272352578 ) ) ;
#5980 = CARTESIAN_POINT ( 'NONE',  ( 0.6554165194554737450, -1.826866057147133349, -1.155366728873077342 ) ) ;
#5981 = CARTESIAN_POINT ( 'NONE',  ( 1.744934968351062210, -1.666494570726485991, 1.053036000364399483 ) ) ;
#5982 = CARTESIAN_POINT ( 'NONE',  ( 6.609000000000034625, 7.052688111495289291, 2.598153854230552895 ) ) ;
#5983 = CARTESIAN_POINT ( 'NONE',  ( 2.015084816950295732, -1.883260942463622856, 0.4737542896416384597 ) ) ;
#5986 = ORIENTED_EDGE ( 'NONE', *, *, #186211, .T. ) ;
#5985 = CARTESIAN_POINT ( 'NONE',  ( -4.990809943606281607, 6.915973915664348937, -1.443375672974066548 ) ) ;
#5984 = FACE_OUTER_BOUND ( 'NONE', #161098, .T. ) ;
#5987 = CARTESIAN_POINT ( 'NONE',  ( -5.600926855776901192, 5.707038551260711579, -0.7216878364870338292 ) ) ;
#5988 = CARTESIAN_POINT ( 'NONE',  ( -0.1108833634137010027, 2.037774818562386514, -2.313487243312782216 ) ) ;
#5989 = CARTESIAN_POINT ( 'NONE',  ( 4.389807875774629942, 8.343469298370917997, 0.7998128361456271485 ) ) ;
#5990 = CARTESIAN_POINT ( 'NONE',  ( -6.981522756394290319, 7.109807735406931783, 0.7998128361456341429 ) ) ;
#5991 = CARTESIAN_POINT ( 'NONE',  ( -6.200875153403786477, 8.327716660428123419, -1.599625672291271394 ) ) ;
#5992 = CARTESIAN_POINT ( 'NONE',  ( -1.264911064067356206, 3.967544000579928287, -0.5000000000000004441 ) ) ;
#5993 = CARTESIAN_POINT ( 'NONE',  ( 6.405331179067034419, 1.913585160600343782, 1.289386977092843889 ) ) ;
#5994 = CARTESIAN_POINT ( 'NONE',  ( 6.812952578306354035, -1.517200236233799071, 1.243500037895750143 ) ) ;
#5995 = CARTESIAN_POINT ( 'NONE',  ( 4.205873059901494848, 0.6649649114027419428, -1.845726756006949909 ) ) ;
#5996 = CARTESIAN_POINT ( 'NONE',  ( 6.760712154708803823, 11.03924794713562818, 1.040834085586084257E-14 ) ) ;
#5997 = CARTESIAN_POINT ( 'NONE',  ( 1.934220422044399035, -1.621183349045727473, -1.198859219795316955 ) ) ;
#5998 = VERTEX_POINT ( 'NONE', #211450 ) ;
#5999 = CARTESIAN_POINT ( 'NONE',  ( 2.237658791021436056, 0.5595254372263277487, -2.042044324946710621 ) ) ;
#6000 = CARTESIAN_POINT ( 'NONE',  ( -0.7500000000000006661, 1.139583334016154526, -1.299038105676652011 ) ) ;
#6003 = ORIENTED_EDGE ( 'NONE', *, *, #129984, .T. ) ;
#6002 = CARTESIAN_POINT ( 'NONE',  ( -5.194745412330402878, 9.212286747694129474, 0.000000000000000000 ) ) ;
#6001 = FACE_OUTER_BOUND ( 'NONE', #149072, .T. ) ;
#6004 = CARTESIAN_POINT ( 'NONE',  ( 3.029072736150268952, -1.236975958831527445, -1.363863411116640334 ) ) ;
#6005 = ORIENTED_EDGE ( 'NONE', *, *, #94249, .T. ) ;
#6006 = CARTESIAN_POINT ( 'NONE',  ( -9.917953063596627317, 11.52969898140628047, -1.199719254218441611 ) ) ;
#6007 = CARTESIAN_POINT ( 'NONE',  ( -1.490514837427357131, 7.209629588552680879, 4.246172784736861772 ) ) ;
#6008 = CARTESIAN_POINT ( 'NONE',  ( 4.553055379497691568, 0.3652949536288411791, 2.088752307168060707 ) ) ;
#6009 = CARTESIAN_POINT ( 'NONE',  ( 0.07576575995338691305, -1.785066692240460551, -0.4505573523648154222 ) ) ;
#6010 = CARTESIAN_POINT ( 'NONE',  ( 0.7499999999999920064, 5.514583334016151639, 1.299038105676669330 ) ) ;
#6011 = CARTESIAN_POINT ( 'NONE',  ( 7.019370843573166319, 9.212351955633947043, 1.599625672291281386 ) ) ;
#6012 = CARTESIAN_POINT ( 'NONE',  ( 5.037736595929563244, 8.035053907629919223, -1.199719254218452047 ) ) ;
#6013 = EDGE_CURVE ( 'NONE', #130707, #106774, #129254, .T. ) ;
#6014 = CARTESIAN_POINT ( 'NONE',  ( 3.901680821178232339, -0.6019389665811913925, 1.970883251864594454 ) ) ;
#6016 = CARTESIAN_POINT ( 'NONE',  ( 1.944624168438695566, -1.479605912621816621, -1.095697124569312564 ) ) ;
#6015 = CARTESIAN_POINT ( 'NONE',  ( -5.540478329478883524, 9.615641817700700145, 0.000000000000000000 ) ) ;
#6017 = CARTESIAN_POINT ( 'NONE',  ( 5.111635199556411102, 6.706590097621358382, -1.441599559997795321 ) ) ;
#6018 = CARTESIAN_POINT ( 'NONE',  ( -5.070386261386537363, 5.017798181146802428, 1.214306433183764966E-14 ) ) ;
#6019 = DIRECTION ( 'NONE',  ( 0.000000000000000000, 0.000000000000000000, -1.000000000000000000 ) ) ;
#6020 = CARTESIAN_POINT ( 'NONE',  ( 10.95855051086948961, -7.723431457505071762, -0.6286713519883982970 ) ) ;
#6021 = CARTESIAN_POINT ( 'NONE',  ( 0.7157882511714327434, -0.3199875008889854766, 2.183444778895065941 ) ) ;
#6022 = CARTESIAN_POINT ( 'NONE',  ( 4.007294123747324299, 1.937827550919896336, 1.167430888521280963 ) ) ;
#6023 = CARTESIAN_POINT ( 'NONE',  ( -7.131225611108100715, 9.342849184424693476, 1.443375672974078761 ) ) ;
#6024 = CARTESIAN_POINT ( 'NONE',  ( 3.955163173390123799, -1.573275279051716158, 0.8980309717551668847 ) ) ;
#6025 = EDGE_CURVE ( 'NONE', #137219, #194636, #141360, .T. ) ;
#6026 = CARTESIAN_POINT ( 'NONE',  ( 4.153473468168114913, 1.856699357379907989, -0.4712526737844865976 ) ) ;
#6027 = CARTESIAN_POINT ( 'NONE',  ( 5.582505937350194181, 1.236201877336528643, -1.660625051266072960 ) ) ;
#6028 = CARTESIAN_POINT ( 'NONE',  ( 1.364683531249988535, 3.967708333674751842, -0.7879004041258239610 ) ) ;
#6029 = CARTESIAN_POINT ( 'NONE',  ( 4.205908039233514195, -1.966248567454803364, 0.1440612947745979200 ) ) ;
#6030 = CARTESIAN_POINT ( 'NONE',  ( 1.114139429068806919, -0.8636777455973219109, -1.721994443286285259 ) ) ;
#6031 = CARTESIAN_POINT ( 'NONE',  ( 3.625732356982212412, -1.113523340526129335, -1.502988901547596567 ) ) ;
#6032 = CARTESIAN_POINT ( 'NONE',  ( 3.967613463194498813, 0.2842429903056520324, -2.290057832888813483 ) ) ;
#6033 = CARTESIAN_POINT ( 'NONE',  ( 3.261990205869094162, -1.859054838292145240, 0.08865997893938745711 ) ) ;
#6034 = CARTESIAN_POINT ( 'NONE',  ( -0.6823417656250212460, 4.551041667008086655, 1.181850606188767472 ) ) ;
#6035 = CARTESIAN_POINT ( 'NONE',  ( 0.000000000000000000, 13.49999999999999822, 0.000000000000000000 ) ) ;
#6036 = CARTESIAN_POINT ( 'NONE',  ( 2.209725257209711469, -0.4604840958662699268, 2.054942820982478935 ) ) ;
#6037 = CARTESIAN_POINT ( 'NONE',  ( 4.338245966248566177, 4.163634503485842409, 1.214306433183764966E-14 ) ) ;
#6039 = CARTESIAN_POINT ( 'NONE',  ( 5.085343294144600179, 4.914812813773358435, 0.1758235994440172922 ) ) ;
#6038 = CARTESIAN_POINT ( 'NONE',  ( -1.201851678989727383E-14, 5.509375000341415252, -1.575800808251660134 ) ) ;
#6040 = CARTESIAN_POINT ( 'NONE',  ( -1.855128211190531395, 8.960462962215050453, -0.7749999999999996891 ) ) ;
#6041 = CARTESIAN_POINT ( 'NONE',  ( 3.568700945156903614, 0.7666329941097769218, 1.977337035738421900 ) ) ;
#6042 = DIRECTION ( 'NONE',  ( 0.000000000000000000, 0.000000000000000000, -1.000000000000000000 ) ) ;
#6043 = CARTESIAN_POINT ( 'NONE',  ( 1.177996693904998615, 1.989173073321507612, -0.3494277517126374577 ) ) ;
#6044 = CARTESIAN_POINT ( 'NONE',  ( -1.364683531250014514, 1.238541667008091096, -0.7879004041258289570 ) ) ;
#6045 = CARTESIAN_POINT ( 'NONE',  ( -2.494337075234348777, 5.853884321174607663, -0.7216878364870267237 ) ) ;
#6046 = CARTESIAN_POINT ( 'NONE',  ( 5.820528018968444961, 5.685037531751635953, 0.7998128361456341429 ) ) ;
#6047 = ORIENTED_EDGE ( 'NONE', *, *, #50358, .F. ) ;
#6048 = EDGE_CURVE ( 'NONE', #44585, #1117, #134517, .T. ) ;
#6049 = CARTESIAN_POINT ( 'NONE',  ( 1.036653925908154639, 2.129443126370239803, 0.3705773954724436159 ) ) ;
#6050 = FACE_OUTER_BOUND ( 'NONE', #40063, .T. ) ;
#6053 = CARTESIAN_POINT ( 'NONE',  ( 5.029711800989886683, 4.970344644017389513, 1.040834085586084257E-14 ) ) ;
#6052 = CARTESIAN_POINT ( 'NONE',  ( 6.825078400183510752, 3.697836898538444217, 2.470016017273040543 ) ) ;
#6051 = CARTESIAN_POINT ( 'NONE',  ( 6.008198349511364000, 7.038594824965278995, 1.199719254218453823 ) ) ;
#6054 = LINE ( 'NONE', #55898, #37491 ) ;
#6055 = CARTESIAN_POINT ( 'NONE',  ( 5.647672796105281279, 1.985869605424210649, -0.3494789899042491932 ) ) ;
#6056 = CARTESIAN_POINT ( 'NONE',  ( -9.002250809794013264, 9.604973487622245898, -0.7216878364870267237 ) ) ;
#6057 = CARTESIAN_POINT ( 'NONE',  ( 6.304249618663324561, 1.548718018665395713, -1.404690827926929453 ) ) ;
#6058 = CARTESIAN_POINT ( 'NONE',  ( 0.000000000000000000, 3.500000000000003109, 0.000000000000000000 ) ) ;
#6060 = CARTESIAN_POINT ( 'NONE',  ( -1.402160292154681736E-14, 12.17187500034140513, 1.575800808251682339 ) ) ;
#6059 = CARTESIAN_POINT ( 'NONE',  ( 0.8840797711214362087, 1.521441056815290516, 1.674750314396955542 ) ) ;
#6061 = CARTESIAN_POINT ( 'NONE',  ( -8.459397779922852578, 11.95671561229694824, 1.199719254218453823 ) ) ;
#6062 = CARTESIAN_POINT ( 'NONE',  ( 4.311732611912100666, -1.244383703160652610, -1.586670621409623116 ) ) ;
#6064 = CARTESIAN_POINT ( 'NONE',  ( 1.440887319015681012, -1.643870157486097217, -0.9831960898977005758 ) ) ;
#6063 = CARTESIAN_POINT ( 'NONE',  ( -6.710922848640111127, 6.931757532942661726, 0.7216878364870317197 ) ) ;
#6065 = CARTESIAN_POINT ( 'NONE',  ( 1.364683531249986537, 2.717708333674754062, -0.7879004041258239610 ) ) ;
#6066 = DIRECTION ( 'NONE',  ( 0.000000000000000000, 0.000000000000000000, 1.000000000000000000 ) ) ;
#6067 = CARTESIAN_POINT ( 'NONE',  ( -0.7500000000000006661, 9.708333333333332149, -1.299038105676657340 ) ) ;
#6068 = CARTESIAN_POINT ( 'NONE',  ( 3.351896425306086336, 1.725068445106912707, -0.001234800371389954687 ) ) ;
#6069 = CARTESIAN_POINT ( 'NONE',  ( 4.258142763143749399, 7.125527769379820242, 1.199719254218451159 ) ) ;
#6070 = CARTESIAN_POINT ( 'NONE',  ( 1.791920237496129609, -1.760627435414298558, -0.1794978127376868071 ) ) ;
#6071 = CARTESIAN_POINT ( 'NONE',  ( 5.051906976816819217, 0.6964463896041681590, -2.094057263239030853 ) ) ;
#6072 = VECTOR ( 'NONE', #69836, 1000.000000000000000 ) ;
#6073 = ORIENTED_EDGE ( 'NONE', *, *, #164541, .T. ) ;
#6074 = CARTESIAN_POINT ( 'NONE',  ( -5.250750630242457362, 9.347902511916677426, 0.000000000000000000 ) ) ;
#6076 = CARTESIAN_POINT ( 'NONE',  ( 4.323842328482737862, 0.8596156136044875717, -1.824127480631778875 ) ) ;
#6075 = CARTESIAN_POINT ( 'NONE',  ( 4.354221869268804390, 0.9056986662851629344, -1.917456963280274040 ) ) ;
#6077 = ORIENTED_EDGE ( 'NONE', *, *, #64021, .T. ) ;
#6078 = CARTESIAN_POINT ( 'NONE',  ( 6.086684617892325733, 6.065829907154645539, -0.7998128361456481317 ) ) ;
#6079 = VERTEX_POINT ( 'NONE', #186414 ) ;
#6080 = CARTESIAN_POINT ( 'NONE',  ( 1.920565142479381038, 1.744437793965779582, 0.6759427408406930571 ) ) ;
#6081 = LINE ( 'NONE', #137195, #51417 ) ;
#6082 = CARTESIAN_POINT ( 'NONE',  ( -0.1935108285373255133, -0.3924519521045151671, -1.774502223569380144 ) ) ;
#6083 = CARTESIAN_POINT ( 'NONE',  ( -3.789667630219657912, 4.380032642466370696, 1.199719254218462483 ) ) ;
#6084 = CARTESIAN_POINT ( 'NONE',  ( -10.71748749772954135, 5.309591131546671505, -6.727448623506740333 ) ) ;
#6085 = CARTESIAN_POINT ( 'NONE',  ( -0.7500000000000179856, 8.822916667349467446, 1.299038105676658228 ) ) ;
#6086 = ADVANCED_FACE ( 'NONE', ( #204780 ), #118293, .F. ) ;
#6087 = CARTESIAN_POINT ( 'NONE',  ( -1.201851678989727383E-14, 2.634375000341417916, 1.575800808251672791 ) ) ;
#6088 = CARTESIAN_POINT ( 'NONE',  ( 0.4395310841842985927, -1.815173276516974799, 0.6020934215927519206 ) ) ;
#6089 = VERTEX_POINT ( 'NONE', #101980 ) ;
#6090 = CARTESIAN_POINT ( 'NONE',  ( 5.370438244788902971, 9.279612028980123384, -0.7216878364870458196 ) ) ;
#6091 = EDGE_CURVE ( 'NONE', #92865, #210464, #15508, .T. ) ;
#6092 = CARTESIAN_POINT ( 'NONE',  ( -5.343321937561608337, 5.406499480009534508, 0.7216878364870257245 ) ) ;
#6093 = CARTESIAN_POINT ( 'NONE',  ( -6.934069218746458318, 7.054445274817795486, -0.7998128361456362523 ) ) ;
#6094 = CARTESIAN_POINT ( 'NONE',  ( 4.658503719480325600, 2.115088938745744329, 0.1532479335744420801 ) ) ;
#6096 = CARTESIAN_POINT ( 'NONE',  ( -11.14501278000869355, 7.223412960316487386, -3.546411330735405265 ) ) ;
#6095 = CARTESIAN_POINT ( 'NONE',  ( -0.1294898018151836583, 2.884012836773319766, -2.415168928093185396 ) ) ;
#6097 = CARTESIAN_POINT ( 'NONE',  ( 5.219980872528355853, -1.052265754357907701, -1.666845346888909729 ) ) ;
#6098 = CARTESIAN_POINT ( 'NONE',  ( 1.364683531249986537, 0.6552083336747522857, -0.7879004041258239610 ) ) ;
#6099 = CARTESIAN_POINT ( 'NONE',  ( 0.5275904727545431827, -0.2913634075805496271, 1.991877199276798516 ) ) ;
#6100 = EDGE_LOOP ( 'NONE', ( #55948, #47799, #113647, #88196 ) ) ;
#6101 = CARTESIAN_POINT ( 'NONE',  ( 0.2459221440733790898, 2.093483123843339122, -0.3155690596675052584 ) ) ;
#6102 = CARTESIAN_POINT ( 'NONE',  ( 1.662640112210824306, -0.7432673875312334477, -1.932532381715674097 ) ) ;
#6103 = EDGE_LOOP ( 'NONE', ( #150005, #196660 ) ) ;
#6104 = CARTESIAN_POINT ( 'NONE',  ( 6.378184920586140727, 6.405913593630768510, 0.000000000000000000 ) ) ;
#6105 = CARTESIAN_POINT ( 'NONE',  ( 6.059568310664962709, 6.034194215389424798, 0.7998128361456352531 ) ) ;
#6107 = CARTESIAN_POINT ( 'NONE',  ( 5.867981556616276073, 5.740399992340775803, -0.7998128361456281477 ) ) ;
#6106 = CARTESIAN_POINT ( 'NONE',  ( 4.330081446525359645, 2.050255175485806269, 0.4079974934644239326 ) ) ;
#6110 = ORIENTED_EDGE ( 'NONE', *, *, #176940, .T. ) ;
#6109 = CARTESIAN_POINT ( 'NONE',  ( 1.277659230087615727, 1.784704083969153920, -0.3092532468622013475 ) ) ;
#6108 = CARTESIAN_POINT ( 'NONE',  ( 3.117977517195897441, -0.8984765085307615529, -1.589086709143338272 ) ) ;
#6111 = CARTESIAN_POINT ( 'NONE',  ( 9.499606442108984083, -9.580649465752458127, -0.08647222121308514864 ) ) ;
#6112 = DIRECTION ( 'NONE',  ( 0.1674078377056216482, 0.000000000000000000, 0.9858877298530133171 ) ) ;
#6113 = CARTESIAN_POINT ( 'NONE',  ( 4.454274341225270994, 2.206355006892012138, -0.05062909709598743119 ) ) ;
#6114 = CARTESIAN_POINT ( 'NONE',  ( 8.606728586576791074, 8.935604860628076906, 0.7998128361456462443 ) ) ;
#6115 = CARTESIAN_POINT ( 'NONE',  ( -1.364683531250000748, 9.671875000341396245, 0.000000000000000000 ) ) ;
#6116 = EDGE_CURVE ( 'NONE', #186972, #144331, #164280, .T. ) ;
#6117 = CARTESIAN_POINT ( 'NONE',  ( 2.402860538037488780, -0.3286879766849961082, -1.883663324302800035 ) ) ;
#6118 = AXIS2_PLACEMENT_3D ( 'NONE', #74804, #144113, #58547 ) ;
#6119 = CARTESIAN_POINT ( 'NONE',  ( 7.476431642932036326, 10.80992178580769014, 1.199719254218460707 ) ) ;
#6120 = CARTESIAN_POINT ( 'NONE',  ( 6.619590326553026038, 0.3579758704960536719, -2.039031579972025554 ) ) ;
#6121 = CARTESIAN_POINT ( 'NONE',  ( 1.500000000000035971, 7.750000000000000000, 10.99818166789401275 ) ) ;
#6122 = CARTESIAN_POINT ( 'NONE',  ( 5.794512526436308875, 1.792401445336734733, -1.260760892635464980 ) ) ;
#6123 = CARTESIAN_POINT ( 'NONE',  ( 5.662876554447811017, 7.443216037249618999, -1.326882488215734845 ) ) ;
#6124 = CARTESIAN_POINT ( 'NONE',  ( -9.609247538824044810, -6.583727468838237229, 0.3728355200474647857 ) ) ;
#6125 = ORIENTED_EDGE ( 'NONE', *, *, #20625, .T. ) ;
#6126 = EDGE_LOOP ( 'NONE', ( #42355, #112917, #69573, #134900 ) ) ;
#6127 = CYLINDRICAL_SURFACE ( 'NONE', #144539, 1.500000000000000222 ) ;
#6128 = CARTESIAN_POINT ( 'NONE',  ( 3.215925951850879816, -0.9189154559356220719, -1.629173103855706906 ) ) ;
#6129 = DIRECTION ( 'NONE',  ( 0.000000000000000000, -1.000000000000000000, -9.023263958591317418E-17 ) ) ;
#6130 = CARTESIAN_POINT ( 'NONE',  ( -0.4019237886466966447, 12.58258545099816850, 1.500000000000003997 ) ) ;
#6131 = CARTESIAN_POINT ( 'NONE',  ( -8.188761592974058701, 8.655902734665618325, -0.7216878364870278340 ) ) ;
#6132 = CARTESIAN_POINT ( 'NONE',  ( 5.086243903782109221, 5.962981304947771122, -1.199719254218452047 ) ) ;
#6133 = CARTESIAN_POINT ( 'NONE',  ( 6.737176827083626307, -0.09545985418329960837, -2.068160202195384656 ) ) ;
#6134 = CARTESIAN_POINT ( 'NONE',  ( 0.6324356828835416833, 0.5880426346329314935, 1.928746166857209676 ) ) ;
#6135 = CARTESIAN_POINT ( 'NONE',  ( -8.727698198895085469, 11.20540053684285553, -1.599625672291263179 ) ) ;
#6136 = CARTESIAN_POINT ( 'NONE',  ( 5.110497557708379546, 4.926945003606695295, -0.7998128361456481317 ) ) ;
#6137 = CARTESIAN_POINT ( 'NONE',  ( 1.939652437182255662, 0.8368340126228106524, -2.025574644071465258 ) ) ;
#6138 = CARTESIAN_POINT ( 'NONE',  ( 5.496661139185262002, -0.4475443406098400523, -1.769863040007889410 ) ) ;
#6139 = CARTESIAN_POINT ( 'NONE',  ( -3.276266675996675204, 6.974061555304760240, -0.7998128361456281477 ) ) ;
#6140 = CARTESIAN_POINT ( 'NONE',  ( 6.238160076063542725, 6.450477308261824305, -0.7216878364870458196 ) ) ;
#6141 = CARTESIAN_POINT ( 'NONE',  ( 8.452618703115982512, 11.94880668935564216, 1.199719254218450271 ) ) ;
#6142 = CARTESIAN_POINT ( 'NONE',  ( -4.145761110728687804, 8.058748072483927771, -0.7998128361456481317 ) ) ;
#6143 = CARTESIAN_POINT ( 'NONE',  ( 5.840865249388943248, 5.708764300575555062, 0.7998128361456341429 ) ) ;
#6144 = CARTESIAN_POINT ( 'NONE',  ( 3.203469434578891661, 6.959407783642502565, -0.7998128361456362523 ) ) ;
#6145 = ORIENTED_EDGE ( 'NONE', *, *, #69227, .T. ) ;
#6147 = CARTESIAN_POINT ( 'NONE',  ( 6.275645410888611941, 0.3399709936107355168, -1.984134265935801000 ) ) ;
#6146 = CARTESIAN_POINT ( 'NONE',  ( 3.087279721815265443, -0.7436087841871074078, 1.684586988852328160 ) ) ;
#6148 = CARTESIAN_POINT ( 'NONE',  ( 1.476342052747819045, 2.027250371889641301, 1.083024425860839690 ) ) ;
#6150 = CARTESIAN_POINT ( 'NONE',  ( 0.3911518402437937358, -1.704754640775848928, 0.7467128926999586636 ) ) ;
#6149 = CARTESIAN_POINT ( 'NONE',  ( 2.575685996916329046, 5.948791396470269888, 0.7216878364870438212 ) ) ;
#6151 = CARTESIAN_POINT ( 'NONE',  ( -5.901876940650454095, 5.779944607047298177, -0.7998128361456291469 ) ) ;
#6152 = CARTESIAN_POINT ( 'NONE',  ( 10.09384670631060921, -7.616807780225003377, 9.269928574751062911E-15 ) ) ;
#6153 = CARTESIAN_POINT ( 'NONE',  ( 3.093911922779784440, 1.216618333484908998, 1.475457842794763996 ) ) ;
#6154 = B_SPLINE_CURVE_WITH_KNOTS ( 'NONE', 3,
 ( #90588, #58065, #41844, #107956, #208558, #175039, #76445, #91666, #9314, #75390 ),
 .UNSPECIFIED., .F., .F.,
 ( 4, 3, 3, 4 ),
 ( 0.000000000000000000, 4.502046072369012122E-05, 9.004093402560476938E-05, 0.0001800865003230942441 ),
 .UNSPECIFIED. ) ;
#6155 = CARTESIAN_POINT ( 'NONE',  ( -9.809487834687324437, 11.40315621434539395, 1.199719254218462483 ) ) ;
#6156 = CARTESIAN_POINT ( 'NONE',  ( 6.361499291607088935, 6.832587723092125032, 0.6030276918116053153 ) ) ;
#6157 = CARTESIAN_POINT ( 'NONE',  ( -6.563555762791521531, 9.711213252348503744, 1.082531754730549967 ) ) ;
#6159 = CARTESIAN_POINT ( 'NONE',  ( 1.639302681421180852, -1.352760811461351187, -1.292285834730775074 ) ) ;
#6158 = CARTESIAN_POINT ( 'NONE',  ( 2.454727380131729753, -1.820530515947630379, -1.027877103350574250 ) ) ;
#6160 = CARTESIAN_POINT ( 'NONE',  ( 1.581407437776818581, 1.356094323556347181, -1.492024998029889638 ) ) ;
#6161 = CARTESIAN_POINT ( 'NONE',  ( 9.422553571817644524, 10.09532670998316384, 0.000000000000000000 ) ) ;
#6162 = CARTESIAN_POINT ( 'NONE',  ( -1.364683531250012516, 3.551041667008085323, -0.7879004041258300672 ) ) ;
#6163 = CARTESIAN_POINT ( 'NONE',  ( 3.403587037673636129, -0.7086591031593177936, -1.589830453666951415 ) ) ;
#6164 = CARTESIAN_POINT ( 'NONE',  ( 3.147464216666835402, 6.823792019419957278, -0.7998128361456291469 ) ) ;
#6166 = CARTESIAN_POINT ( 'NONE',  ( 0.4134119952316945845, 3.004821906555924738, -2.020258976488587432 ) ) ;
#6165 = CARTESIAN_POINT ( 'NONE',  ( 0.000000000000000000, -1.500000000000001332, 0.000000000000000000 ) ) ;
#6167 = CARTESIAN_POINT ( 'NONE',  ( 3.808989599770518097, 1.480563749658039052, 0.8846867361136273589 ) ) ;
#6168 =( BOUNDED_CURVE ( )  B_SPLINE_CURVE ( 2, ( #149856, #1424, #202829, #120623, #183402, #82696, #35006 ),
 .UNSPECIFIED., .F., .T. ) 
 B_SPLINE_CURVE_WITH_KNOTS ( ( 3, 2, 2, 3 ),
 ( 0.2250000000000001998, 0.2291666666666668517, 0.2333333333333335313, 0.2375000000000001832 ),
 .UNSPECIFIED. ) 
 CURVE ( )  GEOMETRIC_REPRESENTATION_ITEM ( )  RATIONAL_B_SPLINE_CURVE ( ( 0.9999999999999937828, 0.8660254037844449249, 1.000000000000000000, 0.8660254037844387076, 1.000000000000000000, 0.8660254037844324904, 1.000000000000006217 ) ) 
 REPRESENTATION_ITEM ( '' )  );
#6169 = CARTESIAN_POINT ( 'NONE',  ( 2.243918346939121733, 2.191141468336772036, 0.05030144379260945153 ) ) ;
#6170 = CARTESIAN_POINT ( 'NONE',  ( 5.356176587289051660, 2.204499490778097481, -0.1052899746726426722 ) ) ;
#6171 = CARTESIAN_POINT ( 'NONE',  ( -9.587917471435847716, 4.026361754648488223, -6.670783315233271615 ) ) ;
#6172 = CARTESIAN_POINT ( 'NONE',  ( 3.889651762418313119, -2.008042162167834377, 0.8258804214429303903 ) ) ;
#6173 = CARTESIAN_POINT ( 'NONE',  ( 2.613660848560446226, -1.805822647967849193, 0.2677728182119283318 ) ) ;
#6174 = CARTESIAN_POINT ( 'NONE',  ( -1.115562610750309283E-14, 9.343750000682801371, 1.500000000000001554 ) ) ;
#6175 = CARTESIAN_POINT ( 'NONE',  ( 4.839118085652931001, -1.790413437384326789, -1.129994989630648261 ) ) ;
#6176 = CARTESIAN_POINT ( 'NONE',  ( 6.639320575229259447, 2.969246179279591225, 2.450030562065998119 ) ) ;
#6177 = VERTEX_POINT ( 'NONE', #87865 ) ;
#6178 = VECTOR ( 'NONE', #132004, 1000.000000000000000 ) ;
#6180 = CARTESIAN_POINT ( 'NONE',  ( -1.201851678989727383E-14, 2.134375000341423689, 1.575800808251672791 ) ) ;
#6179 = CARTESIAN_POINT ( 'NONE',  ( 4.546573649138107243, -1.841725595444974939, 1.364713657601625885 ) ) ;
#6181 = CARTESIAN_POINT ( 'NONE',  ( 0.6124999999999880540, 0.1666666666666899443, -1.060881119635979530 ) ) ;
#6182 = CARTESIAN_POINT ( 'NONE',  ( 3.460355519985863548, 5.060167411448709629, 1.599625672291267398 ) ) ;
#6183 = CARTESIAN_POINT ( 'NONE',  ( 0.06529689308308950224, -1.700389599856198863, 1.266735544122286283 ) ) ;
#6184 = CARTESIAN_POINT ( 'NONE',  ( -6.236387472606166327, 6.378132927569716060, -0.7216878364870278340 ) ) ;
#6185 = CARTESIAN_POINT ( 'NONE',  ( 3.551873057100287223, 5.166937871415542283, 1.443375672974062551 ) ) ;
#6186 = CARTESIAN_POINT ( 'NONE',  ( -6.548225005276122168, 6.741943382351338165, 0.7216878364870317197 ) ) ;
#6187 = DIRECTION ( 'NONE',  ( 5.578564026256490882E-16, 1.000000000000000000, 9.066213480720158442E-32 ) ) ;
#6188 = ORIENTED_EDGE ( 'NONE', *, *, #207750, .F. ) ;
#6189 = CARTESIAN_POINT ( 'NONE',  ( 5.309220276109914316, 1.198862193007979471, -1.621181151826488254 ) ) ;
#6191 = CARTESIAN_POINT ( 'NONE',  ( 3.713784835328519218, 0.5057260441109856508, -1.999473844451674642 ) ) ;
#6190 = CARTESIAN_POINT ( 'NONE',  ( 4.462605117192430804, 8.358123070033169455, 1.040834085586084257E-14 ) ) ;
#6193 = CARTESIAN_POINT ( 'NONE',  ( -0.2411972340276204718, 2.032951786628557134, -2.316127775276015655 ) ) ;
#6192 = CARTESIAN_POINT ( 'NONE',  ( 6.156284269057003655, 9.340026192945279249, -1.199719254218452047 ) ) ;
#6194 = CARTESIAN_POINT ( 'NONE',  ( 7.374709211190586089, 7.568525266002632534, 0.000000000000000000 ) ) ;
#6195 = CARTESIAN_POINT ( 'NONE',  ( 3.285556943749998737, -1.655208332855374609, -1.896917185911906500 ) ) ;
#6196 = DIRECTION ( 'NONE',  ( 0.000000000000000000, -1.000000000000000000, 0.000000000000000000 ) ) ;
#6197 = CARTESIAN_POINT ( 'NONE',  ( 6.017560223340764125, -1.214513600917455083, -1.823921334435735231 ) ) ;
#6198 = CARTESIAN_POINT ( 'NONE',  ( 3.850232551101365086, 0.2440307281281335616, -2.001511205109906655 ) ) ;
#6199 = CARTESIAN_POINT ( 'NONE',  ( 3.298233973420101606, 1.449563003725433896, -1.135193286699177628 ) ) ;
#6200 = CARTESIAN_POINT ( 'NONE',  ( 6.440286661691305703, 7.472421512516709718, 1.199719254218462483 ) ) ;
#6201 = SURFACE_SIDE_STYLE ('',( #206551 ) ) ;
#6202 = CARTESIAN_POINT ( 'NONE',  ( 0.4281588809218932479, 1.648258183568848789, 0.5080355103465240552 ) ) ;
#6203 = DIRECTION ( 'NONE',  ( -3.451266460341926649E-31, -5.200009205990155575E-32, 1.000000000000000000 ) ) ;
#6204 = CARTESIAN_POINT ( 'NONE',  ( 0.5108563537194388271, -2.180326652049785707, 0.7283127579034570642 ) ) ;
#6205 = CARTESIAN_POINT ( 'NONE',  ( -5.554036483092550824, 9.631459663583308739, -0.7998128361456231517 ) ) ;
#6206 = CARTESIAN_POINT ( 'NONE',  ( 6.666858444607468570, -2.065188582200903955, -0.9245386165244884324 ) ) ;
#6207 = CARTESIAN_POINT ( 'NONE',  ( 2.578859754595532294, -2.015555182639038101, -0.6107849380157669428 ) ) ;
#6208 = CARTESIAN_POINT ( 'NONE',  ( -3.935609729716867289, 7.813571461303467913, 0.7998128361456352531 ) ) ;
#6209 = CARTESIAN_POINT ( 'NONE',  ( 6.968000882419564945, 10.21675256520979858, 1.199719254218460707 ) ) ;
#6210 = CARTESIAN_POINT ( 'NONE',  ( 6.549997608733495902, 7.774656977344789333, -1.082531754730548412 ) ) ;
#6211 = CARTESIAN_POINT ( 'NONE',  ( -5.228640796364566690, 9.251831362400652736, -0.7998128361456231517 ) ) ;
#6212 = CARTESIAN_POINT ( 'NONE',  ( 6.765155463094751909, 8.915767345075790828, 1.443375672974076540 ) ) ;
#6213 = CARTESIAN_POINT ( 'NONE',  ( 4.247106804623488330, 7.517614509530361033, 0.9983198370346995087 ) ) ;
#6214 = EDGE_CURVE ( 'NONE', #103536, #133104, #63815, .T. ) ;
#6215 = CARTESIAN_POINT ( 'NONE',  ( -4.086893239515592136, 6.855460315155083251, 1.199719254218464037 ) ) ;
#6217 = CARTESIAN_POINT ( 'NONE',  ( 4.377308812845062569, -1.984989629755340435, -0.9973083610524589027 ) ) ;
#6216 = CARTESIAN_POINT ( 'NONE',  ( 2.180079139336263516, 2.078761533942363737, -0.4183221158333137457 ) ) ;
#6218 = CARTESIAN_POINT ( 'NONE',  ( 2.150558370509841666, -1.692889690492072718, 1.391600924549152296 ) ) ;
#6219 = CARTESIAN_POINT ( 'NONE',  ( -6.413170354464012846, 7.440785820751486312, 1.199719254218450271 ) ) ;
#6220 = CARTESIAN_POINT ( 'NONE',  ( -5.041653019435350380, 6.975290837464928728, -1.599625672291271394 ) ) ;
#6221 = CARTESIAN_POINT ( 'NONE',  ( 5.740667459973674447, -1.913685094937540132, -0.4313615418530327150 ) ) ;
#6222 = CARTESIAN_POINT ( 'NONE',  ( 1.364683531249986537, 1.405208333674755838, -0.7879004041258239610 ) ) ;
#6223 = CARTESIAN_POINT ( 'NONE',  ( -5.180624094197616714, 5.216685329418210948, 0.7216878364870257245 ) ) ;
#6224 = CARTESIAN_POINT ( 'NONE',  ( -5.694061328059534688, 8.626526735169329996, 1.082531754730548412 ) ) ;
#6226 = CARTESIAN_POINT ( 'NONE',  ( 4.183913158364858553, 2.056144659531285779, -0.5182805708664262045 ) ) ;
#6225 = VECTOR ( 'NONE', #14403, 1000.000000000000000 ) ;
#6227 = CARTESIAN_POINT ( 'NONE',  ( -3.851398154733808088, 6.650992392901508232, -1.199719254218450271 ) ) ;
#6228 = VERTEX_POINT ( 'NONE', #168049 ) ;
#6229 = CARTESIAN_POINT ( 'NONE',  ( 5.067319851952804655, 0.2155487944876262052, -2.150937003660175595 ) ) ;
#6230 = CARTESIAN_POINT ( 'NONE',  ( 7.006866460164219212, 7.069099046480051385, -0.7998128361456281477 ) ) ;
#6231 = CARTESIAN_POINT ( 'NONE',  ( 4.669393045487420402, 1.064170941109745305, 1.502380130741477693 ) ) ;
#6232 = FACE_OUTER_BOUND ( 'NONE', #129039, .T. ) ;
#6233 = CARTESIAN_POINT ( 'NONE',  ( -1.402160292154681736E-14, 1.009375000341417916, -1.575800808251659024 ) ) ;
#6234 = CARTESIAN_POINT ( 'NONE',  ( 0.3271923042600047848, 0.8970799620377118977, -1.491255180049656071 ) ) ;
#6236 = EDGE_CURVE ( 'NONE', #94475, #67360, #7009, .T. ) ;
#6235 = CARTESIAN_POINT ( 'NONE',  ( 6.727182134110257117, 2.064761932694148872, 2.218145506119094890 ) ) ;
#6237 = CARTESIAN_POINT ( 'NONE',  ( 4.067082894419602468, 3.847277586352047862, -0.7216878364870188411 ) ) ;
#6238 = DIRECTION ( 'NONE',  ( 0.000000000000000000, 1.000000000000000000, 0.000000000000000000 ) ) ;
#6239 = CARTESIAN_POINT ( 'NONE',  ( 4.188458007013862172, -2.137797052781073237, -0.3198388112101158143 ) ) ;
#6240 = EDGE_CURVE ( 'NONE', #180436, #147186, #129871, .T. ) ;
#6241 = CARTESIAN_POINT ( 'NONE',  ( -3.262708522383007903, 6.958243709422141876, 1.040834085586084257E-14 ) ) ;
#6242 = CARTESIAN_POINT ( 'NONE',  ( -7.687109908824056426, 8.070642436490613747, 0.7216878364870438212 ) ) ;
#6244 = CIRCLE ( 'NONE', #51117, 0.08000000000000020983 ) ;
#6243 = STYLED_ITEM ( 'NONE', ( #12046 ), #202610 ) ;
#6245 = CARTESIAN_POINT ( 'NONE',  ( 3.063507763784904192, 0.3185916186679502715, -2.137983152197140413 ) ) ;
#6246 = CARTESIAN_POINT ( 'NONE',  ( 4.956303624527079066, 0.7517850369052423432, 1.822569506419220220 ) ) ;
#6247 = CARTESIAN_POINT ( 'NONE',  ( 3.479597601185040912, 1.566717760139114901, 0.7430284921127163766 ) ) ;
#6248 = CARTESIAN_POINT ( 'NONE',  ( 0.8553300576445364012, 0.4222666777726029608, -2.150330908352434012 ) ) ;
#6249 = CARTESIAN_POINT ( 'NONE',  ( 0.8159566880532771460, -0.3350741789154148553, 2.283031499596111402 ) ) ;
#6250 = CARTESIAN_POINT ( 'NONE',  ( 4.077457721052785367, 1.941698500476006117, -0.6908173846359686454 ) ) ;
#6251 = CARTESIAN_POINT ( 'NONE',  ( 5.829623785595809515, 0.9536246560681378437, -1.691722214391349732 ) ) ;
#6252 = CARTESIAN_POINT ( 'NONE',  ( -8.148087131688692253, 10.52918762510205042, -1.443375672974058777 ) ) ;
#6253 = CARTESIAN_POINT ( 'NONE',  ( -3.955946960137363799, 7.837298230127379917, 0.7998128361456352531 ) ) ;
#6254 = CARTESIAN_POINT ( 'NONE',  ( -7.334597915313094241, 9.580116872663850813, 1.040834085586084257E-14 ) ) ;
#6255 = EDGE_LOOP ( 'NONE', ( #29576, #72057, #160236, #82265 ) ) ;
#6256 = CARTESIAN_POINT ( 'NONE',  ( -8.636180661780672452, 9.177891648273343250, -0.7216878364870267237 ) ) ;
#6257 = CARTESIAN_POINT ( 'NONE',  ( 3.557846488308267663, 0.5383450771202847873, -2.139971664446515653 ) ) ;
#6258 = CARTESIAN_POINT ( 'NONE',  ( -3.285556943750000514, -3.026041666188709733, -1.896917185911906500 ) ) ;
#6259 = ORIENTED_EDGE ( 'NONE', *, *, #211265, .F. ) ;
#6260 = CARTESIAN_POINT ( 'NONE',  ( 1.094327318609791710, 1.832149372150039479, 0.3252389950085340375 ) ) ;
#6261 = CARTESIAN_POINT ( 'NONE',  ( -0.02900071798684483726, 7.629137130509101361, -2.773797386654376584 ) ) ;
#6262 = CARTESIAN_POINT ( 'NONE',  ( -0.7499999999999972244, 5.389583334016151639, -1.299038105676652899 ) ) ;
#6263 = DIRECTION ( 'NONE',  ( 0.000000000000000000, 0.000000000000000000, -1.000000000000000000 ) ) ;
#6265 = CARTESIAN_POINT ( 'NONE',  ( 0.1253635393240644380, 7.629137130509072051, -2.744100600304347104 ) ) ;
#6264 = CARTESIAN_POINT ( 'NONE',  ( -6.245422037512663671, 7.006708691962935553, -1.003398212925192157 ) ) ;
#6266 = CARTESIAN_POINT ( 'NONE',  ( 6.562460610575872266, -1.685528226061007162, -0.7412392050258274079 ) ) ;
#6267 = VERTEX_POINT ( 'NONE', #36970 ) ;
#6268 = CARTESIAN_POINT ( 'NONE',  ( 1.991158371866567967, 1.793705239296649045, -1.014668517943543513 ) ) ;
#6269 = CARTESIAN_POINT ( 'NONE',  ( -0.6801582343750282034, 0.8489583336747236197, -1.178068619123876282 ) ) ;
#6270 = CARTESIAN_POINT ( 'NONE',  ( -7.393273838153706201, 7.519907654134449615, 0.7998128361456341429 ) ) ;
#6271 = DIRECTION ( 'NONE',  ( 0.6029061840396385819, 0.7978120914393070917, 0.000000000000000000 ) ) ;
#6272 = FACE_OUTER_BOUND ( 'NONE', #116734, .T. ) ;
#6273 = CARTESIAN_POINT ( 'NONE',  ( 3.659811400685081040, 6.357198169852855685, -1.199719254218446718 ) ) ;
#6274 = CARTESIAN_POINT ( 'NONE',  ( 1.024374290915401442, 1.228313541842564138, -1.654675390109799693 ) ) ;
#6276 = CARTESIAN_POINT ( 'NONE',  ( 4.212339636135824961, 1.685202893791247769, 0.7422218904534692019 ) ) ;
#6275 = CARTESIAN_POINT ( 'NONE',  ( -11.40591166468356654, 3.507114751586590362, 3.706005353348402753 ) ) ;
#6277 = CARTESIAN_POINT ( 'NONE',  ( 6.440286661691305703, 7.472421512516709718, 1.199719254218462483 ) ) ;
#6278 = AXIS2_PLACEMENT_3D ( 'NONE', #155863, #25839, #24775 ) ;
#6279 = CARTESIAN_POINT ( 'NONE',  ( -6.466312919074983512, 6.508729591867735031, -0.7998128361456362523 ) ) ;
#6280 = CARTESIAN_POINT ( 'NONE',  ( 5.760442859251142522, 0.8911043219209063837, 2.019162844794204048 ) ) ;
#6281 = CARTESIAN_POINT ( 'NONE',  ( 0.4741787938652639034, 1.244221353789766837, 1.767418780601250017 ) ) ;
#6282 = CARTESIAN_POINT ( 'NONE',  ( -3.619663825168619731, 7.166765529431275539, 1.040834085586084257E-14 ) ) ;
#6283 = CARTESIAN_POINT ( 'NONE',  ( 0.5449873876890098945, 0.1430962203496731200, 1.907122450762772647 ) ) ;
#6284 = CARTESIAN_POINT ( 'NONE',  ( 1.235564962061060257, 0.5807501988173838781, -1.931125984888550473 ) ) ;
#6285 = VECTOR ( 'NONE', #132442, 1000.000000000000000 ) ;
#6286 = DIRECTION ( 'NONE',  ( 0.000000000000000000, 1.000000000000000000, 0.000000000000000000 ) ) ;
#6287 = CARTESIAN_POINT ( 'NONE',  ( -0.4170821662629227156, 3.033599471985643170, 0.4170821662629036752 ) ) ;
#6288 = CARTESIAN_POINT ( 'NONE',  ( 6.463533315534490065, -1.538886664202097965, -1.134999244291827747 ) ) ;
#6289 = LINE ( 'NONE', #205566, #12324 ) ;
#6290 = CARTESIAN_POINT ( 'NONE',  ( 1.393192293617943944, 1.414286473764417185, 1.224485199485196629 ) ) ;
#6291 = CARTESIAN_POINT ( 'NONE',  ( 2.448454179885679149, -1.387098808145654560, 1.463928423225707931 ) ) ;
#6293 = CARTESIAN_POINT ( 'NONE',  ( 6.639320575229282539, 7.629137130509070275, 2.703262396134015866 ) ) ;
#6292 = CARTESIAN_POINT ( 'NONE',  ( -0.6823417656250212460, 1.051041667008083325, 1.181850606188755259 ) ) ;
#6295 = CARTESIAN_POINT ( 'NONE',  ( 5.672525241255916839, -1.337268198843853506, 1.627036470456619810 ) ) ;
#6294 = CARTESIAN_POINT ( 'NONE',  ( -9.203287345578106127, 9.631590079462940324, 0.7998128361456462443 ) ) ;
#6296 = CARTESIAN_POINT ( 'NONE',  ( 8.633844893804129228, 8.967240552393299424, -0.7998128361456211532 ) ) ;
#6298 = CARTESIAN_POINT ( 'NONE',  ( -7.316596452869116973, 11.68777962832266049, 0.7998128361456481317 ) ) ;
#6297 = CARTESIAN_POINT ( 'NONE',  ( 5.086243903782109221, 5.962981304947771122, -1.199719254218452047 ) ) ;
#6299 = CARTESIAN_POINT ( 'NONE',  ( 3.987289958883693419, 7.308088843452864580, 0.8820050823528166051 ) ) ;
#6300 = CARTESIAN_POINT ( 'NONE',  ( 4.025652601906283046, -0.3410878217046057204, 1.990599050954243054 ) ) ;
#6301 = B_SPLINE_CURVE_WITH_KNOTS ( 'NONE', 3,
 ( #149473, #168910, #166791, #150553, #202449, #74359, #67121, #54104, #50905, #35706, #84462, #172938, #186217, #140462, #115963, #100714, #99654, #165723, #133254, #117033, #183028, #34644, #18385, #68188, #200326, #101783, #167850, #138143 ),
 .UNSPECIFIED., .F., .F.,
 ( 4, 3, 3, 3, 3, 3, 3, 3, 3, 4 ),
 ( 0.000000000000000000, 1.600956980237147682E-05, 1.644526376030698057E-05, 3.791386034648869355E-05, 4.420234518516011314E-05, 5.951836916331200894E-05, 6.580566471116502784E-05, 8.237066101204505307E-05, 0.0001137110868648263224, 0.0001607716038169918046 ),
 .UNSPECIFIED. ) ;
#6302 = CARTESIAN_POINT ( 'NONE',  ( -0.6823417656249969321, 5.217708333674756283, -1.181850606188749264 ) ) ;
#6303 = CARTESIAN_POINT ( 'NONE',  ( 6.742638559370645268, -2.022111636011727498, -0.4062529910623476903 ) ) ;
#6304 = CARTESIAN_POINT ( 'NONE',  ( 9.408995418203971894, 11.03987807840189816, 1.082531754730549967 ) ) ;
#6305 = EDGE_CURVE ( 'NONE', #19175, #99973, #137695, .T. ) ;
#6306 = CARTESIAN_POINT ( 'NONE',  ( 4.973979902034267653, 1.240098594129716458, 1.770319513135506062 ) ) ;
#6307 = CARTESIAN_POINT ( 'NONE',  ( 7.374709211190586089, 7.568525266002632534, 0.000000000000000000 ) ) ;
#6308 = CARTESIAN_POINT ( 'NONE',  ( -1.499999999999997780, 5.900000000000023448, 1.214306433183764966E-14 ) ) ;
#6310 = CARTESIAN_POINT ( 'NONE',  ( -2.081668171172168513E-14, 2.800000000000024691, 2.500000000000011102 ) ) ;
#6309 = CARTESIAN_POINT ( 'NONE',  ( 4.667750024854814050, 8.667735138964429709, -0.7998128361456381397 ) ) ;
#6311 = CARTESIAN_POINT ( 'NONE',  ( 6.249945625775433555, 10.23542763013927726, -0.7216878364870267237 ) ) ;
#6313 = CARTESIAN_POINT ( 'NONE',  ( 0.08058605481615531418, -8.243759731405756241, 10.99970480911961701 ) ) ;
#6312 = CARTESIAN_POINT ( 'NONE',  ( 2.031898538270035637, 2.078123050159206286, -0.6288832818364347155 ) ) ;
#6315 = CARTESIAN_POINT ( 'NONE',  ( 1.909461114401575843, -0.8690924446688346183, -1.623246667998109682 ) ) ;
#6314 = CARTESIAN_POINT ( 'NONE',  ( -4.921246572080546500, 8.685278734161874681, 1.214306433183764966E-14 ) ) ;
#6316 = CARTESIAN_POINT ( 'NONE',  ( 1.364683531249990311, 2.884375000341422801, 1.214306433183764966E-14 ) ) ;
#6317 = CARTESIAN_POINT ( 'NONE',  ( 2.771223791512751333, 2.080116120148074010, -0.6901165687889164735 ) ) ;
#6318 = CARTESIAN_POINT ( 'NONE',  ( 6.883263157960364254, 2.431740398616466070, 2.435552827938294751 ) ) ;
#6319 = CARTESIAN_POINT ( 'NONE',  ( 3.942437297418455611, 2.251314906739984245, 0.2249487974115715883 ) ) ;
#6320 = CARTESIAN_POINT ( 'NONE',  ( -7.217017841176048165, 7.314275657660511243, 1.040834085586084257E-14 ) ) ;
#6321 = CARTESIAN_POINT ( 'NONE',  ( -1.500000000000038636, 7.750000000000000000, -10.64483442802187341 ) ) ;
#6322 = CARTESIAN_POINT ( 'NONE',  ( 6.490673131624099312, 6.748652840683030618, -0.08655830178419705867 ) ) ;
#6323 = CARTESIAN_POINT ( 'NONE',  ( 0.7500000000000006661, 13.66666666666666785, -1.299038105676657340 ) ) ;
#6324 = CARTESIAN_POINT ( 'NONE',  ( 6.061904079085887354, 6.244845311787889486, 0.000000000000000000 ) ) ;
#6325 = EDGE_CURVE ( 'NONE', #54346, #18903, #212804, .T. ) ;
#6326 = CARTESIAN_POINT ( 'NONE',  ( 5.061649853805494814, 1.750434175623495348, -0.2595850195740417310 ) ) ;
#6327 = CARTESIAN_POINT ( 'NONE',  ( 7.690499447449630210, 9.995335326823163058, 1.599625672291281386 ) ) ;
#6328 = CARTESIAN_POINT ( 'NONE',  ( 2.432770431885710405, 2.042423857386191255, 0.5128348284264750978 ) ) ;
#6330 = CARTESIAN_POINT ( 'NONE',  ( -0.7500000000000006661, 1.358333333333357151, -1.299038105676652011 ) ) ;
#6329 = CARTESIAN_POINT ( 'NONE',  ( 0.6823417656249969321, 10.52604166700806587, -1.181850606188757036 ) ) ;
#6331 = CARTESIAN_POINT ( 'NONE',  ( 1.223035424556912387, -1.779184897175438707, -0.8450996447877844320 ) ) ;
#6332 = VECTOR ( 'NONE', #120431, 1000.000000000000000 ) ;
#6333 = CARTESIAN_POINT ( 'NONE',  ( -3.149236820124241110, 6.896136400112061970, -0.7998128361456481317 ) ) ;
#6334 = CARTESIAN_POINT ( 'NONE',  ( 0.2913577194270203785, -1.795273245208812485, 0.7915465721433642132 ) ) ;
#6336 = EDGE_LOOP ( 'NONE', ( #159596, #69246, #49544, #120406, #150047, #16458 ) ) ;
#6335 = CARTESIAN_POINT ( 'NONE',  ( 5.449399174529797385, -1.634242350402253852, 0.7820841365046418137 ) ) ;
#6337 = CARTESIAN_POINT ( 'NONE',  ( 6.805829924380118356, 7.042482454639357847, 0.7216878364870317197 ) ) ;
#6338 = CARTESIAN_POINT ( 'NONE',  ( -1.364683531250000748, -1.178124999658580752, 0.000000000000000000 ) ) ;
#6339 = CARTESIAN_POINT ( 'NONE',  ( 5.295714669793899709, -0.6724083694377264164, 1.745798414713333413 ) ) ;
#6340 = CARTESIAN_POINT ( 'NONE',  ( 3.029357257649615054, 5.621668336311468117, -1.199719254218446718 ) ) ;
#6341 = CARTESIAN_POINT ( 'NONE',  ( 5.084861876562203342, 1.979495018489594305, 0.6061691862097525751 ) ) ;
#6342 = CARTESIAN_POINT ( 'NONE',  ( -1.225000000000042277, 2.479166666666715368, -0.7072540797573197979 ) ) ;
#6343 = CARTESIAN_POINT ( 'NONE',  ( -5.058600711230246461, 7.955432358860325515, 1.082531754730549967 ) ) ;
#6344 = CARTESIAN_POINT ( 'NONE',  ( 3.187124369784331002, -0.9488429814887938685, 1.145676217959502585 ) ) ;
#6345 = CARTESIAN_POINT ( 'NONE',  ( 6.428537391173986038, 10.65171072301167854, 0.7998128361456462443 ) ) ;
#6346 = CARTESIAN_POINT ( 'NONE',  ( -8.829384350997580455, 11.32403438096243775, 1.599625672291269396 ) ) ;
#6347 = CARTESIAN_POINT ( 'NONE',  ( 4.681308178468477799, 8.683552984847038303, 0.000000000000000000 ) ) ;
#6348 = EDGE_CURVE ( 'NONE', #47677, #152385, #64088, .T. ) ;
#6349 = CARTESIAN_POINT ( 'NONE',  ( -1.402160292154681736E-14, 0.07187500034142156602, 1.575800808251672791 ) ) ;
#6350 = CARTESIAN_POINT ( 'NONE',  ( 0.7499999999999885647, 0.9833333333333569293, 1.299038105676657340 ) ) ;
#6352 = CARTESIAN_POINT ( 'NONE',  ( 4.985647801523278133, 6.839675073242382553, -1.599625672291256295 ) ) ;
#6351 = CARTESIAN_POINT ( 'NONE',  ( 4.562918044398325712, 1.517878595006398212, -1.242988302126393441 ) ) ;
#6353 = EDGE_CURVE ( 'NONE', #29314, #824, #190404, .T. ) ;
#6354 = CARTESIAN_POINT ( 'NONE',  ( 2.425157474508771838, 0.8594973679685766754, 1.823840639232063632 ) ) ;
#6355 = CARTESIAN_POINT ( 'NONE',  ( 11.52460864928264783, 13.87999999999999723, -3.346683403123526190 ) ) ;
#6356 = CARTESIAN_POINT ( 'NONE',  ( 0.9256184737543894370, -1.394389637717853514, -1.690728713229103342 ) ) ;
#6357 =( BOUNDED_SURFACE ( )  B_SPLINE_SURFACE ( 1, 2, ( 
 ( #155486, #185829, #87284, #186904, #171728, #54784, #37460, #140335, #122004, #71000, #137113, #205278, #106787, #56917, #172815, #203142, #206354, #38536, #24387, #57981, #124144, #63317, #107871, #76362, #144612, #211681, #126272, #142469, #207424, #195460, #129478, #9230, #173897, #60113, #145683, #11349, #75302, #59043, #108937, #25473, #160823, #141417, #43892, #91580, #78495, #111067, #157632, #174958, #125201, #191164, #26540, #92648, #178147, #44959, #177073, #61183, #158690, #42831, #10288, #208477, #192229, #77430, #110006, #79564, #176019, #193313, #27611, #12415, #161902, #93711, #143547, #29761, #159752, #209541, #94775, #127343, #28689, #210627, #62253, #128414, #194381, #46024, #112144, #95846, #13489, #132615, #48164, #212751, #181323, #67543, #117461, #146733, #66475, #51335, #183454, #1476, #34005, #165081, #148830, #35059, #49212, #197568, #80641, #50269, #114276, #101130, #180273, #167218, #18805, #31897, #16672, #198622, #133685, #84890, #150977, #65418, #2542, #100079, #68617, #149909, #116387, #96914, #97974, #131567, #182375, #147779, #162965, #134742, #115332, #196521, #164033, #403, #199690, #32951, #99025, #14544, #47089, #15608, #113207, #64385, #82757, #179212, #30837, #81696, #83816, #130530, #166141, #213795, #17728, #76895, #93189, #105168, #200749, #156032, #27081, #107342, #171206, #88914, #204748, #52398, #42300, #22800, #139805, #118525, #174437, #206896, #159221, #56399, #39082, #10821, #122560, #188522, #59587, #187454, #40153, #154968, #6553, #72631, #141949, #138730, #173364, #106266, #172288, #207961, #23876, #24946, #140884, #58527, #157111, #89982, #7622, #73708, #205833, #57466, #91050, #123625, #175494, #189589, #74784, #41235, #108414, #43364, #8700, #124682, #125744, #190640, #26013, #92124, #158176, #9769, #75842, #191705, #109486, #146202, #11895, #144091, #64910, #180799, #14012, #210087, #94253, #62778, #163499, #213284, #28157, #162436, #147252, #131059, #97443, #130009, #46556, #30299, #197047, #145148, #79032, #176547, #212217, #61726, #48684, #127894, #114800, #32424, #193845, #112676, #80098, #15082, #98491, #164555, #161372, #16140, #196000, #143019, #31367, #63853, #192769, #45495, #12954, #47634, #29231, #44428, #209014, #211154, #77969, #111611, #96384, #81173, #128941, #194918, #110545, #60650, #177622, #126813, #160292, #178686, #95323, #113745, #179749, #119065, #186121, #100614, #50801, #181847, #169876, #37755, #198105, #82225, #34544, #120143, #200230, #49734, #33484, #83285, #148316, #135276, #115862, #18281, #214315, #52931, #85432, #103828, #149370, #132095, #65947, #952, #67018, #152566, #99556, #133154, #165621, #36671, #136335, #151517, #4153, #166690, #199156, #17209, #185047, #116929, #182928, #201290, #84364, #150455, #2016, #68085, #134220, #51880, #118003, #183992, #35606, #101683, #167752, #19352, #3085, #168815, #70224, #69156, #102760, #20419, #202355, #86501, #54005, #91871, #154713, #141704, #89732, #155780, #7365, #106009, #174187, #21466, #73442, #172031, #22547, #139546, #9520, #170947, #187195, #74530, #205572, #57210, #71290, #122302, #207715, #23623, #104907, #124432, #109234, #6294, #25758, #123370, #90793, #38823, #189337, #40976, #88653, #107087, #173109, #72368, #43119, #153645, #24689, #156857, #138469, #157927, #5215, #75592, #140630, #8442, #137402, #206643, #58276, #190390, #42048, #108159, #59338, #125492, #203420, #191454, #87575, #55076, #204491, #121225, #56141, #188259, #39900, #142763, #47381, #196800, #61470, #45242, #147011, #209833, #95063, #10574, #129760, #161112, #46307, #26830, #193600, #79847, #163249, #113494, #78776, #160041, #162185, #213035, #128694, #12698, #11645, #211966, #145956, #144897, #77716, #63605, #143838, #110294, #127635, #13771, #210905, #62532, #76648, #111359, #80922, #177364, #44174, #195744, #48442, #94002, #179500, #194662, #30043, #192520, #112423, #178437, #176302, #96132, #31122, #28978, #175244, #92933, #97196, #14831, #126560, #64664, #158977, #130810, #208768, #60396, #27905, #116669, #133971, #50547, #18022, #167498, #35351, #19096, #98248, #20159, #199979, #81977, #16955 ),
 ( #34289, #51626, #180550, #132897, #85175, #102496, #201033, #84108, #99312, #101427, #86246, #67824, #166431, #165362, #151259, #2831, #150197, #83036, #68900, #149111, #49485, #690, #135019, #168560, #117751, #36418, #66756, #33229, #164304, #52676, #136075, #202091, #118807, #198901, #182667, #100361, #1767, #15893, #115606, #183741, #114557, #184792, #32171, #152316, #3893, #69965, #148065, #214071, #65697, #131844, #197854, #181601, #53749, #71033, #137146, #37495, #119882, #87316, #153383, #4955, #21212, #185860, #103571, #169629, #50689, #149258, #131986, #164442, #30177, #112558, #214207, #147144, #64799, #211036, #47518, #66902, #31256, #96267, #49621, #34432, #79985, #165504, #48576, #16029, #178571, #213170, #130943, #162319, #114692, #180685, #212100, #182815, #78909, #163388, #32311, #13904, #17097, #145033, #835, #65837, #82113, #62662, #14961, #98378, #97330, #196936, #197994, #148206, #115746, #128821, #133042, #181735, #194803, #63737, #33367, #83175, #81059, #99448, #46439, #199042, #161250, #113629, #116814, #12837, #195880, #146088, #129895, #179636, #20311, #186009, #166580, #118960, #5107, #88545, #187085, #4045, #85324, #87471, #72255, #53899, #152465, #151407, #137301, #71183, #70114, #2980, #203318, #69049, #35497, #135169, #54968, #154607, #103723, #22435, #52823, #19244, #84256, #121121, #122190, #188155, #153537, #201184, #184938, #36565, #102651, #1910, #101575, #168707, #100505, #86397, #18168, #120035, #136226, #202248, #38718, #6186, #150341, #37644, #169773, #138362, #67969, #104799, #170845, #21363, #204380, #56036, #134112, #200121, #51775, #117893, #183885, #167643, #205467, #44067, #25650, #27797, #189231, #208660, #190284, #91761, #89619, #159934, #40870, #142650, #155672, #58166, #209725, #39787, #8338, #76539, #143732, #124324, #74423, #139432, #127527, #61369, #7254, #105893, #206536, #77607, #157815, #73330, #57100, #106975, #171918, #92824, #123267, #41941, #23514, #10465, #43009, #173000, #24581, #90688, #156749, #140523, #108054, #110185, #174079, #9413, #75484, #141595, #207602, #192412, #59221, #125379, #191344, #109122, #175136, #26723, #158869, #60290, #126449, #176196, #93895, #11538, #165252, #46200, #64561, #211861, #32062, #33123, #112317, #163142, #49381, #162077, #13666, #180446, #80817, #212926, #82928, #181494, #164198, #196696, #62425, #194556, #115499, #16845, #130705, #178332, #144795, #113386, #213969, #99202, #78669, #48336, #197743, #149000, #147956, #98150, #97089, #146907, #577, #195638, #129653, #12596, #114446, #29940, #66643, #96026, #193498, #45140, #79738, #14725, #15786, #65589, #111252, #177255, #63499, #28869, #81871, #94954, #131737, #161002, #210802, #145854, #47272, #128590, #179395, #31015, #120849, #134909, #67709, #35234, #20047, #100248, #104530, #199867, #3775, #151148, #185744, #186822, #51510, #102379, #203054, #101309, #167390, #119765, #86134, #152206, #22157, #38450, #103453, #135960, #1651, #133858, #54698, #170576, #69850, #117635, #83992, #52564, #153263, #88272, #17906, #201975, #137028, #154339, #87199, #37378, #36302, #53632, #5915, #200916, #68790, #166316, #169513, #183626, #132787, #18980, #198790, #50439, #85063, #168448, #21095, #4838, #116559, #182552, #2717, #34176, #70917, #150080, #118695, #184680, #121919, #205194, #90415, #9150, #172734, #187887, #60035, #74160, #6985, #188961, #173818, #26462, #8074, #124064, #39515, #192151, #73065, #174882, #105614, #156485, #27535, #71989, #40602, #108856, #175939, #140254, #106708, #171644, #159672, #93630, #23241, #138100, #24310, #109928, #190029, #89353, #155402, #139164, #204111, #125126, #56835, #206277, #55763, #42752, #75226, #123007, #57899, #41682, #107792, #25396, #91495, #142393, #157555, #141337, #207351, #58971, #191084, #10211, #92571, #158614, #76285, #208402, #126188, #43815, #28611, #94701, #61106, #194304, #195379, #179132, #63238, #210546, #48088, #196443, #129400, #62181, #114200, #128339, #160741, #45946, #180198, #65343, #14465, #147701, #178066, #144537, #209462, #31819, #32872, #98949, #64309, #112066, #29684, #95768, #161823, #127265, #12336 ) ),
 .UNSPECIFIED., .F., .F., .T. ) 
 B_SPLINE_SURFACE_WITH_KNOTS ( ( 2, 2 ),
 ( 3, 2, 2, 2, 2, 2, 2, 2, 2, 2, 2, 2, 2, 2, 2, 2, 2, 2, 2, 2, 2, 2, 2, 2, 2, 2, 2, 2, 2, 2, 2, 2, 2, 2, 2, 2, 2, 2, 2, 2, 2, 2, 2, 2, 2, 2, 2, 2, 2, 2, 2, 2, 2, 2, 2, 2, 2, 2, 2, 2, 2, 2, 2, 2, 2, 2, 2, 2, 2, 2, 2, 2, 2, 2, 2, 2, 2, 2, 2, 2, 2, 2, 2, 2, 2, 2, 2, 2, 2, 2, 2, 2, 2, 2, 2, 2, 2, 2, 2, 2, 2, 2, 2, 2, 2, 2, 2, 2, 2, 2, 2, 2, 2, 2, 2, 2, 2, 2, 2, 2, 2, 2, 2, 2, 2, 2, 2, 2, 2, 2, 2, 2, 2, 2, 2, 2, 2, 2, 2, 2, 2, 2, 2, 2, 2, 2, 2, 2, 2, 2, 2, 2, 2, 2, 2, 2, 2, 2, 2, 2, 2, 2, 2, 2, 2, 2, 2, 2, 2, 2, 2, 2, 2, 2, 2, 2, 2, 2, 2, 2, 2, 2, 2, 2, 2, 2, 2, 2, 2, 2, 2, 2, 2, 2, 2, 2, 2, 2, 2, 2, 2, 2, 2, 2, 2, 2, 2, 2, 2, 2, 2, 2, 2, 2, 2, 2, 2, 2, 2, 2, 2, 2, 2, 2, 2, 2, 2, 2, 2, 2, 2, 2, 2, 2, 2, 2, 2, 2, 2, 2, 3 ),
 ( 0.000000000000000000, 1.000000000000000000 ),
 ( 0.000000000000000000, 0.004166666666666666609, 0.008333333333333333218, 0.01250000000000000069, 0.01666666666666666644, 0.02083333333333333218, 0.02500000000000000139, 0.02916666666666666713, 0.03333333333333333287, 0.03749999999999999861, 0.04166666666666666435, 0.04583333333333333010, 0.05000000000000000278, 0.05416666666666666852, 0.05833333333333333426, 0.06250000000000000000, 0.06666666666666666574, 0.07083333333333333148, 0.07499999999999999722, 0.07916666666666666297, 0.08333333333333332871, 0.08749999999999999445, 0.09166666666666666019, 0.09583333333333333981, 0.1000000000000000056, 0.1041666666666666713, 0.1083333333333333370, 0.1125000000000000028, 0.1166666666666666685, 0.1208333333333333343, 0.1250000000000000000, 0.1291666666666666796, 0.1333333333333333315, 0.1375000000000000111, 0.1416666666666666630, 0.1458333333333333426, 0.1499999999999999944, 0.1541666666666666741, 0.1583333333333333259, 0.1625000000000000056, 0.1666666666666666574, 0.1708333333333333370, 0.1749999999999999889, 0.1791666666666666685, 0.1833333333333333204, 0.1875000000000000000, 0.1916666666666666796, 0.1958333333333333315, 0.2000000000000000111, 0.2041666666666666630, 0.2083333333333333426, 0.2124999999999999944, 0.2166666666666666741, 0.2208333333333333259, 0.2250000000000000056, 0.2291666666666666574, 0.2333333333333333370, 0.2374999999999999889, 0.2416666666666666685, 0.2458333333333333204, 0.2500000000000000000, 0.2541666666666666519, 0.2583333333333333592, 0.2625000000000000111, 0.2666666666666666630, 0.2708333333333333148, 0.2750000000000000222, 0.2791666666666666741, 0.2833333333333333259, 0.2874999999999999778, 0.2916666666666666852, 0.2958333333333333370, 0.2999999999999999889, 0.3041666666666666408, 0.3083333333333333481, 0.3125000000000000000, 0.3166666666666666519, 0.3208333333333333592, 0.3250000000000000111, 0.3291666666666666630, 0.3333333333333333148, 0.3375000000000000222, 0.3416666666666666741, 0.3458333333333333259, 0.3499999999999999778, 0.3541666666666666852, 0.3583333333333333370, 0.3624999999999999889, 0.3666666666666666408, 0.3708333333333333481, 0.3750000000000000000, 0.3791666666666666519, 0.3833333333333333592, 0.3875000000000000111, 0.3916666666666666630, 0.3958333333333333148, 0.4000000000000000222, 0.4041666666666666741, 0.4083333333333333259, 0.4124999999999999778, 0.4166666666666666852, 0.4208333333333333370, 0.4249999999999999889, 0.4291666666666666408, 0.4333333333333333481, 0.4375000000000000000, 0.4416666666666666519, 0.4458333333333333592, 0.4500000000000000111, 0.4541666666666666630, 0.4583333333333333148, 0.4625000000000000222, 0.4666666666666666741, 0.4708333333333333259, 0.4749999999999999778, 0.4791666666666666852, 0.4833333333333333370, 0.4874999999999999889, 0.4916666666666666408, 0.4958333333333333481, 0.5000000000000000000, 0.5041666666666666519, 0.5083333333333333037, 0.5124999999999999556, 0.5166666666666667185, 0.5208333333333333703, 0.5250000000000000222, 0.5291666666666666741, 0.5333333333333333259, 0.5374999999999999778, 0.5416666666666666297, 0.5458333333333332815, 0.5500000000000000444, 0.5541666666666666963, 0.5583333333333333481, 0.5625000000000000000, 0.5666666666666666519, 0.5708333333333333037, 0.5749999999999999556, 0.5791666666666667185, 0.5833333333333333703, 0.5875000000000000222, 0.5916666666666666741, 0.5958333333333333259, 0.5999999999999999778, 0.6041666666666666297, 0.6083333333333332815, 0.6125000000000000444, 0.6166666666666666963, 0.6208333333333333481, 0.6250000000000000000, 0.6291666666666666519, 0.6333333333333333037, 0.6374999999999999556, 0.6416666666666667185, 0.6458333333333333703, 0.6500000000000000222, 0.6541666666666666741, 0.6583333333333333259, 0.6624999999999999778, 0.6666666666666666297, 0.6708333333333332815, 0.6750000000000000444, 0.6791666666666666963, 0.6833333333333333481, 0.6875000000000000000, 0.6916666666666666519, 0.6958333333333333037, 0.6999999999999999556, 0.7041666666666667185, 0.7083333333333333703, 0.7125000000000000222, 0.7166666666666666741, 0.7208333333333333259, 0.7249999999999999778, 0.7291666666666666297, 0.7333333333333332815, 0.7375000000000000444, 0.7416666666666666963, 0.7458333333333333481, 0.7500000000000000000, 0.7541666666666666519, 0.7583333333333333037, 0.7624999999999999556, 0.7666666666666667185, 0.7708333333333333703, 0.7750000000000000222, 0.7791666666666666741, 0.7833333333333333259, 0.7874999999999999778, 0.7916666666666666297, 0.7958333333333332815, 0.8000000000000000444, 0.8041666666666666963, 0.8083333333333333481, 0.8125000000000000000, 0.8166666666666666519, 0.8208333333333333037, 0.8249999999999999556, 0.8291666666666667185, 0.8333333333333333703, 0.8375000000000000222, 0.8416666666666666741, 0.8458333333333333259, 0.8499999999999999778, 0.8541666666666666297, 0.8583333333333332815, 0.8625000000000000444, 0.8666666666666666963, 0.8708333333333333481, 0.8750000000000000000, 0.8791666666666666519, 0.8833333333333333037, 0.8874999999999999556, 0.8916666666666667185, 0.8958333333333333703, 0.9000000000000000222, 0.9041666666666666741, 0.9083333333333333259, 0.9124999999999999778, 0.9166666666666666297, 0.9208333333333332815, 0.9250000000000000444, 0.9291666666666666963, 0.9333333333333333481, 0.9375000000000000000, 0.9416666666666666519, 0.9458333333333333037, 0.9499999999999999556, 0.9541666666666667185, 0.9583333333333333703, 0.9625000000000000222, 0.9666666666666666741, 0.9708333333333333259, 0.9749999999999999778, 0.9791666666666666297, 0.9833333333333332815, 0.9875000000000000444, 0.9916666666666666963, 0.9958333333333333481, 1.000000000000000000 ),
 .UNSPECIFIED. ) 
 GEOMETRIC_REPRESENTATION_ITEM ( )  RATIONAL_B_SPLINE_SURFACE ( (
 ( 1.000000000000000000, 0.8660254037844387076, 1.000000000000000000, 0.8660254037844387076, 1.000000000000000000, 0.8660254037844387076, 1.000000000000000000, 0.8660254037844387076, 1.000000000000000000, 0.8660254037844387076, 1.000000000000000000, 0.8660254037844387076, 1.000000000000000000, 0.8660254037844387076, 1.000000000000000000, 0.8660254037844387076, 1.000000000000000000, 0.8660254037844387076, 1.000000000000000000, 0.8660254037844387076, 1.000000000000000000, 0.8660254037844387076, 1.000000000000000000, 0.8660254037844387076, 1.000000000000000000, 0.8660254037844387076, 1.000000000000000000, 0.8660254037844387076, 1.000000000000000000, 0.8660254037844387076, 1.000000000000000000, 0.8660254037844387076, 1.000000000000000000, 0.8660254037844387076, 1.000000000000000000, 0.8660254037844387076, 1.000000000000000000, 0.8660254037844387076, 1.000000000000000000, 0.8660254037844387076, 1.000000000000000000, 0.8660254037844387076, 1.000000000000000000, 0.8660254037844387076, 1.000000000000000000, 0.8660254037844387076, 1.000000000000000000, 0.8660254037844387076, 1.000000000000000000, 0.8660254037844387076, 1.000000000000000000, 0.8660254037844387076, 1.000000000000000000, 0.8660254037844387076, 1.000000000000000000, 0.8660254037844387076, 1.000000000000000000, 0.8660254037844387076, 1.000000000000000000, 0.8660254037844387076, 1.000000000000000000, 0.8660254037844387076, 1.000000000000000000, 0.8660254037844387076, 1.000000000000000000, 0.8660254037844387076, 1.000000000000000000, 0.8660254037844387076, 1.000000000000000000, 0.8660254037844387076, 1.000000000000000000, 0.8660254037844387076, 1.000000000000000000, 0.8660254037844387076, 1.000000000000000000, 0.8660254037844387076, 1.000000000000000000, 0.8660254037844387076, 1.000000000000000000, 0.8660254037844387076, 1.000000000000000000, 0.8660254037844387076, 1.000000000000000000, 0.8660254037844387076, 1.000000000000000000, 0.8660254037844387076, 1.000000000000000000, 0.8660254037844387076, 1.000000000000000000, 0.8660254037844387076, 1.000000000000000000, 0.8660254037844387076, 1.000000000000000000, 0.8660254037844387076, 1.000000000000000000, 0.8660254037844387076, 1.000000000000000000, 0.8660254037844387076, 1.000000000000000000, 0.8660254037844387076, 1.000000000000000000, 0.8660254037844387076, 1.000000000000000000, 0.8660254037844387076, 1.000000000000000000, 0.8660254037844387076, 1.000000000000000000, 0.8660254037844387076, 1.000000000000000000, 0.8660254037844387076, 1.000000000000000000, 0.8660254037844387076, 1.000000000000000000, 0.8660254037844387076, 1.000000000000000000, 0.8660254037844387076, 1.000000000000000000, 0.8660254037844387076, 1.000000000000000000, 0.8660254037844387076, 1.000000000000000000, 0.8660254037844387076, 1.000000000000000000, 0.8660254037844387076, 1.000000000000000000, 0.8660254037844387076, 1.000000000000000000, 0.8660254037844387076, 1.000000000000000000, 0.8660254037844387076, 1.000000000000000000, 0.8660254037844387076, 1.000000000000000000, 0.8660254037844387076, 1.000000000000000000, 0.8660254037844387076, 1.000000000000000000, 0.8660254037844387076, 1.000000000000000000, 0.8660254037844387076, 1.000000000000000000, 0.8660254037844387076, 1.000000000000000000, 0.8660254037844387076, 1.000000000000000000, 0.8660254037844387076, 1.000000000000000000, 0.8660254037844387076, 1.000000000000000000, 0.8660254037844387076, 1.000000000000000000, 0.8660254037844387076, 1.000000000000000000, 0.8660254037844387076, 1.000000000000000000, 0.8660254037844387076, 1.000000000000000000, 0.8660254037844387076, 1.000000000000000000, 0.8660254037844387076, 1.000000000000000000, 0.8660254037844387076, 1.000000000000000000, 0.8660254037844387076, 1.000000000000000000, 0.8660254037844387076, 1.000000000000000000, 0.8660254037844387076, 1.000000000000000000, 0.8660254037844387076, 1.000000000000000000, 0.8660254037844387076, 1.000000000000000000, 0.8660254037844387076, 1.000000000000000000, 0.8660254037844387076, 1.000000000000000000, 0.8660254037844387076, 1.000000000000000000, 0.8660254037844387076, 1.000000000000000000, 0.8660254037844387076, 1.000000000000000000, 0.8660254037844387076, 1.000000000000000000, 0.8660254037844387076, 1.000000000000000000, 0.8660254037844387076, 1.000000000000000000, 0.8660254037844387076, 1.000000000000000000, 0.8660254037844387076, 1.000000000000000000, 0.8660254037844387076, 1.000000000000000000, 0.8660254037844387076, 1.000000000000000000, 0.8660254037844387076, 1.000000000000000000, 0.8660254037844387076, 1.000000000000000000, 0.8660254037844387076, 1.000000000000000000, 0.8660254037844387076, 1.000000000000000000, 0.8660254037844387076, 1.000000000000000000, 0.8660254037844387076, 1.000000000000000000, 0.8660254037844387076, 1.000000000000000000, 0.8660254037844387076, 1.000000000000000000, 0.8660254037844387076, 1.000000000000000000, 0.8660254037844387076, 1.000000000000000000, 0.8660254037844387076, 1.000000000000000000, 0.8660254037844387076, 1.000000000000000000, 0.8660254037844387076, 1.000000000000000000, 0.8660254037844387076, 1.000000000000000000, 0.8660254037844387076, 1.000000000000000000, 0.8660254037844387076, 1.000000000000000000, 0.8660254037844387076, 1.000000000000000000, 0.8660254037844387076, 1.000000000000000000, 0.8660254037844387076, 1.000000000000000000, 0.8660254037844387076, 1.000000000000000000, 0.8660254037844387076, 1.000000000000000000, 0.8660254037844387076, 1.000000000000000000, 0.8660254037844387076, 1.000000000000000000, 0.8660254037844387076, 1.000000000000000000, 0.8660254037844387076, 1.000000000000000000, 0.8660254037844387076, 1.000000000000000000, 0.8660254037844387076, 1.000000000000000000, 0.8660254037844387076, 1.000000000000000000, 0.8660254037844387076, 1.000000000000000000, 0.8660254037844387076, 1.000000000000000000, 0.8660254037844387076, 1.000000000000000000, 0.8660254037844387076, 1.000000000000000000, 0.8660254037844387076, 1.000000000000000000, 0.8660254037844387076, 1.000000000000000000, 0.8660254037844387076, 1.000000000000000000, 0.8660254037844387076, 1.000000000000000000, 0.8660254037844387076, 1.000000000000000000, 0.8660254037844387076, 1.000000000000000000, 0.8660254037844387076, 1.000000000000000000, 0.8660254037844387076, 1.000000000000000000, 0.8660254037844387076, 1.000000000000000000, 0.8660254037844387076, 1.000000000000000000, 0.8660254037844387076, 1.000000000000000000, 0.8660254037844387076, 1.000000000000000000, 0.8660254037844387076, 1.000000000000000000, 0.8660254037844387076, 1.000000000000000000, 0.8660254037844387076, 1.000000000000000000, 0.8660254037844387076, 1.000000000000000000, 0.8660254037844387076, 1.000000000000000000, 0.8660254037844387076, 1.000000000000000000, 0.8660254037844387076, 1.000000000000000000, 0.8660254037844387076, 1.000000000000000000, 0.8660254037844387076, 1.000000000000000000, 0.8660254037844387076, 1.000000000000000000, 0.8660254037844387076, 1.000000000000000000, 0.8660254037844387076, 1.000000000000000000, 0.8660254037844387076, 1.000000000000000000, 0.8660254037844387076, 1.000000000000000000, 0.8660254037844387076, 1.000000000000000000, 0.8660254037844387076, 1.000000000000000000, 0.8660254037844387076, 1.000000000000000000, 0.8660254037844387076, 1.000000000000000000, 0.8660254037844387076, 1.000000000000000000, 0.8660254037844387076, 1.000000000000000000, 0.8660254037844387076, 1.000000000000000000, 0.8660254037844387076, 1.000000000000000000, 0.8660254037844387076, 1.000000000000000000, 0.8660254037844387076, 1.000000000000000000, 0.8660254037844387076, 1.000000000000000000, 0.8660254037844387076, 1.000000000000000000, 0.8660254037844387076, 1.000000000000000000, 0.8660254037844387076, 1.000000000000000000, 0.8660254037844387076, 1.000000000000000000, 0.8660254037844387076, 1.000000000000000000, 0.8660254037844387076, 1.000000000000000000, 0.8660254037844387076, 1.000000000000000000, 0.8660254037844387076, 1.000000000000000000, 0.8660254037844387076, 1.000000000000000000, 0.8660254037844387076, 1.000000000000000000, 0.8660254037844387076, 1.000000000000000000, 0.8660254037844387076, 1.000000000000000000, 0.8660254037844387076, 1.000000000000000000, 0.8660254037844387076, 1.000000000000000000, 0.8660254037844387076, 1.000000000000000000, 0.8660254037844387076, 1.000000000000000000, 0.8660254037844387076, 1.000000000000000000, 0.8660254037844387076, 1.000000000000000000, 0.8660254037844387076, 1.000000000000000000, 0.8660254037844387076, 1.000000000000000000, 0.8660254037844387076, 1.000000000000000000, 0.8660254037844387076, 1.000000000000000000, 0.8660254037844387076, 1.000000000000000000, 0.8660254037844387076, 1.000000000000000000, 0.8660254037844387076, 1.000000000000000000, 0.8660254037844387076, 1.000000000000000000, 0.8660254037844387076, 1.000000000000000000, 0.8660254037844387076, 1.000000000000000000, 0.8660254037844387076, 1.000000000000000000, 0.8660254037844387076, 1.000000000000000000, 0.8660254037844387076, 1.000000000000000000, 0.8660254037844387076, 1.000000000000000000, 0.8660254037844387076, 1.000000000000000000, 0.8660254037844387076, 1.000000000000000000, 0.8660254037844387076, 1.000000000000000000, 0.8660254037844387076, 1.000000000000000000, 0.8660254037844387076, 1.000000000000000000, 0.8660254037844387076, 1.000000000000000000, 0.8660254037844387076, 1.000000000000000000, 0.8660254037844387076, 1.000000000000000000, 0.8660254037844387076, 1.000000000000000000, 0.8660254037844387076, 1.000000000000000000, 0.8660254037844387076, 1.000000000000000000, 0.8660254037844387076, 1.000000000000000000, 0.8660254037844387076, 1.000000000000000000, 0.8660254037844387076, 1.000000000000000000, 0.8660254037844387076, 1.000000000000000000, 0.8660254037844387076, 1.000000000000000000, 0.8660254037844387076, 1.000000000000000000, 0.8660254037844387076, 1.000000000000000000, 0.8660254037844387076, 1.000000000000000000, 0.8660254037844387076, 1.000000000000000000, 0.8660254037844387076, 1.000000000000000000, 0.8660254037844387076, 1.000000000000000000, 0.8660254037844387076, 1.000000000000000000, 0.8660254037844387076, 1.000000000000000000, 0.8660254037844387076, 1.000000000000000000, 0.8660254037844387076, 1.000000000000000000, 0.8660254037844387076, 1.000000000000000000, 0.8660254037844387076, 1.000000000000000000, 0.8660254037844387076, 1.000000000000000000, 0.8660254037844387076, 1.000000000000000000, 0.8660254037844387076, 1.000000000000000000, 0.8660254037844387076, 1.000000000000000000, 0.8660254037844387076, 1.000000000000000000, 0.8660254037844387076, 1.000000000000000000, 0.8660254037844387076, 1.000000000000000000, 0.8660254037844387076, 1.000000000000000000, 0.8660254037844387076, 1.000000000000000000, 0.8660254037844387076, 1.000000000000000000, 0.8660254037844387076, 1.000000000000000000, 0.8660254037844387076, 1.000000000000000000, 0.8660254037844387076, 1.000000000000000000),
 ( 1.000000000000000000, 0.8660254037844387076, 1.000000000000000000, 0.8660254037844387076, 1.000000000000000000, 0.8660254037844387076, 1.000000000000000000, 0.8660254037844387076, 1.000000000000000000, 0.8660254037844387076, 1.000000000000000000, 0.8660254037844387076, 1.000000000000000000, 0.8660254037844387076, 1.000000000000000000, 0.8660254037844387076, 1.000000000000000000, 0.8660254037844387076, 1.000000000000000000, 0.8660254037844387076, 1.000000000000000000, 0.8660254037844387076, 1.000000000000000000, 0.8660254037844387076, 1.000000000000000000, 0.8660254037844387076, 1.000000000000000000, 0.8660254037844387076, 1.000000000000000000, 0.8660254037844387076, 1.000000000000000000, 0.8660254037844387076, 1.000000000000000000, 0.8660254037844387076, 1.000000000000000000, 0.8660254037844387076, 1.000000000000000000, 0.8660254037844387076, 1.000000000000000000, 0.8660254037844387076, 1.000000000000000000, 0.8660254037844387076, 1.000000000000000000, 0.8660254037844387076, 1.000000000000000000, 0.8660254037844387076, 1.000000000000000000, 0.8660254037844387076, 1.000000000000000000, 0.8660254037844387076, 1.000000000000000000, 0.8660254037844387076, 1.000000000000000000, 0.8660254037844387076, 1.000000000000000000, 0.8660254037844387076, 1.000000000000000000, 0.8660254037844387076, 1.000000000000000000, 0.8660254037844387076, 1.000000000000000000, 0.8660254037844387076, 1.000000000000000000, 0.8660254037844387076, 1.000000000000000000, 0.8660254037844387076, 1.000000000000000000, 0.8660254037844387076, 1.000000000000000000, 0.8660254037844387076, 1.000000000000000000, 0.8660254037844387076, 1.000000000000000000, 0.8660254037844387076, 1.000000000000000000, 0.8660254037844387076, 1.000000000000000000, 0.8660254037844387076, 1.000000000000000000, 0.8660254037844387076, 1.000000000000000000, 0.8660254037844387076, 1.000000000000000000, 0.8660254037844387076, 1.000000000000000000, 0.8660254037844387076, 1.000000000000000000, 0.8660254037844387076, 1.000000000000000000, 0.8660254037844387076, 1.000000000000000000, 0.8660254037844387076, 1.000000000000000000, 0.8660254037844387076, 1.000000000000000000, 0.8660254037844387076, 1.000000000000000000, 0.8660254037844387076, 1.000000000000000000, 0.8660254037844387076, 1.000000000000000000, 0.8660254037844387076, 1.000000000000000000, 0.8660254037844387076, 1.000000000000000000, 0.8660254037844387076, 1.000000000000000000, 0.8660254037844387076, 1.000000000000000000, 0.8660254037844387076, 1.000000000000000000, 0.8660254037844387076, 1.000000000000000000, 0.8660254037844387076, 1.000000000000000000, 0.8660254037844387076, 1.000000000000000000, 0.8660254037844387076, 1.000000000000000000, 0.8660254037844387076, 1.000000000000000000, 0.8660254037844387076, 1.000000000000000000, 0.8660254037844387076, 1.000000000000000000, 0.8660254037844387076, 1.000000000000000000, 0.8660254037844387076, 1.000000000000000000, 0.8660254037844387076, 1.000000000000000000, 0.8660254037844387076, 1.000000000000000000, 0.8660254037844387076, 1.000000000000000000, 0.8660254037844387076, 1.000000000000000000, 0.8660254037844387076, 1.000000000000000000, 0.8660254037844387076, 1.000000000000000000, 0.8660254037844387076, 1.000000000000000000, 0.8660254037844387076, 1.000000000000000000, 0.8660254037844387076, 1.000000000000000000, 0.8660254037844387076, 1.000000000000000000, 0.8660254037844387076, 1.000000000000000000, 0.8660254037844387076, 1.000000000000000000, 0.8660254037844387076, 1.000000000000000000, 0.8660254037844387076, 1.000000000000000000, 0.8660254037844387076, 1.000000000000000000, 0.8660254037844387076, 1.000000000000000000, 0.8660254037844387076, 1.000000000000000000, 0.8660254037844387076, 1.000000000000000000, 0.8660254037844387076, 1.000000000000000000, 0.8660254037844387076, 1.000000000000000000, 0.8660254037844387076, 1.000000000000000000, 0.8660254037844387076, 1.000000000000000000, 0.8660254037844387076, 1.000000000000000000, 0.8660254037844387076, 1.000000000000000000, 0.8660254037844387076, 1.000000000000000000, 0.8660254037844387076, 1.000000000000000000, 0.8660254037844387076, 1.000000000000000000, 0.8660254037844387076, 1.000000000000000000, 0.8660254037844387076, 1.000000000000000000, 0.8660254037844387076, 1.000000000000000000, 0.8660254037844387076, 1.000000000000000000, 0.8660254037844387076, 1.000000000000000000, 0.8660254037844387076, 1.000000000000000000, 0.8660254037844387076, 1.000000000000000000, 0.8660254037844387076, 1.000000000000000000, 0.8660254037844387076, 1.000000000000000000, 0.8660254037844387076, 1.000000000000000000, 0.8660254037844387076, 1.000000000000000000, 0.8660254037844387076, 1.000000000000000000, 0.8660254037844387076, 1.000000000000000000, 0.8660254037844387076, 1.000000000000000000, 0.8660254037844387076, 1.000000000000000000, 0.8660254037844387076, 1.000000000000000000, 0.8660254037844387076, 1.000000000000000000, 0.8660254037844387076, 1.000000000000000000, 0.8660254037844387076, 1.000000000000000000, 0.8660254037844387076, 1.000000000000000000, 0.8660254037844387076, 1.000000000000000000, 0.8660254037844387076, 1.000000000000000000, 0.8660254037844387076, 1.000000000000000000, 0.8660254037844387076, 1.000000000000000000, 0.8660254037844387076, 1.000000000000000000, 0.8660254037844387076, 1.000000000000000000, 0.8660254037844387076, 1.000000000000000000, 0.8660254037844387076, 1.000000000000000000, 0.8660254037844387076, 1.000000000000000000, 0.8660254037844387076, 1.000000000000000000, 0.8660254037844387076, 1.000000000000000000, 0.8660254037844387076, 1.000000000000000000, 0.8660254037844387076, 1.000000000000000000, 0.8660254037844387076, 1.000000000000000000, 0.8660254037844387076, 1.000000000000000000, 0.8660254037844387076, 1.000000000000000000, 0.8660254037844387076, 1.000000000000000000, 0.8660254037844387076, 1.000000000000000000, 0.8660254037844387076, 1.000000000000000000, 0.8660254037844387076, 1.000000000000000000, 0.8660254037844387076, 1.000000000000000000, 0.8660254037844387076, 1.000000000000000000, 0.8660254037844387076, 1.000000000000000000, 0.8660254037844387076, 1.000000000000000000, 0.8660254037844387076, 1.000000000000000000, 0.8660254037844387076, 1.000000000000000000, 0.8660254037844387076, 1.000000000000000000, 0.8660254037844387076, 1.000000000000000000, 0.8660254037844387076, 1.000000000000000000, 0.8660254037844387076, 1.000000000000000000, 0.8660254037844387076, 1.000000000000000000, 0.8660254037844387076, 1.000000000000000000, 0.8660254037844387076, 1.000000000000000000, 0.8660254037844387076, 1.000000000000000000, 0.8660254037844387076, 1.000000000000000000, 0.8660254037844387076, 1.000000000000000000, 0.8660254037844387076, 1.000000000000000000, 0.8660254037844387076, 1.000000000000000000, 0.8660254037844387076, 1.000000000000000000, 0.8660254037844387076, 1.000000000000000000, 0.8660254037844387076, 1.000000000000000000, 0.8660254037844387076, 1.000000000000000000, 0.8660254037844387076, 1.000000000000000000, 0.8660254037844387076, 1.000000000000000000, 0.8660254037844387076, 1.000000000000000000, 0.8660254037844387076, 1.000000000000000000, 0.8660254037844387076, 1.000000000000000000, 0.8660254037844387076, 1.000000000000000000, 0.8660254037844387076, 1.000000000000000000, 0.8660254037844387076, 1.000000000000000000, 0.8660254037844387076, 1.000000000000000000, 0.8660254037844387076, 1.000000000000000000, 0.8660254037844387076, 1.000000000000000000, 0.8660254037844387076, 1.000000000000000000, 0.8660254037844387076, 1.000000000000000000, 0.8660254037844387076, 1.000000000000000000, 0.8660254037844387076, 1.000000000000000000, 0.8660254037844387076, 1.000000000000000000, 0.8660254037844387076, 1.000000000000000000, 0.8660254037844387076, 1.000000000000000000, 0.8660254037844387076, 1.000000000000000000, 0.8660254037844387076, 1.000000000000000000, 0.8660254037844387076, 1.000000000000000000, 0.8660254037844387076, 1.000000000000000000, 0.8660254037844387076, 1.000000000000000000, 0.8660254037844387076, 1.000000000000000000, 0.8660254037844387076, 1.000000000000000000, 0.8660254037844387076, 1.000000000000000000, 0.8660254037844387076, 1.000000000000000000, 0.8660254037844387076, 1.000000000000000000, 0.8660254037844387076, 1.000000000000000000, 0.8660254037844387076, 1.000000000000000000, 0.8660254037844387076, 1.000000000000000000, 0.8660254037844387076, 1.000000000000000000, 0.8660254037844387076, 1.000000000000000000, 0.8660254037844387076, 1.000000000000000000, 0.8660254037844387076, 1.000000000000000000, 0.8660254037844387076, 1.000000000000000000, 0.8660254037844387076, 1.000000000000000000, 0.8660254037844387076, 1.000000000000000000, 0.8660254037844387076, 1.000000000000000000, 0.8660254037844387076, 1.000000000000000000, 0.8660254037844387076, 1.000000000000000000, 0.8660254037844387076, 1.000000000000000000, 0.8660254037844387076, 1.000000000000000000, 0.8660254037844387076, 1.000000000000000000, 0.8660254037844387076, 1.000000000000000000, 0.8660254037844387076, 1.000000000000000000, 0.8660254037844387076, 1.000000000000000000, 0.8660254037844387076, 1.000000000000000000, 0.8660254037844387076, 1.000000000000000000, 0.8660254037844387076, 1.000000000000000000, 0.8660254037844387076, 1.000000000000000000, 0.8660254037844387076, 1.000000000000000000, 0.8660254037844387076, 1.000000000000000000, 0.8660254037844387076, 1.000000000000000000, 0.8660254037844387076, 1.000000000000000000, 0.8660254037844387076, 1.000000000000000000, 0.8660254037844387076, 1.000000000000000000, 0.8660254037844387076, 1.000000000000000000, 0.8660254037844387076, 1.000000000000000000, 0.8660254037844387076, 1.000000000000000000, 0.8660254037844387076, 1.000000000000000000, 0.8660254037844387076, 1.000000000000000000, 0.8660254037844387076, 1.000000000000000000, 0.8660254037844387076, 1.000000000000000000, 0.8660254037844387076, 1.000000000000000000, 0.8660254037844387076, 1.000000000000000000, 0.8660254037844387076, 1.000000000000000000, 0.8660254037844387076, 1.000000000000000000, 0.8660254037844387076, 1.000000000000000000, 0.8660254037844387076, 1.000000000000000000, 0.8660254037844387076, 1.000000000000000000, 0.8660254037844387076, 1.000000000000000000, 0.8660254037844387076, 1.000000000000000000, 0.8660254037844387076, 1.000000000000000000, 0.8660254037844387076, 1.000000000000000000, 0.8660254037844387076, 1.000000000000000000, 0.8660254037844387076, 1.000000000000000000, 0.8660254037844387076, 1.000000000000000000, 0.8660254037844387076, 1.000000000000000000, 0.8660254037844387076, 1.000000000000000000, 0.8660254037844387076, 1.000000000000000000, 0.8660254037844387076, 1.000000000000000000, 0.8660254037844387076, 1.000000000000000000, 0.8660254037844387076, 1.000000000000000000, 0.8660254037844387076, 1.000000000000000000, 0.8660254037844387076, 1.000000000000000000, 0.8660254037844387076, 1.000000000000000000) ) ) 
 REPRESENTATION_ITEM ( '' )  SURFACE ( )  );
#6358 = FACE_OUTER_BOUND ( 'NONE', #202985, .T. ) ;
#6359 = CARTESIAN_POINT ( 'NONE',  ( 2.196370303256788503, -0.4943915968025693330, -1.803980227719769847 ) ) ;
#6360 = CARTESIAN_POINT ( 'NONE',  ( -1.364683531250010295, 5.030208333674757171, 0.7879004041258379498 ) ) ;
#6361 = CARTESIAN_POINT ( 'NONE',  ( 3.867443265902783534, -1.676145683993632618, -1.114854040202686969 ) ) ;
#6362 = CARTESIAN_POINT ( 'NONE',  ( -8.507905087775398556, 9.884643009614800135, 1.199719254218462483 ) ) ;
#6364 = CARTESIAN_POINT ( 'NONE',  ( 3.146228450019908252, 0.9544266383219732752, 1.889993806685738464 ) ) ;
#6363 = CARTESIAN_POINT ( 'NONE',  ( -4.934804725694220906, 7.740727365743146571, -1.082531754730549967 ) ) ;
#6365 =( NAMED_UNIT ( * ) SI_UNIT ( $, .STERADIAN. ) SOLID_ANGLE_UNIT ( ) );
#6366 = CARTESIAN_POINT ( 'NONE',  ( 4.650872726564402981, -0.4503784926754761386, -2.020631409805350387 ) ) ;
#6367 = CARTESIAN_POINT ( 'NONE',  ( 6.879836604291781121, 6.991173891287354003, -0.7998128361456341429 ) ) ;
#6369 = CARTESIAN_POINT ( 'NONE',  ( 6.620655732516611103, 6.035157181942712334, 2.668628960472289702 ) ) ;
#6368 = CARTESIAN_POINT ( 'NONE',  ( 1.048509228467583876, -1.645825662996244443, 1.289236127856315139 ) ) ;
#6371 = VERTEX_POINT ( 'NONE', #122593 ) ;
#6370 = CARTESIAN_POINT ( 'NONE',  ( 6.229513028222847026, -1.717969363144413952, 0.6179237509907066217 ) ) ;
#6372 = CARTESIAN_POINT ( 'NONE',  ( 6.968000882419564945, 10.21675256520979858, 1.199719254218460707 ) ) ;
#6373 = CARTESIAN_POINT ( 'NONE',  ( 0.000000000000000000, 3.799999999999998046, 0.000000000000000000 ) ) ;
#6374 = EDGE_CURVE ( 'NONE', #25036, #199311, #105200, .T. ) ;
#6375 = CARTESIAN_POINT ( 'NONE',  ( -9.348561386651960348, 2.999999999999999112, 7.001914024036568485 ) ) ;
#6376 = CARTESIAN_POINT ( 'NONE',  ( 7.578644679914713578, 8.904468883731073703, 1.082531754730558626 ) ) ;
#6377 = CARTESIAN_POINT ( 'NONE',  ( 1.364683531249997417, 12.79687500034139980, 2.602085213965210642E-15 ) ) ;
#6378 = CARTESIAN_POINT ( 'NONE',  ( -0.05833479489262324152, -1.112358503097829576, -1.430056051773327841 ) ) ;
#6379 = CARTESIAN_POINT ( 'NONE',  ( -7.507464373665155399, 9.781794407407920389, 1.599625672291295375 ) ) ;
#6380 = CARTESIAN_POINT ( 'NONE',  ( 3.994848817520957773, 7.812407387083109001, 1.040834085586084257E-14 ) ) ;
#6381 = CARTESIAN_POINT ( 'NONE',  ( -7.142181811248260459E-15, -6.134628647623513231, 10.91970695577494865 ) ) ;
#6383 = B_SPLINE_CURVE_WITH_KNOTS ( 'NONE', 3,
 ( #38914, #73536, #152662, #203513, #4244, #70315, #54102, #21555, #138561, #69250, #120238, #204582, #87665, #153735, #22636, #5303 ),
 .UNSPECIFIED., .F., .F.,
 ( 4, 2, 2, 2, 2, 2, 2, 4 ),
 ( 0.000000000000000000, 0.0006374118625136481224, 0.0009561177937704720209, 0.001274823725027296028, 0.001593529656284120143, 0.001912235587540944042, 0.002230941518797768374, 0.002549647450054592056 ),
 .UNSPECIFIED. ) ;
#6382 = CYLINDRICAL_SURFACE ( 'NONE', #89337, 0.6500000000000000222 ) ;
#6384 = CARTESIAN_POINT ( 'NONE',  ( 3.871016551901614200, 4.474939717762034697, -1.199719254218446718 ) ) ;
#6385 = EDGE_LOOP ( 'NONE', ( #14648, #122426, #53005, #29470 ) ) ;
#6386 = CARTESIAN_POINT ( 'NONE',  ( 6.521112179100128969, -1.799899466697444383, 0.9092066555835758290 ) ) ;
#6387 = CARTESIAN_POINT ( 'NONE',  ( -4.036335974549790429, 7.671137949187412985, -0.4422704879359267149 ) ) ;
#6388 = CARTESIAN_POINT ( 'NONE',  ( 1.872228381520312013, 3.299999999999997158, -0.4000000000000131783 ) ) ;
#6389 = CARTESIAN_POINT ( 'NONE',  ( -0.1399997263889611598, 2.874570648431204578, -2.488748559936367233 ) ) ;
#6390 = CARTESIAN_POINT ( 'NONE',  ( -4.609409038966245653, 6.400729850259146758, -1.443375672974053447 ) ) ;
#6391 = CARTESIAN_POINT ( 'NONE',  ( 9.327646496521982300, 11.90534021740758064, -1.443375672974057666 ) ) ;
#6392 = CARTESIAN_POINT ( 'NONE',  ( 3.942214172571806508, -0.9744538365985645489, 1.711425102584500202 ) ) ;
#6393 = CARTESIAN_POINT ( 'NONE',  ( 4.552361342037492875, -1.314984614574012944, 1.528753174698034067 ) ) ;
#6394 = CARTESIAN_POINT ( 'NONE',  ( -7.393273838153706201, 7.519907654134449615, 0.7998128361456341429 ) ) ;
#6395 = CARTESIAN_POINT ( 'NONE',  ( 0.000000000000000000, 0.000000000000000000, 0.000000000000000000 ) ) ;
#6396 = CARTESIAN_POINT ( 'NONE',  ( 4.470767510317084970, 0.001397387737574890204, -2.191629466793604930 ) ) ;
#6397 = PLANE ( 'NONE',  #161063 ) ;
#6398 = CARTESIAN_POINT ( 'NONE',  ( 2.696214026845968448, -1.921097006559132625, -0.1437054574915888616 ) ) ;
#6399 = CARTESIAN_POINT ( 'NONE',  ( -7.309817376062285099, 11.67987070538135264, 0.000000000000000000 ) ) ;
#6400 = CARTESIAN_POINT ( 'NONE',  ( -0.02988540731099428513, 1.418068428043406382, -1.986943242881351601 ) ) ;
#6401 = DIRECTION ( 'NONE',  ( -0.6507913734559640506, -0.7592566023653004592, 0.000000000000000000 ) ) ;
#6402 = CARTESIAN_POINT ( 'NONE',  ( 0.000000000000000000, 1.000000000000000888, 0.000000000000000000 ) ) ;
#6403 = CARTESIAN_POINT ( 'NONE',  ( -0.6823417656250039265, 13.31770833367473195, -1.181850606188755259 ) ) ;
#6404 = CARTESIAN_POINT ( 'NONE',  ( 4.904298879841284098, 6.744767997946721216, 1.599625672291267398 ) ) ;
#6405 = ORIENTED_EDGE ( 'NONE', *, *, #209722, .T. ) ;
#6406 = CARTESIAN_POINT ( 'NONE',  ( 5.289089323106923146, 6.303597310780433283, -1.082531754730548412 ) ) ;
#6407 = VERTEX_POINT ( 'NONE', #11934 ) ;
#6409 = CARTESIAN_POINT ( 'NONE',  ( 2.543610208494262892, -1.877569574052952328, 0.7265587727790027150 ) ) ;
#6408 = CARTESIAN_POINT ( 'NONE',  ( -0.1235792489666731608, -0.1369701924231395973, -1.910945132828122395 ) ) ;
#6410 = CARTESIAN_POINT ( 'NONE',  ( 5.606872354539667036, 0.9390355927846851802, -2.097984029676060125 ) ) ;
#6412 = CARTESIAN_POINT ( 'NONE',  ( 3.537814430808595922, 1.177328839734363308, 1.441218929277183536 ) ) ;
#6411 = CARTESIAN_POINT ( 'NONE',  ( -3.947104627881522720, 8.980740528188976057, -0.7749999999999979128 ) ) ;
#6413 = CARTESIAN_POINT ( 'NONE',  ( 6.016786309414542622, 10.24161080428416426, 0.7998128361456341429 ) ) ;
#6414 = CARTESIAN_POINT ( 'NONE',  ( -9.251576347356463614, -6.938200158402487716, 0.4350533241460385336 ) ) ;
#6415 =( NAMED_UNIT ( * ) SI_UNIT ( $, .STERADIAN. ) SOLID_ANGLE_UNIT ( ) );
#6416 = CARTESIAN_POINT ( 'NONE',  ( -6.531277313481209212, 8.642909503859968368, 1.599625672291283607 ) ) ;
#6417 = CARTESIAN_POINT ( 'NONE',  ( -5.343321937561608337, 5.406499480009534508, 0.7216878364870257245 ) ) ;
#6418 = CARTESIAN_POINT ( 'NONE',  ( 5.601146835291897830, -0.5070800215070477845, 2.028203315493964709 ) ) ;
#6419 = CARTESIAN_POINT ( 'NONE',  ( 4.690757960648213931, 8.416375354157496602, 0.7216878364870438212 ) ) ;
#6420 = ORIENTED_EDGE ( 'NONE', *, *, #182196, .T. ) ;
#6421 = AXIS2_PLACEMENT_3D ( 'NONE', #180734, #16076, #32361 ) ;
#6422 = CARTESIAN_POINT ( 'NONE',  ( -4.260029445439560192, 7.236136616047151193, 2.499999999999999556 ) ) ;
#6423 = CARTESIAN_POINT ( 'NONE',  ( 0.2404813148422607627, 0.3085585699703840556, 1.799268721412583316 ) ) ;
#6424 = CARTESIAN_POINT ( 'NONE',  ( -4.141125853970233806, 6.918731698685530063, -1.199719254218452047 ) ) ;
#6425 = CARTESIAN_POINT ( 'NONE',  ( 2.549097654585132045, -1.194521797001405927, 1.257391726941985421 ) ) ;
#6426 = PLANE ( 'NONE',  #164910 ) ;
#6427 = CARTESIAN_POINT ( 'NONE',  ( -11.94105721237523099, 10.90000000000000036, -1.187919463087249827 ) ) ;
#6428 = CARTESIAN_POINT ( 'NONE',  ( -6.663996196316808174, 7.733415969579778171, -1.199719254218446718 ) ) ;
#6429 = CARTESIAN_POINT ( 'NONE',  ( 4.787437639401280087, 6.678706227425192488, 0.000000000000000000 ) ) ;
#6430 = CARTESIAN_POINT ( 'NONE',  ( 0.2861044793709514589, -1.271156181823060560, -1.634742764404630844 ) ) ;
#6431 = CARTESIAN_POINT ( 'NONE',  ( 5.461492464141177727, 0.3521552718798379722, -1.791230276788812414 ) ) ;
#6432 = CARTESIAN_POINT ( 'NONE',  ( 3.836726278109466204, -1.889416792123297162, -0.5274722977551549175 ) ) ;
#6433 = CARTESIAN_POINT ( 'NONE',  ( -5.508486862036250636E-15, -0.7499999993172156154, -1.414508159514623609 ) ) ;
#6434 = CARTESIAN_POINT ( 'NONE',  ( -7.828943636887387925, 11.22118577875556156, 1.199719254218453823 ) ) ;
#6435 = CARTESIAN_POINT ( 'NONE',  ( 7.124973419181436007, 8.271222729588529887, -1.199719254218446718 ) ) ;
#6436 = CARTESIAN_POINT ( 'NONE',  ( 3.844477943020713440, 1.133112341739877849, -1.792160191984671691 ) ) ;
#6437 = CARTESIAN_POINT ( 'NONE',  ( -3.850152436600983386, 4.554561266531622188, 1.082531754730560403 ) ) ;
#6438 = CARTESIAN_POINT ( 'NONE',  ( -8.784793466650835825, 12.33634391347959713, 1.199719254218462483 ) ) ;
#6439 = CARTESIAN_POINT ( 'NONE',  ( 1.938418878558012315, -1.110983660290700170, 1.746734030103759938 ) ) ;
#6440 = CARTESIAN_POINT ( 'NONE',  ( -1.402160292154681736E-14, -0.9906249996585834161, -1.575800808251665908 ) ) ;
#6442 = VERTEX_POINT ( 'NONE', #209050 ) ;
#6441 = CARTESIAN_POINT ( 'NONE',  ( 4.073042245396302441, -1.645747789204109468, 1.492029542161198430 ) ) ;
#6443 = CARTESIAN_POINT ( 'NONE',  ( 1.916985526034093335, -1.504927692415005014, -1.737642283433957768 ) ) ;
#6445 = CARTESIAN_POINT ( 'NONE',  ( 6.227400143195995774, 0.1575970216860186346, -2.056636196940288652 ) ) ;
#6444 = CARTESIAN_POINT ( 'NONE',  ( 8.839552966430002101, 11.33589776563360019, -1.443375672974052559 ) ) ;
#6447 = CARTESIAN_POINT ( 'NONE',  ( 1.642778471875000035, -3.376041666188708046, -2.845375778867859751 ) ) ;
#6446 = CARTESIAN_POINT ( 'NONE',  ( 4.716257332707354699, 6.595662536282280719, -1.599625672291269396 ) ) ;
#6448 = LINE ( 'NONE', #188415, #192774 ) ;
#6449 = CARTESIAN_POINT ( 'NONE',  ( 6.286648950733226826, 1.598451336667701339, -0.9137711784916457969 ) ) ;
#6450 = CARTESIAN_POINT ( 'NONE',  ( 7.837739514543059934E-16, -0.2000000000000057288, -6.399999999999999467 ) ) ;
#6451 = EDGE_CURVE ( 'NONE', #135502, #92250, #102553, .T. ) ;
#6452 = CARTESIAN_POINT ( 'NONE',  ( 3.216961742616857745, 1.504763323797538410, -1.180078671740567131 ) ) ;
#6453 = CARTESIAN_POINT ( 'NONE',  ( -0.2106725631050099246, 1.363266585364702577, -2.259529575671606505 ) ) ;
#6454 = CARTESIAN_POINT ( 'NONE',  ( 3.926516724862822993, 1.637815149125703584, 0.5408920155725772672 ) ) ;
#6455 = CARTESIAN_POINT ( 'NONE',  ( 2.501185699981960830, -0.1928336239410358699, 2.007256303757164240 ) ) ;
#6456 = CARTESIAN_POINT ( 'NONE',  ( 3.745041490520171212, 2.281215052333289250, -0.2826575254791847680 ) ) ;
#6457 = CARTESIAN_POINT ( 'NONE',  ( 3.444836229973327946, 0.5457880569446837971, 2.195490905318697283 ) ) ;
#6458 = CARTESIAN_POINT ( 'NONE',  ( 6.182269030498733997, -1.128069697684991546, 1.778281062836915449 ) ) ;
#6459 = CARTESIAN_POINT ( 'NONE',  ( -6.468648687495877958, 6.719380688266201496, 0.000000000000000000 ) ) ;
#6460 = ORIENTED_EDGE ( 'NONE', *, *, #38859, .F. ) ;
#6461 = CARTESIAN_POINT ( 'NONE',  ( 5.026482010321593030, 1.693441115147217291, 0.5138918105389718161 ) ) ;
#6463 = CARTESIAN_POINT ( 'NONE',  ( 1.236728449817244835, 0.4514257060114800213, 2.247219992417306411 ) ) ;
#6462 = CARTESIAN_POINT ( 'NONE',  ( 5.742760583840166966, 8.857581893525663830, 1.199719254218452047 ) ) ;
#6464 = CARTESIAN_POINT ( 'NONE',  ( 5.525302006934727395, -1.171079710934025186, -1.420692760577553226 ) ) ;
#6465 = CARTESIAN_POINT ( 'NONE',  ( -3.623053363349869382, 5.249981562040033189, 1.599625672291267398 ) ) ;
#6466 = AXIS2_PLACEMENT_3D ( 'NONE', #127068, #146460, #15339 ) ;
#6467 = CARTESIAN_POINT ( 'NONE',  ( 6.210891007176935652, -0.2719346519345893776, 2.174439262769362280 ) ) ;
#6468 = CARTESIAN_POINT ( 'NONE',  ( -3.793249116773374396, 7.647484079536056356, 0.7998128361456352531 ) ) ;
#6469 = CARTESIAN_POINT ( 'NONE',  ( -3.972702704004144714, 4.593573561881607148, 1.199719254218462483 ) ) ;
#6470 = CYLINDRICAL_SURFACE ( 'NONE', #132658, 2.025000000000006573 ) ;
#6471 = CARTESIAN_POINT ( 'NONE',  ( 6.127406499145813257, 0.1562011534181114436, -2.064545280851529885 ) ) ;
#6472 = DIRECTION ( 'NONE',  ( 0.7592566023652990159, -0.6507913734559659380, 0.000000000000000000 ) ) ;
#6473 = CARTESIAN_POINT ( 'NONE',  ( 1.499999999999987121, -0.7145833326505161009, 0.8660254037844524744 ) ) ;
#6474 = CARTESIAN_POINT ( 'NONE',  ( 4.688067719671657585, -0.9068681981775075229, 1.699704011162524120 ) ) ;
#6475 = CARTESIAN_POINT ( 'NONE',  ( 0.6823417656249969321, 10.52604166700806587, -1.181850606188757036 ) ) ;
#6476 = CARTESIAN_POINT ( 'NONE',  ( -2.819732761962335577, 5.273143408055916304, -1.082531754730543971 ) ) ;
#6477 = CARTESIAN_POINT ( 'NONE',  ( 0.6334296782557496952, 2.055416226174343386, 0.8430641771750585489 ) ) ;
#6479 = ORIENTED_EDGE ( 'NONE', *, *, #122849, .F. ) ;
#6478 = CARTESIAN_POINT ( 'NONE',  ( 2.833104737058811384, 6.457039293210589115, -0.1487728517625390434 ) ) ;
#6481 = CARTESIAN_POINT ( 'NONE',  ( 0.000000000000000000, -4.500000000000003553, 0.000000000000000000 ) ) ;
#6480 = CARTESIAN_POINT ( 'NONE',  ( -2.494940289813118994, 3.499999999999989342, 11.73777120880565583 ) ) ;
#6482 = CARTESIAN_POINT ( 'NONE',  ( 4.552840656090682891, 4.206068941727564514, 1.214306433183764966E-14 ) ) ;
#6483 = CARTESIAN_POINT ( 'NONE',  ( -3.416291520519271874, 6.929497840673697340, 1.040834085586084257E-14 ) ) ;
#6484 = DIRECTION ( 'NONE',  ( 0.000000000000000000, -1.000000000000000000, 0.000000000000000000 ) ) ;
#6485 = AXIS2_PLACEMENT_3D ( 'NONE', #32500, #50884, #135352 ) ;
#6486 = CARTESIAN_POINT ( 'NONE',  ( 11.01931693160843118, 9.191946463694739222, 4.624380626795012716 ) ) ;
#6487 = CARTESIAN_POINT ( 'NONE',  ( 10.34450801710256584, 11.17094022948226240, 0.7216878364870438212 ) ) ;
#6489 = EDGE_CURVE ( 'NONE', #76973, #99811, #113005, .T. ) ;
#6488 = CARTESIAN_POINT ( 'NONE',  ( 1.398799877119625501, 0.3793605821263335565, 1.924665094374561791 ) ) ;
#6490 = CARTESIAN_POINT ( 'NONE',  ( -1.201851678989727383E-14, 3.259375000341420581, -1.575800808251660134 ) ) ;
#6491 = DIRECTION ( 'NONE',  ( 1.224646799147353207E-16, 1.000000000000000000, -0.000000000000000000 ) ) ;
#6492 = CARTESIAN_POINT ( 'NONE',  ( 6.689906388054261299, -1.280585065398877731, -1.486383542710856043 ) ) ;
#6493 = CARTESIAN_POINT ( 'NONE',  ( -8.483651433849100698, 10.92067931095586886, 1.599625672291269396 ) ) ;
#6494 = CARTESIAN_POINT ( 'NONE',  ( -4.406036734316898240, 6.163462161501577441, -1.443375672974051449 ) ) ;
#6495 = CARTESIAN_POINT ( 'NONE',  ( 0.1810634928296238622, -2.195609808662852824, -0.5457317257893978812 ) ) ;
#6497 = EDGE_LOOP ( 'NONE', ( #136821, #141895, #174489, #183087 ) ) ;
#6496 = CARTESIAN_POINT ( 'NONE',  ( -6.013204822860843457, 6.974159367214481264, -1.199719254218446718 ) ) ;
#6498 = CARTESIAN_POINT ( 'NONE',  ( -1.364683531250010295, 5.238541667008086655, -0.7879004041258300672 ) ) ;
#6499 = CARTESIAN_POINT ( 'NONE',  ( 1.000990332655056436, 1.525750722454706443, 1.081861512215509524 ) ) ;
#6500 = CARTESIAN_POINT ( 'NONE',  ( 0.1231123065759693186, 0.2931380485183229800, 1.709000606096510166 ) ) ;
#6502 = CARTESIAN_POINT ( 'NONE',  ( 4.757479570170550787, 2.167726397749652367, -0.3216086267831194112 ) ) ;
#6501 = CARTESIAN_POINT ( 'NONE',  ( -0.6801582343750143256, 1.848958333674724397, -1.178068619123862515 ) ) ;
#6503 = CARTESIAN_POINT ( 'NONE',  ( 4.911288641948820199, 2.004953420984519674, 1.142316731622401882 ) ) ;
#6504 = CARTESIAN_POINT ( 'NONE',  ( 0.1103218441215253337, -0.8811044119183660817, -1.861458889230242164 ) ) ;
#6505 = CARTESIAN_POINT ( 'NONE',  ( 1.992034801999421623, -0.5177828490160235608, -1.871580480717034645 ) ) ;
#6506 = CARTESIAN_POINT ( 'NONE',  ( -5.002595493318215070, 7.819816594637776674, 1.082531754730560403 ) ) ;
#6507 = SURFACE_STYLE_FILL_AREA ( #169027 ) ;
#6508 = ADVANCED_FACE ( 'NONE', ( #60686 ), #119494, .T. ) ;
#6509 = CARTESIAN_POINT ( 'NONE',  ( 0.6801582343749813520, 0.2239583336747300035, 1.178068619123796568 ) ) ;
#6510 = CARTESIAN_POINT ( 'NONE',  ( 3.692029868468839737, 1.730865839653324079, 1.034166058993556181 ) ) ;
#6511 = CARTESIAN_POINT ( 'NONE',  ( -3.728129053633589152, 7.293308295973741195, 0.7216878364870317197 ) ) ;
#6512 = CARTESIAN_POINT ( 'NONE',  ( -6.933015448541747006, 9.181880338089085214, 1.599625672291269396 ) ) ;
#6513 = CARTESIAN_POINT ( 'NONE',  ( 10.07100917685271035, 10.64393221595000938, 0.7998128361456462443 ) ) ;
#6514 = CARTESIAN_POINT ( 'NONE',  ( 0.9964003531478006215, -0.4411313887022934033, -1.771462291394958255 ) ) ;
#6515 = CARTESIAN_POINT ( 'NONE',  ( -4.437261413422502798, 8.398831758960053406, 0.000000000000000000 ) ) ;
#6516 = CARTESIAN_POINT ( 'NONE',  ( -5.061990249855849555, 6.999017606288843396, -1.599625672291271394 ) ) ;
#6517 = CARTESIAN_POINT ( 'NONE',  ( -11.05071387823260487, 4.509444648491869323, 6.218574854545789066 ) ) ;
#6518 = ORIENTED_EDGE ( 'NONE', *, *, #122619, .T. ) ;
#6519 = CARTESIAN_POINT ( 'NONE',  ( 5.084866380259029484, -0.2499542577577648639, -2.045595823183245621 ) ) ;
#6520 = CARTESIAN_POINT ( 'NONE',  ( -6.414416072596837104, 9.537216947121368804, -1.082531754730549967 ) ) ;
#6521 = CARTESIAN_POINT ( 'NONE',  ( 6.983858524370772258, 9.241197259889668558, 1.443375672974063439 ) ) ;
#6522 = CARTESIAN_POINT ( 'NONE',  ( -4.386226389220933441, 5.076017861301227008, -1.199719254218446718 ) ) ;
#6523 = CARTESIAN_POINT ( 'NONE',  ( -8.947491310014823895, 12.52615806407091803, 1.199719254218462483 ) ) ;
#6524 = CARTESIAN_POINT ( 'NONE',  ( 5.584630649692731375, -1.279725605644935760, 1.562507038963067973 ) ) ;
#6526 = ORIENTED_EDGE ( 'NONE', *, *, #214167, .T. ) ;
#6525 = CARTESIAN_POINT ( 'NONE',  ( 5.690131909746282801, 1.321361375537116967, 1.785392519086197671 ) ) ;
#6527 = CARTESIAN_POINT ( 'NONE',  ( -4.787964524281469458, 5.614988695530339413, -1.199719254218453823 ) ) ;
#6528 = CARTESIAN_POINT ( 'NONE',  ( 5.198661835836162481, 8.152523677529138979, 1.199719254218462483 ) ) ;
#6529 = CARTESIAN_POINT ( 'NONE',  ( 4.170816135027268778, -1.922254079802641069, -0.7435701193346122562 ) ) ;
#6530 = CARTESIAN_POINT ( 'NONE',  ( 3.762342404062004597, 1.897698010425369564, -0.6819954029829020659 ) ) ;
#6531 = ORIENTED_EDGE ( 'NONE', *, *, #98433, .T. ) ;
#6532 = DIRECTION ( 'NONE',  ( 0.000000000000000000, -9.023263958591316185E-17, 1.000000000000000000 ) ) ;
#6533 = CARTESIAN_POINT ( 'NONE',  ( 4.241003122976366058, 3.842258486427521103, -0.7998128361456211532 ) ) ;
#6534 = AXIS2_PLACEMENT_3D ( 'NONE', #87452, #5088, #170826 ) ;
#6536 = ORIENTED_EDGE ( 'NONE', *, *, #201142, .T. ) ;
#6535 = CARTESIAN_POINT ( 'NONE',  ( -6.149505192250180663, 9.332117270003974951, -1.199719254218452047 ) ) ;
#6537 = CARTESIAN_POINT ( 'NONE',  ( 5.088145468715395303, 7.830155539619080507, -1.136959649167136543 ) ) ;
#6538 = CARTESIAN_POINT ( 'NONE',  ( 4.481795959180916888, 1.842165523724150544, 0.8196470798618460396 ) ) ;
#6539 = CARTESIAN_POINT ( 'NONE',  ( 3.398233898566359823, 1.450718870894672330, -1.133551952132209717 ) ) ;
#6540 = CARTESIAN_POINT ( 'NONE',  ( 2.494447209962474599, 3.467171072964057910, -11.73545145049397576 ) ) ;
#6541 = CARTESIAN_POINT ( 'NONE',  ( 2.104549495715298590, -2.307096348898482585, 0.05917499873058817972 ) ) ;
#6542 = CARTESIAN_POINT ( 'NONE',  ( 4.947799714344386146, 4.737130853015369958, -0.7998128361456481317 ) ) ;
#6543 = CARTESIAN_POINT ( 'NONE',  ( 3.339309863714147397, -1.908069850993234340, 1.015702806061814734 ) ) ;
#6544 = CARTESIAN_POINT ( 'NONE',  ( 7.422199028477372451, 10.74665040227725044, -1.199719254218441611 ) ) ;
#6545 = CARTESIAN_POINT ( 'NONE',  ( -4.303823697334223652, 7.108545849276850959, -1.199719254218452047 ) ) ;
#6546 = CARTESIAN_POINT ( 'NONE',  ( 3.427438825619326668, 1.030710970775401414, 2.054361689694866211 ) ) ;
#6547 = CARTESIAN_POINT ( 'NONE',  ( 0.7499999999999902300, 4.097916667349481123, -1.299038105676658228 ) ) ;
#6548 = CARTESIAN_POINT ( 'NONE',  ( 2.201827603038747139, -1.870314503716500099, 0.04339327950253490246 ) ) ;
#6549 = CIRCLE ( 'NONE', #89152, 11.09999999999999964 ) ;
#6550 = CARTESIAN_POINT ( 'NONE',  ( 0.4738186427182951577, 1.131346554974651086, 1.614239802345132757 ) ) ;
#6552 = CARTESIAN_POINT ( 'NONE',  ( -6.831329296439251131, 9.063246493969506545, -1.599625672291271394 ) ) ;
#6551 = CARTESIAN_POINT ( 'NONE',  ( 1.364683531249990311, 4.634375000341417916, 1.214306433183764966E-14 ) ) ;
#6554 = CARTESIAN_POINT ( 'NONE',  ( 2.174722684859807575, -1.356406721008751814, 1.740749382485320407 ) ) ;
#6553 = CARTESIAN_POINT ( 'NONE',  ( -6.087774667736030487, 7.061157519568837415, 1.199719254218450271 ) ) ;
#6555 = LINE ( 'NONE', #139807, #74618 ) ;
#6556 = CARTESIAN_POINT ( 'NONE',  ( 4.924636110261782385, 6.768494766770632332, 1.599625672291267398 ) ) ;
#6557 = CARTESIAN_POINT ( 'NONE',  ( -3.601662362724658895, 7.353689856487406473, -0.7998128361456281477 ) ) ;
#6558 = CARTESIAN_POINT ( 'NONE',  ( -8.029456579251441184, -5.199789852012339786, 7.518896314322614849 ) ) ;
#6559 = CARTESIAN_POINT ( 'NONE',  ( 6.069206959712960980, 0.1456670527590266107, -1.966150735595481258 ) ) ;
#6560 = CARTESIAN_POINT ( 'NONE',  ( 5.514422467339478828, -1.033062203415137992, -2.063637023464809594 ) ) ;
#6561 = CARTESIAN_POINT ( 'NONE',  ( 0.1683002474503410839, -0.8351952195557797998, -1.773497582445908938 ) ) ;
#6562 = CARTESIAN_POINT ( 'NONE',  ( 2.746997431529357492, -0.3482204723163102034, -2.032804898803519222 ) ) ;
#6563 = CARTESIAN_POINT ( 'NONE',  ( 7.646435448427411963, 8.023188899361205273, -0.7216878364870257245 ) ) ;
#6564 = EDGE_CURVE ( 'NONE', #45616, #11502, #160330, .T. ) ;
#6565 = CARTESIAN_POINT ( 'NONE',  ( 3.573456005653643519, 6.326726552307992080, -1.199719254218453823 ) ) ;
#6566 = CARTESIAN_POINT ( 'NONE',  ( 6.263503779389103521, 10.25124547602188763, 1.040834085586084257E-14 ) ) ;
#6567 = CARTESIAN_POINT ( 'NONE',  ( 1.364683531249988535, 2.967708333674755394, -0.7879004041258239610 ) ) ;
#6568 = CARTESIAN_POINT ( 'NONE',  ( 0.000000000000000000, 0.06547992991065912372, 0.000000000000000000 ) ) ;
#6569 = CARTESIAN_POINT ( 'NONE',  ( 4.650083499362864359, 7.408552601689905259, 1.082531754730558626 ) ) ;
#6570 = CARTESIAN_POINT ( 'NONE',  ( 5.143125006682406131, -0.2608717942136177248, -2.155377805267975067 ) ) ;
#6572 = CARTESIAN_POINT ( 'NONE',  ( 5.706567001488551227, 1.626822141722890303, 0.8623401093873286349 ) ) ;
#6571 = CARTESIAN_POINT ( 'NONE',  ( -11.44789321844504215, 9.800000000000000711, -3.303298730975397834 ) ) ;
#6573 = CYLINDRICAL_SURFACE ( 'NONE', #33875, 1.250000000000000000 ) ;
#6574 = CARTESIAN_POINT ( 'NONE',  ( 4.549612403093820312, 8.500000000000243361, -0.2314049244472246580 ) ) ;
#6575 = CARTESIAN_POINT ( 'NONE',  ( 0.3329892237508432218, -1.712944741146246841, 0.7519245212838021608 ) ) ;
#6576 = CARTESIAN_POINT ( 'NONE',  ( 0.7907308791721240349, -2.245476950237018432, -0.2759641350603259657 ) ) ;
#6577 = CARTESIAN_POINT ( 'NONE',  ( -4.265659997730736563, 7.487761795085347671, 1.069252549957976361 ) ) ;
#6578 = CARTESIAN_POINT ( 'NONE',  ( -0.2366305240106678365, 2.663423291230584411, 2.061984645680444928 ) ) ;
#6579 = CARTESIAN_POINT ( 'NONE',  ( 6.059925523928845870, 7.140772946495586915, 1.155538509043469997 ) ) ;
#6580 = AXIS2_PLACEMENT_3D ( 'NONE', #81953, #126534, #44147 ) ;
#6581 = CARTESIAN_POINT ( 'NONE',  ( -0.1108833634136767443, 0.0002062650063822807356, -1.896853557917008271 ) ) ;
#6582 = CARTESIAN_POINT ( 'NONE',  ( 1.375481398426938284, 1.050436561215197351, 1.424246879149461797 ) ) ;
#6583 = CARTESIAN_POINT ( 'NONE',  ( -0.04057498839846879202, -1.478066481919372510, -1.213044814162365981 ) ) ;
#6585 = CARTESIAN_POINT ( 'NONE',  ( 2.917496427270527715, -1.288711974188415654, -1.417462588220135933 ) ) ;
#6584 = CARTESIAN_POINT ( 'NONE',  ( -9.450196763925152510, 10.98398329845622001, -1.199719254218441611 ) ) ;
#6586 = CARTESIAN_POINT ( 'NONE',  ( -0.1409997244346088419, 5.722143553014046979, -2.594341442600463843 ) ) ;
#6587 = CARTESIAN_POINT ( 'NONE',  ( 4.633233401965040521, 0.002145104102065781716, -1.969739563307022712 ) ) ;
#6588 = CARTESIAN_POINT ( 'NONE',  ( -0.05226516427493665962, -1.936187138999283297, 0.8653993394739032397 ) ) ;
#6589 = CARTESIAN_POINT ( 'NONE',  ( -2.676845263694313637, 5.210404343363602919, -1.199719254218446718 ) ) ;
#6590 = CARTESIAN_POINT ( 'NONE',  ( 2.676452114398766291, -1.789519730395791486, -0.5449050523786898026 ) ) ;
#6592 = ORIENTED_EDGE ( 'NONE', *, *, #208257, .F. ) ;
#6591 = CARTESIAN_POINT ( 'NONE',  ( 6.656889574143706412, -1.327764893807031221, 1.100862838992909598 ) ) ;
#6594 = CARTESIAN_POINT ( 'NONE',  ( 3.389175213736292047, 5.937492935125556315, 1.082531754730558626 ) ) ;
#6593 = CARTESIAN_POINT ( 'NONE',  ( 2.789901687333019797, 1.561178712900921584, 1.560079944692857046 ) ) ;
#6595 = CARTESIAN_POINT ( 'NONE',  ( -1.364683531250012516, 3.801041667008087099, -0.7879004041258300672 ) ) ;
#6596 = CARTESIAN_POINT ( 'NONE',  ( 0.9243725180730785196, 1.015136377070953388, 1.795498427122848017 ) ) ;
#6598 = VECTOR ( 'NONE', #206948, 1000.000000000000000 ) ;
#6597 = CARTESIAN_POINT ( 'NONE',  ( 8.437251666405968464, 8.737881787095446384, 1.040834085586084257E-14 ) ) ;
#6599 = DIRECTION ( 'NONE',  ( 0.000000000000000000, -1.000000000000000000, 0.000000000000000000 ) ) ;
#6600 = DIRECTION ( 'NONE',  ( 1.000000000000000000, -0.000000000000000000, -0.000000000000000000 ) ) ;
#6601 = CARTESIAN_POINT ( 'NONE',  ( 0.1747926744264712562, 2.889263262932476817, -2.344248796821886138 ) ) ;
#6602 = CARTESIAN_POINT ( 'NONE',  ( -7.712222144930493073, -6.293595771081174739, -7.712222144930445999 ) ) ;
#6603 = ORIENTED_EDGE ( 'NONE', *, *, #84346, .T. ) ;
#6604 = CARTESIAN_POINT ( 'NONE',  ( 2.893098739488662030, 0.2508700648995808025, 2.055025655848155886 ) ) ;
#6605 = CARTESIAN_POINT ( 'NONE',  ( 1.499999999999987121, 3.295833333333354709, -0.8660254037844262731 ) ) ;
#6606 = CARTESIAN_POINT ( 'NONE',  ( 4.039439701867726384, 6.800097854565950506, 1.199719254218462483 ) ) ;
#6607 = CARTESIAN_POINT ( 'NONE',  ( -6.533345026022147728, 6.811601368426168257, 0.5105341503897353750 ) ) ;
#6608 = CARTESIAN_POINT ( 'NONE',  ( 1.067063705314938771, -1.590654782179411031, 1.244411004956039291 ) ) ;
#6609 = CARTESIAN_POINT ( 'NONE',  ( -0.9486429539237359876, 2.855410930033766004, 1.028101543438980858 ) ) ;
#6610 = EDGE_CURVE ( 'NONE', #7772, #62106, #136314, .T. ) ;
#6611 = CARTESIAN_POINT ( 'NONE',  ( -0.6823417656250212460, 4.301041667008085767, 1.181850606188767472 ) ) ;
#6613 = CARTESIAN_POINT ( 'NONE',  ( 8.080296364064698977, 12.37083682481011060, -0.7216878364870328300 ) ) ;
#6612 = CARTESIAN_POINT ( 'NONE',  ( 0.1745949693968692484, 0.009193469831055355729, -1.755468632744116242 ) ) ;
#6614 = CARTESIAN_POINT ( 'NONE',  ( 4.921249881687196570, 0.7690040753521176775, 1.863882819927860313 ) ) ;
#6615 = CARTESIAN_POINT ( 'NONE',  ( 6.438697963858233564, -1.475898738386885123, 1.221124472464208743 ) ) ;
#6616 = CARTESIAN_POINT ( 'NONE',  ( 6.639320575229244348, 1.270172395628932360, 2.119701008677194132 ) ) ;
#6617 = CARTESIAN_POINT ( 'NONE',  ( 3.650093349144762023, 0.7902683543556283663, 2.044282924279612779 ) ) ;
#6618 = CARTESIAN_POINT ( 'NONE',  ( 0.7499999999999902300, 2.264583334016148530, 1.299038105676669330 ) ) ;
#6619 = CARTESIAN_POINT ( 'NONE',  ( 2.847809051801777791, -1.287500320553297994, -1.414207669007704116 ) ) ;
#6620 = CARTESIAN_POINT ( 'NONE',  ( -5.636439174979254396, 7.598931675607687453, -1.599625672291256295 ) ) ;
#6621 = EDGE_CURVE ( 'NONE', #175139, #70421, #53455, .T. ) ;
#6622 = CARTESIAN_POINT ( 'NONE',  ( 5.626270559546826533, 5.666329862333828515, 0.7216878364870317197 ) ) ;
#6624 = CARTESIAN_POINT ( 'NONE',  ( 0.5093889453341126083, -1.913797760093600919, 0.6352206787166372326 ) ) ;
#6623 =( NAMED_UNIT ( * ) PLANE_ANGLE_UNIT ( ) SI_UNIT ( $, .RADIAN. ) );
#6625 = CARTESIAN_POINT ( 'NONE',  ( -1.364683531250000748, 10.67187500034139802, 0.000000000000000000 ) ) ;
#6627 = CARTESIAN_POINT ( 'NONE',  ( -5.607179047703544583, 8.699403434699558346, 1.199719254218454489 ) ) ;
#6626 = CARTESIAN_POINT ( 'NONE',  ( 5.847271748948593029, 0.6375361197438635941, -2.096799129279611762 ) ) ;
#6629 = EDGE_LOOP ( 'NONE', ( #142802, #100215, #187967, #175350, #153356, #26686 ) ) ;
#6628 = CARTESIAN_POINT ( 'NONE',  ( 2.766273355629506714, -1.191139867243676598, 1.247637197061921555 ) ) ;
#6630 = CARTESIAN_POINT ( 'NONE',  ( 6.047156637250688860, 0.2094617991648151656, 2.110256208591613003 ) ) ;
#6631 = CARTESIAN_POINT ( 'NONE',  ( 7.904567251967224095, 9.180748867838630645, 1.199719254218462483 ) ) ;
#6632 = CARTESIAN_POINT ( 'NONE',  ( 3.988069740714122791, 7.804498464141805592, 0.7998128361456321445 ) ) ;
#6633 = DIRECTION ( 'NONE',  ( -0.000000000000000000, -8.546850786086437571E-32, -1.000000000000000000 ) ) ;
#6634 = CARTESIAN_POINT ( 'NONE',  ( 0.4499999999999903522, 3.949999999999988187, -0.8338124244295659349 ) ) ;
#6635 = DIRECTION ( 'NONE',  ( 0.000000000000000000, -7.254698431505058073E-17, 1.000000000000000000 ) ) ;
#6636 = CARTESIAN_POINT ( 'NONE',  ( 4.482942347612929979, 8.381849838857084123, 1.040834085586084257E-14 ) ) ;
#6637 = DIRECTION ( 'NONE',  ( 0.000000000000000000, 0.000000000000000000, 1.000000000000000000 ) ) ;
#6638 = EDGE_LOOP ( 'NONE', ( #124575, #65665, #31410, #32397, #104320, #120467, #203236, #199464, #168970 ) ) ;
#6639 =( LENGTH_UNIT ( ) NAMED_UNIT ( * ) SI_UNIT ( .MILLI., .METRE. ) );
#6640 = B_SPLINE_CURVE_WITH_KNOTS ( 'NONE', 3,
 ( #136123, #105787, #55930, #53796, #167540, #169671, #21258, #87364, #121016, #153432, #188046, #154503, #88441, #5004, #104691, #71077 ),
 .UNSPECIFIED., .F., .F.,
 ( 4, 3, 3, 3, 3, 4 ),
 ( 0.000000000000000000, 2.208392919728564190E-05, 5.593630375490294554E-05, 8.978950068604114713E-05, 0.0001236430975991122182, 0.0001574962648025070408 ),
 .UNSPECIFIED. ) ;
#6641 = EDGE_LOOP ( 'NONE', ( #175472, #208962, #21810, #13960 ) ) ;
#6642 = CARTESIAN_POINT ( 'NONE',  ( 2.314858244453772862, 1.454059926310177220, -1.080092325806664144 ) ) ;
#6643 = VERTEX_POINT ( 'NONE', #57501 ) ;
#6644 = CARTESIAN_POINT ( 'NONE',  ( 9.541187415715040032, 12.15447128979948310, -1.599625672291262513 ) ) ;
#6645 = DIRECTION ( 'NONE',  ( 1.000000000000000000, -0.000000000000000000, 1.779758311459929752E-16 ) ) ;
#6646 = CARTESIAN_POINT ( 'NONE',  ( 3.650846288169238729, 0.2690317868887618369, 1.791254203397556477 ) ) ;
#6647 = CARTESIAN_POINT ( 'NONE',  ( 8.122743427918724279, 8.649157885426255632, 0.7216878364870267237 ) ) ;
#6648 = COLOUR_RGB ( '', 0.31764706, 0.68627451, 0.89019608) ;
#6649 = CARTESIAN_POINT ( 'NONE',  ( 10.97010717055062479, 13.80000000000000071, -1.696399592028411396 ) ) ;
#6650 = CARTESIAN_POINT ( 'NONE',  ( 5.197613018050254219, 6.434050360596694773, 1.175743713691650871 ) ) ;
#6651 = AXIS2_PLACEMENT_3D ( 'NONE', #173243, #146076, #207837 ) ;
#6653 = CARTESIAN_POINT ( 'NONE',  ( -0.6823417656250003738, 14.90104166700806410, 1.181850606188754593 ) ) ;
#6652 = CARTESIAN_POINT ( 'NONE',  ( 5.635155393647417910, -0.04589315835645593061, -1.860648885492953486 ) ) ;
#6654 = CARTESIAN_POINT ( 'NONE',  ( 2.214329231836575040, 1.858617268789555466, 0.4632827458446056035 ) ) ;
#6655 =( NAMED_UNIT ( * ) SI_UNIT ( $, .STERADIAN. ) SOLID_ANGLE_UNIT ( ) );
#6656 = CARTESIAN_POINT ( 'NONE',  ( -11.69380381030441107, 8.410673437356566140, -1.083569014401829955 ) ) ;
#6657 = EDGE_CURVE ( 'NONE', #194727, #183165, #94290, .T. ) ;
#6658 = CARTESIAN_POINT ( 'NONE',  ( 4.834028091705433461, 8.209959199513299666, 0.9267959391740541175 ) ) ;
#6659 = CARTESIAN_POINT ( 'NONE',  ( -10.99943760478737786, -9.902953797791679946, 0.1112316694888332708 ) ) ;
#6660 = CARTESIAN_POINT ( 'NONE',  ( 6.925078400183578786, 0.5640289027524867382, 2.196098379985710114 ) ) ;
#6661 = CARTESIAN_POINT ( 'NONE',  ( 7.049876689426101350, 9.247942109129029475, -1.443375672974057666 ) ) ;
#6662 = CARTESIAN_POINT ( 'NONE',  ( -4.613852347352193739, 4.277249248199312071, 1.214306433183764966E-14 ) ) ;
#6663 = CARTESIAN_POINT ( 'NONE',  ( -9.500370076773343442, -7.189371949516671023, 0.005973655271411463206 ) ) ;
#6664 = CARTESIAN_POINT ( 'NONE',  ( 1.781308773403101231, 1.442672104170627190, 1.513329462076596243 ) ) ;
#6665 = CARTESIAN_POINT ( 'NONE',  ( 6.194356126197313017, -1.917168722191398000, -0.1884046653951119699 ) ) ;
#6666 = CARTESIAN_POINT ( 'NONE',  ( -6.078132937628113908, 5.985576603521232109, 1.040834085586084257E-14 ) ) ;
#6667 = CARTESIAN_POINT ( 'NONE',  ( 2.713660727937648787, -1.805999004224107196, 0.2657717501357085843 ) ) ;
#6668 = CARTESIAN_POINT ( 'NONE',  ( 3.141465813989018141, -1.946189201368169641, 1.040519825639886431 ) ) ;
#6669 = CARTESIAN_POINT ( 'NONE',  ( 11.89204169242350595, 12.30000000000000071, 0.8046421800351223341 ) ) ;
#6670 = CARTESIAN_POINT ( 'NONE',  ( 0.7383556378116812313, 1.137082172773289379, -1.537495029474859276 ) ) ;
#6671 = CARTESIAN_POINT ( 'NONE',  ( 1.275766937089892750, -1.922257851437941811, 0.4282784019480969651 ) ) ;
#6672 = CARTESIAN_POINT ( 'NONE',  ( 3.720204347993858462, 1.845125290474887159, 0.6061553137183937068 ) ) ;
#6673 = ORIENTED_EDGE ( 'NONE', *, *, #72117, .T. ) ;
#6674 = CARTESIAN_POINT ( 'NONE',  ( -1.123270288250342919, 3.096052654332833054, 0.7749999999993751887 ) ) ;
#6676 = CARTESIAN_POINT ( 'NONE',  ( 0.1329588055935396196, 0.006246367379872731426, -1.846049620084761367 ) ) ;
#6675 = CARTESIAN_POINT ( 'NONE',  ( -3.955946960137363799, 7.837298230127379917, 0.7998128361456352531 ) ) ;
#6677 = CARTESIAN_POINT ( 'NONE',  ( 5.248941747146098180, 6.152795455539095570, -1.199719254218452047 ) ) ;
#6678 = CARTESIAN_POINT ( 'NONE',  ( 0.3870642018030800990, -8.176227079964631272, 9.516228778038660963 ) ) ;
#6679 = CARTESIAN_POINT ( 'NONE',  ( 8.992082194361556091, 11.51384853155376220, 1.599625672291279388 ) ) ;
#6680 = CARTESIAN_POINT ( 'NONE',  ( -6.448838341955544173, 7.552674816150118708, 1.199719254218452047 ) ) ;
#6681 = CARTESIAN_POINT ( 'NONE',  ( 3.231779075379137556, 6.036511184309975242, -0.9899555337401846344 ) ) ;
#6682 = VERTEX_POINT ( 'NONE', #90015 ) ;
#6683 = CARTESIAN_POINT ( 'NONE',  ( 5.905458427204159477, 9.047396044116986502, 1.199719254218452047 ) ) ;
#6684 = DIRECTION ( 'NONE',  ( -0.000000000000000000, 0.000000000000000000, -1.000000000000000000 ) ) ;
#6686 = CARTESIAN_POINT ( 'NONE',  ( 5.928922775424462444, -1.700964743930567513, 1.082835439959836776 ) ) ;
#6685 = CARTESIAN_POINT ( 'NONE',  ( 3.351995281737112364, 1.825872481133209879, -0.0009662468829912954560 ) ) ;
#6687 = FILL_AREA_STYLE_COLOUR ( '', #149406 ) ;
#6688 = CARTESIAN_POINT ( 'NONE',  ( -10.49364770729726359, 11.34493653470939023, 0.7216878364870438212 ) ) ;
#6689 = MECHANICAL_DESIGN_GEOMETRIC_PRESENTATION_REPRESENTATION (  '', ( #183110 ), #96735 ) ;
#6690 = CARTESIAN_POINT ( 'NONE',  ( -4.733024909954385073, 8.320217716143888609, 0.7565452571775049817 ) ) ;
#6691 = DIRECTION ( 'NONE',  ( -0.6783731810844091381, 0.000000000000000000, -0.7347175152297780176 ) ) ;
#6692 = CARTESIAN_POINT ( 'NONE',  ( 4.135518821028766112, -1.289757458839156934, -1.355179912160727085 ) ) ;
#6693 = CARTESIAN_POINT ( 'NONE',  ( 7.727257484784855635, 11.10255193463598111, -1.199719254218446718 ) ) ;
#6694 = CARTESIAN_POINT ( 'NONE',  ( 2.086434564137104264, -1.889293373815591481, -0.3759864732829041878 ) ) ;
#6695 = CARTESIAN_POINT ( 'NONE',  ( 6.420756404446520627, -1.389671697431221542, 1.384925340169262054 ) ) ;
#6696 = CARTESIAN_POINT ( 'NONE',  ( -0.6823417656250039265, 8.630208333674733723, -1.181850606188755259 ) ) ;
#6697 = CARTESIAN_POINT ( 'NONE',  ( -6.388916700537716764, 8.476822122092563916, 1.599625672291283607 ) ) ;
#6698 = CARTESIAN_POINT ( 'NONE',  ( 3.472859903394816872, 7.203420320602605287, -0.7998128361456291469 ) ) ;
#6699 = CARTESIAN_POINT ( 'NONE',  ( -4.868786560638931782, 6.773613302202437403, 1.443375672974058777 ) ) ;
#6700 = CARTESIAN_POINT ( 'NONE',  ( 0.5974486649760869517, -0.3061723685214760016, 2.094854868064464970 ) ) ;
#6701 = CARTESIAN_POINT ( 'NONE',  ( 1.737499999999999378, -2.216666666666665453, -3.009438278150925683 ) ) ;
#6702 = CARTESIAN_POINT ( 'NONE',  ( 4.680570891794395116, 1.277791010243028991, -1.628752506732597638 ) ) ;
#6704 = CARTESIAN_POINT ( 'NONE',  ( -1.364683531250012516, 2.301041667008087988, -0.7879004041258289570 ) ) ;
#6703 = CARTESIAN_POINT ( 'NONE',  ( 0.04610459085982108324, -1.479553692838073475, 1.095721268101347734 ) ) ;
#6705 = CARTESIAN_POINT ( 'NONE',  ( 4.887441975664971849, -0.7727101442582262614, -2.165022144963870243 ) ) ;
#6706 = CARTESIAN_POINT ( 'NONE',  ( 7.619319141200072920, 7.991553207595983643, 0.7216878364870317197 ) ) ;
#6708 = DIRECTION ( 'NONE',  ( 0.000000000000000000, 0.000000000000000000, 1.000000000000000000 ) ) ;
#6707 = CARTESIAN_POINT ( 'NONE',  ( 3.106226591306694651, 6.638031766584184368, 0.000000000000000000 ) ) ;
#6709 = CARTESIAN_POINT ( 'NONE',  ( 0.6566820891428931661, -1.656472902050255991, 1.584714856167362074 ) ) ;
#6710 = CARTESIAN_POINT ( 'NONE',  ( 1.264911064067342217, 3.850000000000006306, -0.4999999999999987232 ) ) ;
#6711 = CARTESIAN_POINT ( 'NONE',  ( -6.343235766347277149, 8.493804042195527870, -1.599625672291271394 ) ) ;
#6712 = CARTESIAN_POINT ( 'NONE',  ( 5.226486033959851341, 0.1448775283907685063, 1.936603901228886926 ) ) ;
#6713 = VERTEX_POINT ( 'NONE', #10856 ) ;
#6714 = CARTESIAN_POINT ( 'NONE',  ( 9.558135107509954764, 10.25350516829085379, -0.7216878364870257245 ) ) ;
#6715 = VERTEX_POINT ( 'NONE', #191743 ) ;
#6716 = CARTESIAN_POINT ( 'NONE',  ( -0.1755273284492936958, -0.8636782348834280976, -1.816524446017355743 ) ) ;
#6717 = CARTESIAN_POINT ( 'NONE',  ( 5.981657729715995409, -0.6748525008196132324, 1.900413905137773529 ) ) ;
#6718 = CARTESIAN_POINT ( 'NONE',  ( -8.130085669689073313, 12.63685038127928806, 0.7998128361456481317 ) ) ;
#6719 = CARTESIAN_POINT ( 'NONE',  ( 3.285556943749998737, -1.042708332855377451, -1.896917185911906500 ) ) ;
#6721 = CARTESIAN_POINT ( 'NONE',  ( 1.463349669262783870, 1.744408624272808073, -0.2979475530153224416 ) ) ;
#6720 = CARTESIAN_POINT ( 'NONE',  ( 2.677772397998368081, -1.073972967945693080, 1.793542233829773291 ) ) ;
#6722 = CARTESIAN_POINT ( 'NONE',  ( 6.434220164165640021, -1.621181005584397372, -1.198863592720422977 ) ) ;
#6724 = CARTESIAN_POINT ( 'NONE',  ( 4.734495095973747070, 0.3888400998970488187, 2.258902165976091059 ) ) ;
#6723 = PRESENTATION_STYLE_ASSIGNMENT (( #156218 ) ) ;
#6725 = CARTESIAN_POINT ( 'NONE',  ( 2.677380959318215847, -0.8946470780417746793, 1.492600998661142375 ) ) ;
#6726 = CARTESIAN_POINT ( 'NONE',  ( 4.325214697959421706, 5.004837554829479451, 1.199719254218462483 ) ) ;
#6727 = AXIS2_PLACEMENT_3D ( 'NONE', #5743, #88104, #20933 ) ;
#6728 = CARTESIAN_POINT ( 'NONE',  ( 2.372030889105484430, -0.3844106184479143540, 1.690481094739235912 ) ) ;
#6729 = CARTESIAN_POINT ( 'NONE',  ( 1.360316468749978469, 2.296875000341369599, -4.857225732735059864E-14 ) ) ;
#6730 = CARTESIAN_POINT ( 'NONE',  ( 1.750234856725553900, -1.851685525784763975, -0.1866200871585097509 ) ) ;
#6731 = CARTESIAN_POINT ( 'NONE',  ( 2.998652106967353514, 2.154486853421373027, 0.2683346083656880099 ) ) ;
#6732 = CARTESIAN_POINT ( 'NONE',  ( 4.798696304233017074, 7.685897223992134819, -1.199719254218452047 ) ) ;
#6733 = CARTESIAN_POINT ( 'NONE',  ( 4.926970384345759513, -1.727065721694167832, 1.040790168839386798 ) ) ;
#6734 = CARTESIAN_POINT ( 'NONE',  ( 1.687500000000001110, -1.451031289061048835, 1.451031289061190055 ) ) ;
#6735 = CARTESIAN_POINT ( 'NONE',  ( 0.7499999999999902300, 2.764583334016148974, 1.299038105676669330 ) ) ;
#6736 = CARTESIAN_POINT ( 'NONE',  ( 1.553604983729965472, 0.5615451523532221101, -1.842721482554928514 ) ) ;
#6737 = CARTESIAN_POINT ( 'NONE',  ( 1.364683531249997417, 14.98437500034140157, 2.602085213965210642E-15 ) ) ;
#6738 = CARTESIAN_POINT ( 'NONE',  ( 4.851916359752673991, -1.571614379473328160, -1.570179378767898370 ) ) ;
#6739 = VERTEX_POINT ( 'NONE', #92160 ) ;
#6740 = CARTESIAN_POINT ( 'NONE',  ( -0.2108831679770960255, -0.001785917861228669690, -1.896958272444612792 ) ) ;
#6741 = CARTESIAN_POINT ( 'NONE',  ( 1.499999999999987566, 0.02500000000001806333, 0.000000000000000000 ) ) ;
#6742 = CARTESIAN_POINT ( 'NONE',  ( 7.182068686937156166, 9.402166106225269715, 1.599625672291281386 ) ) ;
#6743 = CARTESIAN_POINT ( 'NONE',  ( 1.364683531249986537, -0.09479166632524321789, -0.7879004041258309554 ) ) ;
#6744 = CARTESIAN_POINT ( 'NONE',  ( 0.08310686162707729696, -1.445780664108237801, 1.686489957186103839 ) ) ;
#6746 = EDGE_CURVE ( 'NONE', #154836, #212421, #35941, .T. ) ;
#6745 = CARTESIAN_POINT ( 'NONE',  ( 6.320756440275017596, -1.388331291134708767, 1.386421665916007795 ) ) ;
#6747 = CARTESIAN_POINT ( 'NONE',  ( 9.598809568795314107, 10.30095870645710754, -0.7216878364870257245 ) ) ;
#6748 = CIRCLE ( 'NONE', #41284, 11.99999999999999112 ) ;
#6749 = LINE ( 'NONE', #125947, #173657 ) ;
#6750 = CARTESIAN_POINT ( 'NONE',  ( 5.712299329104530088, -1.009927678917849736, -2.024548151048012556 ) ) ;
#6751 = CARTESIAN_POINT ( 'NONE',  ( -4.340018570150309785, 7.117086527600392287, -1.082531754730551743 ) ) ;
#6752 = CARTESIAN_POINT ( 'NONE',  ( 2.980982186342299833, 1.941357688518682290, 0.6972846330933372139 ) ) ;
#6753 = CARTESIAN_POINT ( 'NONE',  ( -5.259673527097670664, 8.223703984000886535, -1.199719254218446718 ) ) ;
#6754 =( BOUNDED_SURFACE ( )  B_SPLINE_SURFACE ( 3, 2, ( 
 ( #121485, #174439, #123627 ),
 ( #71557, #189591, #42302 ),
 ( #108417, #41237, #122562 ),
 ( #43366, #24950, #107344 ) ),
 .UNSPECIFIED., .F., .F., .T. ) 
 B_SPLINE_SURFACE_WITH_KNOTS ( ( 4, 4 ),
 ( 3, 3 ),
 ( 5.985662991026288423E-05, 0.0001887152224066689804 ),
 ( 0.000000000000000000, 1.000000000000000000 ),
 .UNSPECIFIED. ) 
 GEOMETRIC_REPRESENTATION_ITEM ( )  RATIONAL_B_SPLINE_SURFACE ( (
 ( 1.000000000000000000, 0.8739472344185998942, 1.000000000000000000),
 ( 1.000000000000000000, 0.8497613059193734886, 1.000000000000000000),
 ( 1.000000000000000000, 0.8164163343283138419, 1.000000000000000000),
 ( 1.000000000000000000, 0.7779734834199523164, 1.000000000000000000) ) ) 
 REPRESENTATION_ITEM ( '' )  SURFACE ( )  );
#6755 = CARTESIAN_POINT ( 'NONE',  ( -0.7500000000000006661, 2.389583334016155636, -1.299038105676652011 ) ) ;
#6756 = CARTESIAN_POINT ( 'NONE',  ( -1.364683531250010295, 4.842708333674756283, 0.7879004041258379498 ) ) ;
#6757 = CARTESIAN_POINT ( 'NONE',  ( 4.411305886619627081, -0.3218996851035611506, 1.842484647571709822 ) ) ;
#6758 = CARTESIAN_POINT ( 'NONE',  ( 3.533592999799278989, -1.415137147236225079, 1.001973916141611687 ) ) ;
#6759 = CARTESIAN_POINT ( 'NONE',  ( 3.386022052710332186, -0.3430625053944387770, -1.706099273433875130 ) ) ;
#6760 = CARTESIAN_POINT ( 'NONE',  ( 1.119135019589584834, -0.04993059730015738523, 2.291989107133483028 ) ) ;
#6761 = CARTESIAN_POINT ( 'NONE',  ( 1.364683531249988535, 3.717708333674750953, -0.7879004041258239610 ) ) ;
#6762 = CARTESIAN_POINT ( 'NONE',  ( 4.757415945720180339, 2.067795187486476394, -0.3081579728113920669 ) ) ;
#6763 = CARTESIAN_POINT ( 'NONE',  ( 6.175724022258248347, -1.036883830621424307, 1.641789595683869729 ) ) ;
#6764 = CARTESIAN_POINT ( 'NONE',  ( 9.228859063121788608, 14.17280082594779600, 7.673751449575783035 ) ) ;
#6765 =( NAMED_UNIT ( * ) SI_UNIT ( $, .STERADIAN. ) SOLID_ANGLE_UNIT ( ) );
#6766 = CARTESIAN_POINT ( 'NONE',  ( 0.9322677863709986079, -1.591319861332978425, -1.238319039483272599 ) ) ;
#6767 = CARTESIAN_POINT ( 'NONE',  ( 0.4750491441844888474, -1.531729482103380224, 1.466773057065169361 ) ) ;
#6768 = CARTESIAN_POINT ( 'NONE',  ( -8.259941899223614215, 10.65968485389279508, -1.599625672291263179 ) ) ;
#6769 = CARTESIAN_POINT ( 'NONE',  ( 5.309989718046547402, 9.346738437696316737, 0.7998128361456462443 ) ) ;
#6770 = DIRECTION ( 'NONE',  ( 0.000000000000000000, -1.000000000000000000, 0.000000000000000000 ) ) ;
#6771 = CARTESIAN_POINT ( 'NONE',  ( 4.811078068098579408, 1.589968679568127596, 0.8971634079883783475 ) ) ;
#6772 = ORIENTED_EDGE ( 'NONE', *, *, #124997, .T. ) ;
#6773 = CARTESIAN_POINT ( 'NONE',  ( -5.302647476276252547, 5.359045941843285199, 0.7216878364870257245 ) ) ;
#6774 = DIRECTION ( 'NONE',  ( -0.000000000000000000, -1.000000000000000000, -0.000000000000000000 ) ) ;
#6775 = CARTESIAN_POINT ( 'NONE',  ( 0.000000000000000000, -3.893749999044084031, -4.012584370867899430 ) ) ;
#6776 = CARTESIAN_POINT ( 'NONE',  ( -6.775324078527193983, 8.927630729746953264, -1.599625672291263179 ) ) ;
#6777 = CARTESIAN_POINT ( 'NONE',  ( 2.162373415809074828, 2.019440163517810749, 0.04526320522070524655 ) ) ;
#6778 = CARTESIAN_POINT ( 'NONE',  ( 6.124089168553260798, -1.220954261165616783, -1.838047742986161026 ) ) ;
#6779 = CARTESIAN_POINT ( 'NONE',  ( -4.122561227007127016, 6.967349310553715647, 1.199719254218452935 ) ) ;
#6780 = CARTESIAN_POINT ( 'NONE',  ( 3.063170293922971243, 1.569483505267080359, 0.9996245905467721071 ) ) ;
#6781 = CARTESIAN_POINT ( 'NONE',  ( 3.999819011231439347, 4.625209253646830554, 1.199719254218464037 ) ) ;
#6782 = DIRECTION ( 'NONE',  ( 0.000000000000000000, -1.000000000000000000, 0.000000000000000000 ) ) ;
#6783 = ORIENTED_EDGE ( 'NONE', *, *, #38562, .T. ) ;
#6784 = CARTESIAN_POINT ( 'NONE',  ( -3.581325132304157943, 7.329963087663487364, -0.7998128361456281477 ) ) ;
#6785 = CARTESIAN_POINT ( 'NONE',  ( -7.971304249830880373, 11.38727316052296601, 1.199719254218453823 ) ) ;
#6786 = CARTESIAN_POINT ( 'NONE',  ( 5.268108045213575785, 0.9031548532531764595, 1.586571422427636824 ) ) ;
#6788 = CARTESIAN_POINT ( 'NONE',  ( -4.351531800032816477, 7.393666969396889499, -1.175081553336376317 ) ) ;
#6787 = CARTESIAN_POINT ( 'NONE',  ( -5.191846479390389568, 5.021852078902356631, 0.7998128361456281477 ) ) ;
#6789 = CARTESIAN_POINT ( 'NONE',  ( 6.604949037901548969, 6.766875157141204689, 0.08182522243922914218 ) ) ;
#6790 = CARTESIAN_POINT ( 'NONE',  ( 0.3504316985127345907, -0.8248687954017698276, 1.525068808560197109 ) ) ;
#6791 = CARTESIAN_POINT ( 'NONE',  ( 6.632757984263843554, -1.642112545546599023, 0.8327811610863435909 ) ) ;
#6792 = CARTESIAN_POINT ( 'NONE',  ( 5.549573066657292664, -1.816037693736268333, -1.423817124750816232 ) ) ;
#6793 = CARTESIAN_POINT ( 'NONE',  ( 5.554000203453580475, 6.508696987897830688, -1.199719254218452047 ) ) ;
#6794 = CARTESIAN_POINT ( 'NONE',  ( 0.2279051764371925748, -1.265926261136205211, -1.626655886597817124 ) ) ;
#6795 = CARTESIAN_POINT ( 'NONE',  ( 4.469384193999260901, 8.366031992974468423, -0.7998128361456231517 ) ) ;
#6796 = VECTOR ( 'NONE', #78584, 1000.000000000000000 ) ;
#6797 = CARTESIAN_POINT ( 'NONE',  ( 5.993622264137510314, 2.212772176713458716, 0.6212890515704305727 ) ) ;
#6798 = CARTESIAN_POINT ( 'NONE',  ( 0.07999999999999327094, -9.999999999999994671, 10.91970695577496286 ) ) ;
#6799 = CARTESIAN_POINT ( 'NONE',  ( -5.424143973919053785, 8.485862515284315677, 1.199719254218454489 ) ) ;
#6800 = CARTESIAN_POINT ( 'NONE',  ( 5.752782329262380756, -1.473788443143897675, 1.151991621687727507 ) ) ;
#6802 = CARTESIAN_POINT ( 'NONE',  ( -4.442231607132987925, 5.211633625523774960, -1.199719254218453823 ) ) ;
#6801 = CARTESIAN_POINT ( 'NONE',  ( 3.990413957267644474, -1.096855775730350757, 1.566394476586838724 ) ) ;
#6803 = CARTESIAN_POINT ( 'NONE',  ( 5.004599478379411437, -0.7411955310945415043, -2.078817424605138964 ) ) ;
#6804 = CARTESIAN_POINT ( 'NONE',  ( 4.698512310153400762, 1.457641359173178275, -1.535954635999142948 ) ) ;
#6805 = CARTESIAN_POINT ( 'NONE',  ( -1.225000000000038058, 1.041666667349488984, -0.7072540797573257931 ) ) ;
#6806 = CARTESIAN_POINT ( 'NONE',  ( 6.883263157960367806, 0.5819222519044697783, 1.998722019247618276 ) ) ;
#6807 = CARTESIAN_POINT ( 'NONE',  ( 4.367134876933267407, 8.109091433148536865, 0.000000000000000000 ) ) ;
#6808 = CARTESIAN_POINT ( 'NONE',  ( -5.031484404002922517, 6.963427452793760963, 1.443375672974058777 ) ) ;
#6809 = CARTESIAN_POINT ( 'NONE',  ( 5.444028431581452665, -1.345373016635186714, -1.639009079359869725 ) ) ;
#6810 = CARTESIAN_POINT ( 'NONE',  ( 2.222082089356589130, -2.238238103340572049, 0.5610464132631690637 ) ) ;
#6811 = CARTESIAN_POINT ( 'NONE',  ( 3.332423539472821439, -1.170687260143790320, 1.574129132985650825 ) ) ;
#6812 = CARTESIAN_POINT ( 'NONE',  ( -4.502189528189771472, 7.410248995266807803, -1.199719254218453823 ) ) ;
#6813 = CARTESIAN_POINT ( 'NONE',  ( 6.368047018367568590, -2.047660648193879496, 0.2468551644246498589 ) ) ;
#6814 = CARTESIAN_POINT ( 'NONE',  ( 3.633221978782282147, 5.261844946711204507, -1.443375672974057666 ) ) ;
#6815 = CARTESIAN_POINT ( 'NONE',  ( 3.691562964670865199, 7.528850235416478576, -0.7998128361456362523 ) ) ;
#6816 = ORIENTED_EDGE ( 'NONE', *, *, #25165, .T. ) ;
#6817 = CARTESIAN_POINT ( 'NONE',  ( 5.454314652423888354, -1.275559214091715354, 1.561879324423600668 ) ) ;
#6818 = CARTESIAN_POINT ( 'NONE',  ( -9.104463846776669200, 10.58062822844965645, -1.199719254218441611 ) ) ;
#6819 = CARTESIAN_POINT ( 'NONE',  ( -4.489270214782448143, 8.251570750202326110, -0.005118047378703463254 ) ) ;
#6820 = CARTESIAN_POINT ( 'NONE',  ( 2.969872605471521432, 6.598710015541000118, -0.2115686265727617921 ) ) ;
#6821 = CARTESIAN_POINT ( 'NONE',  ( 3.309609623814670165, -1.772202297075220256, -1.253863066769088874 ) ) ;
#6822 = CARTESIAN_POINT ( 'NONE',  ( 4.583538449871731757, 7.505156070562471804, 1.199719254218451159 ) ) ;
#6823 = CARTESIAN_POINT ( 'NONE',  ( 0.7387272492362946252, 1.258454933865692293, -1.706699550108881080 ) ) ;
#6824 = CARTESIAN_POINT ( 'NONE',  ( 1.499999999999989120, 1.785416667349487563, 0.8660254037844524744 ) ) ;
#6825 = CARTESIAN_POINT ( 'NONE',  ( -6.756024855156518072, 14.53008480311059714, -9.927621727203854718 ) ) ;
#6826 = DIRECTION ( 'NONE',  ( 0.000000000000000000, 8.546850786086437571E-32, 1.000000000000000000 ) ) ;
#6827 = CARTESIAN_POINT ( 'NONE',  ( 4.812217717264355876, 8.234349973070900219, 0.8868998539744571419 ) ) ;
#6828 = CARTESIAN_POINT ( 'NONE',  ( 0.5970370245043071789, 1.714778692204623312, -1.142632759096851913 ) ) ;
#6830 = DIRECTION ( 'NONE',  ( 0.000000000000000000, -1.000000000000000000, 0.000000000000000000 ) ) ;
#6829 = CARTESIAN_POINT ( 'NONE',  ( -8.292783513053063160, 12.82666453187061073, 0.7998128361456481317 ) ) ;
#6831 = CARTESIAN_POINT ( 'NONE',  ( -1.402160292154681736E-14, 0.9468750003414176941, -1.575800808251659024 ) ) ;
#6832 = CARTESIAN_POINT ( 'NONE',  ( -1.001543065824772872E-14, 5.462500000000020783, 1.732050807568877637 ) ) ;
#6833 = ORIENTED_EDGE ( 'NONE', *, *, #31446, .T. ) ;
#6834 = CARTESIAN_POINT ( 'NONE',  ( 3.369685512061989741, 0.4621021693036463374, -1.855490417808261183 ) ) ;
#6835 =( BOUNDED_CURVE ( )  B_SPLINE_CURVE ( 2, ( #201795, #198600, #383, #35039, #18785, #136837, #2523, #19858, #68599 ),
 .UNSPECIFIED., .F., .T. ) 
 B_SPLINE_CURVE_WITH_KNOTS ( ( 3, 2, 2, 2, 3 ),
 ( 0.4843749999999998335, 0.4895833333333333148, 0.5000000000000000000, 0.5104166666666666297, 0.5156250000000002220 ),
 .UNSPECIFIED. ) 
 CURVE ( )  GEOMETRIC_REPRESENTATION_ITEM ( )  RATIONAL_B_SPLINE_CURVE ( ( 0.9330127018922194093, 0.9330127018922171889, 1.000000000000000000, 0.8660254037844387076, 1.000000000000000000, 0.8660254037844387076, 1.000000000000000000, 0.9330127018922165227, 0.9330127018922194093 ) ) 
 REPRESENTATION_ITEM ( '' )  );
#6836 = CARTESIAN_POINT ( 'NONE',  ( 5.664868940362820737, -1.601528614980719967, -0.7536287887903775351 ) ) ;
#6837 = CARTESIAN_POINT ( 'NONE',  ( 6.038177310039780643, 8.137902509836795417, -1.599625672291283607 ) ) ;
#6838 = CARTESIAN_POINT ( 'NONE',  ( -3.958090780185743451, 6.705190779270287393, -1.199719254218452047 ) ) ;
#6839 = CARTESIAN_POINT ( 'NONE',  ( 0.6678513782990652681, 1.809512280066556400, -0.08962025572057349954 ) ) ;
#6841 = CARTESIAN_POINT ( 'NONE',  ( 1.059628844421168559, 1.143981278108822108, 1.536452684808758962 ) ) ;
#6840 = LINE ( 'NONE', #71840, #63138 ) ;
#6842 = CARTESIAN_POINT ( 'NONE',  ( 1.820844063133007396, -1.465591517063179028, 1.462601037713284535 ) ) ;
#6843 = CARTESIAN_POINT ( 'NONE',  ( 1.364683531249986537, -0.03229166632525094088, -0.7879004041258309554 ) ) ;
#6844 = CARTESIAN_POINT ( 'NONE',  ( 6.086763352761943580, -0.2763008855245497331, -1.850001521387992565 ) ) ;
#6845 = CARTESIAN_POINT ( 'NONE',  ( 2.789462663364688844, 1.291185895303394116, 1.290987730777813702 ) ) ;
#6847 = CARTESIAN_POINT ( 'NONE',  ( 5.448178351099921102, 7.506598249424609293, 1.250114376932524252 ) ) ;
#6846 = CARTESIAN_POINT ( 'NONE',  ( 5.197975494389605267, -0.7968864405506062010, 2.058166701804148957 ) ) ;
#6848 = CARTESIAN_POINT ( 'NONE',  ( 1.364683531249986537, 0.1552083336747499542, -0.7879004041258309554 ) ) ;
#6849 = CARTESIAN_POINT ( 'NONE',  ( 4.211423687607918076, -1.713229066603161099, -1.148409633951211761 ) ) ;
#6850 = CARTESIAN_POINT ( 'NONE',  ( -7.823218330285243383, 9.085841792542966644, -1.199719254218446718 ) ) ;
#6851 = CARTESIAN_POINT ( 'NONE',  ( 9.565441069641300587, 11.11843498845840905, -1.199719254218440723 ) ) ;
#6852 = CARTESIAN_POINT ( 'NONE',  ( 8.832353407160718817, 3.956598013261175772, 7.432338980325266853 ) ) ;
#6853 = CARTESIAN_POINT ( 'NONE',  ( 0.8433209000573947955, -1.854398715148808385, 1.110445933987347367 ) ) ;
#6854 = CARTESIAN_POINT ( 'NONE',  ( 6.496543107701719499, 2.047251205643263017, 0.3077783505985449142 ) ) ;
#6855 = CARTESIAN_POINT ( 'NONE',  ( 1.364683531249988757, 1.696875000341414808, 0.000000000000000000 ) ) ;
#6856 = CARTESIAN_POINT ( 'NONE',  ( 3.778741785029844369, -2.082091666206013159, -0.5805316298483630399 ) ) ;
#6858 = CARTESIAN_POINT ( 'NONE',  ( 2.435929278166943490, 1.204617592564939166, 1.548422000036096202 ) ) ;
#6857 = CARTESIAN_POINT ( 'NONE',  ( 3.721357204503534355, 1.733397938510993885, 1.036269837853747378 ) ) ;
#6859 = CARTESIAN_POINT ( 'NONE',  ( 6.620655732516620873, 2.403464043289889496, 2.653833411862613012 ) ) ;
#6860 = ORIENTED_EDGE ( 'NONE', *, *, #95154, .F. ) ;
#6863 = CARTESIAN_POINT ( 'NONE',  ( 7.321039761699430493, 7.643560598178549270, -0.7216878364870257245 ) ) ;
#6862 = CARTESIAN_POINT ( 'NONE',  ( 1.642778471875001811, -2.792708332855376785, 2.845375778867859751 ) ) ;
#6861 = FACE_OUTER_BOUND ( 'NONE', #192849, .T. ) ;
#6864 = CARTESIAN_POINT ( 'NONE',  ( -5.769876891067536206, 8.889217585290882795, 1.199719254218454489 ) ) ;
#6865 = CARTESIAN_POINT ( 'NONE',  ( 2.026577684455236561, 0.4465047249504557891, 1.966304233017155845 ) ) ;
#6867 = CARTESIAN_POINT ( 'NONE',  ( -4.213005119291713285, 7.494488749433884323, -0.9457084323257232139 ) ) ;
#6866 = CARTESIAN_POINT ( 'NONE',  ( -3.578462479003122976, 6.262291094557191684, 1.199719254218464037 ) ) ;
#6868 = CARTESIAN_POINT ( 'NONE',  ( -1.201851678989727383E-14, 5.618750000682818602, -1.732050807568863648 ) ) ;
#6869 = CARTESIAN_POINT ( 'NONE',  ( 5.976807594091998688, -1.347613670528555740, 1.357171208065083512 ) ) ;
#6870 = CARTESIAN_POINT ( 'NONE',  ( -11.97929049433705373, 12.22000000000000064, 0.7046979865771804130 ) ) ;
#6871 = ADVANCED_FACE ( 'NONE', ( #110582 ), #56223, .T. ) ;
#6872 = CARTESIAN_POINT ( 'NONE',  ( 6.616015773344440021, 6.821032611764393572, 1.040834085586084257E-14 ) ) ;
#6874 = CARTESIAN_POINT ( 'NONE',  ( 4.394157760337158436, -0.8647400765994193161, -1.821735888681835558 ) ) ;
#6873 = CARTESIAN_POINT ( 'NONE',  ( -7.158341917891067219, 11.29522330427417565, 0.000000000000000000 ) ) ;
#6875 = CARTESIAN_POINT ( 'NONE',  ( -1.499999999999997780, 3.900000000000021672, 1.214306433183764966E-14 ) ) ;
#6876 = CARTESIAN_POINT ( 'NONE',  ( -1.364683531250010295, 15.19270833367472839, 0.7879004041258445001 ) ) ;
#6877 = CARTESIAN_POINT ( 'NONE',  ( 6.704117942027653321, -1.724248281341285827, 0.04880198193529976941 ) ) ;
#6878 = CARTESIAN_POINT ( 'NONE',  ( 5.254667053748194760, 8.288139441751686931, 1.199719254218452047 ) ) ;
#6879 = CARTESIAN_POINT ( 'NONE',  ( 7.917598520700710019, 12.18102267421877727, -0.7216878364870328300 ) ) ;
#6880 = FACE_OUTER_BOUND ( 'NONE', #198232, .T. ) ;
#6881 = CARTESIAN_POINT ( 'NONE',  ( 4.745289220334846902, -1.444806058459674691, -1.188008360142885245 ) ) ;
#6882 = CARTESIAN_POINT ( 'NONE',  ( -0.02880301295727832195, -0.006976478922920550246, -2.273770288744045409 ) ) ;
#6883 = CARTESIAN_POINT ( 'NONE',  ( 2.325130699016836555, -1.891071737562113997, -0.8429460452448678254 ) ) ;
#6884 = CARTESIAN_POINT ( 'NONE',  ( 1.499999999999993117, 12.38541666734946212, 0.8660254037844408170 ) ) ;
#6885 = ORIENTED_EDGE ( 'NONE', *, *, #205195, .F. ) ;
#6886 = CARTESIAN_POINT ( 'NONE',  ( 4.577813143269636065, 5.369812084349879555, -1.199719254218450271 ) ) ;
#6887 = CARTESIAN_POINT ( 'NONE',  ( 0.8082205221912192039, 1.198841770460257194, -1.621197638953228548 ) ) ;
#6888 = CARTESIAN_POINT ( 'NONE',  ( 0.1053163366912619470, 1.342294115999270510, 1.216805694454982767 ) ) ;
#6889 = CARTESIAN_POINT ( 'NONE',  ( 5.682275777458854371, 5.801945626556378244, 0.7216878364870328300 ) ) ;
#6890 = CARTESIAN_POINT ( 'NONE',  ( 0.000000000000000000, 7.849261790823902629, 8.049999999999993605 ) ) ;
#6891 = CARTESIAN_POINT ( 'NONE',  ( 6.927853306458731986, 11.02631992426980112, 0.7216878364870438212 ) ) ;
#6892 = AXIS2_PLACEMENT_3D ( 'NONE', #36732, #22605, #119127 ) ;
#6893 = CARTESIAN_POINT ( 'NONE',  ( 8.158255747121103241, 10.54105100977322174, 1.599625672291281386 ) ) ;
#6895 = CARTESIAN_POINT ( 'NONE',  ( 5.712480180419416520, 1.847460191615752700, 0.5061846876120765781 ) ) ;
#6894 = CARTESIAN_POINT ( 'NONE',  ( -5.555090253297260361, 7.504024600312024340, 1.599625672291269396 ) ) ;
#6896 = CARTESIAN_POINT ( 'NONE',  ( 6.727182134110194944, 0.008744176509076190262, 1.710970312420515338 ) ) ;
#6897 = DIRECTION ( 'NONE',  ( 0.000000000000000000, -1.000000000000000000, 0.000000000000000000 ) ) ;
#6898 = EDGE_CURVE ( 'NONE', #90583, #191645, #156657, .T. ) ;
#6899 = DIRECTION ( 'NONE',  ( 0.6507913734559640506, -0.7592566023653003482, 0.000000000000000000 ) ) ;
#6901 = VERTEX_POINT ( 'NONE', #90103 ) ;
#6900 = CARTESIAN_POINT ( 'NONE',  ( 4.365362273920244007, 6.116008624372160973, 1.443375672974062551 ) ) ;
#6902 = CARTESIAN_POINT ( 'NONE',  ( -8.514157279702036618, 9.035531035848267223, -0.7216878364870278340 ) ) ;
#6903 = CARTESIAN_POINT ( 'NONE',  ( 3.186554565756247737, -2.129457467500107004, -0.3711038070777840647 ) ) ;
#6904 = CARTESIAN_POINT ( 'NONE',  ( -5.451787166470911217, 9.374519104275787384, 0.7216878364870267237 ) ) ;
#6905 = CARTESIAN_POINT ( 'NONE',  ( 7.377044979611483200, 7.779176362401098999, -0.7216878364870317197 ) ) ;
#6906 = CARTESIAN_POINT ( 'NONE',  ( 0.9848172835694012361, -1.340914915981223476, 1.642866500755429948 ) ) ;
#6907 = CARTESIAN_POINT ( 'NONE',  ( 6.000976577881287355, 1.490888274384492895, -1.053294804101670090 ) ) ;
#6908 = CARTESIAN_POINT ( 'NONE',  ( 2.495336804025758859, 1.521579944813663099, 1.253379492226768477 ) ) ;
#6909 = CARTESIAN_POINT ( 'NONE',  ( 4.781465250580236415, 0.1816826923375300662, -1.903719681147630016 ) ) ;
#6910 = EDGE_LOOP ( 'NONE', ( #121706, #135092, #177174, #22707 ) ) ;
#6911 = DIRECTION ( 'NONE',  ( 1.000000000000000000, 0.000000000000000000, 0.000000000000000000 ) ) ;
#6912 = CARTESIAN_POINT ( 'NONE',  ( 5.406690398188211510, 0.5700869393594419909, 1.885254869494409791 ) ) ;
#6913 = CARTESIAN_POINT ( 'NONE',  ( 0.05839466612742905127, -1.734069842965625385, -0.8743347890363247776 ) ) ;
#6914 = ORIENTED_EDGE ( 'NONE', *, *, #191961, .F. ) ;
#6915 = CARTESIAN_POINT ( 'NONE',  ( -5.472651281771599763, 6.413789912602166687, 1.199719254218452935 ) ) ;
#6917 = CARTESIAN_POINT ( 'NONE',  ( -0.3769810270648435990, 3.049942316455334090, 0.4288785890452350702 ) ) ;
#6916 = CARTESIAN_POINT ( 'NONE',  ( -3.797165540279144214, 6.587721009371067638, 1.199719254218452935 ) ) ;
#6918 = CARTESIAN_POINT ( 'NONE',  ( 6.672020991256494504, 6.956648375986938859, 0.000000000000000000 ) ) ;
#6920 = ORIENTED_EDGE ( 'NONE', *, *, #131120, .T. ) ;
#6919 = CARTESIAN_POINT ( 'NONE',  ( 4.670513044250029999, 0.7352163052343118066, 1.765496816765201427 ) ) ;
#6921 = CARTESIAN_POINT ( 'NONE',  ( 0.9915960798324228165, 1.945464911009102460, -1.041603813667857370 ) ) ;
#6922 = CARTESIAN_POINT ( 'NONE',  ( 9.651614352920288908, 4.121347559867349020, -7.130841425383052545 ) ) ;
#6923 = CARTESIAN_POINT ( 'NONE',  ( -0.09332341176954485340, -0.4182270256129701491, -1.872751671355552983 ) ) ;
#6924 = CARTESIAN_POINT ( 'NONE',  ( -0.02319159430947542386, 0.2540490248266329965, -1.846305437520213477 ) ) ;
#6926 = CARTESIAN_POINT ( 'NONE',  ( 5.542203953035277131, 0.8216685229280199509, 1.841735684200429990 ) ) ;
#6925 = DIRECTION ( 'NONE',  ( 0.000000000000000000, 1.000000000000000000, 0.000000000000000000 ) ) ;
#6927 = CARTESIAN_POINT ( 'NONE',  ( 6.727182134110222478, 0.005875948494733079785, 1.810970247402940547 ) ) ;
#6928 = CARTESIAN_POINT ( 'NONE',  ( 2.225130849662221966, -1.891980959128433559, -0.8411517639917851508 ) ) ;
#6929 = CARTESIAN_POINT ( 'NONE',  ( -5.982172092127739482, 8.002286745614243912, -1.599625672291263179 ) ) ;
#6930 = CARTESIAN_POINT ( 'NONE',  ( -4.604539980425653489, 8.383423159197839425, -0.07723066608773809794 ) ) ;
#6931 = CARTESIAN_POINT ( 'NONE',  ( 1.094844843509492183, -0.5259716649698794599, -2.096624219460433647 ) ) ;
#6932 = CARTESIAN_POINT ( 'NONE',  ( -11.94041551183581262, 8.961066757473448163, 1.233743901448089764 ) ) ;
#6933 = CARTESIAN_POINT ( 'NONE',  ( 6.061904079085887354, 6.244845311787889486, 0.000000000000000000 ) ) ;
#6934 = CARTESIAN_POINT ( 'NONE',  ( -4.786163832636268545, 5.147994549525747310, 0.9918565312223650565 ) ) ;
#6935 = VECTOR ( 'NONE', #48280, 1000.000000000000000 ) ;
#6936 = CARTESIAN_POINT ( 'NONE',  ( -0.6823417656250003738, 13.21354166700806942, 1.181850606188754593 ) ) ;
#6938 = CARTESIAN_POINT ( 'NONE',  ( -7.117104292530948229, 7.267986194233038155, -0.7998128361456362523 ) ) ;
#6937 = CARTESIAN_POINT ( 'NONE',  ( 6.925078400183523719, 3.697131557392329348, 2.469975972695995559 ) ) ;
#6939 = CARTESIAN_POINT ( 'NONE',  ( 5.256420022722958052, 1.669015333217665820, -0.4704954288548191532 ) ) ;
#6940 = CARTESIAN_POINT ( 'NONE',  ( -5.115504031057831469, 4.862509545855891346, 0.7998128361456341429 ) ) ;
#6941 = CARTESIAN_POINT ( 'NONE',  ( 2.641538584800803502, 1.894577224340647792, -0.8349662684224223863 ) ) ;
#6942 = CARTESIAN_POINT ( 'NONE',  ( 3.831750911750389399, 0.7112487137725398423, -1.994330698664834589 ) ) ;
#6943 = CARTESIAN_POINT ( 'NONE',  ( 7.263417608619159083, 9.497073181520933716, -1.599625672291262513 ) ) ;
#6944 = CARTESIAN_POINT ( 'NONE',  ( 0.08641082498351806973, -9.914243671626374876, 10.99966068378002326 ) ) ;
#6945 = CARTESIAN_POINT ( 'NONE',  ( 1.850388327615314799, -1.959487253598888312, -0.1980615517182797158 ) ) ;
#6946 = CARTESIAN_POINT ( 'NONE',  ( 6.055847235078346991, 6.052673195394750572, 0.4411178842869938888 ) ) ;
#6947 = FACE_OUTER_BOUND ( 'NONE', #134636, .T. ) ;
#6948 = CARTESIAN_POINT ( 'NONE',  ( 3.170184779232795957, -1.365206436085873776, 1.841245074435297502 ) ) ;
#6949 = CARTESIAN_POINT ( 'NONE',  ( 1.576486190600217663, -1.733098801405801304, -0.5742540608338757568 ) ) ;
#6950 = CARTESIAN_POINT ( 'NONE',  ( 3.881377115262159894, 7.750300077773022878, 0.7998128361456271485 ) ) ;
#6951 = CARTESIAN_POINT ( 'NONE',  ( 5.965224399888476192, 6.061776009399090448, 1.040834085586084257E-14 ) ) ;
#6952 = CARTESIAN_POINT ( 'NONE',  ( -7.857113714319432063, 9.125386407249497012, 1.199719254218462483 ) ) ;
#6953 = CARTESIAN_POINT ( 'NONE',  ( 3.287361135653954491, 0.04523670859641867187, -2.012844072734306433 ) ) ;
#6954 = CARTESIAN_POINT ( 'NONE',  ( 3.660947809037872425, 1.549288415169544963, -1.203348422379519667 ) ) ;
#6955 = CARTESIAN_POINT ( 'NONE',  ( -9.006694118179950692, 9.402231314165087284, 1.040834085586084257E-14 ) ) ;
#6956 = CARTESIAN_POINT ( 'NONE',  ( -6.911959384868566758, 6.958374125301778790, 1.040834085586084257E-14 ) ) ;
#6957 = DIRECTION ( 'NONE',  ( 0.000000000000000000, 0.000000000000000000, 1.000000000000000000 ) ) ;
#6959 = CARTESIAN_POINT ( 'NONE',  ( 4.891328792415849058, 1.312644105602623457, 1.187316208720709421 ) ) ;
#6958 = CARTESIAN_POINT ( 'NONE',  ( 6.369093512601681439, 2.000948562089053695, -0.6057377149290378293 ) ) ;
#6960 = CARTESIAN_POINT ( 'NONE',  ( 1.499999999999995115, 3.327083334016150307, -0.8660254037844217212 ) ) ;
#6961 = CARTESIAN_POINT ( 'NONE',  ( 1.043234067691005684, -1.729537258485489115, -1.345685951901639532 ) ) ;
#6962 = CARTESIAN_POINT ( 'NONE',  ( 5.226372699876832506, 0.1332071266631333351, 1.735289576922446786 ) ) ;
#6963 = CARTESIAN_POINT ( 'NONE',  ( 8.751951852821344247, 10.16936423550178503, -1.199719254218446718 ) ) ;
#6964 = CARTESIAN_POINT ( 'NONE',  ( -2.163990585822766377, 5.468480083527750502, -0.4581612399152222848 ) ) ;
#6965 = CARTESIAN_POINT ( 'NONE',  ( 5.924520554715382303, -1.662438412150448963, -1.587772413480701639 ) ) ;
#6966 = CARTESIAN_POINT ( 'NONE',  ( -0.05867695357848409787, -1.698172713885632401, -1.384993232510664640 ) ) ;
#6967 = CARTESIAN_POINT ( 'NONE',  ( 5.571581879130038217, 1.311117947217877555, -1.134664832369073117 ) ) ;
#6968 = CARTESIAN_POINT ( 'NONE',  ( 1.629795212970772456, -2.077151576879713080, 0.7458654493318407352 ) ) ;
#6969 = CARTESIAN_POINT ( 'NONE',  ( 5.301315566676442437, -1.864821911710778490, 1.111730659606048111 ) ) ;
#6970 = DIRECTION ( 'NONE',  ( 0.7592566023652994600, 0.6507913734559651608, 0.000000000000000000 ) ) ;
#6971 = CARTESIAN_POINT ( 'NONE',  ( 1.464221803445309167, -1.127774752583620366, 1.791820951956924812 ) ) ;
#6972 = CARTESIAN_POINT ( 'NONE',  ( 4.218750000000001776, -0.7852924748297752666, 1.895863743164170057 ) ) ;
#6973 = CARTESIAN_POINT ( 'NONE',  ( -0.3461162505576212411, 7.159215625956849571, -1.970439023737479811 ) ) ;
#6974 = CARTESIAN_POINT ( 'NONE',  ( 4.577124784165859772, 0.0005310917307651402686, -1.926566264685470875 ) ) ;
#6975 = CARTESIAN_POINT ( 'NONE',  ( 0.9268046190927975436, -1.003647134691580289, -1.981720526202688015 ) ) ;
#6976 = VERTEX_POINT ( 'NONE', #122685 ) ;
#6977 = CARTESIAN_POINT ( 'NONE',  ( 0.7499999999999920064, 4.483333333333352932, 1.299038105676669330 ) ) ;
#6978 = CARTESIAN_POINT ( 'NONE',  ( 5.066996723205273057, 6.934582148538044777, 1.599625672291267398 ) ) ;
#6979 = CARTESIAN_POINT ( 'NONE',  ( 6.765682348419287173, 7.852049813699357728, 1.199719254218462483 ) ) ;
#6980 = CARTESIAN_POINT ( 'NONE',  ( 4.213700991847090016, 1.784230803775087137, 1.322971166850190450 ) ) ;
#6981 = CARTESIAN_POINT ( 'NONE',  ( -9.192064960385334160, 9.826423329978791088, 0.7216878364870438212 ) ) ;
#6983 = EDGE_CURVE ( 'NONE', #154266, #99737, #40279, .T. ) ;
#6982 = CARTESIAN_POINT ( 'NONE',  ( -0.9174905902287084913, -4.140925090156245325, 0.4108596822575558694 ) ) ;
#6984 = CARTESIAN_POINT ( 'NONE',  ( 6.399085315970131305, 8.488685506763726352, -1.443375672974057666 ) ) ;
#6985 = CARTESIAN_POINT ( 'NONE',  ( -9.015808962963337336, 10.58116054728778366, 1.082531754730558626 ) ) ;
#6986 = CARTESIAN_POINT ( 'NONE',  ( 5.383996398402570271, 9.295429874862735531, 0.000000000000000000 ) ) ;
#6987 = CARTESIAN_POINT ( 'NONE',  ( 2.268204128460939550, 1.842446992372799963, -0.8197738674571022344 ) ) ;
#6989 = CARTESIAN_POINT ( 'NONE',  ( 6.144999177589818729, -0.2990398410713848154, -2.040763669801145319 ) ) ;
#6988 = CARTESIAN_POINT ( 'NONE',  ( 7.751511138711133064, 10.06651563329490529, -1.599625672291262513 ) ) ;
#6990 = CARTESIAN_POINT ( 'NONE',  ( -10.99622371251743225, -6.863149499369328055, 0.2970643657731258935 ) ) ;
#6991 = CARTESIAN_POINT ( 'NONE',  ( 6.604230223188150894, 9.758666789477915771, -1.082531754730548412 ) ) ;
#6992 = CARTESIAN_POINT ( 'NONE',  ( 6.409682876116948869, -0.8291888958818021127, -1.530247525868874581 ) ) ;
#6993 = FILL_AREA_STYLE_COLOUR ( '', #40467 ) ;
#6994 = CARTESIAN_POINT ( 'NONE',  ( 1.364683531249986537, 1.905208333674750287, -0.7879004041258239610 ) ) ;
#6995 = CARTESIAN_POINT ( 'NONE',  ( 1.809446860903692444, -1.757098282301880365, 0.2103932681993408993 ) ) ;
#6996 = CARTESIAN_POINT ( 'NONE',  ( 0.6510177983308338412, 0.9963039324867200008, 1.753029211773032392 ) ) ;
#6997 = CARTESIAN_POINT ( 'NONE',  ( 0.3625324912872701089, 0.1813134127766780901, -1.832273687604975665 ) ) ;
#6998 = CARTESIAN_POINT ( 'NONE',  ( 4.581715332782612116, -1.081557967857611935, 2.021163373060499424 ) ) ;
#6999 = CARTESIAN_POINT ( 'NONE',  ( 3.169683937527142170, -1.096016708463069422, 1.479218548343118389 ) ) ;
#7000 = EDGE_CURVE ( 'NONE', #24990, #89074, #8831, .T. ) ;
#7001 = CARTESIAN_POINT ( 'NONE',  ( 8.992082194361556091, 11.51384853155376220, 1.599625672291279388 ) ) ;
#7002 = CARTESIAN_POINT ( 'NONE',  ( 8.983336459935364005, 13.98445560454119629, 7.957668677609153640 ) ) ;
#7003 = CARTESIAN_POINT ( 'NONE',  ( 3.539906422930443775, 0.8216601389946125433, -1.630302437610211541 ) ) ;
#7004 = CARTESIAN_POINT ( 'NONE',  ( 4.377577386359387646, -0.4445010797573499817, -1.966645064109616481 ) ) ;
#7005 = CARTESIAN_POINT ( 'NONE',  ( -8.859363311525973117, 12.42334206583395328, -1.199719254218446718 ) ) ;
#7007 = CARTESIAN_POINT ( 'NONE',  ( -11.52460864928265138, 12.21999999999999709, -3.346683403123526190 ) ) ;
#7006 = CARTESIAN_POINT ( 'NONE',  ( 3.397619368019880959, 1.782376118940771637, 1.393485768503288202 ) ) ;
#7008 = CARTESIAN_POINT ( 'NONE',  ( 5.754936497916005145, -1.662164095216655202, 1.293063917272518015 ) ) ;
#7009 = B_SPLINE_CURVE_WITH_KNOTS ( 'NONE', 3,
 ( #69454, #71586, #39117, #18583, #202653, #68388, #19651 ),
 .UNSPECIFIED., .F., .F.,
 ( 4, 3, 4 ),
 ( 3.172092245977020233E-15, 6.255038410197399793E-05, 0.0001580841567447031405 ),
 .UNSPECIFIED. ) ;
#7010 = CARTESIAN_POINT ( 'NONE',  ( 8.131154284199636706, 15.75938775753455801, 8.460579169278151568 ) ) ;
#7011 =( BOUNDED_CURVE ( )  B_SPLINE_CURVE ( 2, ( #43130, #109246, #92943, #158988, #208779, #60409, #126570, #192530, #44184 ),
 .UNSPECIFIED., .F., .T. ) 
 B_SPLINE_CURVE_WITH_KNOTS ( ( 3, 2, 2, 2, 3 ),
 ( 0.3125000000000000000, 0.3194444444444444198, 0.3333333333333333148, 0.3472222222222222099, 0.3541666666666666852 ),
 .UNSPECIFIED. ) 
 CURVE ( )  GEOMETRIC_REPRESENTATION_ITEM ( )  RATIONAL_B_SPLINE_CURVE ( ( 0.9330127018922194093, 0.9330127018922194093, 1.000000000000000000, 0.8660254037844387076, 1.000000000000000000, 0.8660254037844387076, 1.000000000000000000, 0.9330127018922190762, 0.9330127018922194093 ) ) 
 REPRESENTATION_ITEM ( '' )  );
#7012 = CARTESIAN_POINT ( 'NONE',  ( 3.508316276398337319, 2.070544812355082254, 0.002818362966339192730 ) ) ;
#7013 = CARTESIAN_POINT ( 'NONE',  ( 4.403700966340357681, 4.032072637018845107, -0.7998128361456211532 ) ) ;
#7014 = CARTESIAN_POINT ( 'NONE',  ( 1.360316468749973140, 0.5468750003413819227, -2.081668171172168513E-14 ) ) ;
#7015 = CARTESIAN_POINT ( 'NONE',  ( 6.252600707356171128, 2.097339953035493476, 0.3115551810550785672 ) ) ;
#7017 = CARTESIAN_POINT ( 'NONE',  ( 0.6625679566808447829, -1.396226752684716521, 1.327616383781888176 ) ) ;
#7016 = CARTESIAN_POINT ( 'NONE',  ( -9.179033691651859783, 10.66762638080401260, 1.199719254218462483 ) ) ;
#7018 = CARTESIAN_POINT ( 'NONE',  ( -5.517242166118370150, 5.401480380085008193, 0.7998128361456281477 ) ) ;
#7019 = CARTESIAN_POINT ( 'NONE',  ( 7.235247531187115833, 11.59287255302699648, -0.7998128361456291469 ) ) ;
#7020 = CARTESIAN_POINT ( 'NONE',  ( 6.333067150914820864, 6.561202228921677815, 0.7216878364870328300 ) ) ;
#7021 = CARTESIAN_POINT ( 'NONE',  ( 4.574835874639041400, 6.943354005153362429, 1.191215277921169324 ) ) ;
#7022 = CARTESIAN_POINT ( 'NONE',  ( 1.123270288250309834, 3.221052654332833054, -0.7749999999993620881 ) ) ;
#7023 = CARTESIAN_POINT ( 'NONE',  ( -5.427341564172148303, 5.226320001155936090, 0.000000000000000000 ) ) ;
#7024 = CARTESIAN_POINT ( 'NONE',  ( 0.5455723692351510667, 0.1713331888719657747, 2.214891930232844253 ) ) ;
#7025 = CARTESIAN_POINT ( 'NONE',  ( 2.397617287051221791, 1.627147360716905800, 1.336933552532795222 ) ) ;
#7026 = CARTESIAN_POINT ( 'NONE',  ( -4.842197138736131556, 5.678260079060780008, 1.199719254218452935 ) ) ;
#7027 = CARTESIAN_POINT ( 'NONE',  ( 8.101160479365381306, 9.410107633136481908, -1.199719254218446718 ) ) ;
#7028 = CARTESIAN_POINT ( 'NONE',  ( 6.227394082031683986, 0.1379007965640146050, -1.855924616290964169 ) ) ;
#7029 = CARTESIAN_POINT ( 'NONE',  ( 7.613066949273408213, 8.840665181362512115, -1.199719254218441611 ) ) ;
#7030 = CARTESIAN_POINT ( 'NONE',  ( -6.400857919427531684, 9.521399101757175742, 1.082531754730549967 ) ) ;
#7031 = CARTESIAN_POINT ( 'NONE',  ( -8.297226821883391779, 11.66355314463053006, 1.082531754730549967 ) ) ;
#7032 = CARTESIAN_POINT ( 'NONE',  ( 0.5453776912951785460, 0.1620316879334358084, 2.114494688702214020 ) ) ;
#7033 = CARTESIAN_POINT ( 'NONE',  ( -4.207966135563095733, 7.175396087857926375, 7.500000000000000000 ) ) ;
#7035 = CARTESIAN_POINT ( 'NONE',  ( 2.998438581075290710, 1.946722116546204306, 0.2428724957088539971 ) ) ;
#7034 = CARTESIAN_POINT ( 'NONE',  ( 1.224999999999971001, -0.6458333333332910708, 0.7072540797572737237 ) ) ;
#7036 = CARTESIAN_POINT ( 'NONE',  ( 2.061604318190731533, 0.3698614785779800185, -2.129673623264888960 ) ) ;
#7037 = CARTESIAN_POINT ( 'NONE',  ( 1.030510548812729965, -1.664561007783531332, 0.7873658874757857307 ) ) ;
#7039 = CARTESIAN_POINT ( 'NONE',  ( -4.595871994550918771, 6.958256438637705266, -1.193191807407071536 ) ) ;
#7038 = CARTESIAN_POINT ( 'NONE',  ( -5.635349125135588721, 6.603604063193491136, 1.199719254218452935 ) ) ;
#7040 = EDGE_CURVE ( 'NONE', #45871, #120076, #40428, .T. ) ;
#7041 = CARTESIAN_POINT ( 'NONE',  ( 3.503586914695429488, -0.7067764301678289840, -1.590537823618918711 ) ) ;
#7042 = CARTESIAN_POINT ( 'NONE',  ( 6.561783159334121152, 8.678499657355050800, -1.443375672974057666 ) ) ;
#7043 = CARTESIAN_POINT ( 'NONE',  ( -11.88731729969462059, 7.000411858491159656, -4.404230128874679906 ) ) ;
#7044 = CARTESIAN_POINT ( 'NONE',  ( 9.908311333488716954, 10.45411806535867782, 0.7998128361456462443 ) ) ;
#7045 = CARTESIAN_POINT ( 'NONE',  ( 0.3390366800232989530, 0.3710982241871863541, 2.129449491308422537 ) ) ;
#7046 = CARTESIAN_POINT ( 'NONE',  ( 2.706407486732204770, -1.492025830231600070, -1.356093404896424826 ) ) ;
#7047 = CARTESIAN_POINT ( 'NONE',  ( -0.08097581798161300470, -9.904508987438854106, -10.99970197202148547 ) ) ;
#7048 = CARTESIAN_POINT ( 'NONE',  ( -2.823841133396259639, 6.516508098929413961, -0.7998128361456481317 ) ) ;
#7049 = CARTESIAN_POINT ( 'NONE',  ( 2.360178788647437464, 0.8414710005770206225, 1.782988266942896693 ) ) ;
#7050 = EDGE_CURVE ( 'NONE', #35130, #78193, #53410, .T. ) ;
#7051 = CARTESIAN_POINT ( 'NONE',  ( 2.989799202408753853, 6.433716316886197717, 0.3763814980636948637 ) ) ;
#7052 = B_SPLINE_CURVE_WITH_KNOTS ( 'NONE', 3,
 ( #178064, #207349, #175937, #27532, #61104, #58969, #107790, #173815, #193234, #128337 ),
 .UNSPECIFIED., .F., .F.,
 ( 4, 1, 1, 1, 1, 1, 1, 4 ),
 ( 0.000000000000000000, 0.09123828766142533242, 0.1830323254715014447, 0.2554767746403809325, 0.3605042187413262100, 0.5206858269973231312, 0.7335850107976985557, 1.000000000000000000 ),
 .UNSPECIFIED. ) ;
#7055 = VERTEX_POINT ( 'NONE', #178820 ) ;
#7054 = CARTESIAN_POINT ( 'NONE',  ( -3.512971199716682591, 7.112567143062499930, 0.000000000000000000 ) ) ;
#7053 =( NAMED_UNIT ( * ) SI_UNIT ( $, .STERADIAN. ) SOLID_ANGLE_UNIT ( ) );
#7056 = CARTESIAN_POINT ( 'NONE',  ( -6.604230223188181093, 6.877559146573883453, 0.7216878364870317197 ) ) ;
#7057 = CARTESIAN_POINT ( 'NONE',  ( 6.412080304620304538, 6.445458208337293549, -0.7998128361456481317 ) ) ;
#7058 = CARTESIAN_POINT ( 'NONE',  ( -4.444040490229335560, 8.406740681901359480, 0.7998128361456352531 ) ) ;
#7059 = CARTESIAN_POINT ( 'NONE',  ( -7.469616286486262524, 7.679250187180907794, 0.7998128361456341429 ) ) ;
#7060 = CARTESIAN_POINT ( 'NONE',  ( 11.41381675112453387, 10.90000000000000036, -3.704697986577182522 ) ) ;
#7061 = CARTESIAN_POINT ( 'NONE',  ( 5.403480793235289070, 1.882684667239397758, 1.334102933689439663 ) ) ;
#7062 = CARTESIAN_POINT ( 'NONE',  ( 6.877413162628407406, -0.1429737755889188000, 1.930079329684093237 ) ) ;
#7063 = CARTESIAN_POINT ( 'NONE',  ( 3.590630163336411051, 1.912927474663427496, 0.4342120235502828773 ) ) ;
#7064 = CARTESIAN_POINT ( 'NONE',  ( 6.584456157731144899, 10.83361595066169514, -0.7998128361456291469 ) ) ;
#7065 = CARTESIAN_POINT ( 'NONE',  ( 0.1939827082095748889, 1.755770691208278889, 0.9913967135185000057 ) ) ;
#7066 = VERTEX_POINT ( 'NONE', #97574 ) ;
#7067 = CARTESIAN_POINT ( 'NONE',  ( 1.938805156862877022, -1.633297379596149845, 1.347353381010838458 ) ) ;
#7068 = CARTESIAN_POINT ( 'NONE',  ( 0.7499999999999885647, 1.597916667349486008, -1.299038105676652899 ) ) ;
#7070 = CARTESIAN_POINT ( 'NONE',  ( -5.343885102080728977, 9.386283052402845328, 0.7998128361456481317 ) ) ;
#7069 =( LENGTH_UNIT ( ) NAMED_UNIT ( * ) SI_UNIT ( .MILLI., .METRE. ) );
#7071 = CARTESIAN_POINT ( 'NONE',  ( 3.556447125109524876, -1.624355972047783148, -0.8667379164201680641 ) ) ;
#7072 = ORIENTED_EDGE ( 'NONE', *, *, #63358, .T. ) ;
#7073 = CARTESIAN_POINT ( 'NONE',  ( -10.64723070543352712, 11.31619066596094392, 0.7998128361456462443 ) ) ;
#7074 = CARTESIAN_POINT ( 'NONE',  ( -1.420000000000079865, 7.176846818246208848, 4.202462424328226476 ) ) ;
#7075 = CARTESIAN_POINT ( 'NONE',  ( 4.008146050417991546, -0.8085630067716749192, 1.960596031080278356 ) ) ;
#7076 = CARTESIAN_POINT ( 'NONE',  ( 0.4800843290509413386, -0.2225996465644273503, -1.827572303103291551 ) ) ;
#7077 = CARTESIAN_POINT ( 'NONE',  ( -1.999999999999988010, 2.428614679364265457E-14, 0.5999999999999969802 ) ) ;
#7078 = CARTESIAN_POINT ( 'NONE',  ( 8.423693512792301163, 8.722063941212843119, 0.7998128361456481317 ) ) ;
#7079 = CARTESIAN_POINT ( 'NONE',  ( 5.840530312436913007, 10.03597880781023299, 0.000000000000000000 ) ) ;
#7080 = CARTESIAN_POINT ( 'NONE',  ( 4.780574613336814771, -1.997868641178605298, -0.5047315492533087644 ) ) ;
#7081 =( GEOMETRIC_REPRESENTATION_CONTEXT ( 3 ) GLOBAL_UNCERTAINTY_ASSIGNED_CONTEXT ( ( #11863 ) ) GLOBAL_UNIT_ASSIGNED_CONTEXT ( ( #8814, #105274, #4511 ) ) REPRESENTATION_CONTEXT ( 'NONE', 'WORKASPACE' ) );
#7083 = CARTESIAN_POINT ( 'NONE',  ( 1.030510548812729965, -1.664561007783531332, 0.7873658874757857307 ) ) ;
#7082 = CARTESIAN_POINT ( 'NONE',  ( -8.199983978166823562, 8.461069484149769337, -0.7998128361456291469 ) ) ;
#7084 = CARTESIAN_POINT ( 'NONE',  ( -0.6823417656250212460, 4.051041667008085767, 1.181850606188767472 ) ) ;
#7085 = DIRECTION ( 'NONE',  ( 0.000000000000000000, 0.000000000000000000, -1.000000000000000000 ) ) ;
#7086 = CARTESIAN_POINT ( 'NONE',  ( -9.499623061593995388, -9.908700546396014275, 0.08463495275094737313 ) ) ;
#7087 = CARTESIAN_POINT ( 'NONE',  ( 10.99039737178640230, -7.697079954928647716, -0.4645147939556434347 ) ) ;
#7088 = CARTESIAN_POINT ( 'NONE',  ( 0.6806489137391663613, -1.222764829241920648, 1.836970590647703627 ) ) ;
#7089 = CARTESIAN_POINT ( 'NONE',  ( 3.356942810317259163, -1.715728140842260441, 1.474839417774987060 ) ) ;
#7090 = CARTESIAN_POINT ( 'NONE',  ( -7.022760382198764084, 11.13704484596649635, 0.7216878364870458196 ) ) ;
#7091 = CARTESIAN_POINT ( 'NONE',  ( 3.726654843667742689, 1.277109331127034952, -1.285116454894990268 ) ) ;
#7092 = CARTESIAN_POINT ( 'NONE',  ( 4.434732071067119641, -1.534896228733380052, 1.146084025706934684 ) ) ;
#7093 = CARTESIAN_POINT ( 'NONE',  ( 4.879381568908511824, -0.1049739508458477355, 2.067839077007492143 ) ) ;
#7094 = CARTESIAN_POINT ( 'NONE',  ( -0.6823417656249969321, 4.780208333674755394, -1.181850606188749264 ) ) ;
#7095 = AXIS2_PLACEMENT_3D ( 'NONE', #116290, #164979, #97873 ) ;
#7096 = CARTESIAN_POINT ( 'NONE',  ( 2.641432621735483544, -1.459803026827242611, -1.325177341282377741 ) ) ;
#7097 = CARTESIAN_POINT ( 'NONE',  ( 0.8153024884889724655, -0.2858729149923607826, 1.904955193227176879 ) ) ;
#7098 = CARTESIAN_POINT ( 'NONE',  ( 3.783945140921864070, -0.9226758061156097313, 1.627204332209288395 ) ) ;
#7099 = CARTESIAN_POINT ( 'NONE',  ( 3.827072092044791596, 2.190881801378454785, 0.7251257774964211533 ) ) ;
#7100 = CARTESIAN_POINT ( 'NONE',  ( 3.156551239342288095, -0.5378050974185369926, -1.781664776597549293 ) ) ;
#7101 = CARTESIAN_POINT ( 'NONE',  ( 0.6823417656249899377, 4.676041667008086655, -1.181850606188754593 ) ) ;
#7102 = CARTESIAN_POINT ( 'NONE',  ( -5.274285450916075035, 6.112086766612214284, 1.199719254218450271 ) ) ;
#7103 = CARTESIAN_POINT ( 'NONE',  ( 6.474182045725470402, 7.511966127223233869, -1.199719254218446718 ) ) ;
#7104 = CARTESIAN_POINT ( 'NONE',  ( 6.605500049835216103, -8.049367966558019560, 6.875062624577640058 ) ) ;
#7105 = CARTESIAN_POINT ( 'NONE',  ( 0.6980488080095709202, -0.7561646473010454894, 1.965825473679798652 ) ) ;
#7106 = CARTESIAN_POINT ( 'NONE',  ( 4.378920427089557421, 5.171457255435017331, -1.082531754730548412 ) ) ;
#7108 = CARTESIAN_POINT ( 'NONE',  ( 0.7500000000000006661, 8.833333333333332149, 1.299038105676657340 ) ) ;
#7107 = CARTESIAN_POINT ( 'NONE',  ( -1.364683531250010295, 5.592708333674750953, 0.7879004041258379498 ) ) ;
#7109 = CARTESIAN_POINT ( 'NONE',  ( 6.907524304660562109, -0.4813806915026208055, 2.115094849305596103 ) ) ;
#7110 = CARTESIAN_POINT ( 'NONE',  ( 1.740644586495963431, 1.216819214799185866, -1.736574482785017359 ) ) ;
#7111 = DIRECTION ( 'NONE',  ( 5.578564026256490882E-16, 1.000000000000000000, 9.066213480720158442E-32 ) ) ;
#7112 = CARTESIAN_POINT ( 'NONE',  ( 0.5276105490271070231, -0.2919958673943868765, 1.998420469645475483 ) ) ;
#7113 = CARTESIAN_POINT ( 'NONE',  ( -0.6823417656250212460, 1.301041667008083547, 1.181850606188755259 ) ) ;
#7114 = CARTESIAN_POINT ( 'NONE',  ( -3.307826292054316664, 4.882216645528547616, -1.443375672974059665 ) ) ;
#7115 = CARTESIAN_POINT ( 'NONE',  ( 5.148345644887269756, 7.029489223833707001, -1.599625672291256295 ) ) ;
#7116 = EDGE_LOOP ( 'NONE', ( #145175, #143722, #160934, #141114, #2642, #68990 ) ) ;
#7117 = CARTESIAN_POINT ( 'NONE',  ( 1.546389740860309781, 2.159050155192781872, 0.1077149563947499555 ) ) ;
#7118 = CARTESIAN_POINT ( 'NONE',  ( 0.000000000000000000, -1.500000000000001332, 0.000000000000000000 ) ) ;
#7121 = CARTESIAN_POINT ( 'NONE',  ( 4.867013957625893283, 4.780530493426062399, 1.040834085586084257E-14 ) ) ;
#7120 = CARTESIAN_POINT ( 'NONE',  ( 6.925078400183559246, 1.280611897634201357, 1.970548662192173284 ) ) ;
#7119 = CARTESIAN_POINT ( 'NONE',  ( 5.061990249855835344, 6.999017606288844284, -1.599625672291273171 ) ) ;
#7122 = CARTESIAN_POINT ( 'NONE',  ( -4.004454267989906668, 5.765225627445230927, 1.599625672291270506 ) ) ;
#7123 = CARTESIAN_POINT ( 'NONE',  ( 6.368375356916068597, -1.978549699825098429, -0.3886382054163611821 ) ) ;
#7124 = CARTESIAN_POINT ( 'NONE',  ( -7.944714827928056167, 10.29191993738131927, 1.443375672974090751 ) ) ;
#7125 = CARTESIAN_POINT ( 'NONE',  ( 6.620655732516666170, 0.0004550665020433551948, 2.073887158236031425 ) ) ;
#7126 = DIRECTION ( 'NONE',  ( -0.000000000000000000, -1.000000000000000000, -0.000000000000000000 ) ) ;
#7128 = CARTESIAN_POINT ( 'NONE',  ( -1.364683531250010740, 10.38020833367473017, 0.7879004041258445001 ) ) ;
#7127 = CARTESIAN_POINT ( 'NONE',  ( 0.3216218905449366172, -0.1073394912241855820, 2.260102045549317928 ) ) ;
#7129 = CARTESIAN_POINT ( 'NONE',  ( -10.08065090696061716, 11.71951313199760136, -1.199719254218441611 ) ) ;
#7130 = EDGE_CURVE ( 'NONE', #65269, #32497, #48810, .T. ) ;
#7132 = CARTESIAN_POINT ( 'NONE',  ( 1.001416299785270247, -1.868574072159228994, 0.4210543004025939506 ) ) ;
#7131 = CARTESIAN_POINT ( 'NONE',  ( -4.731432421044865499, 8.463828891286912182, -0.7216878364870257245 ) ) ;
#7133 = CARTESIAN_POINT ( 'NONE',  ( 1.364683531249988757, 0.9468750003414211358, 0.000000000000000000 ) ) ;
#7134 = CARTESIAN_POINT ( 'NONE',  ( -1.420000000000001039, 6.120000000000041851, -2.579999999999995630 ) ) ;
#7135 = CARTESIAN_POINT ( 'NONE',  ( 1.499999999999993117, 9.604166666666669627, 0.8660254037844409281 ) ) ;
#7136 = CARTESIAN_POINT ( 'NONE',  ( 2.736579049320194468, 0.2108767276123752754, 1.711865116355310246 ) ) ;
#7137 = CARTESIAN_POINT ( 'NONE',  ( 6.052789233858158369, 6.026285292448116948, 0.000000000000000000 ) ) ;
#7138 = CARTESIAN_POINT ( 'NONE',  ( 1.774285776001020221, -1.678457933910833644, -0.5611888468203419800 ) ) ;
#7140 = CARTESIAN_POINT ( 'NONE',  ( 1.805339258485965992, 1.750370858315702272, -0.9942575048343755828 ) ) ;
#7139 = MECHANICAL_DESIGN_GEOMETRIC_PRESENTATION_REPRESENTATION (  '', ( #121350 ), #69448 ) ;
#7141 = CARTESIAN_POINT ( 'NONE',  ( 9.043854491632929538, 2.018041202054163374, 8.143123160307325747 ) ) ;
#7142 = CARTESIAN_POINT ( 'NONE',  ( 10.40996301719436090, 11.03937836301526687, 0.000000000000000000 ) ) ;
#7143 = CARTESIAN_POINT ( 'NONE',  ( 4.419099417909471583, 2.016199240759775524, 0.8975180220924662278 ) ) ;
#7144 = VERTEX_POINT ( 'NONE', #78096 ) ;
#7145 = CARTESIAN_POINT ( 'NONE',  ( -6.424584688029276514, 8.588711117491191871, 1.599625672291269396 ) ) ;
#7147 = CARTESIAN_POINT ( 'NONE',  ( 4.042592340535226647, -1.492244431823461337, 1.356313616978216618 ) ) ;
#7146 = CARTESIAN_POINT ( 'NONE',  ( 3.967525559752110631, -1.763746451813380967, -1.176840329774282212 ) ) ;
#7149 = ORIENTED_EDGE ( 'NONE', *, *, #82737, .F. ) ;
#7148 = CARTESIAN_POINT ( 'NONE',  ( 4.640750240102114788, 1.735609681454729492, 0.5192115853321179753 ) ) ;
#7150 = CARTESIAN_POINT ( 'NONE',  ( 5.896870467300973750, 5.844380064798101237, 0.7998128361456352531 ) ) ;
#7151 = ORIENTED_EDGE ( 'NONE', *, *, #126186, .T. ) ;
#7152 = CARTESIAN_POINT ( 'NONE',  ( 1.779943879855113709, -1.003247456797161652, 1.578688272967261996 ) ) ;
#7153 = EDGE_CURVE ( 'NONE', #110107, #90194, #68756, .T. ) ;
#7154 = CARTESIAN_POINT ( 'NONE',  ( -11.96215121607992593, 11.32833553780823799, -0.9565349792967606790 ) ) ;
#7155 = DIRECTION ( 'NONE',  ( 0.000000000000000000, 1.496258514059622730E-16, -1.000000000000000000 ) ) ;
#7156 = DIRECTION ( 'NONE',  ( -1.000000000000000000, 6.505213034913026604E-16, 0.000000000000000000 ) ) ;
#7157 = DIRECTION ( 'NONE',  ( 1.000000000000000000, -0.000000000000000000, -0.000000000000000000 ) ) ;
#7158 = CARTESIAN_POINT ( 'NONE',  ( 1.364683531249986537, 2.717708333674754062, -0.7879004041258239610 ) ) ;
#7159 = LINE ( 'NONE', #125290, #43171 ) ;
#7160 = ORIENTED_EDGE ( 'NONE', *, *, #59177, .F. ) ;
#7161 = CARTESIAN_POINT ( 'NONE',  ( 6.034787771858531435, 10.05468647722803865, 0.000000000000000000 ) ) ;
#7162 = ADVANCED_FACE ( 'NONE', ( #144223 ), #84647, .T. ) ;
#7163 = CARTESIAN_POINT ( 'NONE',  ( -4.828112100242294424, 5.765790550771681566, -1.082531754730549967 ) ) ;
#7164 = CARTESIAN_POINT ( 'NONE',  ( -6.557303570864871034, 7.679217583210999010, -1.199719254218452047 ) ) ;
#7165 = CARTESIAN_POINT ( 'NONE',  ( 3.937823072884456099, -2.028283017459261650, 0.6187693826033290323 ) ) ;
#7167 = CARTESIAN_POINT ( 'NONE',  ( -10.93377262805118555, 5.994763374826558966, -6.297255446303106297 ) ) ;
#7166 = CARTESIAN_POINT ( 'NONE',  ( 2.530224277154552226, 2.018041202053995953, -11.90376931803466931 ) ) ;
#7168 = CARTESIAN_POINT ( 'NONE',  ( 5.360604507329317592, -1.429826957936894960, 1.357393395290319660 ) ) ;
#7169 = CARTESIAN_POINT ( 'NONE',  ( -1.364683531250012516, 0.7802083336747528408, 0.7879004041258379498 ) ) ;
#7170 = CARTESIAN_POINT ( 'NONE',  ( 0.5979028997950117663, 1.355058449971069834, 1.489028425022032698 ) ) ;
#7171 = VERTEX_POINT ( 'NONE', #30432 ) ;
#7172 = CARTESIAN_POINT ( 'NONE',  ( 0.4392562211190715882, -1.791127875450468920, -1.128673114062600957 ) ) ;
#7173 = CARTESIAN_POINT ( 'NONE',  ( 1.363825363374836286, -0.5049007678423790280, 2.007717453658082629 ) ) ;
#7174 = ORIENTED_EDGE ( 'NONE', *, *, #42629, .F. ) ;
#7175 = CARTESIAN_POINT ( 'NONE',  ( 5.367048706163317640, 7.354919138647580290, -1.599625672291281386 ) ) ;
#7176 = CARTESIAN_POINT ( 'NONE',  ( 6.737475991348287785, 6.825086509519945999, -0.7998128361456481317 ) ) ;
#7178 = CARTESIAN_POINT ( 'NONE',  ( 4.843287188579786573, 6.673587691474970107, -1.599625672291256295 ) ) ;
#7177 = CARTESIAN_POINT ( 'NONE',  ( 3.785173937466048244, 1.514314676582936947, 1.441642292586094110 ) ) ;
#7179 = CARTESIAN_POINT ( 'NONE',  ( 7.550965208168244125, 7.774157262476569130, -0.7998128361456341429 ) ) ;
#7182 = VERTEX_POINT ( 'NONE', #62909 ) ;
#7181 = CARTESIAN_POINT ( 'NONE',  ( 1.910541399130718743, -0.4838386274770510864, -1.745561575705076862 ) ) ;
#7180 = CARTESIAN_POINT ( 'NONE',  ( 3.416849837094409370, 1.649954109374281996, 0.7815844185870900462 ) ) ;
#7183 = CARTESIAN_POINT ( 'NONE',  ( 5.690102719724574598, -0.9953569382129350274, 1.969734210959340093 ) ) ;
#7184 = DIRECTION ( 'NONE',  ( 8.638326563840814399E-31, -0.000000000000000000, 1.000000000000000000 ) ) ;
#7185 = CARTESIAN_POINT ( 'NONE',  ( 4.682781310676605635, -2.139571651222616833, -0.5399477217277389718 ) ) ;
#7186 = CARTESIAN_POINT ( 'NONE',  ( 7.633404179693907388, 8.864391950186421454, -1.199719254218441611 ) ) ;
#7187 = CARTESIAN_POINT ( 'NONE',  ( 4.080641032480825103, 5.783833874167997102, -1.249999999999999334 ) ) ;
#7188 = CARTESIAN_POINT ( 'NONE',  ( 3.211475575234080004, 1.509012206799903666, 1.174515185244667581 ) ) ;
#7189 = CARTESIAN_POINT ( 'NONE',  ( 7.086107841436786181, 11.41887624831828418, 1.040834085586084257E-14 ) ) ;
#7190 = CARTESIAN_POINT ( 'NONE',  ( 6.355931484454268698, -0.7012994977402075003, 1.948090369817329526 ) ) ;
#7191 = CARTESIAN_POINT ( 'NONE',  ( 1.522480120926855029, 8.691153603980712461, -2.524399069149761310 ) ) ;
#7192 = CARTESIAN_POINT ( 'NONE',  ( 5.566036750361066154, -1.391122746885119499, 1.693456055751572986 ) ) ;
#7193 = CARTESIAN_POINT ( 'NONE',  ( 0.4999999999999779066, 3.999999999999989786, 0.4999999999999640288 ) ) ;
#7194 = EDGE_LOOP ( 'NONE', ( #98846, #38360, #129656, #61430 ) ) ;
#7195 = ORIENTED_EDGE ( 'NONE', *, *, #161057, .F. ) ;
#7196 = DIRECTION ( 'NONE',  ( -0.6483454320283799088, 0.000000000000000000, 0.7613463080411786432 ) ) ;
#7197 = ADVANCED_FACE ( 'NONE', ( #129079 ), #61913, .T. ) ;
#7198 = CARTESIAN_POINT ( 'NONE',  ( 5.585032934186686226, 5.480569609498057382, 0.000000000000000000 ) ) ;
#7199 = CARTESIAN_POINT ( 'NONE',  ( -1.642778471874998480, -1.888541666188708890, 2.845375778867863303 ) ) ;
#7200 = PRESENTATION_STYLE_ASSIGNMENT (( #189174 ) ) ;
#7201 = CARTESIAN_POINT ( 'NONE',  ( -7.321039761699444703, 10.52466824108257804, 1.082531754730549967 ) ) ;
#7202 = CARTESIAN_POINT ( 'NONE',  ( 4.224247379109608680, 7.085983154673295203, -1.199719254218452047 ) ) ;
#7203 = CARTESIAN_POINT ( 'NONE',  ( 6.034052368894809781, 1.228512962337786396, 1.666229478724051027 ) ) ;
#7204 = CARTESIAN_POINT ( 'NONE',  ( 3.949766350991973596, 0.6478974803514454539, -1.814415559773856490 ) ) ;
#7205 = CARTESIAN_POINT ( 'NONE',  ( 1.441030037510174777, -1.730879250949714843, -1.034145807338890277 ) ) ;
#7206 = CARTESIAN_POINT ( 'NONE',  ( -8.646349277213090545, 11.11049346154719508, 1.599625672291269396 ) ) ;
#7207 = CARTESIAN_POINT ( 'NONE',  ( 5.982890925380405456, 10.20206618957764100, 0.000000000000000000 ) ) ;
#7208 = CARTESIAN_POINT ( 'NONE',  ( -4.180211397942203533, 3.976498670287245130, -0.5934635338003064753 ) ) ;
#7209 = CARTESIAN_POINT ( 'NONE',  ( 1.008081207548201741, -0.9882381260516819310, -1.956047874660173047 ) ) ;
#7210 = CARTESIAN_POINT ( 'NONE',  ( 5.074738461036464088, -1.720261882950037124, -0.6118011564382742629 ) ) ;
#7211 = CARTESIAN_POINT ( 'NONE',  ( 4.421367491832258523, 8.172362817197399210, 0.7216878364870257245 ) ) ;
#7212 = CARTESIAN_POINT ( 'NONE',  ( 8.563946585326370098, 13.14302144952281814, 0.7998128361456462443 ) ) ;
#7213 = CARTESIAN_POINT ( 'NONE',  ( -5.794130544993808307, 7.853181283949808744, 1.599625672291263179 ) ) ;
#7214 = CARTESIAN_POINT ( 'NONE',  ( 3.734381245560244089, 6.444196322207211836, 1.199719254218462483 ) ) ;
#7215 = CARTESIAN_POINT ( 'NONE',  ( 6.861835142292135536, 9.098836647464588978, 1.443375672974065660 ) ) ;
#7216 = ORIENTED_EDGE ( 'NONE', *, *, #4999, .F. ) ;
#7218 = CARTESIAN_POINT ( 'NONE',  ( 6.328391183068679204, -0.9529656412403487709, -1.773404795463069838 ) ) ;
#7217 = CARTESIAN_POINT ( 'NONE',  ( 3.052128622409277181, -1.392423357299840792, 1.204796875372941667 ) ) ;
#7219 = CARTESIAN_POINT ( 'NONE',  ( 1.898275044819753621, 0.2256094754716081452, 2.287263704067198145 ) ) ;
#7220 = CARTESIAN_POINT ( 'NONE',  ( 6.649272889308863732, 1.708415183241231983, -0.9640671636572254455 ) ) ;
#7221 = CARTESIAN_POINT ( 'NONE',  ( -6.878064000834399394, 6.918829510595249310, -0.7998128361456291469 ) ) ;
#7222 = CARTESIAN_POINT ( 'NONE',  ( 3.726736447152957599, 1.348887845406310682, -1.355897031963343213 ) ) ;
#7223 = CARTESIAN_POINT ( 'NONE',  ( -8.890396042259075315, 11.39521468743417998, -1.599625672291263179 ) ) ;
#7224 = CARTESIAN_POINT ( 'NONE',  ( 0.3267351109269465148, -1.353470794461093973, 1.566751113397255812 ) ) ;
#7225 = CARTESIAN_POINT ( 'NONE',  ( -7.919371124158132602, 8.411890197705517380, -0.7216878364870338292 ) ) ;
#7227 = CARTESIAN_POINT ( 'NONE',  ( 1.533845512228737551, 0.9248708299973290581, -1.625957014461040906 ) ) ;
#7226 = CARTESIAN_POINT ( 'NONE',  ( 2.068024735862358021, -1.283949768261948288, 1.649988806608338798 ) ) ;
#7228 = CARTESIAN_POINT ( 'NONE',  ( 1.915388525686153143, 0.6297767875703685903, 1.915307412907449436 ) ) ;
#7229 = CARTESIAN_POINT ( 'NONE',  ( 9.436111725431318931, 10.11114455586577776, -0.7216878364870257245 ) ) ;
#7230 = CARTESIAN_POINT ( 'NONE',  ( -1.201851678989727383E-14, 4.134375000341417028, 1.575800808251672791 ) ) ;
#7231 = CARTESIAN_POINT ( 'NONE',  ( 2.067524827727816650, -1.070173352442949311, 1.372458522238986234 ) ) ;
#7232 = VECTOR ( 'NONE', #21262, 1000.000000000000114 ) ;
#7233 = CARTESIAN_POINT ( 'NONE',  ( 6.498435699651741615, 6.475929825882159818, -0.7998128361456281477 ) ) ;
#7234 = CARTESIAN_POINT ( 'NONE',  ( 5.477130869796502211, 5.492333557625114437, 1.040834085586084257E-14 ) ) ;
#7235 = CARTESIAN_POINT ( 'NONE',  ( 2.472937804810691809, 0.08526638500995675773, -1.722893361390212874 ) ) ;
#7236 = CARTESIAN_POINT ( 'NONE',  ( 2.613028500285840661, -0.2118117899099076218, 2.181281865515646068 ) ) ;
#7237 = CARTESIAN_POINT ( 'NONE',  ( 4.828867971087246858, 2.111205472107956282, 0.6427781511747706622 ) ) ;
#7238 = CARTESIAN_POINT ( 'NONE',  ( -9.348561386899501002, 3.999985931113709814, -7.001914024221969512 ) ) ;
#7239 = CARTESIAN_POINT ( 'NONE',  ( 2.729531698892784242, 0.1106738598409856555, -2.168390435917330716 ) ) ;
#7240 = CARTESIAN_POINT ( 'NONE',  ( 2.033574986395149775, -1.191784744093337123, -1.383114941912518159 ) ) ;
#7241 = FILL_AREA_STYLE_COLOUR ( '', #142140 ) ;
#7242 = CARTESIAN_POINT ( 'NONE',  ( 4.593022152086825294, 1.843820828628543129, 1.040707789177892861 ) ) ;
#7243 = CARTESIAN_POINT ( 'NONE',  ( 6.639320575229259447, 0.002292789353198348111, 1.996863816985874118 ) ) ;
#7244 = EDGE_CURVE ( 'NONE', #63064, #109831, #112400, .T. ) ;
#7245 = EDGE_LOOP ( 'NONE', ( #76066, #19170, #76185, #121161, #170992, #129106, #195463, #46906, #32354, #38643, #43676, #201622, #71640, #97228, #116706, #543, #72477, #42284, #138579, #164376 ) ) ;
#7247 = CARTESIAN_POINT ( 'NONE',  ( -0.6823417656250212460, 1.863541667008083991, 1.181850606188755259 ) ) ;
#7246 = CARTESIAN_POINT ( 'NONE',  ( 5.284854174503876401, 2.022835781599085614, -1.078525118384612735 ) ) ;
#7248 = DIRECTION ( 'NONE',  ( 1.276756478318932585E-15, -1.000000000000000000, 1.665334536937738262E-16 ) ) ;
#7249 = CARTESIAN_POINT ( 'NONE',  ( 3.999819011231439347, 4.625209253646830554, 1.199719254218464037 ) ) ;
#7250 = CIRCLE ( 'NONE', #166374, 2.080000000000000071 ) ;
#7251 = CARTESIAN_POINT ( 'NONE',  ( 6.633471381225481522, -0.1569934505771773126, 2.186332552071496682 ) ) ;
#7252 = CARTESIAN_POINT ( 'NONE',  ( -6.290620087060847965, 7.401773525401500464, 1.082531754730549967 ) ) ;
#7253 = CARTESIAN_POINT ( 'NONE',  ( 5.029711800989886683, 4.970344644017389513, 1.040834085586084257E-14 ) ) ;
#7254 = CARTESIAN_POINT ( 'NONE',  ( -5.205967797523171292, 9.017453497178271604, 0.000000000000000000 ) ) ;
#7255 = LINE ( 'NONE', #60291, #96440 ) ;
#7256 = VERTEX_POINT ( 'NONE', #165749 ) ;
#7257 = CARTESIAN_POINT ( 'NONE',  ( 5.063125043234593115, -1.117834493326537393, 1.678003986596336761 ) ) ;
#7259 = CARTESIAN_POINT ( 'NONE',  ( 3.537984270275731369, 1.304693584366970249, 1.597530370294945046 ) ) ;
#7258 = CARTESIAN_POINT ( 'NONE',  ( 5.148345644887269756, 7.029489223833707001, -1.599625672291256295 ) ) ;
#7261 = CARTESIAN_POINT ( 'NONE',  ( -0.2409995289980037536, -0.004801160710915518791, -2.000252362011435192 ) ) ;
#7260 = CARTESIAN_POINT ( 'NONE',  ( 5.982890925380405456, 10.20206618957764100, 0.000000000000000000 ) ) ;
#7262 = CARTESIAN_POINT ( 'NONE',  ( 6.339319342841494453, 9.553567112360518365, -1.199719254218452047 ) ) ;
#7263 = CARTESIAN_POINT ( 'NONE',  ( 1.001543065824772753E-15, -3.171874999522042327, 3.793834371823811669 ) ) ;
#7264 = CARTESIAN_POINT ( 'NONE',  ( -1.364683531249997417, 5.759375000341418804, 1.214306433183764966E-14 ) ) ;
#7265 = CARTESIAN_POINT ( 'NONE',  ( 6.544889499999918314, -1.757580744090202041, -1.308772488114395616 ) ) ;
#7266 = CARTESIAN_POINT ( 'NONE',  ( 3.006482587178582300, -1.942541511447487990, 0.5404910644229294903 ) ) ;
#7267 = CARTESIAN_POINT ( 'NONE',  ( 2.876309626556411203, -0.1380247437976732383, -1.836149222064882514 ) ) ;
#7268 = EDGE_CURVE ( 'NONE', #9317, #157271, #151758, .T. ) ;
#7269 = CARTESIAN_POINT ( 'NONE',  ( 6.169123589417988995, 7.156064594864501416, -1.199719254218445830 ) ) ;
#7270 = FILL_AREA_STYLE_COLOUR ( '', #179735 ) ;
#7271 = CARTESIAN_POINT ( 'NONE',  ( 6.088856429251793934, -0.2706771573857471580, -1.805266125362497531 ) ) ;
#7272 = CARTESIAN_POINT ( 'NONE',  ( -7.549192604710863286, 7.701812881784464437, -0.7998128361456291469 ) ) ;
#7273 = CARTESIAN_POINT ( 'NONE',  ( 6.385631343721732911, 1.554564302923328700, 1.644106664497286596 ) ) ;
#7274 = CARTESIAN_POINT ( 'NONE',  ( 2.227300950330353579, 0.0009978793536376256035, 2.106257355060832115 ) ) ;
#7275 = CARTESIAN_POINT ( 'NONE',  ( -5.424143973919053785, 8.485862515284315677, 1.199719254218454489 ) ) ;
#7276 = CARTESIAN_POINT ( 'NONE',  ( 8.125414133291656071, 8.374071331795406081, -0.7998128361456291469 ) ) ;
#7277 = CARTESIAN_POINT ( 'NONE',  ( 6.983858524370782916, 7.320458831286981827, 0.7216878364870328300 ) ) ;
#7278 = CARTESIAN_POINT ( 'NONE',  ( 0.000000000000000000, 0.000000000000000000, 0.000000000000000000 ) ) ;
#7279 = CARTESIAN_POINT ( 'NONE',  ( -6.256197817702116026, 9.386315656372753224, -1.199719254218440723 ) ) ;
#7280 = CARTESIAN_POINT ( 'NONE',  ( 5.287316719205157334, 9.112360572473935605, 1.040834085586084257E-14 ) ) ;
#7281 = CARTESIAN_POINT ( 'NONE',  ( 4.279786810092509164, 7.480689796721937235, 1.046525044888670486 ) ) ;
#7282 = CARTESIAN_POINT ( 'NONE',  ( -6.098470168048611306, 6.009303372345148553, 1.040834085586084257E-14 ) ) ;
#7283 = CARTESIAN_POINT ( 'NONE',  ( 3.744553100839841608, 1.186064971860462114, -1.878093021827110354 ) ) ;
#7284 = CARTESIAN_POINT ( 'NONE',  ( 2.097856687836355150, -2.190910012095201420, 0.05558666267656967030 ) ) ;
#7285 = CARTESIAN_POINT ( 'NONE',  ( -5.656776405399756236, 7.622658444431597680, -1.599625672291256295 ) ) ;
#7286 = CARTESIAN_POINT ( 'NONE',  ( 0.1884680354247054990, -1.036234488384666586, 1.948478269905975946 ) ) ;
#7287 = CARTESIAN_POINT ( 'NONE',  ( -4.773352600463090845, 7.726605912919016106, 1.199719254218452935 ) ) ;
#7288 = CARTESIAN_POINT ( 'NONE',  ( 5.002378505967388200, 1.956489882415031190, 0.1462272935644214900 ) ) ;
#7289 = CARTESIAN_POINT ( 'NONE',  ( 0.4635302585514287088, 1.806487598472360956, -0.2625014351145052438 ) ) ;
#7290 = DIRECTION ( 'NONE',  ( 0.1653894851707868319, -0.9636043447860246358, -0.2100309141636969024 ) ) ;
#7291 = CARTESIAN_POINT ( 'NONE',  ( 0.6823417656249882723, 1.926041667008083991, -1.181850606188749264 ) ) ;
#7292 = CARTESIAN_POINT ( 'NONE',  ( -3.011319516011047082, 6.527306845405913549, 0.7216878364870328300 ) ) ;
#7293 = CARTESIAN_POINT ( 'NONE',  ( -5.666945020832185875, 7.634521829102760115, 1.443375672974064550 ) ) ;
#7294 = AXIS2_PLACEMENT_3D ( 'NONE', #13753, #192501, #191433 ) ;
#7295 = CARTESIAN_POINT ( 'NONE',  ( 3.832379111121624327, -1.093062754469842579, -1.817066923117337751 ) ) ;
#7296 = CARTESIAN_POINT ( 'NONE',  ( -5.008811405605897882, 4.808311159487113073, 0.7998128361456281477 ) ) ;
#7297 = CARTESIAN_POINT ( 'NONE',  ( 5.454052192070485638, 2.159419290912270029, -0.1019294599445344784 ) ) ;
#7298 = CARTESIAN_POINT ( 'NONE',  ( 6.657217119509961201, 7.725507046638470321, -1.199719254218446718 ) ) ;
#7299 = CARTESIAN_POINT ( 'NONE',  ( 5.530750200611445067, -1.661959182355336795, 0.7928504710919548337 ) ) ;
#7300 = UNCERTAINTY_MEASURE_WITH_UNIT (LENGTH_MEASURE( 1.000000000000000082E-05 ), #207618, 'distance_accuracy_value', 'NONE');
#7301 = VECTOR ( 'NONE', #176467, 1000.000000000000000 ) ;
#7302 = CARTESIAN_POINT ( 'NONE',  ( -5.833005281931015418, 6.047509994665502653, 0.4702358434125544773 ) ) ;
#7303 = CARTESIAN_POINT ( 'NONE',  ( 1.364683531249986537, 1.467708333674748289, -0.7879004041258239610 ) ) ;
#7304 = CARTESIAN_POINT ( 'NONE',  ( -0.1239745564502250652, -0.1323307239476738673, -1.711383809018538038 ) ) ;
#7305 = CARTESIAN_POINT ( 'NONE',  ( 6.827182134110196365, 2.083530588508203607, 2.119847806254702594 ) ) ;
#7306 = CARTESIAN_POINT ( 'NONE',  ( 3.958617665510264949, 5.641473247893851628, -1.443375672974051449 ) ) ;
#7307 = PLANE ( 'NONE',  #52974 ) ;
#7308 = CARTESIAN_POINT ( 'NONE',  ( 4.452137864729129646, 2.161286467946467837, -0.05003489268536746859 ) ) ;
#7309 = CARTESIAN_POINT ( 'NONE',  ( -3.588104209110990706, 7.337872010604796991, 1.040834085586084257E-14 ) ) ;
#7310 = CARTESIAN_POINT ( 'NONE',  ( 0.3327679910518215878, -1.139612444193355278, 1.306804640533586026 ) ) ;
#7311 = CARTESIAN_POINT ( 'NONE',  ( -8.500599125644013654, 9.019713189447241319, 0.7216878364870438212 ) ) ;
#7312 = CARTESIAN_POINT ( 'NONE',  ( 3.098656953246520906, -0.6260995091542166380, -2.069055637940686143 ) ) ;
#7313 = CARTESIAN_POINT ( 'NONE',  ( 5.343030940550726804, -1.692140053440434277, 1.011138898101251016 ) ) ;
#7314 = CARTESIAN_POINT ( 'NONE',  ( 4.288270029534011485, -1.659180151977168283, 0.5033209731903751649 ) ) ;
#7315 = ADVANCED_FACE ( 'NONE', ( #180925 ), #12, .T. ) ;
#7316 = CARTESIAN_POINT ( 'NONE',  ( 0.6795420635867071013, 1.475991390215245058, 1.620154534501851096 ) ) ;
#7317 = CARTESIAN_POINT ( 'NONE',  ( 1.519075522400476830, 1.548194965108589782, -1.711296875134951545 ) ) ;
#7318 = CARTESIAN_POINT ( 'NONE',  ( 3.145831276397454079, 0.7450406991881215468, -1.921561753228885783 ) ) ;
#7319 = CARTESIAN_POINT ( 'NONE',  ( 6.093304272135602773, -0.6500253571345508963, 1.830188593850643697 ) ) ;
#7320 = CARTESIAN_POINT ( 'NONE',  ( -6.954969613686107444, 10.09758640173367894, 1.082531754730549967 ) ) ;
#7322 = ADVANCED_FACE ( 'NONE', ( #68216 ), #52000, .F. ) ;
#7321 = CARTESIAN_POINT ( 'NONE',  ( -5.143339171537843590, 7.093924681584509173, 1.599625672291263179 ) ) ;
#7323 = CARTESIAN_POINT ( 'NONE',  ( -1.084637062511556005, 2.963621193390831632, 1.105835307554803082 ) ) ;
#7325 = VERTEX_POINT ( 'NONE', #118126 ) ;
#7324 = CARTESIAN_POINT ( 'NONE',  ( -4.787964524281469458, 5.614988695530339413, -1.199719254218453823 ) ) ;
#7326 = CARTESIAN_POINT ( 'NONE',  ( -7.985389288324703294, 9.379004260209384825, -1.082531754730543083 ) ) ;
#7327 = CARTESIAN_POINT ( 'NONE',  ( 2.239569982544288518, -1.971322999760493300, 0.9919465654871155724 ) ) ;
#7328 = CARTESIAN_POINT ( 'NONE',  ( 1.001543065824772753E-15, -3.609374999522044547, 3.793834371823811669 ) ) ;
#7329 = ORIENTED_EDGE ( 'NONE', *, *, #102584, .T. ) ;
#7330 = CARTESIAN_POINT ( 'NONE',  ( 0.6372766190945264864, 1.739209566756502845, -0.6625725129940361890 ) ) ;
#7331 = CARTESIAN_POINT ( 'NONE',  ( -0.1291982275798261026, 4.084732128465967449, -2.628654587324832814 ) ) ;
#7332 = CARTESIAN_POINT ( 'NONE',  ( 1.499999999999991118, 5.535416667349481123, 0.8660254037844524744 ) ) ;
#7333 = CARTESIAN_POINT ( 'NONE',  ( -9.512045263456275990, -8.176568542494926817, 0.4655551865852147753 ) ) ;
#7335 = CARTESIAN_POINT ( 'NONE',  ( 0.000000000000000000, 12.22000000000000064, 0.000000000000000000 ) ) ;
#7334 = CARTESIAN_POINT ( 'NONE',  ( -0.7499999999999972244, 5.139583334016151639, -1.299038105676652899 ) ) ;
#7336 = CARTESIAN_POINT ( 'NONE',  ( 6.228435704027582176, 0.1854037366294820077, 1.831779187086844729 ) ) ;
#7337 = ORIENTED_EDGE ( 'NONE', *, *, #129965, .T. ) ;
#7338 = CARTESIAN_POINT ( 'NONE',  ( 2.641540400197890825, -1.526127808488053628, -1.385168266076434174 ) ) ;
#7339 = CARTESIAN_POINT ( 'NONE',  ( -0.6801582343750074422, 0.5989583336747372755, -1.178068619123841643 ) ) ;
#7340 = CARTESIAN_POINT ( 'NONE',  ( -7.691553217654356622, 7.867900263551875994, -0.7998128361456291469 ) ) ;
#7341 = CARTESIAN_POINT ( 'NONE',  ( 11.07790593930098311, 13.79999999999999893, -0.7000000000000009548 ) ) ;
#7342 = CARTESIAN_POINT ( 'NONE',  ( 11.94980361723123785, 11.00238056585436652, 1.099999926404769290 ) ) ;
#7343 = CARTESIAN_POINT ( 'NONE',  ( 3.497113557321089861, 6.167384019261527683, -1.199719254218446718 ) ) ;
#7344 = CARTESIAN_POINT ( 'NONE',  ( 0.8310182365124726411, 0.1507505247145359273, 2.055422933874837099 ) ) ;
#7346 = CARTESIAN_POINT ( 'NONE',  ( 4.757273854911123756, 1.820453720981948242, -0.2752165127944474210 ) ) ;
#7345 = DIRECTION ( 'NONE',  ( 0.000000000000000000, 1.000000000000000000, 0.000000000000000000 ) ) ;
#7347 = CARTESIAN_POINT ( 'NONE',  ( 7.820355676984174664, 8.018169799436671852, -0.7998128361456281477 ) ) ;
#7348 = CARTESIAN_POINT ( 'NONE',  ( -5.119085517611572378, 8.129960982925583224, 1.199719254218452935 ) ) ;
#7349 = CARTESIAN_POINT ( 'NONE',  ( -0.2409995289980037536, -0.004801160710915518791, -2.000252362011435192 ) ) ;
#7350 = CARTESIAN_POINT ( 'NONE',  ( 4.477303810882872881, 0.001702072213635372200, -2.207063162522747479 ) ) ;
#7351 = CARTESIAN_POINT ( 'NONE',  ( 6.872354139354274416, -1.400524804419982727, 1.777693731722047588 ) ) ;
#7352 = CARTESIAN_POINT ( 'NONE',  ( -5.802526556968872207, 6.832331073627524454, 1.082531754730548412 ) ) ;
#7353 = CARTESIAN_POINT ( 'NONE',  ( 0.6328886395040033142, 1.767934563615305432, 0.7296191750566642931 ) ) ;
#7354 = CARTESIAN_POINT ( 'NONE',  ( 0.8312679839070147292, -1.592664559859976237, -1.236796411087807801 ) ) ;
#7355 = FACE_OUTER_BOUND ( 'NONE', #24652, .T. ) ;
#7356 = CARTESIAN_POINT ( 'NONE',  ( 1.546695614565428922, 2.123301925303363369, -0.8802762395820094010 ) ) ;
#7357 = CARTESIAN_POINT ( 'NONE',  ( -0.5000000000000022204, 3.300000000000004263, 0.4000000000000010214 ) ) ;
#7358 = CARTESIAN_POINT ( 'NONE',  ( -0.4362825330288316317, -6.085430761754772711, -10.10516068267230594 ) ) ;
#7359 = FILL_AREA_STYLE_COLOUR ( '', #175023 ) ;
#7360 = AXIS2_PLACEMENT_3D ( 'NONE', #71860, #19921, #90286 ) ;
#7361 = CARTESIAN_POINT ( 'NONE',  ( 0.8131078318618142342, -0.2785150557334699073, 1.849687307983488571 ) ) ;
#7362 = CARTESIAN_POINT ( 'NONE',  ( 2.026577684455236561, 0.4465047249504557891, 1.966304233017155845 ) ) ;
#7364 = CARTESIAN_POINT ( 'NONE',  ( -5.793963627187476817, 6.347147481417366066, 0.7933461710243456810 ) ) ;
#7363 = CARTESIAN_POINT ( 'NONE',  ( -1.364683531250012516, 0.5302083336747518416, 0.7879004041258379498 ) ) ;
#7366 = CARTESIAN_POINT ( 'NONE',  ( 3.563196004013529983, -1.857486927118640718, -0.9925908497740908443 ) ) ;
#7365 = CARTESIAN_POINT ( 'NONE',  ( -7.340850106795412167, 10.65174332698158643, 1.199719254218453823 ) ) ;
#7367 = CARTESIAN_POINT ( 'NONE',  ( 6.936968151686458306, 11.24487994360957188, 0.7998128361456462443 ) ) ;
#7369 = CARTESIAN_POINT ( 'NONE',  ( -7.004758919754800139, 11.32396917302262018, 0.000000000000000000 ) ) ;
#7368 = CARTESIAN_POINT ( 'NONE',  ( 4.655245641445829641, 6.524482229810530498, 1.599625672291269396 ) ) ;
#7370 =( LENGTH_UNIT ( ) NAMED_UNIT ( * ) SI_UNIT ( .MILLI., .METRE. ) );
#7371 = CARTESIAN_POINT ( 'NONE',  ( 3.867448311701796371, -1.681569574351711838, -1.118542113429069396 ) ) ;
#7372 = CARTESIAN_POINT ( 'NONE',  ( -1.364683531250010295, 5.280208333674758059, 0.7879004041258379498 ) ) ;
#7373 = CARTESIAN_POINT ( 'NONE',  ( 6.637180544258393766, -0.09741176211745629365, -2.060485520500746848 ) ) ;
#7374 = CARTESIAN_POINT ( 'NONE',  ( 7.782016984564043227, 12.02284421539267356, 0.7216878364870438212 ) ) ;
#7375 = CARTESIAN_POINT ( 'NONE',  ( 4.183022562662654487, -0.2072598778708051315, -2.151613130492259440 ) ) ;
#7376 = CARTESIAN_POINT ( 'NONE',  ( 5.528692779322568640, 9.672168352510192690, 0.7998128361456341429 ) ) ;
#7377 = CARTESIAN_POINT ( 'NONE',  ( -1.201851678989727383E-14, 5.837500000000023448, -1.732050807568863648 ) ) ;
#7379 = CARTESIAN_POINT ( 'NONE',  ( -9.499562137383497529, -9.414773216041247395, 0.1228851354130223589 ) ) ;
#7378 = CARTESIAN_POINT ( 'NONE',  ( 6.692885107001518286, 7.837396042037102717, -1.199719254218452047 ) ) ;
#7380 = CARTESIAN_POINT ( 'NONE',  ( 7.958272981097359811, 9.347368568444167636, -1.082531754730537976 ) ) ;
#7382 = CARTESIAN_POINT ( 'NONE',  ( 0.04325334852941317004, -8.075271019047999488, 11.00023204605253113 ) ) ;
#7381 = CARTESIAN_POINT ( 'NONE',  ( 2.365899470183946640, -0.4773124685180894500, 2.117905883517334775 ) ) ;
#7384 = CARTESIAN_POINT ( 'NONE',  ( 1.276629239279066574, 1.701104413791530767, -0.7050613402737049284 ) ) ;
#7383 = CARTESIAN_POINT ( 'NONE',  ( -4.419594888374909658, 8.100018436505289188, 0.7216878364870458196 ) ) ;
#7385 = CARTESIAN_POINT ( 'NONE',  ( 0.6823417656249899377, 1.842708333674752952, 1.181850606188755259 ) ) ;
#7386 = CARTESIAN_POINT ( 'NONE',  ( 3.087623348389135547, -0.8860277256741244667, 2.004638750299721828 ) ) ;
#7387 = CARTESIAN_POINT ( 'NONE',  ( 4.393008644795362905, 7.016788222801661590, 1.284222742053114041 ) ) ;
#7388 = CARTESIAN_POINT ( 'NONE',  ( 4.047957556655322087, 0.7652766760943878754, -2.129282649148962925 ) ) ;
#7389 = CARTESIAN_POINT ( 'NONE',  ( -6.205881626753225966, 8.263281202677319470, 1.599625672291283607 ) ) ;
#7390 = CARTESIAN_POINT ( 'NONE',  ( 0.6823417656249917140, 4.905208333674755394, 1.181850606188765695 ) ) ;
#7391 = CARTESIAN_POINT ( 'NONE',  ( 6.400493444083267036, 6.807005473012165631, 0.5116258143813920967 ) ) ;
#7392 = CIRCLE ( 'NONE', #55803, 12.00000000000000178 ) ;
#7393 = CARTESIAN_POINT ( 'NONE',  ( 1.499999999999993117, 13.10416666666666963, 0.8660254037844409281 ) ) ;
#7394 = CARTESIAN_POINT ( 'NONE',  ( 6.712695452541852070, 7.004101914153185504, 0.000000000000000000 ) ) ;
#7395 = CARTESIAN_POINT ( 'NONE',  ( 5.641803817319237524, 0.7161603046910887116, -1.618556768665664114 ) ) ;
#7396 = CARTESIAN_POINT ( 'NONE',  ( 8.945682426918439845, 9.331051007693339727, 1.040834085586084257E-14 ) ) ;
#7397 = CARTESIAN_POINT ( 'NONE',  ( 1.975741970143765736, 2.015461639870301358, -0.6107432106882881850 ) ) ;
#7399 = CARTESIAN_POINT ( 'NONE',  ( 1.499999999999987121, 1.254166666666689300, 0.8660254037844524744 ) ) ;
#7398 = CARTESIAN_POINT ( 'NONE',  ( -1.402160292154681736E-14, 10.67187500034139624, 1.575800808251682339 ) ) ;
#7400 = CARTESIAN_POINT ( 'NONE',  ( 1.029674291210751269, 1.899031994249468225, -0.5220998716058099509 ) ) ;
#7401 = CARTESIAN_POINT ( 'NONE',  ( -3.363304624641834106, 6.081549941127532222, -1.199719254218452047 ) ) ;
#7402 = CARTESIAN_POINT ( 'NONE',  ( 1.284279953904121641, 3.284610286488902187, 0.7750000000000135669 ) ) ;
#7404 = ORIENTED_EDGE ( 'NONE', *, *, #207587, .F. ) ;
#7403 = CARTESIAN_POINT ( 'NONE',  ( 6.011934222899888880, -0.6017306232493442320, 1.708898994858050191 ) ) ;
#7405 = CARTESIAN_POINT ( 'NONE',  ( 7.293923454472080792, 9.532663335016016148, 1.443375672974076540 ) ) ;
#7406 = AXIS2_PLACEMENT_3D ( 'NONE', #155832, #139600, #188311 ) ;
#7407 = CARTESIAN_POINT ( 'NONE',  ( 5.190257414508706368, -1.856628772771324210, -0.2281712211116558864 ) ) ;
#7408 = ORIENTED_EDGE ( 'NONE', *, *, #41018, .F. ) ;
#7409 = CARTESIAN_POINT ( 'NONE',  ( 4.645415698524104187, 1.851598927129452177, -0.9261206523473937136 ) ) ;
#7410 = CARTESIAN_POINT ( 'NONE',  ( 0.6124999999999637401, 2.416666666666629659, -1.060881119635962211 ) ) ;
#7411 = CARTESIAN_POINT ( 'NONE',  ( -5.275531169048909952, 7.248148678680751189, -1.443375672974066548 ) ) ;
#7412 = DIRECTION ( 'NONE',  ( 0.000000000000000000, 1.000000000000000000, 0.000000000000000000 ) ) ;
#7413 = CARTESIAN_POINT ( 'NONE',  ( 8.749089199520284410, 9.101692242395490240, 0.7998128361456481317 ) ) ;
#7414 = CARTESIAN_POINT ( 'NONE',  ( -10.65400978224035811, 11.32409958890225710, 1.040834085586084257E-14 ) ) ;
#7415 = CARTESIAN_POINT ( 'NONE',  ( 9.649519325286297189, 4.269047477884574171, 7.134145662718395897 ) ) ;
#7416 = DIRECTION ( 'NONE',  ( -0.6507913734559640506, -0.7592566023653004592, 0.000000000000000000 ) ) ;
#7417 = CARTESIAN_POINT ( 'NONE',  ( -1.364683531250014514, 0.2802083336747505649, 0.7879004041258379498 ) ) ;
#7418 = CARTESIAN_POINT ( 'NONE',  ( -1.500000000000013101, 1.170833333333352710, 0.8660254037844403729 ) ) ;
#7420 = CARTESIAN_POINT ( 'NONE',  ( 4.150767584078112193, 7.994312614733129152, 0.7998128361456321445 ) ) ;
#7419 = CARTESIAN_POINT ( 'NONE',  ( 4.316819842036943911, -1.455217238560998272, 1.315978175897666080 ) ) ;
#7421 = ADVANCED_FACE ( 'NONE', ( #105027 ), #121341, .T. ) ;
#7422 = CARTESIAN_POINT ( 'NONE',  ( 1.634138513624566080, 0.1511188354343559193, -2.010518437453466589 ) ) ;
#7423 = CARTESIAN_POINT ( 'NONE',  ( 3.563261906135759993, 6.332667919118538435, -2.500000000000000444 ) ) ;
#7424 = CARTESIAN_POINT ( 'NONE',  ( -1.992711204631002198E-15, 2.999999999999989342, 1.224999999999989875 ) ) ;
#7425 = CARTESIAN_POINT ( 'NONE',  ( -11.92050416151433012, 9.947946247203631742, 1.381922468431395767 ) ) ;
#7426 = CARTESIAN_POINT ( 'NONE',  ( 2.407302635362520427, -0.4140892318466664057, 1.823965488845371796 ) ) ;
#7427 = CARTESIAN_POINT ( 'NONE',  ( -1.364683531250012516, 4.488541667008090208, -0.7879004041258300672 ) ) ;
#7428 = CARTESIAN_POINT ( 'NONE',  ( 4.570568844821727872, 0.7744313447282255014, 1.858482759491510095 ) ) ;
#7429 = CARTESIAN_POINT ( 'NONE',  ( -8.402302512167102222, 10.82577223566020841, -1.599625672291263179 ) ) ;
#7431 = CARTESIAN_POINT ( 'NONE',  ( 3.480171074976373013, -2.114893226951024108, -0.1016293738061168905 ) ) ;
#7430 = CARTESIAN_POINT ( 'NONE',  ( -5.043269954603569083, 7.867270132804026872, 1.082531754730560403 ) ) ;
#7432 = CARTESIAN_POINT ( 'NONE',  ( -5.952598981286905122, 7.203796195765662880, -1.286163493473730934 ) ) ;
#7433 = CARTESIAN_POINT ( 'NONE',  ( 5.072747062355987602, 1.430223858385268665, -1.497173470029027120 ) ) ;
#7434 = CARTESIAN_POINT ( 'NONE',  ( 6.801350335910821165, 7.963938809097990124, 1.199719254218452047 ) ) ;
#7436 = CARTESIAN_POINT ( 'NONE',  ( 6.620655732516647518, 3.684600858287550906, 2.687722323901103660 ) ) ;
#7435 = CARTESIAN_POINT ( 'NONE',  ( 1.435225040761441972, -1.516673362169782990, -1.439332739067126443 ) ) ;
#7438 = VERTEX_POINT ( 'NONE', #17335 ) ;
#7437 = CARTESIAN_POINT ( 'NONE',  ( 0.09417432218480553674, -0.3651332853754212238, -1.691417143215419028 ) ) ;
#7439 = CARTESIAN_POINT ( 'NONE',  ( 8.098297826064319693, 8.342435640030188893, 0.7998128361456481317 ) ) ;
#7440 = CARTESIAN_POINT ( 'NONE',  ( -3.917943204224951348, 7.514758138330256187, -0.7216878364870535911 ) ) ;
#7441 = SURFACE_STYLE_FILL_AREA ( #173185 ) ;
#7442 = CARTESIAN_POINT ( 'NONE',  ( -10.47051000334347570, 4.046481986658133856, 7.152373939818348347 ) ) ;
#7443 = CARTESIAN_POINT ( 'NONE',  ( 6.602457619730756733, 9.686322408785807525, 1.082531754730558626 ) ) ;
#7445 =( BOUNDED_SURFACE ( )  B_SPLINE_SURFACE ( 3, 2, ( 
 ( #108228, #91935, #21537 ),
 ( #87647, #153717, #5285 ),
 ( #10634, #127699, #109297 ),
 ( #29043, #61533, #193659 ),
 ( #110359, #176363, #76710 ),
 ( #43184, #126620, #192583 ) ),
 .UNSPECIFIED., .F., .F., .T. ) 
 B_SPLINE_SURFACE_WITH_KNOTS ( ( 4, 2, 4 ),
 ( 3, 3 ),
 ( 0.000000000000000000, 0.0003766405729503175871, 0.0007532811459006351741 ),
 ( 0.000000000000000000, 1.000000000000000000 ),
 .UNSPECIFIED. ) 
 GEOMETRIC_REPRESENTATION_ITEM ( )  RATIONAL_B_SPLINE_SURFACE ( (
 ( 1.000000000000000000, 0.7071067811865551223, 1.000000000000000000),
 ( 1.000000000000000000, 0.7211294902950703412, 1.000000000000000000),
 ( 1.000000000000000000, 0.7311181975234362085, 1.000000000000000000),
 ( 1.000000000000000000, 0.7429553055057509514, 1.000000000000000000),
 ( 1.000000000000000000, 0.7451698531061192732, 1.000000000000000000),
 ( 1.000000000000000000, 0.7452309222763021657, 1.000000000000000000) ) ) 
 REPRESENTATION_ITEM ( '' )  SURFACE ( )  );
#7444 = CARTESIAN_POINT ( 'NONE',  ( -1.910130646976150981, 3.278792710263227050, 0.4195261609910668210 ) ) ;
#7446 = CARTESIAN_POINT ( 'NONE',  ( 5.883449979803576646, 0.1360998956825946737, -1.907488392096804874 ) ) ;
#7447 = CARTESIAN_POINT ( 'NONE',  ( -9.671043645249580933, 10.17730576241299900, 0.7998128361456462443 ) ) ;
#7448 = CIRCLE ( 'NONE', #159615, 3.432849766368862632 ) ;
#7449 = CARTESIAN_POINT ( 'NONE',  ( 6.667912619822566000, 6.673652899414787676, 1.040834085586084257E-14 ) ) ;
#7450 = AXIS2_PLACEMENT_3D ( 'NONE', #119670, #169424, #134819 ) ;
#7451 = CARTESIAN_POINT ( 'NONE',  ( -0.4373225248172924462, -7.723431457505077979, 10.96785329849814161 ) ) ;
#7452 = CARTESIAN_POINT ( 'NONE',  ( 2.521453382017309952, 5.885520012421409319, 0.000000000000000000 ) ) ;
#7453 = FACE_OUTER_BOUND ( 'NONE', #22740, .T. ) ;
#7454 = CARTESIAN_POINT ( 'NONE',  ( 2.672928840188529609, 6.270167413528593414, 0.000000000000000000 ) ) ;
#7455 = ORIENTED_EDGE ( 'NONE', *, *, #45482, .T. ) ;
#7456 = EDGE_CURVE ( 'NONE', #6442, #201530, #213028, .T. ) ;
#7457 = CARTESIAN_POINT ( 'NONE',  ( 6.503528962204017994, -1.955192063461574259, 0.4926555484118036454 ) ) ;
#7458 = FACE_OUTER_BOUND ( 'NONE', #209093, .T. ) ;
#7459 = CARTESIAN_POINT ( 'NONE',  ( -1.734723475976807094E-15, 2.999999999999988898, -6.938893903907228378E-15 ) ) ;
#7460 = CARTESIAN_POINT ( 'NONE',  ( -0.1399997263889663501, 0.2375346743129815030, -2.034463206964792548 ) ) ;
#7461 = CARTESIAN_POINT ( 'NONE',  ( -5.748293942514186128, 6.769059690097084747, -1.082531754730544860 ) ) ;
#7462 = CARTESIAN_POINT ( 'NONE',  ( 2.347533153460546806, 5.890539112345938300, 0.000000000000000000 ) ) ;
#7463 = CARTESIAN_POINT ( 'NONE',  ( 2.658990959838656742, 1.584636853462956685, -1.169278883008363135 ) ) ;
#7464 = CARTESIAN_POINT ( 'NONE',  ( 4.851185501729457172, 0.1948232160459452411, -2.006962824030594561 ) ) ;
#7465 = CARTESIAN_POINT ( 'NONE',  ( -6.531277313481209212, 8.642909503859968368, 1.599625672291283607 ) ) ;
#7466 = CARTESIAN_POINT ( 'NONE',  ( 6.727182134110181622, 6.034673098952469950, 2.683942742083842425 ) ) ;
#7467 = CARTESIAN_POINT ( 'NONE',  ( 5.296902861200166512, 1.790115547914197247, 1.263834295783084150 ) ) ;
#7468 = CARTESIAN_POINT ( 'NONE',  ( 0.000000000000000000, 12.29999999999998295, 0.000000000000000000 ) ) ;
#7469 = CARTESIAN_POINT ( 'NONE',  ( 3.452094016638465490, 1.926566264197142830, 0.001310335549949831480 ) ) ;
#7470 = CARTESIAN_POINT ( 'NONE',  ( -8.158255747121117452, 10.54105100977322174, 1.599625672291295375 ) ) ;
#7471 = CARTESIAN_POINT ( 'NONE',  ( -0.02968770228139669398, 7.629137130509076492, -2.426318643530885222 ) ) ;
#7472 = FACE_OUTER_BOUND ( 'NONE', #34916, .T. ) ;
#7473 = CARTESIAN_POINT ( 'NONE',  ( -1.364683531250000748, 12.85937500034139980, 0.000000000000000000 ) ) ;
#7474 = CARTESIAN_POINT ( 'NONE',  ( 5.606460214450851964, 6.499623990736163037, 1.199719254218462483 ) ) ;
#7475 = CARTESIAN_POINT ( 'NONE',  ( -3.733524485140106819, 7.410126666105433024, -2.499999999999995559 ) ) ;
#7476 = CARTESIAN_POINT ( 'NONE',  ( 4.041739190649647817, 6.769093918182960579, -1.082531754730548412 ) ) ;
#7477 = ORIENTED_EDGE ( 'NONE', *, *, #39920, .F. ) ;
#7479 = CARTESIAN_POINT ( 'NONE',  ( 2.807291710112637340, 1.725400251052783052, -1.036881053028392508 ) ) ;
#7478 = CARTESIAN_POINT ( 'NONE',  ( 5.671403949121008203, 1.101820082107987098, 1.475039313902235305 ) ) ;
#7480 = CARTESIAN_POINT ( 'NONE',  ( 5.800273438847154850, -2.081326394616866970, 0.9752826944557994038 ) ) ;
#7482 = CARTESIAN_POINT ( 'NONE',  ( 2.887382943596613849, -1.738241981009930992, 0.6650857031204291392 ) ) ;
#7481 = CARTESIAN_POINT ( 'NONE',  ( 11.92045683181315674, 11.15275927879483220, 1.382340670101856350 ) ) ;
#7483 = CARTESIAN_POINT ( 'NONE',  ( 1.642778471875000035, -0.5760416661887077794, -2.845375778867859751 ) ) ;
#7484 = DIRECTION ( 'NONE',  ( 0.000000000000000000, 0.000000000000000000, 1.000000000000000000 ) ) ;
#7485 = CARTESIAN_POINT ( 'NONE',  ( -5.910464900553636269, 8.982960586366182554, -1.199719254218440723 ) ) ;
#7486 = CARTESIAN_POINT ( 'NONE',  ( -5.329763783947941036, 5.390681634126922361, 0.000000000000000000 ) ) ;
#7487 = CARTESIAN_POINT ( 'NONE',  ( 6.251524270843968445, 2.085125267542327965, -0.1543399900023248728 ) ) ;
#7488 = CARTESIAN_POINT ( 'NONE',  ( 4.528060117284222308, 8.226561203566173930, 0.7216878364870438212 ) ) ;
#7489 = ORIENTED_EDGE ( 'NONE', *, *, #207104, .F. ) ;
#7490 =( NAMED_UNIT ( * ) SI_UNIT ( $, .STERADIAN. ) SOLID_ANGLE_UNIT ( ) );
#7491 = CARTESIAN_POINT ( 'NONE',  ( 6.340463942928090901, 1.707257656261139234, 0.2451334271395839426 ) ) ;
#7492 = CARTESIAN_POINT ( 'NONE',  ( -5.925076824372040640, 6.871343368977510302, 1.199719254218450271 ) ) ;
#7493 = CARTESIAN_POINT ( 'NONE',  ( 1.845948222207854483, 0.2957656664513158007, -1.708526460754287157 ) ) ;
#7494 = CARTESIAN_POINT ( 'NONE',  ( -8.752316528461410172, 14.55265192235988536, 8.156921273040330433 ) ) ;
#7495 = CARTESIAN_POINT ( 'NONE',  ( 7.245729715095587942, -5.507058666270979508, 7.863746947443980062 ) ) ;
#7496 = CARTESIAN_POINT ( 'NONE',  ( -6.501298352952815662, 7.543601818988450169, -1.199719254218446718 ) ) ;
#7497 = DIRECTION ( 'NONE',  ( 5.551115123125765446E-17, 0.000000000000000000, -1.000000000000000000 ) ) ;
#7498 = CARTESIAN_POINT ( 'NONE',  ( 6.614155491087242211, 2.165850671381476023, -0.1511765098734293433 ) ) ;
#7499 = CARTESIAN_POINT ( 'NONE',  ( 5.936143289257818978, 0.8957264799932495025, -1.590785280889392528 ) ) ;
#7500 = CARTESIAN_POINT ( 'NONE',  ( 2.272246806564695021, -0.9202570425024100276, -1.732484491337261456 ) ) ;
#7501 = DIRECTION ( 'NONE',  ( -5.578564026256490882E-16, -1.000000000000000000, -9.066213480720158442E-32 ) ) ;
#7502 = CARTESIAN_POINT ( 'NONE',  ( -10.64045162862669081, 11.30828174301964140, -0.7998128361456221525 ) ) ;
#7503 = CARTESIAN_POINT ( 'NONE',  ( 7.344766530301147789, 9.591980256816594164, 1.599625672291281386 ) ) ;
#7504 = CARTESIAN_POINT ( 'NONE',  ( 3.545663791850160784, -1.958584582392399742, 0.8131309587096480218 ) ) ;
#7505 = LINE ( 'NONE', #41118, #127825 ) ;
#7506 = CARTESIAN_POINT ( 'NONE',  ( 0.4363033266127375742, -8.563898737988809629, -10.12670668089735138 ) ) ;
#7507 = VECTOR ( 'NONE', #53106, 1000.000000000000000 ) ;
#7508 = CARTESIAN_POINT ( 'NONE',  ( -5.590823505525904125, 6.198478227408987351, -0.8910005059661347815 ) ) ;
#7509 = CARTESIAN_POINT ( 'NONE',  ( 1.657173498210939622, 1.694793865239911712, -1.188712540599102141 ) ) ;
#7511 = CARTESIAN_POINT ( 'NONE',  ( -1.364683531250000748, -1.178124999658580752, 0.000000000000000000 ) ) ;
#7510 = CARTESIAN_POINT ( 'NONE',  ( -10.51337128857758074, 4.000503439385035165, 5.786193332252632437 ) ) ;
#7513 = ORIENTED_EDGE ( 'NONE', *, *, #197258, .F. ) ;
#7512 = CARTESIAN_POINT ( 'NONE',  ( 3.071146466883535098, -1.680802468121232573, 1.452339882875167021 ) ) ;
#7514 = CARTESIAN_POINT ( 'NONE',  ( 1.442429577410338615, -1.974492438002553918, -1.176823363874231587 ) ) ;
#7516 = CARTESIAN_POINT ( 'NONE',  ( 6.543808478091840186, 1.418056970388498206, 1.498012503012560170 ) ) ;
#7515 = CARTESIAN_POINT ( 'NONE',  ( 9.625925876022625616, 11.29296361252366765, -1.082531754730537088 ) ) ;
#7518 = CARTESIAN_POINT ( 'NONE',  ( 0.000000000000000000, -3.696874999522040017, -3.793834371823813001 ) ) ;
#7517 = CARTESIAN_POINT ( 'NONE',  ( 3.054329744828568227, 6.785411478933790264, 0.000000000000000000 ) ) ;
#7519 = CARTESIAN_POINT ( 'NONE',  ( 1.734723475976807292E-15, 15.42691958146951414, 11.91973154060106665 ) ) ;
#7520 = DIRECTION ( 'NONE',  ( 0.9829311923673920148, -0.1839735607939816386, 0.000000000000000000 ) ) ;
#7521 = CARTESIAN_POINT ( 'NONE',  ( -5.618132639473230050, 6.180982067432974070, -0.8581683403942765853 ) ) ;
#7522 = EDGE_CURVE ( 'NONE', #7836, #136449, #86622, .T. ) ;
#7523 = CARTESIAN_POINT ( 'NONE',  ( 2.812653035604309348, -0.5591599321941118639, -1.828790038765286452 ) ) ;
#7524 = CARTESIAN_POINT ( 'NONE',  ( -0.1102773484823885153, 6.947233595868168798, -2.798541112319170576 ) ) ;
#7525 = CARTESIAN_POINT ( 'NONE',  ( 4.014446192991796281, 1.219382930577699309, -1.220076339321971570 ) ) ;
#7526 = CARTESIAN_POINT ( 'NONE',  ( 1.885954221117658092, -2.015980662343511032, 0.05432778586660082232 ) ) ;
#7527 = CARTESIAN_POINT ( 'NONE',  ( 4.324990310505356206, 0.9834070133523404866, -2.077815080336536280 ) ) ;
#7528 = CARTESIAN_POINT ( 'NONE',  ( 3.919400689748584465, -0.1713981403653370705, 2.255992170122776308 ) ) ;
#7529 = CARTESIAN_POINT ( 'NONE',  ( 5.197925827040419833, -0.7590715138193807610, 1.964706065220876541 ) ) ;
#7530 = CARTESIAN_POINT ( 'NONE',  ( -6.672020991700860826, 7.917017590806697314, 1.082531754730549078 ) ) ;
#7531 = CARTESIAN_POINT ( 'NONE',  ( 5.096827573163183800, 1.471272477087566699, -0.9831756853606200552 ) ) ;
#7533 = CARTESIAN_POINT ( 'NONE',  ( 1.271856881794002136, 1.368814058113819732, 1.838566387026792093 ) ) ;
#7532 = CARTESIAN_POINT ( 'NONE',  ( 6.875920180786008196, 8.050936961452347163, -1.199719254218452047 ) ) ;
#7534 = CARTESIAN_POINT ( 'NONE',  ( 5.648353745280480176, -1.448853643138726000, 1.135948691490688667 ) ) ;
#7535 = CARTESIAN_POINT ( 'NONE',  ( -3.541704441667874903, 5.155074486744371853, -1.599625672291256295 ) ) ;
#7536 = VECTOR ( 'NONE', #199616, 1000.000000000000000 ) ;
#7537 = CARTESIAN_POINT ( 'NONE',  ( 5.789076383285488347, 1.657349226701849476, 1.433863557930945110 ) ) ;
#7538 = CARTESIAN_POINT ( 'NONE',  ( -2.272963308585411735, 5.803540959991587478, 0.7998128361456341429 ) ) ;
#7539 = CARTESIAN_POINT ( 'NONE',  ( -10.12536109763334835, -7.563986176625362212, 0.4645846211130850723 ) ) ;
#7540 = ADVANCED_FACE ( 'NONE', ( #18411 ), #133280, .F. ) ;
#7541 = CARTESIAN_POINT ( 'NONE',  ( 5.617656447048144486, 0.4075009240860455462, -2.029694874052537568 ) ) ;
#7542 = CARTESIAN_POINT ( 'NONE',  ( 0.1808755166769344669, 1.673851406602990366, -1.124249698880399162 ) ) ;
#7543 = CARTESIAN_POINT ( 'NONE',  ( -1.402160292154681736E-14, -0.5062499993171791779, 1.732050807568877637 ) ) ;
#7544 = CARTESIAN_POINT ( 'NONE',  ( 4.248602273900093707, 0.5149172349826669493, 1.856347322705960146 ) ) ;
#7545 = CARTESIAN_POINT ( 'NONE',  ( -8.012344526598182026E-15, 10.29687500034139447, -1.575800808251669460 ) ) ;
#7546 = CARTESIAN_POINT ( 'NONE',  ( -2.168941388506379742, 5.474256019991960542, -0.7216878364870267237 ) ) ;
#7547 = CARTESIAN_POINT ( 'NONE',  ( 1.371645089906252446, -1.908569115047893394, -1.136440837462453723 ) ) ;
#7549 = ORIENTED_EDGE ( 'NONE', *, *, #36887, .F. ) ;
#7548 = CARTESIAN_POINT ( 'NONE',  ( -2.788906526875773208E-15, 13.21875000068279427, -1.499999999999998446 ) ) ;
#7551 = DIRECTION ( 'NONE',  ( 0.000000000000000000, -1.000000000000000000, 0.000000000000000000 ) ) ;
#7550 = CARTESIAN_POINT ( 'NONE',  ( -5.153507786970285665, 5.185049637652990207, -0.7216878364870338292 ) ) ;
#7552 = CARTESIAN_POINT ( 'NONE',  ( 2.866659414285625651, 5.431854185720147221, -1.199719254218446718 ) ) ;
#7553 = CARTESIAN_POINT ( 'NONE',  ( 11.41381675112453387, 19.00000000000000000, -3.704697986577182522 ) ) ;
#7554 = CARTESIAN_POINT ( 'NONE',  ( 0.000000000000000000, 6.999999999999999112, -11.00000000000000000 ) ) ;
#7555 = CARTESIAN_POINT ( 'NONE',  ( 9.693716643646595799, 11.37205284141829686, 1.082531754730548412 ) ) ;
#7557 = CARTESIAN_POINT ( 'NONE',  ( 1.486689167417578616, 1.889818972856545987, 0.5264814339432167811 ) ) ;
#7556 = PRESENTATION_LAYER_ASSIGNMENT (  '', '', ( #107520 ) ) ;
#7558 = CARTESIAN_POINT ( 'NONE',  ( -1.201851678989727383E-14, 3.134375000341420137, 1.575800808251672791 ) ) ;
#7559 = CARTESIAN_POINT ( 'NONE',  ( 9.251576347356465391, -6.938200158402489492, -0.4350533241460284861 ) ) ;
#7560 = CARTESIAN_POINT ( 'NONE',  ( 6.566857081534598350, 1.454584517406570132, -1.316677807353151097 ) ) ;
#7561 = CARTESIAN_POINT ( 'NONE',  ( -7.995557903757128493, 10.35123685918189729, 1.599625672291295375 ) ) ;
#7562 = CARTESIAN_POINT ( 'NONE',  ( -6.534666851662457532, 6.726125536468730459, 1.040834085586084257E-14 ) ) ;
#7563 = CARTESIAN_POINT ( 'NONE',  ( 0.1985910703563107393, -2.262096406685298877, -0.05156929113746439725 ) ) ;
#7565 = VERTEX_POINT ( 'NONE', #136459 ) ;
#7564 = CARTESIAN_POINT ( 'NONE',  ( -5.045605722580076780, 9.038290442985410067, -0.7998128361456231517 ) ) ;
#7566 = CARTESIAN_POINT ( 'NONE',  ( -1.364683531249997417, 5.759375000341418804, 1.214306433183764966E-14 ) ) ;
#7567 = CARTESIAN_POINT ( 'NONE',  ( 0.9131076777311696313, -0.2804849920042574718, 1.849292663789033009 ) ) ;
#7568 = CARTESIAN_POINT ( 'NONE',  ( 0.3517064098005295292, 0.1722828621854489983, -1.725525930370126249 ) ) ;
#7569 = EDGE_CURVE ( 'NONE', #18531, #71097, #98950, .T. ) ;
#7571 = CARTESIAN_POINT ( 'NONE',  ( 3.913774547416096095, -1.127657808996849198, -1.879056921112078893 ) ) ;
#7570 = CARTESIAN_POINT ( 'NONE',  ( 0.6801582343749987825, 2.557291667008069869, -1.178068619123886718 ) ) ;
#7572 = CARTESIAN_POINT ( 'NONE',  ( 4.489522129203258771, 2.063289974401757654, -1.033470928033096037 ) ) ;
#7573 = CARTESIAN_POINT ( 'NONE',  ( 6.854767756753092023, -1.595935894175725123, 1.303543064889536751 ) ) ;
#7574 = CARTESIAN_POINT ( 'NONE',  ( 2.800647771853786772, 1.640754720439155268, 1.038516083699735582 ) ) ;
#7575 = CARTESIAN_POINT ( 'NONE',  ( -5.382223794500845315, 6.341977850748185652, -1.082531754730543971 ) ) ;
#7576 = EDGE_CURVE ( 'NONE', #105749, #160775, #119719, .T. ) ;
#7577 = CARTESIAN_POINT ( 'NONE',  ( 5.115537534566190203, 1.735013203181461350, 1.219038288318145646 ) ) ;
#7578 = CARTESIAN_POINT ( 'NONE',  ( -0.6801582343750143256, 0.3489583336747370534, -1.178068619123865846 ) ) ;
#7579 = CARTESIAN_POINT ( 'NONE',  ( 3.445935549842124690, -1.779626424299302956, -0.9480406757386842242 ) ) ;
#7580 = CARTESIAN_POINT ( 'NONE',  ( -3.429849674132936066, 6.945315686556313040, -0.7216878364870257245 ) ) ;
#7581 = CARTESIAN_POINT ( 'NONE',  ( 11.41381675112453387, 12.69999999999999929, -3.704697986577184299 ) ) ;
#7582 = CARTESIAN_POINT ( 'NONE',  ( 10.24726517383036928, 10.84956421242393887, 0.000000000000000000 ) ) ;
#7583 = CARTESIAN_POINT ( 'NONE',  ( 0.4865809202317071813, -0.2202831055867389420, -1.812292406919484344 ) ) ;
#7584 = CARTESIAN_POINT ( 'NONE',  ( -6.394605727500880299, 7.489403432619674561, -1.199719254218452047 ) ) ;
#7585 = CARTESIAN_POINT ( 'NONE',  ( -4.471156797456669274, 8.438376373666580221, -0.7998128361456361413 ) ) ;
#7586 = CARTESIAN_POINT ( 'NONE',  ( -10.39851513827935747, 3.504673854002353206, 5.419231829292963099 ) ) ;
#7587 = EDGE_LOOP ( 'NONE', ( #123989, #41831, #16770, #109642 ) ) ;
#7588 = CARTESIAN_POINT ( 'NONE',  ( 6.034070662188514511, 1.017841854155163706, -1.791927558475673754 ) ) ;
#7589 = CARTESIAN_POINT ( 'NONE',  ( -7.743115126736118015, 8.206258200713163475, 0.7216878364870317197 ) ) ;
#7590 = CARTESIAN_POINT ( 'NONE',  ( 8.122743427918724279, 8.649157885426255632, 0.7216878364870267237 ) ) ;
#7591 = CARTESIAN_POINT ( 'NONE',  ( -4.762992037102518950, 4.451245552908022596, -0.7998128361456221525 ) ) ;
#7592 = DIRECTION ( 'NONE',  ( -5.578564026256483980E-16, -1.000000000000000000, 2.168404344971008079E-15 ) ) ;
#7593 = CARTESIAN_POINT ( 'NONE',  ( 4.723309930327257433, 1.758355855194023487, 0.9934411112178792580 ) ) ;
#7595 = VERTEX_POINT ( 'NONE', #117056 ) ;
#7594 = CARTESIAN_POINT ( 'NONE',  ( 5.356174596383207032, 0.9017655805138939940, -2.030186355573161627 ) ) ;
#7597 = CARTESIAN_POINT ( 'NONE',  ( 8.188761592974039161, 10.57664116326830595, -1.443375672974063439 ) ) ;
#7596 = CARTESIAN_POINT ( 'NONE',  ( -2.830620210203090181, 6.524417021870718258, 0.000000000000000000 ) ) ;
#7598 = CARTESIAN_POINT ( 'NONE',  ( 5.819474248763732760, 7.812472595022922128, -1.599625672291262513 ) ) ;
#7599 = CARTESIAN_POINT ( 'NONE',  ( 4.205972405791720270, -2.055509729078345948, 0.1495927064073861168 ) ) ;
#7600 = CARTESIAN_POINT ( 'NONE',  ( 3.463517678199812266, -1.944071305346905643, -0.5350885120067663259 ) ) ;
#7601 = ORIENTED_EDGE ( 'NONE', *, *, #10916, .T. ) ;
#7602 = CARTESIAN_POINT ( 'NONE',  ( -15.75000000000000000, 13.79999999999999893, -0.7000000000000009548 ) ) ;
#7603 = CARTESIAN_POINT ( 'NONE',  ( 4.566398809704347528, 4.221886787610169556, -0.7998128361456211532 ) ) ;
#7604 = AXIS2_PLACEMENT_3D ( 'NONE', #94446, #62976, #101876 ) ;
#7606 = ORIENTED_EDGE ( 'NONE', *, *, #7783, .F. ) ;
#7605 = CARTESIAN_POINT ( 'NONE',  ( -8.093291352714894415, 8.406871097780989288, -0.7998128361456362523 ) ) ;
#7607 = CARTESIAN_POINT ( 'NONE',  ( 4.868750418105482147, 8.172599172502351905, -0.9747704861028365642 ) ) ;
#7608 = CARTESIAN_POINT ( 'NONE',  ( 3.638045922354939954, 0.05228986736816390590, -2.015604357568132166 ) ) ;
#7609 = CARTESIAN_POINT ( 'NONE',  ( 3.275182144284936925, 1.168729223632531733, 1.422615900182722992 ) ) ;
#7610 = CIRCLE ( 'NONE', #17959, 0.7499999999999997780 ) ;
#7611 = CARTESIAN_POINT ( 'NONE',  ( -4.207966135563093957, 7.175396087857926375, -0.9899555337401829691 ) ) ;
#7612 = CARTESIAN_POINT ( 'NONE',  ( 0.5050340691590156084, -0.7831231796689057667, -2.170891709475693876 ) ) ;
#7613 = CARTESIAN_POINT ( 'NONE',  ( 4.760848217054122422, 5.583353003765119560, -1.199719254218452047 ) ) ;
#7614 = CARTESIAN_POINT ( 'NONE',  ( 4.218171724704827596, -1.107204882465680607, -1.856345114869990320 ) ) ;
#7615 = CARTESIAN_POINT ( 'NONE',  ( -4.726989112658928072, 8.666571064744069020, 1.040834085586084257E-14 ) ) ;
#7616 = CARTESIAN_POINT ( 'NONE',  ( 3.708664688178139102, -1.738024148615105569, -1.504010254680566483 ) ) ;
#7617 = CARTESIAN_POINT ( 'NONE',  ( -0.001121896803087802687, -7.189645481337962885, -9.584290747382974374 ) ) ;
#7618 = CARTESIAN_POINT ( 'NONE',  ( 2.729206520949432946, -1.746158693253213379, 0.6715030345267187784 ) ) ;
#7619 = CARTESIAN_POINT ( 'NONE',  ( 0.3859243437699639845, -0.9334011365476569955, 1.736406649063494623 ) ) ;
#7621 = FACE_OUTER_BOUND ( 'NONE', #13282, .T. ) ;
#7620 = CARTESIAN_POINT ( 'NONE',  ( 1.364683531249990311, 4.884375000341417916, 1.214306433183764966E-14 ) ) ;
#7623 = CARTESIAN_POINT ( 'NONE',  ( 1.366164030173490973, 2.173753390890633685, -0.3800739277931909355 ) ) ;
#7622 = CARTESIAN_POINT ( 'NONE',  ( -5.225778143063529946, 8.184159369294361497, 1.199719254218452047 ) ) ;
#7624 = CARTESIAN_POINT ( 'NONE',  ( -1.854049621773892653, 4.999999999999997335, -0.7500000000000015543 ) ) ;
#7625 = CARTESIAN_POINT ( 'NONE',  ( 5.005985031943777308, 6.863401842066294556, -1.599625672291256295 ) ) ;
#7626 = CARTESIAN_POINT ( 'NONE',  ( -6.247609857798938293, 6.183299677053865295, -0.7998128361456291469 ) ) ;
#7627 = CARTESIAN_POINT ( 'NONE',  ( 11.97929049433705373, 13.88000000000000078, 0.7046979865771804130 ) ) ;
#7628 = CARTESIAN_POINT ( 'NONE',  ( 5.612177202991157188, -0.8859793764278474093, -1.761228054870385806 ) ) ;
#7629 = CARTESIAN_POINT ( 'NONE',  ( 5.707753894846095299, -0.5660891107236701858, 2.237086922978877457 ) ) ;
#7630 = CARTESIAN_POINT ( 'NONE',  ( 0.3089402658475807195, -1.578002999302514642, 1.165503548361209063 ) ) ;
#7631 = CARTESIAN_POINT ( 'NONE',  ( 2.975492196776472031, -0.2068670369150918398, 2.052202205628439913 ) ) ;
#7632 = CARTESIAN_POINT ( 'NONE',  ( 7.456621297836082185, 7.801739057004660971, 0.7216878364870317197 ) ) ;
#7633 = CARTESIAN_POINT ( 'NONE',  ( 6.156284269057003655, 9.340026192945279249, -1.199719254218452047 ) ) ;
#7634 =( BOUNDED_CURVE ( )  B_SPLINE_CURVE ( 3, ( #196803, #35354, #132900, #198905 ),
 .UNSPECIFIED., .F., .T. ) 
 B_SPLINE_CURVE_WITH_KNOTS ( ( 4, 4 ),
 ( 4.082329036743152173, 4.712388980384690562 ),
 .UNSPECIFIED. ) 
 CURVE ( )  GEOMETRIC_REPRESENTATION_ITEM ( )  RATIONAL_B_SPLINE_CURVE ( ( 1.000000000000000000, 0.9671913951488351202, 0.9671913951488351202, 1.000000000000000000 ) ) 
 REPRESENTATION_ITEM ( '' )  );
#7635 = CARTESIAN_POINT ( 'NONE',  ( 6.439759776366765998, 9.496508258194486629, 1.082531754730558626 ) ) ;
#7636 = CARTESIAN_POINT ( 'NONE',  ( 1.364683531249988535, 3.676041667008087099, 0.7879004041258500513 ) ) ;
#7637 = CARTESIAN_POINT ( 'NONE',  ( -10.06363042846879807, 3.665155796981559355, -6.455816864028870228 ) ) ;
#7638 = CARTESIAN_POINT ( 'NONE',  ( 5.965224399888476192, 6.061776009399090448, 1.040834085586084257E-14 ) ) ;
#7639 = CARTESIAN_POINT ( 'NONE',  ( 4.932167329841075976, 1.246153044254302289, 1.777787927081382779 ) ) ;
#7640 = DIRECTION ( 'NONE',  ( 0.05872483221476467591, 7.952201780260630618E-17, 0.9982742078614211811 ) ) ;
#7642 = CARTESIAN_POINT ( 'NONE',  ( 4.827609030688454261, 0.9420861819694618111, -1.581835861328761528 ) ) ;
#7641 = CARTESIAN_POINT ( 'NONE',  ( 1.224999999999989875, 0.4375000006828014265, -4.510281037539698445E-14 ) ) ;
#7644 = CARTESIAN_POINT ( 'NONE',  ( 6.620655732516645742, 3.706282450693794139, 2.340867613974298767 ) ) ;
#7643 = CARTESIAN_POINT ( 'NONE',  ( -11.84668729035137069, 11.00518580017409143, 1.399999999999998357 ) ) ;
#7645 = CARTESIAN_POINT ( 'NONE',  ( 1.930984528693787894, 3.480873151563967927, 0.3999999999999849232 ) ) ;
#7646 = CARTESIAN_POINT ( 'NONE',  ( 0.6318452133688509109, 0.9670987946563678328, -1.601024004909731513 ) ) ;
#7647 = CARTESIAN_POINT ( 'NONE',  ( 0.3513179634891601677, -1.816012830335328232, 1.349138783986586931 ) ) ;
#7648 = CARTESIAN_POINT ( 'NONE',  ( -4.902910567894817717, 6.875085367926331514, 1.448488056007392721 ) ) ;
#7649 = DIRECTION ( 'NONE',  ( -0.000000000000000000, -1.000000000000000000, -0.000000000000000000 ) ) ;
#7650 = CARTESIAN_POINT ( 'NONE',  ( 5.703612580814390043, 7.410739916031705121, 1.319003781635886163 ) ) ;
#7651 = VECTOR ( 'NONE', #194721, 1000.000000000000000 ) ;
#7652 = CARTESIAN_POINT ( 'NONE',  ( -4.950135482320926705, 6.868520377498098739, -1.443375672974066548 ) ) ;
#7653 = CARTESIAN_POINT ( 'NONE',  ( -1.286813488861823895, 3.652992958535467238, -0.4595522011843558574 ) ) ;
#7654 = CARTESIAN_POINT ( 'NONE',  ( 1.516075769870619316, 1.192070010050453099, -1.308345436402546191 ) ) ;
#7655 = CARTESIAN_POINT ( 'NONE',  ( 0.04731519813723152057, -1.748418646119804576, 0.7749314921376224685 ) ) ;
#7657 = CARTESIAN_POINT ( 'NONE',  ( 3.444859266486454352, -1.690994526066817105, -0.8999980677824627184 ) ) ;
#7656 = CARTESIAN_POINT ( 'NONE',  ( -10.47775378526269918, 11.11846759242831872, -0.7998128361456221525 ) ) ;
#7658 = CARTESIAN_POINT ( 'NONE',  ( 2.737856954955798727, 5.281584649835344258, 1.199719254218452047 ) ) ;
#7659 = CARTESIAN_POINT ( 'NONE',  ( 3.842214238857721842, -0.9727578572899638898, 1.712498773813153408 ) ) ;
#7660 = CARTESIAN_POINT ( 'NONE',  ( -0.08743476694611679312, -2.120266877281291595, -0.04547849331201780226 ) ) ;
#7661 = CARTESIAN_POINT ( 'NONE',  ( 0.3967682513765422581, -3.073437234850263433, 3.444363204092072195 ) ) ;
#7662 = CARTESIAN_POINT ( 'NONE',  ( 2.483090063216564669, 1.711211315118581711, -0.7561169667836544761 ) ) ;
#7664 = ORIENTED_EDGE ( 'NONE', *, *, #100518, .T. ) ;
#7663 = CARTESIAN_POINT ( 'NONE',  ( 6.721331452548120922, -0.1233026559786208343, 1.696394328608492819 ) ) ;
#7666 = CARTESIAN_POINT ( 'NONE',  ( 2.711267533052988732, 6.106969855296372707, -0.7216878364870267237 ) ) ;
#7665 = CARTESIAN_POINT ( 'NONE',  ( 2.315298440750997777, 1.971968782506158924, 0.9909306302095726160 ) ) ;
#7667 = CARTESIAN_POINT ( 'NONE',  ( 1.364683531249988535, 3.926041667008087543, 0.7879004041258500513 ) ) ;
#7668 = CARTESIAN_POINT ( 'NONE',  ( 6.144970055084349347, -0.2864424343173576082, -1.940704187532462210 ) ) ;
#7669 = CARTESIAN_POINT ( 'NONE',  ( 7.130698725783555680, 10.40656671580112658, 1.199719254218460707 ) ) ;
#7670 = CARTESIAN_POINT ( 'NONE',  ( -9.317477881089553549, 11.89347683273641820, 1.599625672291281386 ) ) ;
#7671 = CARTESIAN_POINT ( 'NONE',  ( 0.000000000000000000, 6.999999999999992006, 0.000000000000000000 ) ) ;
#7672 = CARTESIAN_POINT ( 'NONE',  ( -3.228813138348844536, 6.918699094715619502, 0.7998128361456341429 ) ) ;
#7673 = VECTOR ( 'NONE', #205828, 1000.000000000000000 ) ;
#7674 = VERTEX_POINT ( 'NONE', #158041 ) ;
#7675 = CARTESIAN_POINT ( 'NONE',  ( 0.000000000000000000, 13.87999999999998302, 0.000000000000000000 ) ) ;
#7676 = CARTESIAN_POINT ( 'NONE',  ( 2.102089431743926706, 0.7944251937819692966, -1.912079865474418439 ) ) ;
#7677 = CARTESIAN_POINT ( 'NONE',  ( -1.201851678989727383E-14, 3.462500000000019895, 1.732050807568877637 ) ) ;
#7678 = CARTESIAN_POINT ( 'NONE',  ( 6.322179702674084467, 6.270297829408224111, 1.040834085586084257E-14 ) ) ;
#7679 = CARTESIAN_POINT ( 'NONE',  ( 3.770049233051776749, 6.556085317605844232, 1.199719254218451159 ) ) ;
#7680 = CARTESIAN_POINT ( 'NONE',  ( 6.041668349913133618, -1.996727924239691587, 0.7141442534656232688 ) ) ;
#7681 = CARTESIAN_POINT ( 'NONE',  ( 1.499999999999990896, 8.627523663848672086, 2.580000000000004068 ) ) ;
#7682 = CARTESIAN_POINT ( 'NONE',  ( 0.6823417656249899377, 4.426041667008086655, -1.181850606188754593 ) ) ;
#7684 = CARTESIAN_POINT ( 'NONE',  ( 8.256552361042350796, 12.57646882128404187, 1.040834085586084257E-14 ) ) ;
#7683 = CARTESIAN_POINT ( 'NONE',  ( 0.1747926744264920174, 4.095712681614646300, -2.410328719303979739 ) ) ;
#7685 = EDGE_CURVE ( 'NONE', #45106, #127089, #57325, .T. ) ;
#7686 = CARTESIAN_POINT ( 'NONE',  ( 5.905624997962407363, 0.3905408587613137805, 1.977747231101577352 ) ) ;
#7687 = CARTESIAN_POINT ( 'NONE',  ( 6.122283701245728516, 1.895932525083013465, 0.2736375990538899572 ) ) ;
#7688 = CARTESIAN_POINT ( 'NONE',  ( 6.539320575229292665, 4.694805244051019066, 2.565894911293948422 ) ) ;
#7689 = CARTESIAN_POINT ( 'NONE',  ( 3.773127072069931032, 2.063069237518061705, -0.7396954945804237180 ) ) ;
#7690 = CARTESIAN_POINT ( 'NONE',  ( -1.500000000000013101, 1.452083334016150085, 0.8660254037844403729 ) ) ;
#7691 = CARTESIAN_POINT ( 'NONE',  ( 2.478646075381494285, -1.315928518397539548, 1.387899491812602637 ) ) ;
#7692 = CARTESIAN_POINT ( 'NONE',  ( -6.891622154448065807, 6.934647356477856128, 1.040834085586084257E-14 ) ) ;
#7694 = CARTESIAN_POINT ( 'NONE',  ( 6.204719021523306566, 1.975628225290576356, 0.7617523325972180848 ) ) ;
#7693 = CARTESIAN_POINT ( 'NONE',  ( 3.576974914035945030, 7.342233597957815938, -0.3073933414947004894 ) ) ;
#7695 = CARTESIAN_POINT ( 'NONE',  ( 1.364683531249997417, 9.046875000341403350, 2.602085213965210642E-15 ) ) ;
#7697 = CARTESIAN_POINT ( 'NONE',  ( -4.769436176957319695, 8.786368983084006601, 0.7998128361456281477 ) ) ;
#7696 = CARTESIAN_POINT ( 'NONE',  ( 6.005464345382193869, -2.175231771021503668, 0.2666438670960933344 ) ) ;
#7699 = ORIENTED_EDGE ( 'NONE', *, *, #116206, .F. ) ;
#7698 = CARTESIAN_POINT ( 'NONE',  ( 3.205755162861756435, -1.722880287277430478, 0.08319854473674663520 ) ) ;
#7700 = CARTESIAN_POINT ( 'NONE',  ( 6.152600690169603759, 2.097733681304454034, 0.3095894981632039689 ) ) ;
#7701 = CARTESIAN_POINT ( 'NONE',  ( 7.955937213120826357, 8.176348258262782664, 0.7998128361456481317 ) ) ;
#7702 = CARTESIAN_POINT ( 'NONE',  ( 5.657830175604453338, 5.495223381160312393, 0.7998128361456341429 ) ) ;
#7703 = AXIS2_PLACEMENT_3D ( 'NONE', #151708, #57391, #86688 ) ;
#7704 = CARTESIAN_POINT ( 'NONE',  ( 7.032125997333287692, 15.00041888085534758, 9.944927957745147040 ) ) ;
#7705 = CARTESIAN_POINT ( 'NONE',  ( 0.5550359226569913096, 1.633180182981083028, -1.086726831054436682 ) ) ;
#7706 = CARTESIAN_POINT ( 'NONE',  ( 11.44786932348528907, 9.799999999999998934, -3.303370173849653035 ) ) ;
#7707 = CARTESIAN_POINT ( 'NONE',  ( 4.819033534653518025, 7.709623992816043270, -1.199719254218452047 ) ) ;
#7708 = DIRECTION ( 'NONE',  ( 0.6095094443608750634, 0.000000000000000000, 0.7927788072564109223 ) ) ;
#7709 = ORIENTED_EDGE ( 'NONE', *, *, #85341, .T. ) ;
#7710 = CARTESIAN_POINT ( 'NONE',  ( -3.577867169202164632E-15, -5.221050908132836454, 10.98765602437503652 ) ) ;
#7711 = VERTEX_POINT ( 'NONE', #8562 ) ;
#7712 = CARTESIAN_POINT ( 'NONE',  ( 2.771877521378500742, 1.802570752484193184, -0.1794005705246705940 ) ) ;
#7713 = ORIENTED_EDGE ( 'NONE', *, *, #70219, .F. ) ;
#7714 = CARTESIAN_POINT ( 'NONE',  ( 10.16199982864259788, 11.81442020729326536, 1.199719254218452047 ) ) ;
#7715 = CARTESIAN_POINT ( 'NONE',  ( 5.598591087800349086, 5.496387455380669529, -0.7998128361456481317 ) ) ;
#7716 = CARTESIAN_POINT ( 'NONE',  ( 4.195841788199461853, 1.186545534222239962, 1.368844175430401933 ) ) ;
#7717 = CARTESIAN_POINT ( 'NONE',  ( 0.5993104169204894749, 3.417580942362360652, 0.2596433605236490028 ) ) ;
#7718 = CARTESIAN_POINT ( 'NONE',  ( 0.7500000000000006661, 9.197916667349467446, -1.299038105676657340 ) ) ;
#7719 = CARTESIAN_POINT ( 'NONE',  ( 4.911299649074239326, 6.652374229206746037, 1.248453844233877286 ) ) ;
#7720 = ADVANCED_FACE ( 'NONE', ( #74642 ), #56262, .F. ) ;
#7722 = CARTESIAN_POINT ( 'NONE',  ( -8.012344526598182026E-15, 14.54687500034139802, -1.575800808251669460 ) ) ;
#7721 = CARTESIAN_POINT ( 'NONE',  ( 4.861673063681271501, -0.4970775243713953517, 1.793344219904927206 ) ) ;
#7723 = EDGE_CURVE ( 'NONE', #45056, #7438, #135925, .T. ) ;
#7724 = CARTESIAN_POINT ( 'NONE',  ( 3.163600654563469838, 1.217692022474494262, 1.478743580268084390 ) ) ;
#7725 = CARTESIAN_POINT ( 'NONE',  ( 0.9205982885796895054, 1.684962172289593996, 0.7030880920091547859 ) ) ;
#7726 = CARTESIAN_POINT ( 'NONE',  ( -11.04445182892037813, 5.143275749589305335, -4.203165840917552742 ) ) ;
#7727 = CARTESIAN_POINT ( 'NONE',  ( 5.931307043615195340, 7.129970210930432373, 1.110187140972586306 ) ) ;
#7728 = CARTESIAN_POINT ( 'NONE',  ( 7.449721630645223414, 15.00158243878686726, 10.26201403118819044 ) ) ;
#7729 = DIRECTION ( 'NONE',  ( -0.000000000000000000, 1.000000000000000000, -0.000000000000000000 ) ) ;
#7730 = FACE_OUTER_BOUND ( 'NONE', #105285, .T. ) ;
#7731 = CARTESIAN_POINT ( 'NONE',  ( 6.155038550924139429, 9.164333495178082600, 1.082531754730558626 ) ) ;
#7732 = CARTESIAN_POINT ( 'NONE',  ( -4.548924232584923288, 5.265832011892554121, -1.199719254218446718 ) ) ;
#7733 = CARTESIAN_POINT ( 'NONE',  ( 1.886780952650327636, 1.818441039422484806, -1.031378756152110610 ) ) ;
#7734 = CARTESIAN_POINT ( 'NONE',  ( 6.493193421754636319, 1.675589973874438643, -0.9503142578028888066 ) ) ;
#7735 = CARTESIAN_POINT ( 'NONE',  ( -6.067437437315529536, 7.037430750744921859, 1.199719254218450271 ) ) ;
#7736 = CARTESIAN_POINT ( 'NONE',  ( 2.854317205943053271, 0.6132515345431619469, 1.719634925709014439 ) ) ;
#7737 = CARTESIAN_POINT ( 'NONE',  ( 3.000804911251079510, -0.6410980074830170405, -2.111705341948390657 ) ) ;
#7738 = CARTESIAN_POINT ( 'NONE',  ( 11.97185388258315086, 12.22000009279607546, 0.8311143155443657671 ) ) ;
#7739 = CARTESIAN_POINT ( 'NONE',  ( 1.388764059443419407, -1.816923020173771830, -0.5969786173363604842 ) ) ;
#7740 = ORIENTED_EDGE ( 'NONE', *, *, #78129, .T. ) ;
#7741 = CARTESIAN_POINT ( 'NONE',  ( 1.557020932125362078, 1.611981373198448253, -1.131376696270647075 ) ) ;
#7742 = CARTESIAN_POINT ( 'NONE',  ( 2.226030366740273880, 1.884328139559983573, 0.4695921692644353107 ) ) ;
#7743 = ORIENTED_EDGE ( 'NONE', *, *, #62843, .F. ) ;
#7744 = CARTESIAN_POINT ( 'NONE',  ( 10.62873463776380056, 12.30000000000000071, -3.200000000000001510 ) ) ;
#7746 = CARTESIAN_POINT ( 'NONE',  ( 6.543805726556771951, 1.282826940501276880, 1.348393317287248205 ) ) ;
#7745 = CARTESIAN_POINT ( 'NONE',  ( -5.354544322754380303, 5.211666229493680191, 0.7998128361456281477 ) ) ;
#7747 = CARTESIAN_POINT ( 'NONE',  ( 4.603875680292229156, 7.528882839386387360, 1.199719254218452047 ) ) ;
#7748 = DIRECTION ( 'NONE',  ( 5.578564026256490882E-16, 1.000000000000000000, 2.168404344971008079E-15 ) ) ;
#7749 = CARTESIAN_POINT ( 'NONE',  ( 9.236128959407556849, 11.79856975744075598, -1.599625672291262513 ) ) ;
#7750 = CARTESIAN_POINT ( 'NONE',  ( -4.450819567036169211, 8.414649604842665553, -0.7998128361456362523 ) ) ;
#7751 = CARTESIAN_POINT ( 'NONE',  ( 2.226364491882920404, 2.126620374013419301, 0.5291077681483095096 ) ) ;
#7752 = CARTESIAN_POINT ( 'NONE',  ( 3.145128448690309053, 4.692402494937224056, -1.443375672974057666 ) ) ;
#7753 = ORIENTED_EDGE ( 'NONE', *, *, #182547, .F. ) ;
#7754 = CARTESIAN_POINT ( 'NONE',  ( 6.984385409695311964, 8.177479728513226576, 1.199719254218452935 ) ) ;
#7755 = DIRECTION ( 'NONE',  ( 0.000000000000000000, 1.000000000000000000, 0.000000000000000000 ) ) ;
#7756 = CARTESIAN_POINT ( 'NONE',  ( 2.613660848560446226, -1.805822647967849193, 0.2677728182119283318 ) ) ;
#7757 = CARTESIAN_POINT ( 'NONE',  ( -9.002250809794000830, 11.52571191622492464, -1.443375672974059665 ) ) ;
#7758 = VECTOR ( 'NONE', #72110, 1000.000000000000000 ) ;
#7759 = CARTESIAN_POINT ( 'NONE',  ( -5.679622069920094773, 7.427521650927588759, -1.335666627332438683 ) ) ;
#7760 = CARTESIAN_POINT ( 'NONE',  ( 7.401861798056875053, 10.72292363345333399, -1.199719254218441611 ) ) ;
#7761 = CARTESIAN_POINT ( 'NONE',  ( 2.525899207762692722, -1.109253551102797664, -1.574925972939792418 ) ) ;
#7762 = CARTESIAN_POINT ( 'NONE',  ( 6.438335799692933570, -1.052282694883142078, 1.655480336553965648 ) ) ;
#7763 = CARTESIAN_POINT ( 'NONE',  ( 1.499999999999997113, 14.39583333333333215, -0.8660254037844378194 ) ) ;
#7764 = CARTESIAN_POINT ( 'NONE',  ( -5.768104287610143821, 8.816873204598778102, -1.199719254218440723 ) ) ;
#7765 = CARTESIAN_POINT ( 'NONE',  ( 5.183294799126148433, 4.941598775268944976, 1.040834085586084257E-14 ) ) ;
#7766 = CARTESIAN_POINT ( 'NONE',  ( -5.031484404002922517, 6.963427452793760963, 1.443375672974058777 ) ) ;
#7767 = CARTESIAN_POINT ( 'NONE',  ( 10.71502147350184231, 11.39527989537399755, 0.000000000000000000 ) ) ;
#7768 = CARTESIAN_POINT ( 'NONE',  ( -3.687454593236990430, 4.364747115940301292, 1.082531754730560403 ) ) ;
#7769 = CARTESIAN_POINT ( 'NONE',  ( 4.662978783614929235, 1.603679166536524869, -1.309313232293010776 ) ) ;
#7771 = CARTESIAN_POINT ( 'NONE',  ( -0.6823417656250003738, 3.030208333674754062, -1.181850606188749264 ) ) ;
#7770 = CARTESIAN_POINT ( 'NONE',  ( -0.07694640568740516995, -1.131669979810394633, -1.452919414246391261 ) ) ;
#7772 = VERTEX_POINT ( 'NONE', #122420 ) ;
#7773 = CARTESIAN_POINT ( 'NONE',  ( 5.028124288008245735, -1.972403190421234687, 1.180361310613570414 ) ) ;
#7774 = CARTESIAN_POINT ( 'NONE',  ( 5.666945020832160118, 9.555260257705446847, 0.7216878364870438212 ) ) ;
#7776 = LINE ( 'NONE', #173529, #53129 ) ;
#7775 = CARTESIAN_POINT ( 'NONE',  ( 4.367134877377630175, 7.148722219365612141, -1.082531754730548412 ) ) ;
#7777 = CARTESIAN_POINT ( 'NONE',  ( 0.3579208530809056543, 2.266420720034970415, -0.3425275222256763397 ) ) ;
#7778 = CARTESIAN_POINT ( 'NONE',  ( 7.821934338880105031, -6.709380320845391488, -7.553974597844388406 ) ) ;
#7779 = CARTESIAN_POINT ( 'NONE',  ( -7.370792787684826486, 8.628288336167626582, -1.199719254218452047 ) ) ;
#7780 = CARTESIAN_POINT ( 'NONE',  ( 5.279219580190475547, 1.305526251850267272, 1.437786642569781614 ) ) ;
#7781 = ORIENTED_EDGE ( 'NONE', *, *, #172733, .T. ) ;
#7782 = CARTESIAN_POINT ( 'NONE',  ( 10.19536832735223975, 10.99694392477354477, 0.000000000000000000 ) ) ;
#7783 = EDGE_CURVE ( 'NONE', #179842, #192556, #181951, .T. ) ;
#7784 = ORIENTED_EDGE ( 'NONE', *, *, #32673, .T. ) ;
#7785 = CARTESIAN_POINT ( 'NONE',  ( 6.240485052285455581, 1.095381943021833449, -1.567431287326017664 ) ) ;
#7786 = CARTESIAN_POINT ( 'NONE',  ( 1.119288186499637794, -1.683610015651057168, 0.3742365367947718124 ) ) ;
#7787 = CARTESIAN_POINT ( 'NONE',  ( 5.735564631760891707, 0.5807582108038509272, -1.931123567068816271 ) ) ;
#7789 = CARTESIAN_POINT ( 'NONE',  ( 3.511198596259284876, 6.271927390929313617, -1.052294140492317842 ) ) ;
#7788 = CARTESIAN_POINT ( 'NONE',  ( -9.504429378379839477, 11.04725468198666150, 1.199719254218462483 ) ) ;
#7790 = CARTESIAN_POINT ( 'NONE',  ( -3.285556943750000514, -1.276041666188709511, -1.896917185911906500 ) ) ;
#7792 = CARTESIAN_POINT ( 'NONE',  ( 0.6722625022101048620, -1.664400848580146919, -0.6021564899992714048 ) ) ;
#7791 = CARTESIAN_POINT ( 'NONE',  ( 2.642619598058312036, -1.737709898662170183, 1.162055570667380300 ) ) ;
#7793 = CARTESIAN_POINT ( 'NONE',  ( 6.557263107265463020, -1.238491779027944162, 1.591905563659588907 ) ) ;
#7795 = CARTESIAN_POINT ( 'NONE',  ( 4.611445210273608986, -2.248620548832699573, 0.4443846451570551692 ) ) ;
#7794 = CYLINDRICAL_SURFACE ( 'NONE', #162836, 10.75000000000000000 ) ;
#7796 = CARTESIAN_POINT ( 'NONE',  ( 2.501564275351343181, -0.6656319730054968131, -1.608207657179961947 ) ) ;
#7797 = CARTESIAN_POINT ( 'NONE',  ( 5.366329872910639232, 5.155139694684188534, 1.040834085586084257E-14 ) ) ;
#7798 = CIRCLE ( 'NONE', #211895, 2.000000000000000000 ) ;
#7799 = CARTESIAN_POINT ( 'NONE',  ( -4.886220305951450626, 4.880249661270116057, -0.6067207380149993723 ) ) ;
#7800 = CARTESIAN_POINT ( 'NONE',  ( 2.248989396041571887, -1.699371294898213369, -0.3429280648484279714 ) ) ;
#7801 = CARTESIAN_POINT ( 'NONE',  ( 1.360316468749975582, 2.317708333674725285, -0.7853790794158961308 ) ) ;
#7802 = CARTESIAN_POINT ( 'NONE',  ( 1.785388869275974955, -1.753811856250932610, 0.6230531623785877660 ) ) ;
#7803 = CARTESIAN_POINT ( 'NONE',  ( 2.207711330564741559, -1.742939566808225482, -1.294460726261867034 ) ) ;
#7804 = CARTESIAN_POINT ( 'NONE',  ( 4.852928918687680948, 7.749168607522574526, 1.199719254218462483 ) ) ;
#7805 = CARTESIAN_POINT ( 'NONE',  ( 3.397672961473942266, -1.985868886743065609, 0.3494831190506141883 ) ) ;
#7806 = CARTESIAN_POINT ( 'NONE',  ( 1.937500000000002220, 1.451031289061040841, -1.451031289061198049 ) ) ;
#7807 = CARTESIAN_POINT ( 'NONE',  ( 1.499999999999989120, 3.056250000682818158, 1.214306433183764966E-14 ) ) ;
#7808 = CARTESIAN_POINT ( 'NONE',  ( 1.500868375504460728, 1.576442195784112155, -1.106916717273882300 ) ) ;
#7809 = CARTESIAN_POINT ( 'NONE',  ( -0.6823417656250003738, 14.40104166700806232, 1.181850606188754593 ) ) ;
#7810 = CARTESIAN_POINT ( 'NONE',  ( 4.500347021246276391, -1.045864285740649935, 1.959767921951799829 ) ) ;
#7811 = ORIENTED_EDGE ( 'NONE', *, *, #40880, .F. ) ;
#7812 = CARTESIAN_POINT ( 'NONE',  ( 0.6125000000000071498, 2.395833334016134408, 1.060881119635924019 ) ) ;
#7813 = CARTESIAN_POINT ( 'NONE',  ( 0.7499999999999885647, 1.066666666666687968, -1.299038105676652899 ) ) ;
#7814 = CARTESIAN_POINT ( 'NONE',  ( 8.586391356156291010, 8.911878091804165791, 0.7998128361456481317 ) ) ;
#7815 = CARTESIAN_POINT ( 'NONE',  ( -1.364683531250000748, -0.2406249996585799189, 0.000000000000000000 ) ) ;
#7816 = CARTESIAN_POINT ( 'NONE',  ( 6.381102873985867063, -2.030373413249999093, -0.9015990085984818547 ) ) ;
#7817 = CARTESIAN_POINT ( 'NONE',  ( 4.475024536774164119, 1.792854848340214025, 0.7970393728587571447 ) ) ;
#7818 = CARTESIAN_POINT ( 'NONE',  ( 9.585251415181632595, 10.28514086057449184, 0.000000000000000000 ) ) ;
#7819 = CARTESIAN_POINT ( 'NONE',  ( -11.40591166468356654, 3.507114751586590362, 3.706005353348402753 ) ) ;
#7820 = CARTESIAN_POINT ( 'NONE',  ( 5.237693395785977479, -1.594672120175673946, -1.605097536805524916 ) ) ;
#7822 = CIRCLE ( 'NONE', #35498, 11.68000000000000149 ) ;
#7821 = CARTESIAN_POINT ( 'NONE',  ( -5.641601317062247212, 7.675230518029648508, -1.443375672974066548 ) ) ;
#7823 = CARTESIAN_POINT ( 'NONE',  ( 2.857939457652844073, -0.6493452292726099584, 1.957851178230881395 ) ) ;
#7824 = CARTESIAN_POINT ( 'NONE',  ( -5.205440912643032547, 8.160432600470439723, 1.199719254218452047 ) ) ;
#7825 = CARTESIAN_POINT ( 'NONE',  ( -1.500000000000011324, 3.202083334016150307, 0.8660254037844403729 ) ) ;
#7826 = CARTESIAN_POINT ( 'NONE',  ( -0.6823417656250246877, -1.198958332991911790, 1.181850606188755259 ) ) ;
#7827 = CARTESIAN_POINT ( 'NONE',  ( 4.762891570102392613, -1.670096840553733752, -0.8426394062573672183 ) ) ;
#7828 = CARTESIAN_POINT ( 'NONE',  ( 3.181945575597402431, 1.368952998951804556, 1.064414454346799266 ) ) ;
#7829 = CARTESIAN_POINT ( 'NONE',  ( 2.841039829263870775, 0.6241981022326682504, -1.624847995071764917 ) ) ;
#7830 = EDGE_CURVE ( 'NONE', #166540, #80549, #114491, .T. ) ;
#7831 = CARTESIAN_POINT ( 'NONE',  ( 0.2754559168597633390, 2.135984121793169432, -0.8326521888945382921 ) ) ;
#7832 = CARTESIAN_POINT ( 'NONE',  ( 0.9388347430083656686, 2.174419798330699649, 0.3756190385216377492 ) ) ;
#7833 = CARTESIAN_POINT ( 'NONE',  ( 4.353126977966869759, 0.4563941458865827805, -2.040161790709469791 ) ) ;
#7834 = CARTESIAN_POINT ( 'NONE',  ( 5.455005553751488989, 0.3768678912985870544, -1.904869181234331910 ) ) ;
#7836 = VERTEX_POINT ( 'NONE', #141820 ) ;
#7835 = CARTESIAN_POINT ( 'NONE',  ( 9.427850895902814443, 13.54474674066948481, 7.423989997610747515 ) ) ;
#7837 =( NAMED_UNIT ( * ) PLANE_ANGLE_UNIT ( ) SI_UNIT ( $, .RADIAN. ) );
#7838 = CARTESIAN_POINT ( 'NONE',  ( 0.5631252389872200004, -1.117830369828230808, 1.678006741548984770 ) ) ;
#7839 =( NAMED_UNIT ( * ) PLANE_ANGLE_UNIT ( ) SI_UNIT ( $, .RADIAN. ) );
#7840 = FILL_AREA_STYLE_COLOUR ( '', #145667 ) ;
#7842 = CARTESIAN_POINT ( 'NONE',  ( 6.504528880466823537, -1.955196382115764964, 0.4926337920100053447 ) ) ;
#7841 = CIRCLE ( 'NONE', #42522, 6.249999999999995559 ) ;
#7843 = CARTESIAN_POINT ( 'NONE',  ( -9.352427035328430449, 9.805586384171650849, 1.040834085586084257E-14 ) ) ;
#7844 = CARTESIAN_POINT ( 'NONE',  ( 5.296431564432884542, 9.330920591813708143, 1.040834085586084257E-14 ) ) ;
#7845 = CARTESIAN_POINT ( 'NONE',  ( 0.6681007961515190718, -4.204658361605604355, -0.8428154764883271088 ) ) ;
#7847 = ADVANCED_FACE ( 'NONE', ( #174298 ), #39773, .T. ) ;
#7846 = CARTESIAN_POINT ( 'NONE',  ( 4.863791234866603475, 1.805334366393744450, -0.2710410529033688842 ) ) ;
#7848 = EDGE_LOOP ( 'NONE', ( #62901, #115179, #180099, #101146, #185364 ) ) ;
#7849 = CARTESIAN_POINT ( 'NONE',  ( -4.678972410047611774, 5.591794245544547515, 1.082531754730549078 ) ) ;
#7850 = CARTESIAN_POINT ( 'NONE',  ( 0.07933194154488537597, -7.473374494045017968, -9.499668754385634628 ) ) ;
#7851 = CARTESIAN_POINT ( 'NONE',  ( 1.642778471875000035, -2.063541666188710266, -2.845375778867859751 ) ) ;
#7852 = CARTESIAN_POINT ( 'NONE',  ( -7.694415870955439551, 8.935572256658169010, 1.199719254218462483 ) ) ;
#7853 = CARTESIAN_POINT ( 'NONE',  ( 2.373312353838610722, -1.759458965525468210, -0.9916931515873882441 ) ) ;
#7854 = AXIS2_PLACEMENT_3D ( 'NONE', #135107, #88484, #101514 ) ;
#7855 = CARTESIAN_POINT ( 'NONE',  ( -4.659162064951642535, 5.464719159645540003, 1.199719254218452935 ) ) ;
#7856 = EDGE_CURVE ( 'NONE', #146171, #29173, #14129, .T. ) ;
#7857 = CARTESIAN_POINT ( 'NONE',  ( 3.361990069819278837, -1.859032935646281581, 0.08664877711485326206 ) ) ;
#7858 = CARTESIAN_POINT ( 'NONE',  ( 10.53876547652418338, 11.18964789890005918, 0.7998128361456462443 ) ) ;
#7859 = CARTESIAN_POINT ( 'NONE',  ( 4.929342268689171469, 7.989555622611471897, -1.003472558803005565 ) ) ;
#7860 = EDGE_LOOP ( 'NONE', ( #175725, #207513, #107386, #19877, #104616, #115424 ) ) ;
#7861 = CARTESIAN_POINT ( 'NONE',  ( -4.391951695823077984, 7.211361847513815704, 1.199719254218464037 ) ) ;
#7862 = CARTESIAN_POINT ( 'NONE',  ( -7.645908563102897126, 11.00764485934031889, 1.199719254218453823 ) ) ;
#7863 = CARTESIAN_POINT ( 'NONE',  ( 4.986841741376339066, -0.2268417095559888130, -1.811474396668552700 ) ) ;
#7865 = CARTESIAN_POINT ( 'NONE',  ( -4.212224785787594961, 7.548845203666256332, -0.9872405639642158892 ) ) ;
#7864 = CARTESIAN_POINT ( 'NONE',  ( -3.318713740295064163, 7.093859473644694269, 0.000000000000000000 ) ) ;
#7866 = CARTESIAN_POINT ( 'NONE',  ( 6.576141308597898139, 6.785670920958930985, -0.3094590540993913952 ) ) ;
#7867 = CARTESIAN_POINT ( 'NONE',  ( 6.837263156049210089, -1.242709075549037312, 1.588189626643407681 ) ) ;
#7868 = CARTESIAN_POINT ( 'NONE',  ( 0.5677837317836741393, -1.637140195495973671, -0.5907660828440349787 ) ) ;
#7869 = CARTESIAN_POINT ( 'NONE',  ( 3.932480676516422413, 1.235928489987428325, -1.948660470369364628 ) ) ;
#7870 = CARTESIAN_POINT ( 'NONE',  ( 5.716698046817569434, 6.698511138489155137, -1.199719254218452047 ) ) ;
#7871 = CARTESIAN_POINT ( 'NONE',  ( 0.1809649437218979473, -0.1514441579043615538, -2.027393396774066936 ) ) ;
#7872 = CARTESIAN_POINT ( 'NONE',  ( 4.821896187954575197, 8.777295985922343391, 0.7998128361456462443 ) ) ;
#7873 = CARTESIAN_POINT ( 'NONE',  ( 5.940817214068299990, 1.361788364613376601, 1.851425077211141801 ) ) ;
#7874 = CARTESIAN_POINT ( 'NONE',  ( 3.642672431166742886, 3.097590952613315185, 2.447572309175040761 ) ) ;
#7875 = CARTESIAN_POINT ( 'NONE',  ( -6.074935347375019390, 9.245119117649618801, 1.199719254218452047 ) ) ;
#7876 = EDGE_CURVE ( 'NONE', #94296, #212297, #196117, .T. ) ;
#7877 = CARTESIAN_POINT ( 'NONE',  ( 5.242975984329111050, -1.603930480038592510, 0.9624218375651683033 ) ) ;
#7879 = CARTESIAN_POINT ( 'NONE',  ( -5.307090785106547415, 5.156303768904543894, -0.7998128361456362523 ) ) ;
#7878 = CARTESIAN_POINT ( 'NONE',  ( 3.410326831400651404, -1.910418641682644969, -0.08914582809275289899 ) ) ;
#7880 = CARTESIAN_POINT ( 'NONE',  ( 4.916741810085082598, 1.523553907054091328, -1.596827639139485777 ) ) ;
#7881 = CARTESIAN_POINT ( 'NONE',  ( 4.575475080723796495, 1.571334676144776621, 1.419386683734702226 ) ) ;
#7882 = CARTESIAN_POINT ( 'NONE',  ( -0.6125000000000019318, 0.2708333340161322988, -1.060881119635941339 ) ) ;
#7883 = CARTESIAN_POINT ( 'NONE',  ( 6.983263157960366563, -0.003091553303710344557, 1.945923119799706669 ) ) ;
#7884 = CARTESIAN_POINT ( 'NONE',  ( 6.170369307550823912, 7.331757292631694511, 1.082531754730549967 ) ) ;
#7885 = CARTESIAN_POINT ( 'NONE',  ( -4.407809337774280856, 7.196175756495025055, 1.082531754730549967 ) ) ;
#7886 = CARTESIAN_POINT ( 'NONE',  ( 5.971359625099014856, -1.818578809777360972, -1.090262957368436147 ) ) ;
#7887 = CARTESIAN_POINT ( 'NONE',  ( 2.819673282491507393, -0.2271757706859862669, 2.296386706371948527 ) ) ;
#7888 = CARTESIAN_POINT ( 'NONE',  ( 4.141029529442549872, -0.1900441490861082827, -1.952618137025011746 ) ) ;
#7889 = CARTESIAN_POINT ( 'NONE',  ( 6.471393748265519719, 5.229711127717882491, -2.419999999999995932 ) ) ;
#7890 = CARTESIAN_POINT ( 'NONE',  ( 6.877782380132525297, -2.002170498271789167, 0.4952429967341723804 ) ) ;
#7891 = CARTESIAN_POINT ( 'NONE',  ( 2.399429999938675007, 5.743159399996332404, 0.000000000000000000 ) ) ;
#7892 = CARTESIAN_POINT ( 'NONE',  ( 2.878073747850912412, 6.579779482459851003, -0.7998128361456362523 ) ) ;
#7893 = ORIENTED_EDGE ( 'NONE', *, *, #126677, .T. ) ;
#7894 = CARTESIAN_POINT ( 'NONE',  ( 5.753138727196851043, 0.1435251449807967150, -2.011451301405759118 ) ) ;
#7895 = CARTESIAN_POINT ( 'NONE',  ( -9.643927338022246332, 10.14567007064778004, -0.7998128361456291469 ) ) ;
#7896 = DIRECTION ( 'NONE',  ( -0.9999980456341539536, 0.000000000000000000, -0.001977050295949901899 ) ) ;
#7897 = CARTESIAN_POINT ( 'NONE',  ( -10.44369227015510049, 5.112964020592959180, 5.232143560358710310 ) ) ;
#7898 = CARTESIAN_POINT ( 'NONE',  ( 1.745237678848761576, -0.3157848129633227807, -2.147843386395100751 ) ) ;
#7899 = CARTESIAN_POINT ( 'NONE',  ( 0.000000000000000000, 1.000000000000000888, 0.000000000000000000 ) ) ;
#7900 = CARTESIAN_POINT ( 'NONE',  ( -1.402160292154681736E-14, 0.3687500006828169363, -1.732050807568870754 ) ) ;
#7901 = CARTESIAN_POINT ( 'NONE',  ( -8.803307360466531506, 14.48154073751409499, -8.204672630978624426 ) ) ;
#7902 = CARTESIAN_POINT ( 'NONE',  ( 0.000000000000000000, 5.000000000000000888, -11.00000000000000000 ) ) ;
#7903 = CARTESIAN_POINT ( 'NONE',  ( 4.757636082118741783, 8.295611710538327799, 0.7840751985381082534 ) ) ;
#7904 = CARTESIAN_POINT ( 'NONE',  ( 1.475930922893650798, 1.225283507603215805, 1.656815433548680438 ) ) ;
#7906 = DIRECTION ( 'NONE',  ( -0.000000000000000000, 1.000000000000000000, -0.000000000000000000 ) ) ;
#7905 = CARTESIAN_POINT ( 'NONE',  ( -8.482597663644387609, 13.04811437422715414, -0.7998128361456281477 ) ) ;
#7907 = CARTESIAN_POINT ( 'NONE',  ( 1.364683531249986537, 0.3635416670080869328, 0.7879004041258500513 ) ) ;
#7908 = CARTESIAN_POINT ( 'NONE',  ( -2.482948226198870678, 5.072301959192136778, -2.419999999999995044 ) ) ;
#7909 = ORIENTED_EDGE ( 'NONE', *, *, #145707, .T. ) ;
#7910 = CARTESIAN_POINT ( 'NONE',  ( 3.106014470790594562, -0.7728303494197851231, 1.749331318715248385 ) ) ;
#7911 = AXIS2_PLACEMENT_3D ( 'NONE', #110446, #85061, #176448 ) ;
#7913 = EDGE_CURVE ( 'NONE', #139957, #62806, #110663, .T. ) ;
#7912 = CARTESIAN_POINT ( 'NONE',  ( 5.225387627957367442, -1.679756879107903833, 0.5577133518330120721 ) ) ;
#7914 = CARTESIAN_POINT ( 'NONE',  ( 5.363132282657546490, 8.414682208812571673, -1.199719254218452047 ) ) ;
#7915 = VECTOR ( 'NONE', #52190, 1000.000000000000000 ) ;
#7916 = CARTESIAN_POINT ( 'NONE',  ( -4.009460741339347045, 5.700790169694431420, -1.599625672291256295 ) ) ;
#7917 = CARTESIAN_POINT ( 'NONE',  ( -0.08802119743880723601, -1.811174541614871236, -0.04475806069833241502 ) ) ;
#7919 = CARTESIAN_POINT ( 'NONE',  ( 6.099236069963973605, -0.2290726985337887822, 1.901777391499546166 ) ) ;
#7918 = CARTESIAN_POINT ( 'NONE',  ( 1.499999999989245048, 7.854386371692742230, -3.680172642288968010 ) ) ;
#7920 = CARTESIAN_POINT ( 'NONE',  ( -0.7500000000000249800, -0.3083333333333132531, 1.299038105676659116 ) ) ;
#7921 = CARTESIAN_POINT ( 'NONE',  ( 0.3970419974134197783, 0.3524218036512065111, 2.039982198586967943 ) ) ;
#7922 = CARTESIAN_POINT ( 'NONE',  ( -1.364683531250014514, -0.6989583329919100141, -0.7879004041258359514 ) ) ;
#7923 = CARTESIAN_POINT ( 'NONE',  ( 6.121928861531041655, -1.040746078065577063, -1.554202398018275755 ) ) ;
#7924 = CARTESIAN_POINT ( 'NONE',  ( 3.369579884941567016, 1.780956498284639533, -0.4009276245297774266 ) ) ;
#7926 = CARTESIAN_POINT ( 'NONE',  ( 6.297309100973213170, 6.875137029808006339, 0.7249047842670247599 ) ) ;
#7925 = CARTESIAN_POINT ( 'NONE',  ( 6.199877634063251541, -0.7475181258948644381, 2.076568058718592624 ) ) ;
#7927 = CARTESIAN_POINT ( 'NONE',  ( -1.402160292154681736E-14, 0.4468750003414233563, -1.575800808251665908 ) ) ;
#7928 = CARTESIAN_POINT ( 'NONE',  ( 3.068856176772206457, 1.495872946324308783, -1.420456422295824916 ) ) ;
#7929 = CARTESIAN_POINT ( 'NONE',  ( -8.040148788103921973, 9.338927326664741457, 1.199719254218462483 ) ) ;
#7930 = CARTESIAN_POINT ( 'NONE',  ( 7.892817981449907982, 12.36003807833360391, 0.7998128361456462443 ) ) ;
#7931 = CARTESIAN_POINT ( 'NONE',  ( 4.976006071415387311, 5.764094157194782575, 1.199719254218462483 ) ) ;
#7932 = CARTESIAN_POINT ( 'NONE',  ( -0.05648045292897504316, -9.990726591626529540, -10.91961852020054380 ) ) ;
#7933 = CARTESIAN_POINT ( 'NONE',  ( 5.441872305809390298, 1.387781221417656141, 1.536568222347669987 ) ) ;
#7934 = CARTESIAN_POINT ( 'NONE',  ( 0.6823417656249864960, -0.5114583329919111243, -1.181850606188749264 ) ) ;
#7935 = CARTESIAN_POINT ( 'NONE',  ( 3.866626755795209203, -1.454868229745639008, 1.598846606682593929 ) ) ;
#7937 = CARTESIAN_POINT ( 'NONE',  ( 1.961309178647975715, 1.629323162926434199, 1.092499269706406428 ) ) ;
#7936 = CARTESIAN_POINT ( 'NONE',  ( 4.213539248340679499, 1.623360089863118860, 1.201376956910469307 ) ) ;
#7938 = SURFACE_STYLE_FILL_AREA ( #86005 ) ;
#7939 = ORIENTED_EDGE ( 'NONE', *, *, #181170, .T. ) ;
#7942 = CARTESIAN_POINT ( 'NONE',  ( 6.263503779833467178, 9.290876262238963790, -1.082531754730537088 ) ) ;
#7941 = CARTESIAN_POINT ( 'NONE',  ( 3.285556943750000514, -3.463541666188707957, 1.896917185911906500 ) ) ;
#7940 = CARTESIAN_POINT ( 'NONE',  ( -11.84668730067608422, 13.40000000000000036, -1.320000000000001616 ) ) ;
#7943 = CARTESIAN_POINT ( 'NONE',  ( -6.526270840131767059, 8.707344961610770540, -1.599625672291271394 ) ) ;
#7944 = CARTESIAN_POINT ( 'NONE',  ( 2.430875351317234756, -1.673853735218135741, 1.124246214196801485 ) ) ;
#7946 = CARTESIAN_POINT ( 'NONE',  ( -4.251504296082277534, 7.448701262369814557, -1.004931253576486272 ) ) ;
#7945 = CARTESIAN_POINT ( 'NONE',  ( -5.148345644887285744, 7.029489223833707001, -1.599625672291256295 ) ) ;
#7947 = DIRECTION ( 'NONE',  ( 0.7592566023653005702, 0.6507913734559639396, 0.000000000000000000 ) ) ;
#7948 = CARTESIAN_POINT ( 'NONE',  ( 5.924064563541377559, -1.897137492723115049, 0.2407653536913647030 ) ) ;
#7949 = FACE_OUTER_BOUND ( 'NONE', #105805, .T. ) ;
#7951 = CARTESIAN_POINT ( 'NONE',  ( 2.917592388753763810, -1.356314522985989646, -1.492243612603139979 ) ) ;
#7950 = CARTESIAN_POINT ( 'NONE',  ( -7.307481607641392429, 11.46921960898288972, 0.7216878364870458196 ) ) ;
#7952 = CARTESIAN_POINT ( 'NONE',  ( -1.001543065824772872E-14, 4.212500000000023448, 1.732050807568877637 ) ) ;
#7953 = CARTESIAN_POINT ( 'NONE',  ( 0.6823417656249969321, 14.58854166700806410, -1.181850606188757036 ) ) ;
#7954 = CARTESIAN_POINT ( 'NONE',  ( 6.739270712165630783, -1.537707103621160476, 0.7812997327944263271 ) ) ;
#7955 = CARTESIAN_POINT ( 'NONE',  ( 7.062871678076271920, 7.204714810702593120, -0.7998128361456341429 ) ) ;
#7956 = CARTESIAN_POINT ( 'NONE',  ( 7.443063144222396232, 11.62739806832741785, 1.040834085586084257E-14 ) ) ;
#7957 = CARTESIAN_POINT ( 'NONE',  ( 10.99953061226852746, -9.919996481109301101, -0.1022074249662192763 ) ) ;
#7958 = CARTESIAN_POINT ( 'NONE',  ( 4.587079231881330266, 1.671727914585485530, -0.8392916717318499309 ) ) ;
#7959 = CARTESIAN_POINT ( 'NONE',  ( -4.207966135563093957, 7.175396087857926375, 1.072179110320391260 ) ) ;
#7960 = CARTESIAN_POINT ( 'NONE',  ( 2.377862429009020229, -2.009158356589606953, 0.4988364127441884399 ) ) ;
#7961 = CARTESIAN_POINT ( 'NONE',  ( -6.089020385868850305, 10.11795786024005572, -0.7216878364870338292 ) ) ;
#7962 = ORIENTED_EDGE ( 'NONE', *, *, #121327, .T. ) ;
#7963 = CARTESIAN_POINT ( 'NONE',  ( 4.740510986633625024, 5.559626234941203116, -1.199719254218450271 ) ) ;
#7964 = SURFACE_STYLE_USAGE ( .BOTH. , #57801 ) ;
#7965 = CARTESIAN_POINT ( 'NONE',  ( 0.4569037783100584060, -1.553534471429316666, 0.9316326570649158256 ) ) ;
#7966 = CARTESIAN_POINT ( 'NONE',  ( 4.217995187182922656, 6.014356699837137832, 1.443375672974058777 ) ) ;
#7967 = CARTESIAN_POINT ( 'NONE',  ( -2.398572866711294438, 5.287202466803544887, -0.8077998227820496480 ) ) ;
#7968 = VERTEX_POINT ( 'NONE', #167592 ) ;
#7969 = EDGE_CURVE ( 'NONE', #77260, #204799, #204949, .T. ) ;
#7970 = CARTESIAN_POINT ( 'NONE',  ( 8.419250203962011625, 8.924806114151579095, -0.7216878364870267237 ) ) ;
#7971 = CARTESIAN_POINT ( 'NONE',  ( 8.535021395002688749, 9.916278701380017324, 1.199719254218462483 ) ) ;
#7972 = AXIS2_PLACEMENT_3D ( 'NONE', #102703, #136280, #56088 ) ;
#7973 = CARTESIAN_POINT ( 'NONE',  ( 6.204688727450275110, 1.789332568231709608, 0.6845011832880606439 ) ) ;
#7974 = CIRCLE ( 'NONE', #32258, 0.09999999999999982514 ) ;
#7975 = CARTESIAN_POINT ( 'NONE',  ( 4.690757960648231695, 5.535267711253469614, 1.082531754730560403 ) ) ;
#7976 = CARTESIAN_POINT ( 'NONE',  ( -1.177606547106018198, -3.137449485356257561, 3.183006684848862733 ) ) ;
#7977 = CARTESIAN_POINT ( 'NONE',  ( 6.827182134110199030, -0.004087946457608307438, 2.088967824442849341 ) ) ;
#7979 = EDGE_LOOP ( 'NONE', ( #85596, #131208, #146291, #20492 ) ) ;
#7978 = CARTESIAN_POINT ( 'NONE',  ( 4.528060117284240071, 5.345453560662148718, 1.082531754730560403 ) ) ;
#7980 = CARTESIAN_POINT ( 'NONE',  ( -7.917598520700757980, 9.299915031314755609, 1.082531754730558626 ) ) ;
#7981 = CARTESIAN_POINT ( 'NONE',  ( 2.940462584922590938, 2.145230175562794717, 0.2658940370997217584 ) ) ;
#7982 = CARTESIAN_POINT ( 'NONE',  ( -7.160114521792834807, 8.486460042580672436, 1.082531754730549078 ) ) ;
#7983 = CARTESIAN_POINT ( 'NONE',  ( 7.349928672384119288, 8.707909884937221179, 1.082531754730549967 ) ) ;
#7984 = CARTESIAN_POINT ( 'NONE',  ( 0.1410940620840978321, 2.031152781523197337, 0.6094965309384676733 ) ) ;
#7985 = CARTESIAN_POINT ( 'NONE',  ( 5.614214418409626539, -0.8227427255552113294, -1.629729119005427496 ) ) ;
#7986 = ADVANCED_FACE ( 'NONE', ( #210208 ), #166937, .T. ) ;
#7987 = AXIS2_PLACEMENT_3D ( 'NONE', #124601, #59503, #93101 ) ;
#7988 = CARTESIAN_POINT ( 'NONE',  ( 8.417021892111831605, 12.86188997900043596, -8.495519444159276290 ) ) ;
#7989 = CARTESIAN_POINT ( 'NONE',  ( 0.9308618464644430324, 0.1408870404581187008, 1.966361230860876441 ) ) ;
#7990 = CARTESIAN_POINT ( 'NONE',  ( 4.007995338699682719, -0.7271224857151190601, 1.768968726348684406 ) ) ;
#7991 = CARTESIAN_POINT ( 'NONE',  ( -11.43190902327450509, 9.944778717421446146, -3.649704988378223991 ) ) ;
#7992 = CARTESIAN_POINT ( 'NONE',  ( 5.072688767047404568, 1.359683132420253182, -1.425145238552152582 ) ) ;
#7993 = CARTESIAN_POINT ( 'NONE',  ( 0.6736475468689150370, -1.079418705485206020, 1.614127575861698416 ) ) ;
#7994 = ORIENTED_EDGE ( 'NONE', *, *, #110028, .T. ) ;
#7995 = CARTESIAN_POINT ( 'NONE',  ( -4.111865726694519552, 8.019203457777400956, 0.000000000000000000 ) ) ;
#7997 = CARTESIAN_POINT ( 'NONE',  ( 6.205353461901607304, 1.844339991697005798, -1.046509186232460697 ) ) ;
#7996 = CARTESIAN_POINT ( 'NONE',  ( -4.274563570058511175, 8.209017608368725405, 0.000000000000000000 ) ) ;
#7998 = CARTESIAN_POINT ( 'NONE',  ( 6.821160681006793070, 7.130644680695653825, 0.7216878364870328300 ) ) ;
#8000 = EDGE_LOOP ( 'NONE', ( #169777, #110513, #206840, #203741 ) ) ;
#7999 = CARTESIAN_POINT ( 'NONE',  ( 3.738835060935014276, 1.816739721148411757, 0.5971339541979635568 ) ) ;
#8001 = VECTOR ( 'NONE', #60877, 1000.000000000000000 ) ;
#8002 = CARTESIAN_POINT ( 'NONE',  ( 0.6752036787147744912, -2.078553970830565145, -0.7415856106591718344 ) ) ;
#8003 = CARTESIAN_POINT ( 'NONE',  ( 9.649010003797926061, 3.730310916805920751, -7.134817918383260071 ) ) ;
#8004 = CARTESIAN_POINT ( 'NONE',  ( 6.235026786510912800, 1.879206351595325231, 0.7223523585505615685 ) ) ;
#8005 = DIRECTION ( 'NONE',  ( -4.336808689941987759E-15, -0.6000000000000035305, -0.7999999999999976019 ) ) ;
#8006 = DIRECTION ( 'NONE',  ( 0.000000000000000000, 0.000000000000000000, 1.000000000000000000 ) ) ;
#8007 = CARTESIAN_POINT ( 'NONE',  ( -0.07432994781761058378, 7.051017997671326754, -3.950880802765572408 ) ) ;
#8008 = CARTESIAN_POINT ( 'NONE',  ( 2.365759603224312446, -0.4558734232973960521, 2.019384234097781672 ) ) ;
#8009 = CARTESIAN_POINT ( 'NONE',  ( -5.930802130974132780, 9.006687355190106103, -1.199719254218440723 ) ) ;
#8010 = CARTESIAN_POINT ( 'NONE',  ( -5.005744162364479166, 7.928486884654230238, -1.069363714833789558 ) ) ;
#8011 = CARTESIAN_POINT ( 'NONE',  ( -6.661184041420952440, -7.246166700180828535, 6.773376349083140013 ) ) ;
#8012 = CARTESIAN_POINT ( 'NONE',  ( 6.498435699651741615, 6.475929825882159818, -0.7998128361456281477 ) ) ;
#8013 = DIRECTION ( 'NONE',  ( 0.000000000000000000, 0.000000000000000000, -1.000000000000000000 ) ) ;
#8014 = CARTESIAN_POINT ( 'NONE',  ( 5.126391479742934187, 6.113783160189109722, -1.082531754730548412 ) ) ;
#8015 = CARTESIAN_POINT ( 'NONE',  ( 8.103009739377979415, -6.893137084989842123, -7.439168848974011539 ) ) ;
#8016 = DIRECTION ( 'NONE',  ( 0.000000000000000000, 0.000000000000000000, -1.000000000000000000 ) ) ;
#8017 = CARTESIAN_POINT ( 'NONE',  ( 1.364683531249996529, 11.52604166700806410, 0.7879004041258405033 ) ) ;
#8019 = CARTESIAN_POINT ( 'NONE',  ( -6.954406449166956605, 7.078172043641714595, -0.7998128361456362523 ) ) ;
#8018 = CARTESIAN_POINT ( 'NONE',  ( 6.825078400183526739, 3.708013787890347857, 2.270222819304415385 ) ) ;
#8020 = CARTESIAN_POINT ( 'NONE',  ( 4.764171500175623741, 1.615563337074712225, -0.6307657835151522230 ) ) ;
#8021 = CARTESIAN_POINT ( 'NONE',  ( -2.916975605234527702, 6.554888639415577423, 1.040834085586084257E-14 ) ) ;
#8022 = CARTESIAN_POINT ( 'NONE',  ( 2.430607852509637290, -1.277051959022021066, 1.629327859714514659 ) ) ;
#8023 =( BOUNDED_SURFACE ( )  B_SPLINE_SURFACE ( 3, 2, ( 
 ( #117061, #31505, #14145 ),
 ( #163637, #178826, #15219 ),
 ( #162571, #80239, #212351 ),
 ( #183059, #52006, #148449 ) ),
 .UNSPECIFIED., .F., .F., .T. ) 
 B_SPLINE_SURFACE_WITH_KNOTS ( ( 4, 4 ),
 ( 3, 3 ),
 ( 4.712388980384689674, 6.283185307179586232 ),
 ( 0.000000000000000000, 1.000000000000000000 ),
 .UNSPECIFIED. ) 
 GEOMETRIC_REPRESENTATION_ITEM ( )  RATIONAL_B_SPLINE_SURFACE ( (
 ( 1.000000000000000000, 0.7071067811865294761, 1.000000000000000000),
 ( 1.000000000000000000, 0.8014503788335076706, 1.000000000000000000),
 ( 1.000000000000000000, 0.8676977444974025566, 1.000000000000000000),
 ( 1.000000000000000000, 0.8661919058288510831, 1.000000000000000000) ) ) 
 REPRESENTATION_ITEM ( '' )  SURFACE ( )  );
#8024 = CARTESIAN_POINT ( 'NONE',  ( 3.902059883959855924, -1.090250183479730461, -1.814828101457645060 ) ) ;
#8025 = CARTESIAN_POINT ( 'NONE',  ( 7.935599982700328958, 8.152621489438862667, 0.7998128361456481317 ) ) ;
#8026 = CARTESIAN_POINT ( 'NONE',  ( 1.364683531249990311, 3.384375000341416140, 1.214306433183764966E-14 ) ) ;
#8027 = CARTESIAN_POINT ( 'NONE',  ( 1.516386633922983895, 0.7932475597272764523, 1.802804710252394527 ) ) ;
#8028 = CARTESIAN_POINT ( 'NONE',  ( 5.430717995911492402, 6.471920874811950775, 1.294091166901890633 ) ) ;
#8030 = CARTESIAN_POINT ( 'NONE',  ( -0.1757481403069499348, -0.8193859263425256056, -1.726394157293544840 ) ) ;
#8029 = CARTESIAN_POINT ( 'NONE',  ( 3.475000000000000533, -1.254166666666665098, 2.006292185433948827 ) ) ;
#8031 = CARTESIAN_POINT ( 'NONE',  ( 3.468945898361298408, 0.05672114714776231581, -2.291715584554415930 ) ) ;
#8032 = CARTESIAN_POINT ( 'NONE',  ( 1.541335573940459058, -1.321205422867760548, -1.260230113935792318 ) ) ;
#8033 = CARTESIAN_POINT ( 'NONE',  ( 5.727393547130178675, 5.646656991265468939, 0.000000000000000000 ) ) ;
#8034 = CARTESIAN_POINT ( 'NONE',  ( 6.439759776366775768, 7.575769829591800786, 1.082531754730558626 ) ) ;
#8035 = CARTESIAN_POINT ( 'NONE',  ( -6.821723845970312894, 11.11042825360738284, 0.000000000000000000 ) ) ;
#8036 = CARTESIAN_POINT ( 'NONE',  ( 2.689700119490782360, 1.910346015757229177, -0.6353908363993918673 ) ) ;
#8037 =( BOUNDED_CURVE ( )  B_SPLINE_CURVE ( 2, ( #98377, #62661, #29114, #128819, #79984, #65836, #213169 ),
 .UNSPECIFIED., .F., .T. ) 
 B_SPLINE_CURVE_WITH_KNOTS ( ( 3, 2, 2, 3 ),
 ( 0.3500000000000000888, 0.3583333333333335036, 0.3666666666666668628, 0.3750000000000002776 ),
 .UNSPECIFIED. ) 
 CURVE ( )  GEOMETRIC_REPRESENTATION_ITEM ( )  RATIONAL_B_SPLINE_CURVE ( ( 0.9999999999999982236, 0.8660254037844404840, 1.000000000000000000, 0.8660254037844387076, 1.000000000000000000, 0.8660254037844342667, 1.000000000000004441 ) ) 
 REPRESENTATION_ITEM ( '' )  );
#8038 = CARTESIAN_POINT ( 'NONE',  ( 3.221486639279776298, 0.2924833653642990861, -1.939731193138781951 ) ) ;
#8039 = CARTESIAN_POINT ( 'NONE',  ( -8.345207244411405156, 9.694828859023472134, 1.199719254218462483 ) ) ;
#8040 = B_SPLINE_CURVE_WITH_KNOTS ( 'NONE', 3,
 ( #68659, #200791, #64426, #31933, #34048, #66514, #151022, #166183, #149950, #52442 ),
 .UNSPECIFIED., .F., .F.,
 ( 4, 1, 1, 1, 1, 1, 1, 4 ),
 ( 0.000000000000000000, 0.09487947018404768729, 0.1878442364269655440, 0.2584026419818104547, 0.3617053504666527530, 0.5211417612611924932, 0.7337075935910832847, 1.000000000000000000 ),
 .UNSPECIFIED. ) ;
#8041 = CARTESIAN_POINT ( 'NONE',  ( -5.551173829791513192, 8.563787670477010394, 1.199719254218452047 ) ) ;
#8042 = FACE_OUTER_BOUND ( 'NONE', #164786, .T. ) ;
#8044 = CARTESIAN_POINT ( 'NONE',  ( 4.715556530927702106, -1.735345248271908947, 0.3467660769565800161 ) ) ;
#8043 = CARTESIAN_POINT ( 'NONE',  ( 5.999963288868293887, -0.7514721766869683073, -1.951089947871258001 ) ) ;
#8045 = CARTESIAN_POINT ( 'NONE',  ( -1.225000000000042277, 2.229166666666690499, -0.7072540797573217963 ) ) ;
#8046 = CARTESIAN_POINT ( 'NONE',  ( 1.148660753082946240, -1.725648174752218100, 1.350667304935410318 ) ) ;
#8047 = CARTESIAN_POINT ( 'NONE',  ( 5.894438200647534210, 1.418812651433436933, -1.007543873543685020 ) ) ;
#8048 = B_SPLINE_CURVE_WITH_KNOTS ( 'NONE', 3,
 ( #16100, #150411, #909, #66978 ),
 .UNSPECIFIED., .F., .F.,
 ( 4, 4 ),
 ( 0.000000000000000000, 0.0003450753579246922977 ),
 .UNSPECIFIED. ) ;
#8049 = CARTESIAN_POINT ( 'NONE',  ( 7.456094412511537151, 10.78619501698377370, 1.199719254218460707 ) ) ;
#8050 = CARTESIAN_POINT ( 'NONE',  ( 0.2331713839410758660, 6.947498546895825022, -2.548426565200106353 ) ) ;
#8051 = CARTESIAN_POINT ( 'NONE',  ( 0.1580921841808444750, -0.5169658338281759580, -2.248806653996893168 ) ) ;
#8052 =( BOUNDED_SURFACE ( )  B_SPLINE_SURFACE ( 3, 3, ( 
 ( #148817, #127606, #118512, #50254, #82744, #389, #183441, #116374, #184496, #67529, #16658, #33992, #167203, #100066, #68604, #99010, #198608, #83803, #35045, #165067, #182362, #1464, #166129, #17715, #149896, #114264, #61439, #81680, #2529, #143806, #200734, #180260, #133672, #15593, #18792, #134727, #209804, #199676, #51319, #52384, #49198, #66461, #36115, #117447, #147766, #101116, #77686, #31884, #97961, #84875, #196508, #213782, #102198, #115319, #150964, #48150, #168264, #164019, #65405, #131552, #197554, #181309, #132602, #32936, #205008, #85950, #89170, #106518, #56655, #54516, #71803, #154157, #188777, #189843, #123878, #4658, #135777, #37193, #53442, #137914, #70730, #40415, #55582, #24129, #5724, #187703, #140063, #171464, #90231, #185564, #88085, #69671, #57720, #203934, #21975, #121737, #122818, #39331, #41490, #6803, #170386, #105428, #172544, #23052, #7880, #38265, #155222, #72879, #156296, #104342, #138987, #73968, #206085, #107602, #19865, #119580, #3593, #20915, #152025, #201800, #103269, #169331, #87010, #153082, #136843, #202868, #120660, #186639, #193039, #79304, #142201, #63052, #42563, #207159, #144353, #12160, #59848, #173633, #91309, #127077, #29495, #161636, #141150, #143282, #208216, #43626, #45760, #78231, #195193, #160552, #109741, #44693, #13230, #145420, #108665, #210355, #77160, #111878, #8960, #126000, #58782, #110801, #27343, #209273, #176805, #158423, #75035, #10023, #177882, #174696, #211420, #191959, #28421, #25204, #129218, #157366, #175752, #93446, #159484, #60918, #95587, #61994, #94514, #128150, #46829, #124936, #11084, #190899, #26270, #92387, #76098, #194110, #31632, #100872, #81438, #83554, #96649, #33741, #116124, #182111, #64126, #163767, #196258, #212484, #178955, #146466, #213537, #117193, #16408, #198360, #132357, #115067, #144, #149636, #97709, #181063, #200489, #30569, #1217, #162703, #67280, #147516, #15345, #51069, #34798, #18549, #133419, #166959, #150717, #84625, #82488, #50000, #65160, #99819, #130269, #112942, #32681, #197308, #114015, #66210, #148575, #98760, #131316, #199425, #14275, #165884, #183192, #2277, #48948, #164817, #17470, #68353, #134486, #80370, #47905, #180010, #69420, #85690, #104089, #36935, #6554, #87834, #56400, #38017, #5475, #172289, #203684, #122561, #3350, #120405, #101948, #89983, #21724, #54269, #186381, #154969, #153905, #156033, #39083, #202619, #71555, #138731, #137663, #40154, #70480, #170138, #55332, #72632, #136595, #121483, #187455, #105169, #171207, #22801, #151778, #35873, #53196, #188523, #118262, #23877, #135526, #88915, #201550, #204749, #106267, #184246, #7623, #73709, #139806, #103018, #52134, #168014, #19618, #119327, #185313, #169073, #20672, #4408, #86762, #152832, #95324, #205834, #9770, #75843, #141950, #93190, #61727, #28158, #60651, #109487, #79033, #107343, #207962, #27082, #26014, #59588, #157112, #41236, #76896, #108415, #57467, #174438, #125745, #159222, #189590, #45496, #43365, #111612, #42301, #94254, #160293, #127895, #191706, #74785, #175495, #10822, #177623, #143020, #209015, #24947, #8701, #176548, #140885, #161373, #58528, #126814, #110546, #92125, #91051, #144092, #11896, #173365, #206897, #77970, #158177, #29232, #123626, #192770, #44429, #193846, #124683, #210088, #12955, #190641, #65948, #34545, #953 ),
 ( #132096, #212218, #50802, #198106, #113746, #30300, #18282, #100615, #14013, #178687, #115863, #49735, #31368, #145149, #62779, #98492, #67019, #133155, #112677, #114801, #179750, #15083, #17210, #181848, #166691, #33485, #81174, #164556, #199157, #116930, #80099, #99557, #48685, #83286, #194919, #97444, #96385, #82226, #213285, #180800, #16141, #130010, #46557, #196001, #149371, #163500, #162437, #146203, #148317, #47635, #211155, #147253, #64911, #32425, #128942, #182929, #197048, #63854, #131060, #165622, #214316, #6295, #102761, #167753, #168816, #152567, #56142, #21467, #37756, #118004, #35607, #55077, #101684, #188260, #151518, #87576, #203421, #119066, #183993, #22548, #187196, #200231, #85433, #121226, #52932, #122303, #150456, #135277, #70225, #72369, #3086, #20420, #138470, #84365, #5216, #39901, #154714, #86502, #38824, #201291, #169877, #103829, #153646, #71291, #137403, #104908, #51881, #170948, #88654, #69157, #204492, #106010, #185048, #19353, #172032, #2017, #36672, #4154, #68086, #134221, #136336, #202356, #54006, #120144, #186122, #11646, #205573, #207716, #206644, #108160, #110295, #76649, #45243, #10575, #174188, #43120, #77717, #143839, #107088, #142764, #141705, #176303, #73443, #58277, #123371, #175245, #91872, #59339, #109235, #8443, #139547, #74531, #27906, #173110, #209834, #190391, #92934, #23624, #127636, #89733, #42049, #25759, #157928, #125493, #94003, #60397, #158978, #191455, #111360, #57211, #9521, #26831, #124433, #24690, #160042, #155781, #61471, #189338, #208769, #90794, #193601, #7366, #40977, #126561, #156858, #192521, #140631, #44175, #75593, #180551, #178438, #32172, #177365, #128695, #62533, #181602, #28979, #96133, #165363, #145957, #148066, #161113, #98249, #164305, #15894, #194663, #13772, #46308, #112424, #95064, #210906, #63606, #33230, #80923, #48443, #196801, #179501, #64665, #214072, #162186, #31123, #50548, #12699, #65698, #78777, #131845, #211967, #79848, #115607, #99313, #83037, #197855, #16956, #691, #149112, #147012, #114558, #129761, #81978, #30044, #144898, #97197, #47382, #195745, #130811, #213036, #163250, #113495, #49486, #14832, #66757, #132898, #198902, #151260, #168561, #36419, #71034, #72106, #6036, #101428, #18023, #133972, #150198, #20160, #167499, #137147, #152317, #120968, #102497, #69966, #22279, #53750, #186938, #67825, #184793, #166432, #154458, #86247, #118808, #3894, #4956, #136076, #138216, #103572, #52677, #202092, #203173, #119883, #104646, #135020, #185861, #37496, #54819, #201034, #169630, #21213, #87317, #153384, #38570, #1768, #100362, #170692, #88390, #204229, #116670, #182668, #34290, #84109, #199980, #51627, #117752, #183742, #35352, #19097, #85176, #2832, #68901, #25509, #191198, #91617, #9265, #75336, #89471, #39629, #56953, #192265, #122039, #176053, #155524, #157667, #205315, #208513, #43926, #188003, #141453, #142505, #173936, #40717, #42865, #159784, #59079, #123125, #125239, #55881, #7105, #73179, #60147, #105736, #189084, #110041, #24423, #26577, #171765, #108973, #174991, #92680, #139285, #106823, #172852, #90536, #23361, #156601, #8192, #126305, #207460, #158725, #10322, #58015, #76396, #27647, #74277, #124179, #143582, #140370, #93746, #206388, #11386, #190142, #41796, #77464, #107909, #115368, #98011, #49247, #32984, #197603, #179248 ),
 ( #128448, #180309, #61221, #64420, #81733, #31929, #29798, #47128, #129513, #164067, #165115, #99060, #194415, #111102, #12452, #28724, #113244, #46057, #15645, #30872, #213834, #195493, #162999, #181360, #146767, #65452, #160860, #63354, #44993, #16707, #96951, #79600, #131601, #209575, #130565, #82792, #127377, #211718, #147815, #112179, #80676, #14580, #196555, #212784, #48197, #193349, #177108, #114310, #94810, #62288, #78529, #144647, #178183, #210662, #95882, #161937, #13530, #145719, #119631, #201850, #35097, #148866, #66509, #102245, #4707, #136895, #116422, #118562, #117497, #18841, #20965, #53494, #173399, #135826, #84927, #168318, #202922, #54566, #17765, #185615, #52436, #87062, #198655, #183488, #34042, #85999, #2583, #184546, #19914, #133722, #50304, #199728, #153134, #83853, #120714, #101168, #3643, #440, #41268, #132651, #167255, #151015, #68653, #36166, #70781, #37248, #69722, #152073, #24981, #182413, #134776, #103318, #200784, #169380, #100115, #166177, #186687, #51374, #149943, #107376, #1513, #67577, #74818, #145184, #143053, #211190, #141982, #127930, #45530, #12991, #109518, #174469, #175525, #159253, #62815, #28193, #44464, #124715, #42335, #61762, #108450, #194955, #158211, #94288, #210121, #125779, #190674, #29265, #193882, #206932, #92158, #111645, #59623, #128976, #157144, #207996, #76927, #79066, #9800, #46591, #161407, #93221, #177657, #191741, #176582, #110580, #160328, #11932, #78004, #95357, #58561, #144128, #112709, #75875, #178721, #91084, #43396, #26045, #8737, #140918, #27115, #10854, #209048, #60684, #126848, #192805, #162472, #198138, #100648, #18317, #212253, #214349, #213317, #114832, #116963, #83317, #51912, #17242, #180831, #49769, #84400, #150488, #113780, #149404, #148349, #182961, #80132, #64941, #130042, #181880, #98526, #65979, #115895, #15117, #146236, #81206, #34576, #179782, #2047, #197081, #99589, #30336, #134254, #96421, #48718, #32456, #164587, #132129, #166725, #67051, #165655, #33517, #118035, #63887, #16173, #986, #131092, #82257, #196035, #47669, #133188, #147285, #14045, #199188, #50836, #68118, #31402, #200261, #97476, #163532, #20451, #6328, #138501, #106040, #202389, #52961, #54041, #37788, #155813, #121255, #137438, #3118, #135309, #154745, #201322, #73477, #36705, #187227, #88685, #4185, #69188, #122335, #72401, #85463, #185081, #204524, #152600, #7397, #35638, #86534, #169911, #172063, #102792, #120178, #23656, #184021, #104940, #89767, #101717, #139578, #119099, #5248, #168848, #188292, #205604, #167788, #55109, #56173, #87608, #70256, #170980, #57242, #38856, #136370, #22579, #19384, #186154, #103862, #39932, #151549, #21500, #153678, #71323, #203454, #107118, #44206, #126590, #192551, #74561, #174218, #206676, #8474, #189366, #156887, #9551, #127667, #26860, #208801, #142795, #125526, #10604, #94033, #42079, #191485, #210935, #41008, #11674, #173141, #160071, #157958, #25792, #61501, #45271, #29009, #77749, #177395, #161144, #111392, #92964, #60430, #75626, #110326, #140661, #123402, #43153, #207743, #124463, #76680, #159010, #109266, #108193, #143870, #24722, #176331, #209863, #193629, #141736, #175274, #27938, #95095, #78805, #12731, #91902, #90824, #58307, #190422, #144928, #59369, #16985, #98276, #66787, #48471, #15923, #182700, #214099, #132927, #13803 ),
 ( #34318, #128724, #113525, #114588, #198932, #129792, #147040, #50578, #62560, #197884, #166463, #116700, #64693, #165390, #179532, #148096, #99341, #131875, #180579, #150229, #178465, #130838, #164334, #97224, #80949, #79875, #112452, #65728, #31151, #194696, #163277, #196830, #82006, #46338, #100393, #32199, #18056, #14859, #83065, #149142, #84142, #213063, #145985, #49513, #115633, #30075, #181628, #33258, #96166, #211996, #722, #63637, #162216, #195772, #47411, #121003, #36455, #35386, #154492, #104680, #117785, #2864, #186971, #184825, #188036, #67857, #52710, #202126, #138251, #68933, #86280, #204264, #1800, #137184, #105775, #72142, #3928, #170728, #118842, #87353, #21246, #71067, #4990, #169662, #38602, #183775, #153421, #203206, #135056, #122075, #54852, #102531, #101461, #89506, #171801, #85208, #167532, #22315, #88427, #168593, #134006, #200011, #6071, #55916, #39665, #19129, #185893, #20193, #152352, #23393, #51661, #151293, #201068, #69997, #136110, #53786, #119918, #37528, #103605, #59112, #27681, #205350, #190176, #40752, #92710, #9299, #125271, #175022, #140406, #56985, #206425, #93778, #24460, #61251, #107942, #10352, #155560, #45025, #7143, #173968, #25542, #91650, #42896, #11419, #123158, #172886, #189118, #207492, #58048, #110070, #191233, #159816, #141486, #109005, #127408, #158757, #77495, #106859, #75371, #90574, #193381, #26610, #157702, #76427, #43955, #142537, #111136, #208543, #60178, #126336, #143614, #192295, #209607, #176083, #177139, #28756, #73214, #139320, #156634, #8226, #74310, #124214, #41830, #210691, #12486, #112208, #213864, #94840, #197635, #128479, #163031, #178216, #81765, #65487, #78560, #212817, #147846, #96982, #161968, #48230, #115400, #130598, #29831, #196587, #160891, #95915, #13559, #131634, #144679, #211750, #181393, #47161, #49280, #194447, #98043, #31960, #164096, #79630, #129542, #145749, #63388, #62320, #195524, #14613, #33017, #114342, #15679, #46091, #113277, #179282, #30907, #80710, #146800, #64453, #180338, #176764, #140028, #44651, #108633, #190865, #12118, #210316, #194069, #28380, #128111, #111841, #61952, #43589, #159445, #174660, #11043, #91275, #73934, #142164, #158390, #75004, #27302, #191924, #76065, #207124, #110765, #206053, #143245, #160515, #94474, #26235, #125968, #208181, #78192, #29458, #177845, #58749, #57688, #209234, #144318, #45722, #92352, #109707, #59813, #95547, #161599, #123845, #124902, #189806, #157332, #107566, #175711, #42528, #41458, #93408, #173601, #77122, #60879, #25173, #127038, #8923, #141113, #192998, #9987, #174647, #157319, #172499, #76052, #11030, #24085, #123833, #93394, #91260, #94461, #188732, #173588, #108619, #44638, #189795, #207109, #110753, #122772, #43576, #12106, #192984, #124888, #77108, #25158, #208168, #142153, #191912, #125956, #59799, #159431, #90190, #109694, #175698, #41446, #28366, #27288, #8910, #7832, #210298, #78176, #206041, #156253, #143232, #209222, #74990, #40370, #106472, #60864, #176751, #160501, #73923, #92339, #141098, #58736, #127026, #144304, #140016, #57675, #190852, #107554, #42513, #26223, #158381, #9974, #179955, #148522, #111825, #96595, #161584, #213483, #130212, #31578, #81378, #46774, #177827, #112888, #88, #145368, #182056, #14218, #131263, #61938, #165830, #128096, #80313, #146413, #212426, #163711 ),
 ( #29444, #147462, #64068, #62992, #15293, #97652, #196205, #195138, #32626, #194054, #197250, #66153, #98703, #162645, #113958, #47847, #16352, #17414, #83498, #178900, #95535, #79250, #13171, #65107, #30514, #82432, #48889, #132298, #115009, #181006, #33686, #164762, #198305, #211367, #49945, #129161, #116066, #99763, #149580, #45706, #104038, #36881, #39032, #202564, #151725, #169022, #87779, #20620, #203630, #19565, #119272, #4359, #170084, #85639, #185257, #136544, #102964, #86708, #152777, #34744, #199369, #2223, #137614, #67228, #121430, #100817, #70428, #150661, #153853, #55282, #133362, #54216, #5424, #120354, #200434, #186331, #105116, #37965, #68298, #21671, #1164, #166902, #18495, #71503, #51015, #134431, #187400, #184195, #171156, #117136, #22746, #88864, #183139, #84573, #52081, #118208, #35818, #101894, #167959, #3297, #69365, #135474, #201495, #53142, #157062, #42249, #125693, #73657, #8650, #28107, #6503, #43317, #72578, #191652, #189537, #57409, #93134, #76847, #60601, #109435, #208969, #192720, #142966, #124634, #25964, #41185, #92069, #172240, #154919, #74729, #138679, #205781, #140834, #126760, #7572, #24893, #44374, #204698, #75794, #110497, #10773, #206847, #175441, #123575, #158127, #174386, #9718, #141902, #108362, #27026, #56348, #207912, #59533, #139757, #176496, #159173, #107292, #40102, #122510, #188470, #23828, #106214, #89933, #155984, #173314, #90999, #58479, #190592, #164510, #82178, #61675, #63803, #62728, #178637, #180753, #147209, #115817, #81124, #30249, #113699, #148272, #214271, #177567, #213234, #212169, #32380, #144038, #128889, #193795, #31319, #162389, #129961, #179703, #78981, #210035, #145100, #98446, #29180, #65904, #46504, #163452, #94202, #198060, #160242, #112627, #96333, #13966, #195949, #16094, #131011, #15032, #47585, #181804, #127843, #80050, #97396, #194870, #146153, #45444, #111558, #64866, #211104, #11842, #197003, #48638, #114756, #77919, #132050, #49689, #95269, #161317, #12901, #202311, #169837, #51836, #116882, #117954, #101640, #5172, #185004, #201246, #66972, #199108, #4109, #50753, #137361, #100571, #36628, #85387, #68035, #83240, #52887, #136290, #149325, #34497, #70178, #1972, #71245, #183949, #35559, #167706, #135233, #103786, #53960, #102713, #151471, #121179, #903, #19308, #69111, #134175, #3042, #182881, #133111, #119022, #150405, #33437, #200183, #168770, #20375, #17166, #87533, #86460, #153600, #84319, #120098, #186076, #21424, #152524, #166644, #37710, #203378, #55031, #99514, #165571, #18235, #138424, #157878, #204443, #76600, #39852, #190341, #24639, #7317, #22496, #140585, #75544, #88608, #188212, #9471, #155732, #158930, #38777, #23574, #173059, #109184, #105958, #57161, #175197, #187148, #108111, #142713, #43071, #189287, #141653, #89683, #58225, #206596, #42003, #174138, #124383, #207665, #154663, #25712, #91821, #171982, #92885, #59284, #73395, #72318, #60348, #208722, #56097, #6249, #125443, #191404, #139498, #104859, #170903, #26780, #10526, #122253, #205526, #156809, #123324, #40929, #107033, #90749, #8396, #74480, #213772, #148807, #117434, #35032, #212724, #33980, #32923, #1451, #179188, #164005, #14521, #66450, #197542, #98999, #376, #114252, #30812, #180248, #67516, #64363, #101106, #81668, #198594, #126511, #18779, #192473, #133661 ),
 ( #47067, #100055, #15581, #31872, #199662, #51308, #167192, #17704, #183431, #84865, #150953, #165054, #132592, #147754, #50241, #146708, #113184, #49187, #65394, #130509, #82731, #16646, #131540, #48139, #166119, #96891, #116361, #2517, #83791, #115306, #181296, #182351, #149886, #162940, #80615, #97951, #196496, #85939, #102186, #120649, #53429, #23042, #104329, #72869, #54505, #21964, #188765, #5713, #138975, #19852, #136831, #118502, #135766, #55572, #172534, #89158, #171453, #170377, #106507, #121726, #4648, #88072, #155211, #154145, #56642, #86998, #186628, #71790, #6792, #153071, #38255, #203924, #137905, #187691, #39320, #168253, #52373, #69658, #204998, #134716, #40405, #152012, #105415, #3583, #122806, #24118, #200722, #90221, #156285, #68590, #119566, #184484, #36101, #201789, #185553, #37182, #103257, #169318, #20902, #70718, #202857, #141137, #210340, #190886, #193025, #206074, #143269, #11069, #77148, #173622, #58770, #91298, #107590, #73957, #41479, #108655, #44677, #42552, #59835, #142188, #176791, #177869, #111864, #207147, #123865, #25194, #157356, #125988, #124925, #28406, #43611, #12144, #208202, #175736, #128133, #159471, #78217, #8945, #76086, #57708, #75025, #209259, #29481, #94500, #110789, #109729, #45746, #60904, #158410, #27329, #160538, #93431, #61979, #26257, #191945, #127063, #144340, #92373, #194097, #95572, #7869, #140049, #189830, #174683, #10010, #162687, #83541, #13215, #67266, #46813, #197292, #96633, #99805, #149622, #79288, #32665, #33727, #65145, #146452, #148563, #51055, #164802, #14262, #16394, #161622, #112927, #178940, #165870, #145406, #80353, #1204, #130253, #132341, #211406, #82473, #129, #66197, #30554, #212467, #64111, #196244, #63036, #195180, #47887, #17456, #131301, #98744, #181049, #163751, #48933, #198347, #114000, #15330, #34784, #129203, #49987, #179995, #116105, #31619, #97693, #133405, #199410, #117179, #182096, #183180, #81420, #147501, #115051, #213522, #201535, #186368, #118251, #100859, #169060, #185297, #101934, #54256, #4395, #103004, #19606, #71541, #166943, #170123, #187442, #36921, #120393, #39069, #38003, #88902, #119311, #70466, #104075, #203671, #20657, #136583, #21709, #202603, #87820, #153892, #134472, #84613, #168000, #22785, #18536, #6541, #200476, #5461, #35856, #105156, #154955, #150702, #137651, #171195, #55320, #85678, #121471, #204736, #72619, #151766, #138718, #2264, #52122, #184232, #56385, #68340, #3335, #122548, #69406, #188510, #135513, #53183, #86747, #152819, #205820, #91038, #123613, #139793, #106253, #73695, #140873, #44415, #158164, #125731, #59574, #42289, #141938, #10810, #173353, #108400, #127882, #172277, #143005, #23864, #76885, #74769, #157098, #192758, #176535, #160280, #209003, #94241, #77958, #28146, #9756, #191692, #206884, #43352, #57453, #40140, #174424, #124671, #41224, #207951, #75831, #26000, #24935, #60640, #89971, #109472, #126802, #110534, #58516, #92109, #175480, #11882, #210075, #144079, #8687, #156023, #189576, #107329, #27067, #190628, #61714, #93175, #7612, #159209, #147242, #213269, #45483, #145137, #83270, #46544, #197035, #31355, #14001, #29219, #64898, #82211, #95309, #194906, #148304, #33469, #17196, #181834, #163485, #131045, #80085, #48670, #211143, #193832, #47620, #63840, #112664, #114787, #97430, #195987 ),
 ( #30287, #16127, #214303, #115849, #212204, #62765, #129997, #113732, #165606, #180787, #178672, #32410, #98476, #111599, #128929, #149358, #96372, #164542, #15067, #146189, #161358, #65934, #132083, #12941, #162424, #198093, #179738, #940, #177607, #81159, #49720, #99543, #67005, #79020, #55060, #133142, #53992, #22531, #203408, #135264, #21455, #35592, #4140, #152553, #202340, #136322, #86489, #103817, #34531, #70210, #120131, #200215, #38807, #186108, #101670, #18270, #6280, #88640, #2004, #166678, #169864, #37741, #19339, #199142, #50786, #87563, #121211, #187180, #100602, #102745, #167740, #3071, #5204, #153631, #154697, #71277, #69143, #137391, #104893, #170932, #68070, #116915, #36660, #182915, #84352, #85418, #150442, #134206, #201278, #168801, #51867, #117988, #183981, #151502, #52919, #119050, #185035, #20406, #141690, #72352, #176290, #73429, #25746, #190377, #74516, #205557, #43108, #138456, #207704, #158967, #109223, #107069, #124418, #206631, #26817, #27894, #93989, #57197, #188244, #89715, #105995, #42036, #123357, #92921, #108149, #76636, #75581, #155766, #10561, #7350, #142750, #23607, #140619, #122287, #139532, #59324, #160030, #208759, #175233, #174175, #110281, #125481, #8428, #91858, #60384, #157914, #126548, #90781, #9509, #191443, #192509, #156844, #44161, #204475, #56128, #39885, #172016, #189322, #40962, #173094, #24675, #58262, #131834, #111347, #47368, #161100, #164292, #214058, #77705, #97183, #98237, #129748, #210894, #213019, #115594, #14819, #12688, #80911, #11632, #177352, #28966, #15881, #143825, #144887, #65686, #194652, #196789, #209822, #147001, #64654, #130795, #95049, #62521, #78764, #128683, #61458, #45232, #112411, #81965, #195733, #163237, #31110, #13759, #113481, #48430, #46296, #79835, #99301, #127624, #114545, #193588, #180537, #178423, #30032, #148052, #197841, #49474, #32160, #181588, #33217, #96118, #179488, #162173, #145944, #211955, #63593, #165348, #19083, #35336, #86233, #168549, #20148, #116658, #1754, #34276, #50535, #16943, #198889, #51614, #169615, #68888, #36406, #184780, #167488, #52664, #136063, #84098, #85164, #38554, #83022, #53736, #149097, #202076, #199966, #67811, #103556, #87301, #71017, #119868, #4941, #203159, #153370, #135007, #102485, #117737, #152304, #182656, #678, #151248, #101415, #166415, #118793, #201020, #2816, #150185, #185847, #66744, #3880, #37479, #21199, #183728, #69951, #137130, #54804, #120952, #186923, #133958, #132886, #100349, #18008, #156582, #89454, #59061, #140353, #108954, #107891, #187989, #42847, #39614, #174974, #55865, #172834, #154441, #171747, #91599, #208493, #125220, #207442, #206371, #142486, #157650, #40701, #57998, #191179, #124162, #92663, #123108, #8176, #173919, #26556, #189066, #74260, #25492, #190124, #41778, #9248, #138201, #88374, #105718, #158707, #170678, #10304, #204213, #75319, #23343, #76378, #60128, #22265, #141436, #126286, #192245, #155506, #104631, #6021, #72091, #7088, #122021, #73161, #139267, #205297, #56935, #106805, #24405, #90519, #12431, #14561, #27627, #78511, #80658, #93727, #179228, #47108, #113224, #209556, #94791, #127359, #143563, #110021, #77445, #144628, #48181, #161918, #129494, #63335, #46039, #145699, #146749, #177089, #112160, #131585, #176035, #212767, #159767, #64403, #210643, #160839, #196538 ) ),
 .UNSPECIFIED., .T., .F., .F. ) 
 B_SPLINE_SURFACE_WITH_KNOTS ( ( 4, 3, 4 ),
 ( 4, 1, 1, 1, 1, 1, 1, 1, 1, 1, 1, 1, 1, 1, 1, 1, 1, 1, 1, 1, 1, 1, 1, 1, 1, 1, 1, 1, 1, 1, 1, 1, 1, 1, 1, 1, 1, 1, 1, 1, 1, 1, 1, 1, 1, 1, 1, 1, 1, 1, 1, 1, 1, 1, 1, 1, 1, 1, 1, 1, 1, 1, 1, 1, 1, 1, 1, 1, 1, 1, 1, 1, 1, 1, 1, 1, 1, 1, 1, 1, 1, 1, 1, 1, 1, 1, 1, 1, 1, 1, 1, 1, 1, 1, 1, 1, 1, 1, 1, 1, 1, 1, 1, 1, 1, 1, 1, 1, 1, 1, 1, 1, 1, 1, 1, 1, 1, 1, 1, 1, 1, 1, 1, 1, 1, 1, 1, 1, 1, 1, 1, 1, 1, 1, 1, 1, 1, 1, 1, 1, 1, 1, 1, 1, 1, 1, 1, 1, 1, 1, 1, 1, 1, 1, 1, 1, 1, 1, 1, 1, 1, 1, 1, 1, 1, 1, 1, 1, 1, 1, 1, 1, 1, 1, 1, 1, 1, 1, 1, 1, 1, 1, 1, 1, 1, 1, 1, 1, 1, 1, 1, 1, 1, 1, 1, 1, 1, 1, 1, 1, 1, 1, 1, 1, 1, 1, 1, 1, 1, 1, 1, 1, 1, 1, 1, 1, 1, 1, 1, 1, 1, 1, 1, 1, 1, 1, 1, 1, 1, 1, 1, 1, 1, 1, 1, 1, 1, 1, 1, 1, 1, 1, 1, 1, 1, 1, 1, 1, 1, 1, 1, 1, 1, 1, 1, 1, 1, 1, 1, 1, 1, 1, 1, 1, 1, 1, 1, 1, 1, 1, 1, 1, 1, 1, 1, 1, 1, 1, 1, 1, 1, 1, 1, 1, 1, 1, 1, 1, 1, 1, 1, 1, 1, 1, 1, 1, 1, 1, 1, 1, 1, 1, 1, 1, 1, 1, 1, 1, 1, 1, 1, 1, 1, 1, 1, 1, 1, 1, 1, 1, 1, 1, 1, 1, 1, 1, 1, 1, 1, 1, 1, 1, 1, 1, 1, 1, 1, 1, 1, 1, 1, 1, 1, 1, 1, 1, 1, 1, 1, 1, 1, 1, 1, 1, 1, 1, 1, 1, 1, 1, 1, 1, 1, 1, 1, 1, 1, 1, 1, 1, 1, 1, 1, 1, 1, 1, 1, 1, 1, 1, 1, 1, 1, 1, 4 ),
 ( 0.000000000000000000, 0.5000000000000000000, 1.000000000000000000 ),
 ( 0.000000000000000000, 0.002599878613971510263, 0.005208762566300055921, 0.007813076245110234588, 0.01041697056762492211, 0.01302017924898362516, 0.01562522799165661294, 0.01822895742955179393, 0.02083332403451576206, 0.02343772221867868391, 0.02604143078293654281, 0.02864626161639613477, 0.03124961764961396021, 0.03385452714844047750, 0.03645799780571232912, 0.03906266225314121432, 0.04166671052383312535, 0.04427076094224517699, 0.04687542278318937439, 0.04947889361195772356, 0.05208380280015859759, 0.05468715921365963767, 0.05729198803509916865, 0.05989568673917144287, 0.06250009379223495087, 0.06510449848632135494, 0.06770819839843210397, 0.07031302545632363288, 0.07291638160390327694, 0.07552129054917994244, 0.07812475961953217751, 0.08072942239586503033, 0.08333346963797970408, 0.08593751866472883194, 0.08854217935802578821, 0.09114564884740632145, 0.09375055680876714925, 0.09635391199924973893, 0.09895873945611717570, 0.1015624370353711836, 0.1041668426700886191, 0.1067712463110160465, 0.1093749448896196713, 0.1119797708301935452, 0.1145831257515418783, 0.1171880334468678037, 0.1197915013940491491, 0.1223961628153678316, 0.1250002090321265524, 0.1276042567216372492, 0.1302089163955687523, 0.1328123846563000476, 0.1354172914881497103, 0.1380206455552074885, 0.1406254717515977581, 0.1432291683081768907, 0.1458335726268597532, 0.1484379753169847160, 0.1510416726638619811, 0.1536464975900906083, 0.1562498513865758776, 0.1588547579349887939, 0.1614582248604825021, 0.1640628850295551278, 0.1666669303230295940, 0.1692709767774011609, 0.1718756355346959253, 0.1744791026682601387, 0.1770840084736199360, 0.1796873615186004858, 0.1822921865574477218, 0.1848958821930496710, 0.1875002852981585977, 0.1901046871399069693, 0.1927083833567690418, 0.1953132073715553307, 0.1979165601445126987, 0.2005214656490191816, 0.2031249316542690642, 0.2057295906738217384, 0.2083336351460475244, 0.2109376804673406547, 0.2135423384106908962, 0.2161458045185324639, 0.2187507094003866837, 0.2213540615246011867, 0.2239588855088016361, 0.2265625803250888304, 0.2291669823190463362, 0.2317713834148095453, 0.2343750786033309830, 0.2369799018095430365, 0.2395832536602726381, 0.2421881582238437913, 0.2447916234102597566, 0.2473962813829825302, 0.2500003251359625422, 0.2526043694262022354, 0.2552090266582678346, 0.2578124918417971090, 0.2604173959030967600, 0.2630207472078238129, 0.2656255702402394725, 0.2682292643388430320, 0.2708336653240377978, 0.2734380657761767419, 0.2760417600379992398, 0.2786465825384744077, 0.2812499335682448476, 0.2838548372938197173, 0.2864583017627815864, 0.2890629587913320364, 0.2916670019270400371, 0.2942710452882197347, 0.2968757019116316509, 0.2994791662722288139, 0.3020840696158954564, 0.3046874202023847622, 0.3072922423858477359, 0.3098959358683710530, 0.3125003359471613118, 0.3151047358580104651, 0.3177084292947467969, 0.3203132511922952008, 0.3229166015023476888, 0.3255215044928377321, 0.3281249683456989308, 0.3307296245327063788, 0.3333336671530912065, 0.3359377096871765112, 0.3385423658045411677, 0.3411458294435600336, 0.3437507321724898035, 0.3463540821419661686, 0.3489589035792820537, 0.3515625965473047621, 0.3541669958220223235, 0.3567713952938928457, 0.3593750880071304721, 0.3619799094045394461, 0.3645832590960911834, 0.3671881614543835437, 0.3697916247924753486, 0.3723962802405443862, 0.3750003224475334518, 0.3776043642564660408, 0.3802090199703688222, 0.3828124829891406122, 0.3854173852062082184, 0.3880207346598750218, 0.3906255554538268782, 0.3932292480089087938, 0.3958336465818629857, 0.3984380457170473289, 0.4010417378083525053, 0.4036465588083897882, 0.4062499079826380477, 0.4088548098116001062, 0.4114582727362346981, 0.4140629275479489335, 0.4166669694434522730, 0.4192710106291533956, 0.4218756660421624782, 0.4244791285419997062, 0.4270840303500617607, 0.4296873793891050619, 0.4322921996424575197, 0.4348958918861421385, 0.4375002898596233591, 0.4401046887603987101, 0.4427083803313200949, 0.4453132010367379379, 0.4479165497948640051, 0.4505214511973463787, 0.4531249138098211726, 0.4557295680877478938, 0.4583336097736617210, 0.4609376504380365280, 0.4635423056527069874, 0.4661457677349071238, 0.4687506692368063055, 0.4713540179623986193, 0.4739588377779012651, 0.4765625298117197040, 0.4791669272880037522, 0.4817713260566358624, 0.4843750172087082362, 0.4869798377222476216, 0.4895831861654201811, 0.4921880872442612742, 0.4947915496458628049, 0.4973962034925555886, 0.5000002450707665691, 0.5026042853157074441, 0.5052089404345847523, 0.5078124022004342208, 0.5104173034990032720, 0.5130206520123070657, 0.5156254714926987726, 0.5182291634181735995, 0.5208335604995248946, 0.5234379592382720769, 0.5260416500730202838, 0.5286464704974140894, 0.5312498187267931105, 0.5338547195848227789, 0.5364581818768299204, 0.5390628353948335727, 0.5416668769672219330, 0.5442709168946127107, 0.5468755720202369552, 0.5494790335710144635, 0.5520839347690799093, 0.5546872831712518215, 0.5572921024192640793, 0.5598957943379132551, 0.5625001911265891108, 0.5651045899377058479, 0.5677082805566486812, 0.5703131009946261765, 0.5729164491113668545, 0.5755213498514099024, 0.5781248121350983649, 0.5807294654269519185, 0.5833335070953961088, 0.5859375468071157389, 0.5885422020420250089, 0.5911456634790059894, 0.5937505646793920233, 0.5963539130715860281, 0.5989587321899475514, 0.6015624242032879820, 0.6041668208015419372, 0.6067712197872831004, 0.6093749102919370220, 0.6119797308462270324, 0.6145830789514836745, 0.6171879796763642956, 0.6197914420530098445, 0.6223960952212510556, 0.6250001370876311357, 0.6276041766855571247, 0.6302088321322918407, 0.6328122935567517260, 0.6354171948622837629, 0.6380205433456558328, 0.6406253624370956690, 0.6432290546466469250, 0.6458334511567334069, 0.6484378504193577530, 0.6510415409112403351, 0.6536463616845760161, 0.6562497098795055939, 0.6588546106920506462, 0.6614580732629331550, 0.6640627264101022220, 0.6666667685763031370, 0.6692708081623160998, 0.6718754639234225667, 0.6744789254366408970, 0.6770838269501499029, 0.6796871756258610064, 0.6822919947931124218, 0.6848956873004010681, 0.6875000838245786117, 0.6901044834663523364, 0.6927081740469867022, 0.6953129951421085364, 0.6979163435278744609, 0.7005212445309179081, 0.7031247073973251327, 0.7057293606259679164, 0.7083334031938842701, 0.7109374428698714832, 0.7135420990479055536, 0.7161455607511696408, 0.7187504625754957965, 0.7213538115447158949, 0.7239586308905210377, 0.7265623237970838533, 0.7291667204376187650, 0.7317711205608201652, 0.7343748113317387638, 0.7369796328513985584, 0.7395829815291747877, 0.7421878828255610294, 0.7447913460887924941, 0.7473959995014650692, 0.7500000425730045661, 0.7526040824408628538, 0.7552087391383944803, 0.7578122011330034047, 0.7604171033709996586, 0.7630204527349119248, 0.7656252723620247114, 0.7682289657694127971, 0.7708333626285834850, 0.7734377633355060677, 0.7760414543982535607, 0.7786462764452187768, 0.7812496255161931469, 0.7838545272087811266, 0.7864579909701516769, 0.7890626446694239959, 0.7916666883465109938, 0.7942707285081521684, 0.7968753858277685120, 0.7994788482150362308, 0.8020837509695725176, 0.8046871008293766669, 0.8072919208405671121, 0.8098956148503495545, 0.8125000120304503026, 0.8151044134234068927, 0.8177081048795449281, 0.8203129275566022338, 0.8229162771219805661, 0.8255211793136476572, 0.8281246436744912343, 0.8307292977629509023, 0.8333333421475307423, 0.8359373827048843797, 0.8385420407491936956, 0.8411455036304537058, 0.8437504070044209437, 0.8463537574613370085, 0.8489585779593948889, 0.8515622726731627568, 0.8541666702765071673, 0.8567710724578335713, 0.8593747644089445581, 0.8619795878189033811, 0.8645829379799131464, 0.8671878407735589267, 0.8697913058352330085, 0.8723959604154888359, 0.8750000056095312839, 0.8776040466645483873, 0.8802087055361843548, 0.8828121690127931354, 0.8854170731091063340, 0.8880204242643787715, 0.8906252453521178447, 0.8932289408714879642, 0.8958333390004131758, 0.8984377420724726226, 0.9010414346201626179, 0.9036462588658594752, 0.9062496097237539017, 0.9088545132223035949, 0.9114579790861923048, 0.9140626342608790811, 0.9166666803663815477, 0.9192707220210388774, 0.9218753818226663732, 0.9244788459960084914, 0.9270837509176034219, 0.9296871028724987829, 0.9322919246527909820, 0.9348956210794385768, 0.9375000198362011261, 0.9401044239011964176, 0.9427081171475072408, 0.9453129423329229564, 0.9479162939871883520, 0.9505211982878988275, 0.9531246650646376661, 0.9557293209618126228, 0.9583333680330715643, 0.9609374102905526849, 0.9635420713365114853, 0.9661455366701111602, 0.9687504417289087844, 0.9713537931426093897, 0.9739586182492501187, 0.9765623229037746489, 0.9791667147516245340, 0.9817710778420317697, 0.9843748014325267581, 0.9869798465897002826, 0.9895830499482988207, 0.9921869381715581193, 0.9947912477285243416, 0.9974001254724073062, 1.000000000000000000 ),
 .UNSPECIFIED. ) 
 GEOMETRIC_REPRESENTATION_ITEM ( )  RATIONAL_B_SPLINE_SURFACE ( (
 ( 1.000000000000000222, 1.000000000000000222, 1.000000000000000222, 1.000000000000000222, 1.000000000000000444, 1.000000000000000000, 1.000000000000000666, 0.9999999999999997780, 1.000000000000000444, 1.000000000000000000, 1.000000000000000444, 1.000000000000000444, 1.000000000000000000, 1.000000000000000444, 1.000000000000000000, 1.000000000000000444, 1.000000000000000222, 1.000000000000000222, 1.000000000000000222, 1.000000000000000444, 1.000000000000000444, 1.000000000000000000, 1.000000000000000444, 1.000000000000000000, 1.000000000000000222, 1.000000000000000222, 1.000000000000000444, 1.000000000000000222, 1.000000000000000222, 1.000000000000000444, 1.000000000000000444, 1.000000000000000444, 1.000000000000000000, 1.000000000000000444, 1.000000000000000444, 1.000000000000000000, 1.000000000000000444, 1.000000000000000444, 1.000000000000000000, 1.000000000000000444, 1.000000000000000444, 1.000000000000000000, 1.000000000000000222, 1.000000000000000444, 1.000000000000000222, 1.000000000000000222, 1.000000000000000000, 1.000000000000000444, 1.000000000000000222, 1.000000000000000222, 1.000000000000000222, 1.000000000000000222, 1.000000000000000222, 1.000000000000000222, 1.000000000000000444, 1.000000000000000000, 1.000000000000000444, 0.9999999999999997780, 1.000000000000000666, 1.000000000000000444, 1.000000000000000444, 1.000000000000000000, 1.000000000000000444, 1.000000000000000222, 1.000000000000000222, 1.000000000000000444, 1.000000000000000222, 1.000000000000000444, 1.000000000000000000, 1.000000000000000444, 1.000000000000000222, 1.000000000000000444, 1.000000000000000444, 1.000000000000000222, 1.000000000000000222, 1.000000000000000222, 1.000000000000000444, 0.9999999999999997780, 1.000000000000000444, 1.000000000000000000, 1.000000000000000444, 1.000000000000000000, 1.000000000000000444, 0.9999999999999997780, 1.000000000000000444, 0.9999999999999997780, 1.000000000000000444, 1.000000000000000222, 1.000000000000000444, 1.000000000000000000, 1.000000000000000222, 1.000000000000000444, 1.000000000000000444, 1.000000000000000222, 1.000000000000000444, 1.000000000000000444, 1.000000000000000222, 1.000000000000000222, 1.000000000000000222, 1.000000000000000222, 1.000000000000000000, 1.000000000000000222, 1.000000000000000222, 1.000000000000000222, 1.000000000000000444, 1.000000000000000000, 1.000000000000000444, 0.9999999999999997780, 1.000000000000000666, 1.000000000000000222, 1.000000000000000444, 1.000000000000000000, 1.000000000000000444, 1.000000000000000222, 1.000000000000000222, 1.000000000000000444, 1.000000000000000000, 1.000000000000000000, 1.000000000000000444, 1.000000000000000000, 1.000000000000000444, 1.000000000000000000, 1.000000000000000444, 1.000000000000000222, 1.000000000000000444, 1.000000000000000222, 1.000000000000000444, 1.000000000000000222, 1.000000000000000444, 1.000000000000000000, 1.000000000000000444, 1.000000000000000222, 1.000000000000000444, 1.000000000000000000, 1.000000000000000444, 1.000000000000000000, 1.000000000000000444, 1.000000000000000000, 1.000000000000000444, 1.000000000000000222, 1.000000000000000444, 1.000000000000000222, 1.000000000000000444, 0.9999999999999997780, 1.000000000000000444, 1.000000000000000000, 1.000000000000000444, 1.000000000000000222, 1.000000000000000222, 1.000000000000000222, 1.000000000000000222, 1.000000000000000444, 0.9999999999999997780, 1.000000000000000444, 1.000000000000000000, 1.000000000000000000, 1.000000000000000222, 1.000000000000000222, 1.000000000000000666, 0.9999999999999997780, 1.000000000000000000, 1.000000000000000444, 1.000000000000000222, 1.000000000000000444, 1.000000000000000000, 1.000000000000000222, 1.000000000000000444, 1.000000000000000222, 1.000000000000000000, 1.000000000000000444, 1.000000000000000222, 1.000000000000000222, 1.000000000000000444, 1.000000000000000222, 1.000000000000000000, 1.000000000000000444, 1.000000000000000000, 1.000000000000000444, 1.000000000000000222, 1.000000000000000222, 1.000000000000000444, 0.9999999999999997780, 1.000000000000000444, 0.9999999999999997780, 1.000000000000000444, 1.000000000000000222, 1.000000000000000444, 1.000000000000000222, 1.000000000000000222, 1.000000000000000444, 1.000000000000000000, 1.000000000000000222, 1.000000000000000444, 1.000000000000000000, 1.000000000000000444, 1.000000000000000000, 1.000000000000000222, 1.000000000000000444, 1.000000000000000000, 1.000000000000000444, 0.9999999999999997780, 1.000000000000000444, 1.000000000000000222, 1.000000000000000444, 1.000000000000000000, 1.000000000000000000, 1.000000000000000444, 1.000000000000000000, 1.000000000000000222, 1.000000000000000444, 1.000000000000000222, 1.000000000000000444, 1.000000000000000222, 1.000000000000000444, 1.000000000000000444, 1.000000000000000444, 1.000000000000000000, 1.000000000000000444, 1.000000000000000222, 1.000000000000000444, 1.000000000000000222, 1.000000000000000000, 1.000000000000000222, 1.000000000000000444, 1.000000000000000222, 1.000000000000000444, 1.000000000000000000, 1.000000000000000222, 1.000000000000000000, 1.000000000000000444, 1.000000000000000000, 1.000000000000000444, 1.000000000000000444, 1.000000000000000444, 1.000000000000000444, 1.000000000000000000, 1.000000000000000222, 1.000000000000000444, 1.000000000000000000, 1.000000000000000444, 1.000000000000000444, 1.000000000000000444, 1.000000000000000222, 1.000000000000000222, 1.000000000000000222, 0.9999999999999997780, 1.000000000000000444, 1.000000000000000222, 1.000000000000000222, 1.000000000000000000, 1.000000000000000444, 1.000000000000000000, 1.000000000000000444, 1.000000000000000000, 1.000000000000000000, 1.000000000000000666, 1.000000000000000000, 1.000000000000000444, 1.000000000000000000, 1.000000000000000444, 1.000000000000000222, 0.9999999999999997780, 1.000000000000000444, 1.000000000000000000, 1.000000000000000444, 1.000000000000000222, 1.000000000000000444, 1.000000000000000222, 1.000000000000000222, 1.000000000000000444, 1.000000000000000000, 1.000000000000000222, 1.000000000000000444, 1.000000000000000222, 1.000000000000000000, 1.000000000000000444, 0.9999999999999997780, 1.000000000000000444, 1.000000000000000222, 1.000000000000000222, 1.000000000000000222, 1.000000000000000000, 1.000000000000000444, 1.000000000000000222, 1.000000000000000666, 0.9999999999999997780, 1.000000000000000444, 1.000000000000000222, 1.000000000000000000, 1.000000000000000222, 1.000000000000000444, 1.000000000000000222, 1.000000000000000000, 1.000000000000000444, 1.000000000000000222, 1.000000000000000444, 1.000000000000000000, 1.000000000000000444, 1.000000000000000222, 1.000000000000000444, 1.000000000000000222, 1.000000000000000222, 1.000000000000000444, 1.000000000000000222, 1.000000000000000444, 1.000000000000000000, 1.000000000000000444, 1.000000000000000222, 1.000000000000000222, 1.000000000000000000, 1.000000000000000666, 0.9999999999999997780, 1.000000000000000444, 1.000000000000000222, 1.000000000000000444, 1.000000000000000222, 1.000000000000000444, 1.000000000000000000, 1.000000000000000444, 1.000000000000000222, 1.000000000000000222, 1.000000000000000444, 1.000000000000000222, 1.000000000000000444, 1.000000000000000000, 1.000000000000000444, 1.000000000000000444, 0.9999999999999997780, 1.000000000000000444, 1.000000000000000000, 1.000000000000000444, 1.000000000000000444, 1.000000000000000222, 1.000000000000000000, 1.000000000000000444, 1.000000000000000222, 1.000000000000000444, 1.000000000000000000, 1.000000000000000444, 1.000000000000000222, 1.000000000000000444, 1.000000000000000222, 1.000000000000000444, 1.000000000000000222, 1.000000000000000222, 1.000000000000000444, 1.000000000000000444, 1.000000000000000000, 1.000000000000000444, 0.9999999999999997780, 1.000000000000000444, 1.000000000000000222, 1.000000000000000222, 1.000000000000000222, 1.000000000000000444, 1.000000000000000222, 1.000000000000000222, 1.000000000000000444, 1.000000000000000000, 1.000000000000000444, 1.000000000000000000, 1.000000000000000444, 1.000000000000000222, 1.000000000000000000, 1.000000000000000222, 1.000000000000000444, 1.000000000000000000, 1.000000000000000444, 1.000000000000000000, 1.000000000000000444, 1.000000000000000444, 1.000000000000000000, 1.000000000000000444, 1.000000000000000000, 1.000000000000000444, 1.000000000000000000, 1.000000000000000444, 1.000000000000000000, 1.000000000000000444, 1.000000000000000000, 1.000000000000000444, 1.000000000000000000, 1.000000000000000444, 1.000000000000000222, 1.000000000000000222, 1.000000000000000222, 1.000000000000000222),
 ( 0.3333333333333334259, 0.3333333333333334259, 0.3333333333333333703, 0.3333333333333334259, 0.3333333333333334814, 0.3333333333333333148, 0.3333333333333335924, 0.3333333333333333148, 0.3333333333333334259, 0.3333333333333333703, 0.3333333333333334814, 0.3333333333333334814, 0.3333333333333333148, 0.3333333333333334814, 0.3333333333333333703, 0.3333333333333334259, 0.3333333333333334259, 0.3333333333333333703, 0.3333333333333334814, 0.3333333333333334259, 0.3333333333333335369, 0.3333333333333333148, 0.3333333333333335369, 0.3333333333333333703, 0.3333333333333333703, 0.3333333333333334259, 0.3333333333333334814, 0.3333333333333334814, 0.3333333333333333148, 0.3333333333333335369, 0.3333333333333335924, 0.3333333333333334259, 0.3333333333333333703, 0.3333333333333335369, 0.3333333333333334259, 0.3333333333333334259, 0.3333333333333334814, 0.3333333333333335369, 0.3333333333333333703, 0.3333333333333334259, 0.3333333333333335369, 0.3333333333333333148, 0.3333333333333334259, 0.3333333333333335369, 0.3333333333333333703, 0.3333333333333334259, 0.3333333333333333703, 0.3333333333333335369, 0.3333333333333333703, 0.3333333333333334814, 0.3333333333333333703, 0.3333333333333334259, 0.3333333333333333703, 0.3333333333333333703, 0.3333333333333334259, 0.3333333333333333703, 0.3333333333333334259, 0.3333333333333333148, 0.3333333333333336479, 0.3333333333333334259, 0.3333333333333334814, 0.3333333333333333703, 0.3333333333333335369, 0.3333333333333334259, 0.3333333333333334259, 0.3333333333333334259, 0.3333333333333334259, 0.3333333333333333703, 0.3333333333333333703, 0.3333333333333335369, 0.3333333333333333703, 0.3333333333333335369, 0.3333333333333334259, 0.3333333333333333703, 0.3333333333333334814, 0.3333333333333334259, 0.3333333333333333703, 0.3333333333333333148, 0.3333333333333335369, 0.3333333333333333703, 0.3333333333333335369, 0.3333333333333333703, 0.3333333333333334814, 0.3333333333333333703, 0.3333333333333334259, 0.3333333333333333148, 0.3333333333333335369, 0.3333333333333333703, 0.3333333333333334814, 0.3333333333333333148, 0.3333333333333334814, 0.3333333333333334259, 0.3333333333333335369, 0.3333333333333334259, 0.3333333333333334814, 0.3333333333333334259, 0.3333333333333334259, 0.3333333333333334259, 0.3333333333333334259, 0.3333333333333333703, 0.3333333333333333703, 0.3333333333333334814, 0.3333333333333333703, 0.3333333333333333703, 0.3333333333333335369, 0.3333333333333332593, 0.3333333333333335369, 0.3333333333333332593, 0.3333333333333335924, 0.3333333333333334259, 0.3333333333333334814, 0.3333333333333333703, 0.3333333333333334814, 0.3333333333333334259, 0.3333333333333334259, 0.3333333333333334814, 0.3333333333333333703, 0.3333333333333333703, 0.3333333333333334814, 0.3333333333333333703, 0.3333333333333334814, 0.3333333333333333703, 0.3333333333333334259, 0.3333333333333334259, 0.3333333333333335369, 0.3333333333333333703, 0.3333333333333335369, 0.3333333333333334259, 0.3333333333333335369, 0.3333333333333334259, 0.3333333333333334259, 0.3333333333333334814, 0.3333333333333334814, 0.3333333333333333703, 0.3333333333333334814, 0.3333333333333333148, 0.3333333333333335369, 0.3333333333333333148, 0.3333333333333335369, 0.3333333333333334259, 0.3333333333333334259, 0.3333333333333334814, 0.3333333333333334814, 0.3333333333333333703, 0.3333333333333335369, 0.3333333333333333703, 0.3333333333333334259, 0.3333333333333334814, 0.3333333333333334814, 0.3333333333333334259, 0.3333333333333334259, 0.3333333333333335369, 0.3333333333333333148, 0.3333333333333335924, 0.3333333333333333703, 0.3333333333333333703, 0.3333333333333335369, 0.3333333333333333703, 0.3333333333333335924, 0.3333333333333333148, 0.3333333333333333703, 0.3333333333333334814, 0.3333333333333333703, 0.3333333333333335369, 0.3333333333333333703, 0.3333333333333334259, 0.3333333333333334814, 0.3333333333333333703, 0.3333333333333334259, 0.3333333333333334259, 0.3333333333333334259, 0.3333333333333334814, 0.3333333333333333703, 0.3333333333333334259, 0.3333333333333333703, 0.3333333333333335369, 0.3333333333333333703, 0.3333333333333334259, 0.3333333333333334259, 0.3333333333333333703, 0.3333333333333334814, 0.3333333333333333703, 0.3333333333333334259, 0.3333333333333333703, 0.3333333333333334814, 0.3333333333333335369, 0.3333333333333334259, 0.3333333333333334259, 0.3333333333333333703, 0.3333333333333335369, 0.3333333333333333703, 0.3333333333333333703, 0.3333333333333335369, 0.3333333333333333703, 0.3333333333333335924, 0.3333333333333332593, 0.3333333333333335369, 0.3333333333333334259, 0.3333333333333333703, 0.3333333333333335369, 0.3333333333333333703, 0.3333333333333333703, 0.3333333333333334259, 0.3333333333333335369, 0.3333333333333333148, 0.3333333333333333703, 0.3333333333333335369, 0.3333333333333334259, 0.3333333333333333703, 0.3333333333333335369, 0.3333333333333333703, 0.3333333333333335924, 0.3333333333333333703, 0.3333333333333335369, 0.3333333333333334259, 0.3333333333333334814, 0.3333333333333334259, 0.3333333333333334259, 0.3333333333333334814, 0.3333333333333334259, 0.3333333333333334259, 0.3333333333333333148, 0.3333333333333333703, 0.3333333333333334814, 0.3333333333333334814, 0.3333333333333334259, 0.3333333333333333703, 0.3333333333333334259, 0.3333333333333333148, 0.3333333333333335369, 0.3333333333333333703, 0.3333333333333334814, 0.3333333333333335369, 0.3333333333333335369, 0.3333333333333335369, 0.3333333333333333703, 0.3333333333333334259, 0.3333333333333334259, 0.3333333333333333148, 0.3333333333333335369, 0.3333333333333334259, 0.3333333333333334259, 0.3333333333333334259, 0.3333333333333334814, 0.3333333333333334259, 0.3333333333333333148, 0.3333333333333334814, 0.3333333333333334259, 0.3333333333333333703, 0.3333333333333333703, 0.3333333333333334814, 0.3333333333333333703, 0.3333333333333334814, 0.3333333333333334814, 0.3333333333333333148, 0.3333333333333335924, 0.3333333333333333148, 0.3333333333333335369, 0.3333333333333333148, 0.3333333333333335924, 0.3333333333333333703, 0.3333333333333333148, 0.3333333333333334259, 0.3333333333333334259, 0.3333333333333334259, 0.3333333333333333703, 0.3333333333333334814, 0.3333333333333333703, 0.3333333333333334814, 0.3333333333333334814, 0.3333333333333333703, 0.3333333333333334259, 0.3333333333333334259, 0.3333333333333334814, 0.3333333333333333703, 0.3333333333333333703, 0.3333333333333334259, 0.3333333333333334259, 0.3333333333333333703, 0.3333333333333334259, 0.3333333333333333703, 0.3333333333333334259, 0.3333333333333334259, 0.3333333333333333703, 0.3333333333333335924, 0.3333333333333332593, 0.3333333333333335369, 0.3333333333333334259, 0.3333333333333333703, 0.3333333333333333148, 0.3333333333333335924, 0.3333333333333333148, 0.3333333333333333703, 0.3333333333333334259, 0.3333333333333334814, 0.3333333333333335369, 0.3333333333333333703, 0.3333333333333334259, 0.3333333333333333703, 0.3333333333333335369, 0.3333333333333333703, 0.3333333333333334259, 0.3333333333333334814, 0.3333333333333333703, 0.3333333333333335369, 0.3333333333333333148, 0.3333333333333335369, 0.3333333333333334259, 0.3333333333333334259, 0.3333333333333333703, 0.3333333333333335369, 0.3333333333333333703, 0.3333333333333335369, 0.3333333333333334814, 0.3333333333333333703, 0.3333333333333334814, 0.3333333333333333703, 0.3333333333333333703, 0.3333333333333335369, 0.3333333333333333703, 0.3333333333333334259, 0.3333333333333334814, 0.3333333333333333703, 0.3333333333333334259, 0.3333333333333333148, 0.3333333333333335369, 0.3333333333333334259, 0.3333333333333333703, 0.3333333333333334814, 0.3333333333333334259, 0.3333333333333334814, 0.3333333333333334259, 0.3333333333333333703, 0.3333333333333333703, 0.3333333333333334259, 0.3333333333333334259, 0.3333333333333334259, 0.3333333333333334259, 0.3333333333333333703, 0.3333333333333334814, 0.3333333333333334814, 0.3333333333333333703, 0.3333333333333335369, 0.3333333333333333703, 0.3333333333333334814, 0.3333333333333334814, 0.3333333333333335369, 0.3333333333333333148, 0.3333333333333335369, 0.3333333333333333703, 0.3333333333333333148, 0.3333333333333334814, 0.3333333333333333703, 0.3333333333333334814, 0.3333333333333333703, 0.3333333333333334814, 0.3333333333333333703, 0.3333333333333335369, 0.3333333333333333703, 0.3333333333333334814, 0.3333333333333334259, 0.3333333333333334814, 0.3333333333333334259, 0.3333333333333333703, 0.3333333333333333703, 0.3333333333333334814, 0.3333333333333334259, 0.3333333333333334814, 0.3333333333333334259, 0.3333333333333334259, 0.3333333333333334259, 0.3333333333333333703, 0.3333333333333334259, 0.3333333333333333703, 0.3333333333333334814, 0.3333333333333333148, 0.3333333333333335369, 0.3333333333333333703, 0.3333333333333334814, 0.3333333333333333703, 0.3333333333333335369, 0.3333333333333334259, 0.3333333333333334259, 0.3333333333333334259, 0.3333333333333334259, 0.3333333333333334259, 0.3333333333333334259),
 ( 0.3333333333333334259, 0.3333333333333334259, 0.3333333333333333703, 0.3333333333333334259, 0.3333333333333334814, 0.3333333333333333148, 0.3333333333333335924, 0.3333333333333333148, 0.3333333333333334259, 0.3333333333333333703, 0.3333333333333334814, 0.3333333333333334814, 0.3333333333333333148, 0.3333333333333334814, 0.3333333333333333703, 0.3333333333333334259, 0.3333333333333334259, 0.3333333333333333703, 0.3333333333333334814, 0.3333333333333334259, 0.3333333333333335369, 0.3333333333333333148, 0.3333333333333335369, 0.3333333333333333703, 0.3333333333333333703, 0.3333333333333334259, 0.3333333333333334814, 0.3333333333333334814, 0.3333333333333333148, 0.3333333333333335369, 0.3333333333333335924, 0.3333333333333334259, 0.3333333333333333703, 0.3333333333333335369, 0.3333333333333334259, 0.3333333333333334259, 0.3333333333333334814, 0.3333333333333335369, 0.3333333333333333703, 0.3333333333333334259, 0.3333333333333335369, 0.3333333333333333148, 0.3333333333333334259, 0.3333333333333335369, 0.3333333333333333703, 0.3333333333333334259, 0.3333333333333333703, 0.3333333333333335369, 0.3333333333333333703, 0.3333333333333334814, 0.3333333333333333703, 0.3333333333333334259, 0.3333333333333333703, 0.3333333333333333703, 0.3333333333333334259, 0.3333333333333333703, 0.3333333333333334259, 0.3333333333333333148, 0.3333333333333336479, 0.3333333333333334259, 0.3333333333333334814, 0.3333333333333333703, 0.3333333333333335369, 0.3333333333333334259, 0.3333333333333334259, 0.3333333333333334259, 0.3333333333333334259, 0.3333333333333333703, 0.3333333333333333703, 0.3333333333333335369, 0.3333333333333333703, 0.3333333333333335369, 0.3333333333333334259, 0.3333333333333333703, 0.3333333333333334814, 0.3333333333333334259, 0.3333333333333333703, 0.3333333333333333148, 0.3333333333333335369, 0.3333333333333333703, 0.3333333333333335369, 0.3333333333333333703, 0.3333333333333334814, 0.3333333333333333703, 0.3333333333333334259, 0.3333333333333333148, 0.3333333333333335369, 0.3333333333333333703, 0.3333333333333334814, 0.3333333333333333148, 0.3333333333333334814, 0.3333333333333334259, 0.3333333333333335369, 0.3333333333333334259, 0.3333333333333334814, 0.3333333333333334259, 0.3333333333333334259, 0.3333333333333334259, 0.3333333333333334259, 0.3333333333333333703, 0.3333333333333333703, 0.3333333333333334814, 0.3333333333333333703, 0.3333333333333333703, 0.3333333333333335369, 0.3333333333333332593, 0.3333333333333335369, 0.3333333333333332593, 0.3333333333333335924, 0.3333333333333334259, 0.3333333333333334814, 0.3333333333333333703, 0.3333333333333334814, 0.3333333333333334259, 0.3333333333333334259, 0.3333333333333334814, 0.3333333333333333703, 0.3333333333333333703, 0.3333333333333334814, 0.3333333333333333703, 0.3333333333333334814, 0.3333333333333333703, 0.3333333333333334259, 0.3333333333333334259, 0.3333333333333335369, 0.3333333333333333703, 0.3333333333333335369, 0.3333333333333334259, 0.3333333333333335369, 0.3333333333333334259, 0.3333333333333334259, 0.3333333333333334814, 0.3333333333333334814, 0.3333333333333333703, 0.3333333333333334814, 0.3333333333333333148, 0.3333333333333335369, 0.3333333333333333148, 0.3333333333333335369, 0.3333333333333334259, 0.3333333333333334259, 0.3333333333333334814, 0.3333333333333334814, 0.3333333333333333703, 0.3333333333333335369, 0.3333333333333333703, 0.3333333333333334259, 0.3333333333333334814, 0.3333333333333334814, 0.3333333333333334259, 0.3333333333333334259, 0.3333333333333335369, 0.3333333333333333148, 0.3333333333333335924, 0.3333333333333333703, 0.3333333333333333703, 0.3333333333333335369, 0.3333333333333333703, 0.3333333333333335924, 0.3333333333333333148, 0.3333333333333333703, 0.3333333333333334814, 0.3333333333333333703, 0.3333333333333335369, 0.3333333333333333703, 0.3333333333333334259, 0.3333333333333334814, 0.3333333333333333703, 0.3333333333333334259, 0.3333333333333334259, 0.3333333333333334259, 0.3333333333333334814, 0.3333333333333333703, 0.3333333333333334259, 0.3333333333333333703, 0.3333333333333335369, 0.3333333333333333703, 0.3333333333333334259, 0.3333333333333334259, 0.3333333333333333703, 0.3333333333333334814, 0.3333333333333333703, 0.3333333333333334259, 0.3333333333333333703, 0.3333333333333334814, 0.3333333333333335369, 0.3333333333333334259, 0.3333333333333334259, 0.3333333333333333703, 0.3333333333333335369, 0.3333333333333333703, 0.3333333333333333703, 0.3333333333333335369, 0.3333333333333333703, 0.3333333333333335924, 0.3333333333333332593, 0.3333333333333335369, 0.3333333333333334259, 0.3333333333333333703, 0.3333333333333335369, 0.3333333333333333703, 0.3333333333333333703, 0.3333333333333334259, 0.3333333333333335369, 0.3333333333333333148, 0.3333333333333333703, 0.3333333333333335369, 0.3333333333333334259, 0.3333333333333333703, 0.3333333333333335369, 0.3333333333333333703, 0.3333333333333335924, 0.3333333333333333703, 0.3333333333333335369, 0.3333333333333334259, 0.3333333333333334814, 0.3333333333333334259, 0.3333333333333334259, 0.3333333333333334814, 0.3333333333333334259, 0.3333333333333334259, 0.3333333333333333148, 0.3333333333333333703, 0.3333333333333334814, 0.3333333333333334814, 0.3333333333333334259, 0.3333333333333333703, 0.3333333333333334259, 0.3333333333333333148, 0.3333333333333335369, 0.3333333333333333703, 0.3333333333333334814, 0.3333333333333335369, 0.3333333333333335369, 0.3333333333333335369, 0.3333333333333333703, 0.3333333333333334259, 0.3333333333333334259, 0.3333333333333333148, 0.3333333333333335369, 0.3333333333333334259, 0.3333333333333334259, 0.3333333333333334259, 0.3333333333333334814, 0.3333333333333334259, 0.3333333333333333148, 0.3333333333333334814, 0.3333333333333334259, 0.3333333333333333703, 0.3333333333333333703, 0.3333333333333334814, 0.3333333333333333703, 0.3333333333333334814, 0.3333333333333334814, 0.3333333333333333148, 0.3333333333333335924, 0.3333333333333333148, 0.3333333333333335369, 0.3333333333333333148, 0.3333333333333335924, 0.3333333333333333703, 0.3333333333333333148, 0.3333333333333334259, 0.3333333333333334259, 0.3333333333333334259, 0.3333333333333333703, 0.3333333333333334814, 0.3333333333333333703, 0.3333333333333334814, 0.3333333333333334814, 0.3333333333333333703, 0.3333333333333334259, 0.3333333333333334259, 0.3333333333333334814, 0.3333333333333333703, 0.3333333333333333703, 0.3333333333333334259, 0.3333333333333334259, 0.3333333333333333703, 0.3333333333333334259, 0.3333333333333333703, 0.3333333333333334259, 0.3333333333333334259, 0.3333333333333333703, 0.3333333333333335924, 0.3333333333333332593, 0.3333333333333335369, 0.3333333333333334259, 0.3333333333333333703, 0.3333333333333333148, 0.3333333333333335924, 0.3333333333333333148, 0.3333333333333333703, 0.3333333333333334259, 0.3333333333333334814, 0.3333333333333335369, 0.3333333333333333703, 0.3333333333333334259, 0.3333333333333333703, 0.3333333333333335369, 0.3333333333333333703, 0.3333333333333334259, 0.3333333333333334814, 0.3333333333333333703, 0.3333333333333335369, 0.3333333333333333148, 0.3333333333333335369, 0.3333333333333334259, 0.3333333333333334259, 0.3333333333333333703, 0.3333333333333335369, 0.3333333333333333703, 0.3333333333333335369, 0.3333333333333334814, 0.3333333333333333703, 0.3333333333333334814, 0.3333333333333333703, 0.3333333333333333703, 0.3333333333333335369, 0.3333333333333333703, 0.3333333333333334259, 0.3333333333333334814, 0.3333333333333333703, 0.3333333333333334259, 0.3333333333333333148, 0.3333333333333335369, 0.3333333333333334259, 0.3333333333333333703, 0.3333333333333334814, 0.3333333333333334259, 0.3333333333333334814, 0.3333333333333334259, 0.3333333333333333703, 0.3333333333333333703, 0.3333333333333334259, 0.3333333333333334259, 0.3333333333333334259, 0.3333333333333334259, 0.3333333333333333703, 0.3333333333333334814, 0.3333333333333334814, 0.3333333333333333703, 0.3333333333333335369, 0.3333333333333333703, 0.3333333333333334814, 0.3333333333333334814, 0.3333333333333335369, 0.3333333333333333148, 0.3333333333333335369, 0.3333333333333333703, 0.3333333333333333148, 0.3333333333333334814, 0.3333333333333333703, 0.3333333333333334814, 0.3333333333333333703, 0.3333333333333334814, 0.3333333333333333703, 0.3333333333333335369, 0.3333333333333333703, 0.3333333333333334814, 0.3333333333333334259, 0.3333333333333334814, 0.3333333333333334259, 0.3333333333333333703, 0.3333333333333333703, 0.3333333333333334814, 0.3333333333333334259, 0.3333333333333334814, 0.3333333333333334259, 0.3333333333333334259, 0.3333333333333334259, 0.3333333333333333703, 0.3333333333333334259, 0.3333333333333333703, 0.3333333333333334814, 0.3333333333333333148, 0.3333333333333335369, 0.3333333333333333703, 0.3333333333333334814, 0.3333333333333333703, 0.3333333333333335369, 0.3333333333333334259, 0.3333333333333334259, 0.3333333333333334259, 0.3333333333333334259, 0.3333333333333334259, 0.3333333333333334259),
 ( 1.000000000000000222, 1.000000000000000222, 1.000000000000000222, 1.000000000000000222, 1.000000000000000444, 1.000000000000000000, 1.000000000000000666, 0.9999999999999997780, 1.000000000000000444, 1.000000000000000000, 1.000000000000000444, 1.000000000000000444, 1.000000000000000000, 1.000000000000000444, 1.000000000000000000, 1.000000000000000444, 1.000000000000000222, 1.000000000000000222, 1.000000000000000222, 1.000000000000000444, 1.000000000000000444, 1.000000000000000000, 1.000000000000000444, 1.000000000000000000, 1.000000000000000222, 1.000000000000000222, 1.000000000000000444, 1.000000000000000222, 1.000000000000000222, 1.000000000000000444, 1.000000000000000444, 1.000000000000000444, 1.000000000000000000, 1.000000000000000444, 1.000000000000000444, 1.000000000000000000, 1.000000000000000444, 1.000000000000000444, 1.000000000000000000, 1.000000000000000444, 1.000000000000000444, 1.000000000000000000, 1.000000000000000222, 1.000000000000000444, 1.000000000000000222, 1.000000000000000222, 1.000000000000000000, 1.000000000000000444, 1.000000000000000222, 1.000000000000000222, 1.000000000000000222, 1.000000000000000222, 1.000000000000000222, 1.000000000000000222, 1.000000000000000444, 1.000000000000000000, 1.000000000000000444, 0.9999999999999997780, 1.000000000000000666, 1.000000000000000444, 1.000000000000000444, 1.000000000000000000, 1.000000000000000444, 1.000000000000000222, 1.000000000000000222, 1.000000000000000444, 1.000000000000000222, 1.000000000000000444, 1.000000000000000000, 1.000000000000000444, 1.000000000000000222, 1.000000000000000444, 1.000000000000000444, 1.000000000000000222, 1.000000000000000222, 1.000000000000000222, 1.000000000000000444, 0.9999999999999997780, 1.000000000000000444, 1.000000000000000000, 1.000000000000000444, 1.000000000000000000, 1.000000000000000444, 0.9999999999999997780, 1.000000000000000444, 0.9999999999999997780, 1.000000000000000444, 1.000000000000000222, 1.000000000000000444, 1.000000000000000000, 1.000000000000000222, 1.000000000000000444, 1.000000000000000444, 1.000000000000000222, 1.000000000000000444, 1.000000000000000444, 1.000000000000000222, 1.000000000000000222, 1.000000000000000222, 1.000000000000000222, 1.000000000000000000, 1.000000000000000222, 1.000000000000000222, 1.000000000000000222, 1.000000000000000444, 1.000000000000000000, 1.000000000000000444, 0.9999999999999997780, 1.000000000000000666, 1.000000000000000222, 1.000000000000000444, 1.000000000000000000, 1.000000000000000444, 1.000000000000000222, 1.000000000000000222, 1.000000000000000444, 1.000000000000000000, 1.000000000000000000, 1.000000000000000444, 1.000000000000000000, 1.000000000000000444, 1.000000000000000000, 1.000000000000000444, 1.000000000000000222, 1.000000000000000444, 1.000000000000000222, 1.000000000000000444, 1.000000000000000222, 1.000000000000000444, 1.000000000000000000, 1.000000000000000444, 1.000000000000000222, 1.000000000000000444, 1.000000000000000000, 1.000000000000000444, 1.000000000000000000, 1.000000000000000444, 1.000000000000000000, 1.000000000000000444, 1.000000000000000222, 1.000000000000000444, 1.000000000000000222, 1.000000000000000444, 0.9999999999999997780, 1.000000000000000444, 1.000000000000000000, 1.000000000000000444, 1.000000000000000222, 1.000000000000000222, 1.000000000000000222, 1.000000000000000222, 1.000000000000000444, 0.9999999999999997780, 1.000000000000000444, 1.000000000000000000, 1.000000000000000000, 1.000000000000000222, 1.000000000000000222, 1.000000000000000666, 0.9999999999999997780, 1.000000000000000000, 1.000000000000000444, 1.000000000000000222, 1.000000000000000444, 1.000000000000000000, 1.000000000000000222, 1.000000000000000444, 1.000000000000000222, 1.000000000000000000, 1.000000000000000444, 1.000000000000000222, 1.000000000000000222, 1.000000000000000444, 1.000000000000000222, 1.000000000000000000, 1.000000000000000444, 1.000000000000000000, 1.000000000000000444, 1.000000000000000222, 1.000000000000000222, 1.000000000000000444, 0.9999999999999997780, 1.000000000000000444, 0.9999999999999997780, 1.000000000000000444, 1.000000000000000222, 1.000000000000000444, 1.000000000000000222, 1.000000000000000222, 1.000000000000000444, 1.000000000000000000, 1.000000000000000222, 1.000000000000000444, 1.000000000000000000, 1.000000000000000444, 1.000000000000000000, 1.000000000000000222, 1.000000000000000444, 1.000000000000000000, 1.000000000000000444, 0.9999999999999997780, 1.000000000000000444, 1.000000000000000222, 1.000000000000000444, 1.000000000000000000, 1.000000000000000000, 1.000000000000000444, 1.000000000000000000, 1.000000000000000222, 1.000000000000000444, 1.000000000000000222, 1.000000000000000444, 1.000000000000000222, 1.000000000000000444, 1.000000000000000444, 1.000000000000000444, 1.000000000000000000, 1.000000000000000444, 1.000000000000000222, 1.000000000000000444, 1.000000000000000222, 1.000000000000000000, 1.000000000000000222, 1.000000000000000444, 1.000000000000000222, 1.000000000000000444, 1.000000000000000000, 1.000000000000000222, 1.000000000000000000, 1.000000000000000444, 1.000000000000000000, 1.000000000000000444, 1.000000000000000444, 1.000000000000000444, 1.000000000000000444, 1.000000000000000000, 1.000000000000000222, 1.000000000000000444, 1.000000000000000000, 1.000000000000000444, 1.000000000000000444, 1.000000000000000444, 1.000000000000000222, 1.000000000000000222, 1.000000000000000222, 0.9999999999999997780, 1.000000000000000444, 1.000000000000000222, 1.000000000000000222, 1.000000000000000000, 1.000000000000000444, 1.000000000000000000, 1.000000000000000444, 1.000000000000000000, 1.000000000000000000, 1.000000000000000666, 1.000000000000000000, 1.000000000000000444, 1.000000000000000000, 1.000000000000000444, 1.000000000000000222, 0.9999999999999997780, 1.000000000000000444, 1.000000000000000000, 1.000000000000000444, 1.000000000000000222, 1.000000000000000444, 1.000000000000000222, 1.000000000000000222, 1.000000000000000444, 1.000000000000000000, 1.000000000000000222, 1.000000000000000444, 1.000000000000000222, 1.000000000000000000, 1.000000000000000444, 0.9999999999999997780, 1.000000000000000444, 1.000000000000000222, 1.000000000000000222, 1.000000000000000222, 1.000000000000000000, 1.000000000000000444, 1.000000000000000222, 1.000000000000000666, 0.9999999999999997780, 1.000000000000000444, 1.000000000000000222, 1.000000000000000000, 1.000000000000000222, 1.000000000000000444, 1.000000000000000222, 1.000000000000000000, 1.000000000000000444, 1.000000000000000222, 1.000000000000000444, 1.000000000000000000, 1.000000000000000444, 1.000000000000000222, 1.000000000000000444, 1.000000000000000222, 1.000000000000000222, 1.000000000000000444, 1.000000000000000222, 1.000000000000000444, 1.000000000000000000, 1.000000000000000444, 1.000000000000000222, 1.000000000000000222, 1.000000000000000000, 1.000000000000000666, 0.9999999999999997780, 1.000000000000000444, 1.000000000000000222, 1.000000000000000444, 1.000000000000000222, 1.000000000000000444, 1.000000000000000000, 1.000000000000000444, 1.000000000000000222, 1.000000000000000222, 1.000000000000000444, 1.000000000000000222, 1.000000000000000444, 1.000000000000000000, 1.000000000000000444, 1.000000000000000444, 0.9999999999999997780, 1.000000000000000444, 1.000000000000000000, 1.000000000000000444, 1.000000000000000444, 1.000000000000000222, 1.000000000000000000, 1.000000000000000444, 1.000000000000000222, 1.000000000000000444, 1.000000000000000000, 1.000000000000000444, 1.000000000000000222, 1.000000000000000444, 1.000000000000000222, 1.000000000000000444, 1.000000000000000222, 1.000000000000000222, 1.000000000000000444, 1.000000000000000444, 1.000000000000000000, 1.000000000000000444, 0.9999999999999997780, 1.000000000000000444, 1.000000000000000222, 1.000000000000000222, 1.000000000000000222, 1.000000000000000444, 1.000000000000000222, 1.000000000000000222, 1.000000000000000444, 1.000000000000000000, 1.000000000000000444, 1.000000000000000000, 1.000000000000000444, 1.000000000000000222, 1.000000000000000000, 1.000000000000000222, 1.000000000000000444, 1.000000000000000000, 1.000000000000000444, 1.000000000000000000, 1.000000000000000444, 1.000000000000000444, 1.000000000000000000, 1.000000000000000444, 1.000000000000000000, 1.000000000000000444, 1.000000000000000000, 1.000000000000000444, 1.000000000000000000, 1.000000000000000444, 1.000000000000000000, 1.000000000000000444, 1.000000000000000000, 1.000000000000000444, 1.000000000000000222, 1.000000000000000222, 1.000000000000000222, 1.000000000000000222),
 ( 0.3333333333333334259, 0.3333333333333334259, 0.3333333333333333703, 0.3333333333333334259, 0.3333333333333334814, 0.3333333333333333148, 0.3333333333333335924, 0.3333333333333333148, 0.3333333333333334259, 0.3333333333333333703, 0.3333333333333334814, 0.3333333333333334814, 0.3333333333333333148, 0.3333333333333334814, 0.3333333333333333703, 0.3333333333333334259, 0.3333333333333334259, 0.3333333333333333703, 0.3333333333333334814, 0.3333333333333334259, 0.3333333333333335369, 0.3333333333333333148, 0.3333333333333335369, 0.3333333333333333703, 0.3333333333333333703, 0.3333333333333334259, 0.3333333333333334814, 0.3333333333333334814, 0.3333333333333333148, 0.3333333333333335369, 0.3333333333333335924, 0.3333333333333334259, 0.3333333333333333703, 0.3333333333333335369, 0.3333333333333334259, 0.3333333333333334259, 0.3333333333333334814, 0.3333333333333335369, 0.3333333333333333703, 0.3333333333333334259, 0.3333333333333335369, 0.3333333333333333148, 0.3333333333333334259, 0.3333333333333335369, 0.3333333333333333703, 0.3333333333333334259, 0.3333333333333333703, 0.3333333333333335369, 0.3333333333333333703, 0.3333333333333334814, 0.3333333333333333703, 0.3333333333333334259, 0.3333333333333333703, 0.3333333333333333703, 0.3333333333333334259, 0.3333333333333333703, 0.3333333333333334259, 0.3333333333333333148, 0.3333333333333336479, 0.3333333333333334259, 0.3333333333333334814, 0.3333333333333333703, 0.3333333333333335369, 0.3333333333333334259, 0.3333333333333334259, 0.3333333333333334259, 0.3333333333333334259, 0.3333333333333333703, 0.3333333333333333703, 0.3333333333333335369, 0.3333333333333333703, 0.3333333333333335369, 0.3333333333333334259, 0.3333333333333333703, 0.3333333333333334814, 0.3333333333333334259, 0.3333333333333333703, 0.3333333333333333148, 0.3333333333333335369, 0.3333333333333333703, 0.3333333333333335369, 0.3333333333333333703, 0.3333333333333334814, 0.3333333333333333703, 0.3333333333333334259, 0.3333333333333333148, 0.3333333333333335369, 0.3333333333333333703, 0.3333333333333334814, 0.3333333333333333148, 0.3333333333333334814, 0.3333333333333334259, 0.3333333333333335369, 0.3333333333333334259, 0.3333333333333334814, 0.3333333333333334259, 0.3333333333333334259, 0.3333333333333334259, 0.3333333333333334259, 0.3333333333333333703, 0.3333333333333333703, 0.3333333333333334814, 0.3333333333333333703, 0.3333333333333333703, 0.3333333333333335369, 0.3333333333333332593, 0.3333333333333335369, 0.3333333333333332593, 0.3333333333333335924, 0.3333333333333334259, 0.3333333333333334814, 0.3333333333333333703, 0.3333333333333334814, 0.3333333333333334259, 0.3333333333333334259, 0.3333333333333334814, 0.3333333333333333703, 0.3333333333333333703, 0.3333333333333334814, 0.3333333333333333703, 0.3333333333333334814, 0.3333333333333333703, 0.3333333333333334259, 0.3333333333333334259, 0.3333333333333335369, 0.3333333333333333703, 0.3333333333333335369, 0.3333333333333334259, 0.3333333333333335369, 0.3333333333333334259, 0.3333333333333334259, 0.3333333333333334814, 0.3333333333333334814, 0.3333333333333333703, 0.3333333333333334814, 0.3333333333333333148, 0.3333333333333335369, 0.3333333333333333148, 0.3333333333333335369, 0.3333333333333334259, 0.3333333333333334259, 0.3333333333333334814, 0.3333333333333334814, 0.3333333333333333703, 0.3333333333333335369, 0.3333333333333333703, 0.3333333333333334259, 0.3333333333333334814, 0.3333333333333334814, 0.3333333333333334259, 0.3333333333333334259, 0.3333333333333335369, 0.3333333333333333148, 0.3333333333333335924, 0.3333333333333333703, 0.3333333333333333703, 0.3333333333333335369, 0.3333333333333333703, 0.3333333333333335924, 0.3333333333333333148, 0.3333333333333333703, 0.3333333333333334814, 0.3333333333333333703, 0.3333333333333335369, 0.3333333333333333703, 0.3333333333333334259, 0.3333333333333334814, 0.3333333333333333703, 0.3333333333333334259, 0.3333333333333334259, 0.3333333333333334259, 0.3333333333333334814, 0.3333333333333333703, 0.3333333333333334259, 0.3333333333333333703, 0.3333333333333335369, 0.3333333333333333703, 0.3333333333333334259, 0.3333333333333334259, 0.3333333333333333703, 0.3333333333333334814, 0.3333333333333333703, 0.3333333333333334259, 0.3333333333333333703, 0.3333333333333334814, 0.3333333333333335369, 0.3333333333333334259, 0.3333333333333334259, 0.3333333333333333703, 0.3333333333333335369, 0.3333333333333333703, 0.3333333333333333703, 0.3333333333333335369, 0.3333333333333333703, 0.3333333333333335924, 0.3333333333333332593, 0.3333333333333335369, 0.3333333333333334259, 0.3333333333333333703, 0.3333333333333335369, 0.3333333333333333703, 0.3333333333333333703, 0.3333333333333334259, 0.3333333333333335369, 0.3333333333333333148, 0.3333333333333333703, 0.3333333333333335369, 0.3333333333333334259, 0.3333333333333333703, 0.3333333333333335369, 0.3333333333333333703, 0.3333333333333335924, 0.3333333333333333703, 0.3333333333333335369, 0.3333333333333334259, 0.3333333333333334814, 0.3333333333333334259, 0.3333333333333334259, 0.3333333333333334814, 0.3333333333333334259, 0.3333333333333334259, 0.3333333333333333148, 0.3333333333333333703, 0.3333333333333334814, 0.3333333333333334814, 0.3333333333333334259, 0.3333333333333333703, 0.3333333333333334259, 0.3333333333333333148, 0.3333333333333335369, 0.3333333333333333703, 0.3333333333333334814, 0.3333333333333335369, 0.3333333333333335369, 0.3333333333333335369, 0.3333333333333333703, 0.3333333333333334259, 0.3333333333333334259, 0.3333333333333333148, 0.3333333333333335369, 0.3333333333333334259, 0.3333333333333334259, 0.3333333333333334259, 0.3333333333333334814, 0.3333333333333334259, 0.3333333333333333148, 0.3333333333333334814, 0.3333333333333334259, 0.3333333333333333703, 0.3333333333333333703, 0.3333333333333334814, 0.3333333333333333703, 0.3333333333333334814, 0.3333333333333334814, 0.3333333333333333148, 0.3333333333333335924, 0.3333333333333333148, 0.3333333333333335369, 0.3333333333333333148, 0.3333333333333335924, 0.3333333333333333703, 0.3333333333333333148, 0.3333333333333334259, 0.3333333333333334259, 0.3333333333333334259, 0.3333333333333333703, 0.3333333333333334814, 0.3333333333333333703, 0.3333333333333334814, 0.3333333333333334814, 0.3333333333333333703, 0.3333333333333334259, 0.3333333333333334259, 0.3333333333333334814, 0.3333333333333333703, 0.3333333333333333703, 0.3333333333333334259, 0.3333333333333334259, 0.3333333333333333703, 0.3333333333333334259, 0.3333333333333333703, 0.3333333333333334259, 0.3333333333333334259, 0.3333333333333333703, 0.3333333333333335924, 0.3333333333333332593, 0.3333333333333335369, 0.3333333333333334259, 0.3333333333333333703, 0.3333333333333333148, 0.3333333333333335924, 0.3333333333333333148, 0.3333333333333333703, 0.3333333333333334259, 0.3333333333333334814, 0.3333333333333335369, 0.3333333333333333703, 0.3333333333333334259, 0.3333333333333333703, 0.3333333333333335369, 0.3333333333333333703, 0.3333333333333334259, 0.3333333333333334814, 0.3333333333333333703, 0.3333333333333335369, 0.3333333333333333148, 0.3333333333333335369, 0.3333333333333334259, 0.3333333333333334259, 0.3333333333333333703, 0.3333333333333335369, 0.3333333333333333703, 0.3333333333333335369, 0.3333333333333334814, 0.3333333333333333703, 0.3333333333333334814, 0.3333333333333333703, 0.3333333333333333703, 0.3333333333333335369, 0.3333333333333333703, 0.3333333333333334259, 0.3333333333333334814, 0.3333333333333333703, 0.3333333333333334259, 0.3333333333333333148, 0.3333333333333335369, 0.3333333333333334259, 0.3333333333333333703, 0.3333333333333334814, 0.3333333333333334259, 0.3333333333333334814, 0.3333333333333334259, 0.3333333333333333703, 0.3333333333333333703, 0.3333333333333334259, 0.3333333333333334259, 0.3333333333333334259, 0.3333333333333334259, 0.3333333333333333703, 0.3333333333333334814, 0.3333333333333334814, 0.3333333333333333703, 0.3333333333333335369, 0.3333333333333333703, 0.3333333333333334814, 0.3333333333333334814, 0.3333333333333335369, 0.3333333333333333148, 0.3333333333333335369, 0.3333333333333333703, 0.3333333333333333148, 0.3333333333333334814, 0.3333333333333333703, 0.3333333333333334814, 0.3333333333333333703, 0.3333333333333334814, 0.3333333333333333703, 0.3333333333333335369, 0.3333333333333333703, 0.3333333333333334814, 0.3333333333333334259, 0.3333333333333334814, 0.3333333333333334259, 0.3333333333333333703, 0.3333333333333333703, 0.3333333333333334814, 0.3333333333333334259, 0.3333333333333334814, 0.3333333333333334259, 0.3333333333333334259, 0.3333333333333334259, 0.3333333333333333703, 0.3333333333333334259, 0.3333333333333333703, 0.3333333333333334814, 0.3333333333333333148, 0.3333333333333335369, 0.3333333333333333703, 0.3333333333333334814, 0.3333333333333333703, 0.3333333333333335369, 0.3333333333333334259, 0.3333333333333334259, 0.3333333333333334259, 0.3333333333333334259, 0.3333333333333334259, 0.3333333333333334259),
 ( 0.3333333333333334259, 0.3333333333333334259, 0.3333333333333333703, 0.3333333333333334259, 0.3333333333333334814, 0.3333333333333333148, 0.3333333333333335924, 0.3333333333333333148, 0.3333333333333334259, 0.3333333333333333703, 0.3333333333333334814, 0.3333333333333334814, 0.3333333333333333148, 0.3333333333333334814, 0.3333333333333333703, 0.3333333333333334259, 0.3333333333333334259, 0.3333333333333333703, 0.3333333333333334814, 0.3333333333333334259, 0.3333333333333335369, 0.3333333333333333148, 0.3333333333333335369, 0.3333333333333333703, 0.3333333333333333703, 0.3333333333333334259, 0.3333333333333334814, 0.3333333333333334814, 0.3333333333333333148, 0.3333333333333335369, 0.3333333333333335924, 0.3333333333333334259, 0.3333333333333333703, 0.3333333333333335369, 0.3333333333333334259, 0.3333333333333334259, 0.3333333333333334814, 0.3333333333333335369, 0.3333333333333333703, 0.3333333333333334259, 0.3333333333333335369, 0.3333333333333333148, 0.3333333333333334259, 0.3333333333333335369, 0.3333333333333333703, 0.3333333333333334259, 0.3333333333333333703, 0.3333333333333335369, 0.3333333333333333703, 0.3333333333333334814, 0.3333333333333333703, 0.3333333333333334259, 0.3333333333333333703, 0.3333333333333333703, 0.3333333333333334259, 0.3333333333333333703, 0.3333333333333334259, 0.3333333333333333148, 0.3333333333333336479, 0.3333333333333334259, 0.3333333333333334814, 0.3333333333333333703, 0.3333333333333335369, 0.3333333333333334259, 0.3333333333333334259, 0.3333333333333334259, 0.3333333333333334259, 0.3333333333333333703, 0.3333333333333333703, 0.3333333333333335369, 0.3333333333333333703, 0.3333333333333335369, 0.3333333333333334259, 0.3333333333333333703, 0.3333333333333334814, 0.3333333333333334259, 0.3333333333333333703, 0.3333333333333333148, 0.3333333333333335369, 0.3333333333333333703, 0.3333333333333335369, 0.3333333333333333703, 0.3333333333333334814, 0.3333333333333333703, 0.3333333333333334259, 0.3333333333333333148, 0.3333333333333335369, 0.3333333333333333703, 0.3333333333333334814, 0.3333333333333333148, 0.3333333333333334814, 0.3333333333333334259, 0.3333333333333335369, 0.3333333333333334259, 0.3333333333333334814, 0.3333333333333334259, 0.3333333333333334259, 0.3333333333333334259, 0.3333333333333334259, 0.3333333333333333703, 0.3333333333333333703, 0.3333333333333334814, 0.3333333333333333703, 0.3333333333333333703, 0.3333333333333335369, 0.3333333333333332593, 0.3333333333333335369, 0.3333333333333332593, 0.3333333333333335924, 0.3333333333333334259, 0.3333333333333334814, 0.3333333333333333703, 0.3333333333333334814, 0.3333333333333334259, 0.3333333333333334259, 0.3333333333333334814, 0.3333333333333333703, 0.3333333333333333703, 0.3333333333333334814, 0.3333333333333333703, 0.3333333333333334814, 0.3333333333333333703, 0.3333333333333334259, 0.3333333333333334259, 0.3333333333333335369, 0.3333333333333333703, 0.3333333333333335369, 0.3333333333333334259, 0.3333333333333335369, 0.3333333333333334259, 0.3333333333333334259, 0.3333333333333334814, 0.3333333333333334814, 0.3333333333333333703, 0.3333333333333334814, 0.3333333333333333148, 0.3333333333333335369, 0.3333333333333333148, 0.3333333333333335369, 0.3333333333333334259, 0.3333333333333334259, 0.3333333333333334814, 0.3333333333333334814, 0.3333333333333333703, 0.3333333333333335369, 0.3333333333333333703, 0.3333333333333334259, 0.3333333333333334814, 0.3333333333333334814, 0.3333333333333334259, 0.3333333333333334259, 0.3333333333333335369, 0.3333333333333333148, 0.3333333333333335924, 0.3333333333333333703, 0.3333333333333333703, 0.3333333333333335369, 0.3333333333333333703, 0.3333333333333335924, 0.3333333333333333148, 0.3333333333333333703, 0.3333333333333334814, 0.3333333333333333703, 0.3333333333333335369, 0.3333333333333333703, 0.3333333333333334259, 0.3333333333333334814, 0.3333333333333333703, 0.3333333333333334259, 0.3333333333333334259, 0.3333333333333334259, 0.3333333333333334814, 0.3333333333333333703, 0.3333333333333334259, 0.3333333333333333703, 0.3333333333333335369, 0.3333333333333333703, 0.3333333333333334259, 0.3333333333333334259, 0.3333333333333333703, 0.3333333333333334814, 0.3333333333333333703, 0.3333333333333334259, 0.3333333333333333703, 0.3333333333333334814, 0.3333333333333335369, 0.3333333333333334259, 0.3333333333333334259, 0.3333333333333333703, 0.3333333333333335369, 0.3333333333333333703, 0.3333333333333333703, 0.3333333333333335369, 0.3333333333333333703, 0.3333333333333335924, 0.3333333333333332593, 0.3333333333333335369, 0.3333333333333334259, 0.3333333333333333703, 0.3333333333333335369, 0.3333333333333333703, 0.3333333333333333703, 0.3333333333333334259, 0.3333333333333335369, 0.3333333333333333148, 0.3333333333333333703, 0.3333333333333335369, 0.3333333333333334259, 0.3333333333333333703, 0.3333333333333335369, 0.3333333333333333703, 0.3333333333333335924, 0.3333333333333333703, 0.3333333333333335369, 0.3333333333333334259, 0.3333333333333334814, 0.3333333333333334259, 0.3333333333333334259, 0.3333333333333334814, 0.3333333333333334259, 0.3333333333333334259, 0.3333333333333333148, 0.3333333333333333703, 0.3333333333333334814, 0.3333333333333334814, 0.3333333333333334259, 0.3333333333333333703, 0.3333333333333334259, 0.3333333333333333148, 0.3333333333333335369, 0.3333333333333333703, 0.3333333333333334814, 0.3333333333333335369, 0.3333333333333335369, 0.3333333333333335369, 0.3333333333333333703, 0.3333333333333334259, 0.3333333333333334259, 0.3333333333333333148, 0.3333333333333335369, 0.3333333333333334259, 0.3333333333333334259, 0.3333333333333334259, 0.3333333333333334814, 0.3333333333333334259, 0.3333333333333333148, 0.3333333333333334814, 0.3333333333333334259, 0.3333333333333333703, 0.3333333333333333703, 0.3333333333333334814, 0.3333333333333333703, 0.3333333333333334814, 0.3333333333333334814, 0.3333333333333333148, 0.3333333333333335924, 0.3333333333333333148, 0.3333333333333335369, 0.3333333333333333148, 0.3333333333333335924, 0.3333333333333333703, 0.3333333333333333148, 0.3333333333333334259, 0.3333333333333334259, 0.3333333333333334259, 0.3333333333333333703, 0.3333333333333334814, 0.3333333333333333703, 0.3333333333333334814, 0.3333333333333334814, 0.3333333333333333703, 0.3333333333333334259, 0.3333333333333334259, 0.3333333333333334814, 0.3333333333333333703, 0.3333333333333333703, 0.3333333333333334259, 0.3333333333333334259, 0.3333333333333333703, 0.3333333333333334259, 0.3333333333333333703, 0.3333333333333334259, 0.3333333333333334259, 0.3333333333333333703, 0.3333333333333335924, 0.3333333333333332593, 0.3333333333333335369, 0.3333333333333334259, 0.3333333333333333703, 0.3333333333333333148, 0.3333333333333335924, 0.3333333333333333148, 0.3333333333333333703, 0.3333333333333334259, 0.3333333333333334814, 0.3333333333333335369, 0.3333333333333333703, 0.3333333333333334259, 0.3333333333333333703, 0.3333333333333335369, 0.3333333333333333703, 0.3333333333333334259, 0.3333333333333334814, 0.3333333333333333703, 0.3333333333333335369, 0.3333333333333333148, 0.3333333333333335369, 0.3333333333333334259, 0.3333333333333334259, 0.3333333333333333703, 0.3333333333333335369, 0.3333333333333333703, 0.3333333333333335369, 0.3333333333333334814, 0.3333333333333333703, 0.3333333333333334814, 0.3333333333333333703, 0.3333333333333333703, 0.3333333333333335369, 0.3333333333333333703, 0.3333333333333334259, 0.3333333333333334814, 0.3333333333333333703, 0.3333333333333334259, 0.3333333333333333148, 0.3333333333333335369, 0.3333333333333334259, 0.3333333333333333703, 0.3333333333333334814, 0.3333333333333334259, 0.3333333333333334814, 0.3333333333333334259, 0.3333333333333333703, 0.3333333333333333703, 0.3333333333333334259, 0.3333333333333334259, 0.3333333333333334259, 0.3333333333333334259, 0.3333333333333333703, 0.3333333333333334814, 0.3333333333333334814, 0.3333333333333333703, 0.3333333333333335369, 0.3333333333333333703, 0.3333333333333334814, 0.3333333333333334814, 0.3333333333333335369, 0.3333333333333333148, 0.3333333333333335369, 0.3333333333333333703, 0.3333333333333333148, 0.3333333333333334814, 0.3333333333333333703, 0.3333333333333334814, 0.3333333333333333703, 0.3333333333333334814, 0.3333333333333333703, 0.3333333333333335369, 0.3333333333333333703, 0.3333333333333334814, 0.3333333333333334259, 0.3333333333333334814, 0.3333333333333334259, 0.3333333333333333703, 0.3333333333333333703, 0.3333333333333334814, 0.3333333333333334259, 0.3333333333333334814, 0.3333333333333334259, 0.3333333333333334259, 0.3333333333333334259, 0.3333333333333333703, 0.3333333333333334259, 0.3333333333333333703, 0.3333333333333334814, 0.3333333333333333148, 0.3333333333333335369, 0.3333333333333333703, 0.3333333333333334814, 0.3333333333333333703, 0.3333333333333335369, 0.3333333333333334259, 0.3333333333333334259, 0.3333333333333334259, 0.3333333333333334259, 0.3333333333333334259, 0.3333333333333334259),
 ( 1.000000000000000222, 1.000000000000000222, 1.000000000000000222, 1.000000000000000222, 1.000000000000000444, 1.000000000000000000, 1.000000000000000666, 0.9999999999999997780, 1.000000000000000444, 1.000000000000000000, 1.000000000000000444, 1.000000000000000444, 1.000000000000000000, 1.000000000000000444, 1.000000000000000000, 1.000000000000000444, 1.000000000000000222, 1.000000000000000222, 1.000000000000000222, 1.000000000000000444, 1.000000000000000444, 1.000000000000000000, 1.000000000000000444, 1.000000000000000000, 1.000000000000000222, 1.000000000000000222, 1.000000000000000444, 1.000000000000000222, 1.000000000000000222, 1.000000000000000444, 1.000000000000000444, 1.000000000000000444, 1.000000000000000000, 1.000000000000000444, 1.000000000000000444, 1.000000000000000000, 1.000000000000000444, 1.000000000000000444, 1.000000000000000000, 1.000000000000000444, 1.000000000000000444, 1.000000000000000000, 1.000000000000000222, 1.000000000000000444, 1.000000000000000222, 1.000000000000000222, 1.000000000000000000, 1.000000000000000444, 1.000000000000000222, 1.000000000000000222, 1.000000000000000222, 1.000000000000000222, 1.000000000000000222, 1.000000000000000222, 1.000000000000000444, 1.000000000000000000, 1.000000000000000444, 0.9999999999999997780, 1.000000000000000666, 1.000000000000000444, 1.000000000000000444, 1.000000000000000000, 1.000000000000000444, 1.000000000000000222, 1.000000000000000222, 1.000000000000000444, 1.000000000000000222, 1.000000000000000444, 1.000000000000000000, 1.000000000000000444, 1.000000000000000222, 1.000000000000000444, 1.000000000000000444, 1.000000000000000222, 1.000000000000000222, 1.000000000000000222, 1.000000000000000444, 0.9999999999999997780, 1.000000000000000444, 1.000000000000000000, 1.000000000000000444, 1.000000000000000000, 1.000000000000000444, 0.9999999999999997780, 1.000000000000000444, 0.9999999999999997780, 1.000000000000000444, 1.000000000000000222, 1.000000000000000444, 1.000000000000000000, 1.000000000000000222, 1.000000000000000444, 1.000000000000000444, 1.000000000000000222, 1.000000000000000444, 1.000000000000000444, 1.000000000000000222, 1.000000000000000222, 1.000000000000000222, 1.000000000000000222, 1.000000000000000000, 1.000000000000000222, 1.000000000000000222, 1.000000000000000222, 1.000000000000000444, 1.000000000000000000, 1.000000000000000444, 0.9999999999999997780, 1.000000000000000666, 1.000000000000000222, 1.000000000000000444, 1.000000000000000000, 1.000000000000000444, 1.000000000000000222, 1.000000000000000222, 1.000000000000000444, 1.000000000000000000, 1.000000000000000000, 1.000000000000000444, 1.000000000000000000, 1.000000000000000444, 1.000000000000000000, 1.000000000000000444, 1.000000000000000222, 1.000000000000000444, 1.000000000000000222, 1.000000000000000444, 1.000000000000000222, 1.000000000000000444, 1.000000000000000000, 1.000000000000000444, 1.000000000000000222, 1.000000000000000444, 1.000000000000000000, 1.000000000000000444, 1.000000000000000000, 1.000000000000000444, 1.000000000000000000, 1.000000000000000444, 1.000000000000000222, 1.000000000000000444, 1.000000000000000222, 1.000000000000000444, 0.9999999999999997780, 1.000000000000000444, 1.000000000000000000, 1.000000000000000444, 1.000000000000000222, 1.000000000000000222, 1.000000000000000222, 1.000000000000000222, 1.000000000000000444, 0.9999999999999997780, 1.000000000000000444, 1.000000000000000000, 1.000000000000000000, 1.000000000000000222, 1.000000000000000222, 1.000000000000000666, 0.9999999999999997780, 1.000000000000000000, 1.000000000000000444, 1.000000000000000222, 1.000000000000000444, 1.000000000000000000, 1.000000000000000222, 1.000000000000000444, 1.000000000000000222, 1.000000000000000000, 1.000000000000000444, 1.000000000000000222, 1.000000000000000222, 1.000000000000000444, 1.000000000000000222, 1.000000000000000000, 1.000000000000000444, 1.000000000000000000, 1.000000000000000444, 1.000000000000000222, 1.000000000000000222, 1.000000000000000444, 0.9999999999999997780, 1.000000000000000444, 0.9999999999999997780, 1.000000000000000444, 1.000000000000000222, 1.000000000000000444, 1.000000000000000222, 1.000000000000000222, 1.000000000000000444, 1.000000000000000000, 1.000000000000000222, 1.000000000000000444, 1.000000000000000000, 1.000000000000000444, 1.000000000000000000, 1.000000000000000222, 1.000000000000000444, 1.000000000000000000, 1.000000000000000444, 0.9999999999999997780, 1.000000000000000444, 1.000000000000000222, 1.000000000000000444, 1.000000000000000000, 1.000000000000000000, 1.000000000000000444, 1.000000000000000000, 1.000000000000000222, 1.000000000000000444, 1.000000000000000222, 1.000000000000000444, 1.000000000000000222, 1.000000000000000444, 1.000000000000000444, 1.000000000000000444, 1.000000000000000000, 1.000000000000000444, 1.000000000000000222, 1.000000000000000444, 1.000000000000000222, 1.000000000000000000, 1.000000000000000222, 1.000000000000000444, 1.000000000000000222, 1.000000000000000444, 1.000000000000000000, 1.000000000000000222, 1.000000000000000000, 1.000000000000000444, 1.000000000000000000, 1.000000000000000444, 1.000000000000000444, 1.000000000000000444, 1.000000000000000444, 1.000000000000000000, 1.000000000000000222, 1.000000000000000444, 1.000000000000000000, 1.000000000000000444, 1.000000000000000444, 1.000000000000000444, 1.000000000000000222, 1.000000000000000222, 1.000000000000000222, 0.9999999999999997780, 1.000000000000000444, 1.000000000000000222, 1.000000000000000222, 1.000000000000000000, 1.000000000000000444, 1.000000000000000000, 1.000000000000000444, 1.000000000000000000, 1.000000000000000000, 1.000000000000000666, 1.000000000000000000, 1.000000000000000444, 1.000000000000000000, 1.000000000000000444, 1.000000000000000222, 0.9999999999999997780, 1.000000000000000444, 1.000000000000000000, 1.000000000000000444, 1.000000000000000222, 1.000000000000000444, 1.000000000000000222, 1.000000000000000222, 1.000000000000000444, 1.000000000000000000, 1.000000000000000222, 1.000000000000000444, 1.000000000000000222, 1.000000000000000000, 1.000000000000000444, 0.9999999999999997780, 1.000000000000000444, 1.000000000000000222, 1.000000000000000222, 1.000000000000000222, 1.000000000000000000, 1.000000000000000444, 1.000000000000000222, 1.000000000000000666, 0.9999999999999997780, 1.000000000000000444, 1.000000000000000222, 1.000000000000000000, 1.000000000000000222, 1.000000000000000444, 1.000000000000000222, 1.000000000000000000, 1.000000000000000444, 1.000000000000000222, 1.000000000000000444, 1.000000000000000000, 1.000000000000000444, 1.000000000000000222, 1.000000000000000444, 1.000000000000000222, 1.000000000000000222, 1.000000000000000444, 1.000000000000000222, 1.000000000000000444, 1.000000000000000000, 1.000000000000000444, 1.000000000000000222, 1.000000000000000222, 1.000000000000000000, 1.000000000000000666, 0.9999999999999997780, 1.000000000000000444, 1.000000000000000222, 1.000000000000000444, 1.000000000000000222, 1.000000000000000444, 1.000000000000000000, 1.000000000000000444, 1.000000000000000222, 1.000000000000000222, 1.000000000000000444, 1.000000000000000222, 1.000000000000000444, 1.000000000000000000, 1.000000000000000444, 1.000000000000000444, 0.9999999999999997780, 1.000000000000000444, 1.000000000000000000, 1.000000000000000444, 1.000000000000000444, 1.000000000000000222, 1.000000000000000000, 1.000000000000000444, 1.000000000000000222, 1.000000000000000444, 1.000000000000000000, 1.000000000000000444, 1.000000000000000222, 1.000000000000000444, 1.000000000000000222, 1.000000000000000444, 1.000000000000000222, 1.000000000000000222, 1.000000000000000444, 1.000000000000000444, 1.000000000000000000, 1.000000000000000444, 0.9999999999999997780, 1.000000000000000444, 1.000000000000000222, 1.000000000000000222, 1.000000000000000222, 1.000000000000000444, 1.000000000000000222, 1.000000000000000222, 1.000000000000000444, 1.000000000000000000, 1.000000000000000444, 1.000000000000000000, 1.000000000000000444, 1.000000000000000222, 1.000000000000000000, 1.000000000000000222, 1.000000000000000444, 1.000000000000000000, 1.000000000000000444, 1.000000000000000000, 1.000000000000000444, 1.000000000000000444, 1.000000000000000000, 1.000000000000000444, 1.000000000000000000, 1.000000000000000444, 1.000000000000000000, 1.000000000000000444, 1.000000000000000000, 1.000000000000000444, 1.000000000000000000, 1.000000000000000444, 1.000000000000000000, 1.000000000000000444, 1.000000000000000222, 1.000000000000000222, 1.000000000000000222, 1.000000000000000222) ) ) 
 REPRESENTATION_ITEM ( '' )  SURFACE ( )  );
#8053 = CARTESIAN_POINT ( 'NONE',  ( 0.000000000000000000, 4.518467169708412889, 0.000000000000000000 ) ) ;
#8054 = CARTESIAN_POINT ( 'NONE',  ( 5.659468189498653601, -0.4240490459222304165, -1.681042783800198448 ) ) ;
#8055 = CARTESIAN_POINT ( 'NONE',  ( 1.436444770134176485, 1.085300811998829662, -1.921501399296850821 ) ) ;
#8056 = PRESENTATION_LAYER_ASSIGNMENT (  '', '', ( #87697 ) ) ;
#8057 = CARTESIAN_POINT ( 'NONE',  ( 6.355955588539900170, -0.7375000094371157999, 2.042207395130499759 ) ) ;
#8058 = CARTESIAN_POINT ( 'NONE',  ( 5.346851039111009563, 6.199209027673978412, 1.092492203018504471 ) ) ;
#8059 = CARTESIAN_POINT ( 'NONE',  ( 0.3920140705387532010, -2.106502388992930630, 0.2143382252216985973 ) ) ;
#8060 = CARTESIAN_POINT ( 'NONE',  ( 2.812500000000002665, 1.451031289061236684, 1.451031289061000873 ) ) ;
#8061 = CIRCLE ( 'NONE', #129250, 7.750000000000000888 ) ;
#8062 = DIRECTION ( 'NONE',  ( 0.000000000000000000, 0.000000000000000000, -1.000000000000000000 ) ) ;
#8063 = CARTESIAN_POINT ( 'NONE',  ( 4.049766240643924320, 0.6497466500948418933, -1.813626049157530229 ) ) ;
#8064 = CARTESIAN_POINT ( 'NONE',  ( -1.500000000000015099, 11.51041666734946567, -0.8660254037844309360 ) ) ;
#8065 = CARTESIAN_POINT ( 'NONE',  ( 1.014661930782149168, -2.221473418436111125, 0.005229513783167742333 ) ) ;
#8066 = ORIENTED_EDGE ( 'NONE', *, *, #173298, .T. ) ;
#8067 = CARTESIAN_POINT ( 'NONE',  ( 1.499999999999987121, 4.545833333333352932, -0.8660254037844323793 ) ) ;
#8068 = CARTESIAN_POINT ( 'NONE',  ( 5.332434488876471868, 5.115595079977664383, 0.7998128361456341429 ) ) ;
#8069 = CARTESIAN_POINT ( 'NONE',  ( 6.982612806237943559, 8.105135347821125436, -1.199719254218446718 ) ) ;
#8070 = CARTESIAN_POINT ( 'NONE',  ( 3.950012332353939559, -1.532167235135332373, -1.608510083909537869 ) ) ;
#8071 = CARTESIAN_POINT ( 'NONE',  ( -7.863365906246061243, 10.19701286208565705, -1.443375672974059665 ) ) ;
#8072 =( LENGTH_UNIT ( ) NAMED_UNIT ( * ) SI_UNIT ( .MILLI., .METRE. ) );
#8073 = CARTESIAN_POINT ( 'NONE',  ( 5.327991180490514012, 9.159814110640187579, 1.040834085586084257E-14 ) ) ;
#8074 = CARTESIAN_POINT ( 'NONE',  ( -7.646435447983039424, 11.86466575604815787, 0.000000000000000000 ) ) ;
#8075 = CARTESIAN_POINT ( 'NONE',  ( 6.292392690518195941, 8.434487120394948079, -1.443375672974078761 ) ) ;
#8076 = CARTESIAN_POINT ( 'NONE',  ( 0.9498425221252141393, -1.824119990893595888, -0.8596288560165299408 ) ) ;
#8078 = CARTESIAN_POINT ( 'NONE',  ( 0.2509072133702301421, -0.4515964501156078392, -2.020277220192217449 ) ) ;
#8077 = CARTESIAN_POINT ( 'NONE',  ( 7.727257484784855635, 11.10255193463598111, -1.199719254218446718 ) ) ;
#8079 = PLANE ( 'NONE',  #88919 ) ;
#8080 = CARTESIAN_POINT ( 'NONE',  ( 5.492461626867537916, 9.421972641405202964, -0.7216878364870458196 ) ) ;
#8081 = CARTESIAN_POINT ( 'NONE',  ( 6.181193141064822427, 1.207202257718576144, 1.253980304253142997 ) ) ;
#8082 = CARTESIAN_POINT ( 'NONE',  ( -2.314109536355652530, 5.457892750589173225, -0.8025987720412944837 ) ) ;
#8083 = CARTESIAN_POINT ( 'NONE',  ( 1.364683531249988535, 2.363541667008088432, 0.7879004041258500513 ) ) ;
#8084 = CARTESIAN_POINT ( 'NONE',  ( 1.088686764528872919, 1.564356141470560679, -0.8274751086292527757 ) ) ;
#8085 = CARTESIAN_POINT ( 'NONE',  ( 6.574911468446097196, -0.7340051069854407473, 1.570379515389648040 ) ) ;
#8086 = CARTESIAN_POINT ( 'NONE',  ( 0.1339853816830008371, 0.3136495386693045062, 1.814181566856580607 ) ) ;
#8087 = EDGE_CURVE ( 'NONE', #191425, #2091, #133614, .T. ) ;
#8088 = CARTESIAN_POINT ( 'NONE',  ( 4.529038776287770851, -2.096192991274762996, 0.9282860960324219590 ) ) ;
#8089 = CARTESIAN_POINT ( 'NONE',  ( -0.6823417656250003738, -0.7822916663252423852, -1.181850606188749264 ) ) ;
#8090 = CARTESIAN_POINT ( 'NONE',  ( 1.921575063125853022, 1.060747535801230379, -1.504664925706208578 ) ) ;
#8091 = CARTESIAN_POINT ( 'NONE',  ( 8.940712233207955606, 12.51824914112961729, 1.199719254218450271 ) ) ;
#8092 = CARTESIAN_POINT ( 'NONE',  ( 3.170728842436408179, -1.686227525993441834, -0.7000332573987508855 ) ) ;
#8093 = CARTESIAN_POINT ( 'NONE',  ( 3.481092415823695774, -2.014232707597499505, -0.09613569647320965861 ) ) ;
#8094 = CARTESIAN_POINT ( 'NONE',  ( -10.49131193887636826, 11.13428543831092909, 1.040834085586084257E-14 ) ) ;
#8096 = CARTESIAN_POINT ( 'NONE',  ( 0.000000000000000000, 7.500000000000000000, 0.000000000000000000 ) ) ;
#8095 = CARTESIAN_POINT ( 'NONE',  ( 3.221791447092836602, -2.180992460559240786, 0.6016781482265749492 ) ) ;
#8097 = CARTESIAN_POINT ( 'NONE',  ( 5.684633084330723563, -2.053880889230023321, -0.4646916863456708735 ) ) ;
#8098 = CARTESIAN_POINT ( 'NONE',  ( 9.246599373783906728, 13.75186350236544008, 6.856982591890075085 ) ) ;
#8099 = CARTESIAN_POINT ( 'NONE',  ( 2.576698201331685922, 1.354182300986291887, -1.566139152919379107 ) ) ;
#8100 = CARTESIAN_POINT ( 'NONE',  ( 3.571683402196252910, 6.254382171615883834, 1.199719254218462483 ) ) ;
#8101 = CARTESIAN_POINT ( 'NONE',  ( -1.360316468750012886, -0.05729166632526227348, 0.7853790794158901356 ) ) ;
#8102 = CARTESIAN_POINT ( 'NONE',  ( 5.584674446412367210, -1.345185468269005424, 1.639207791927596247 ) ) ;
#8103 = PRODUCT_CONTEXT ( 'NONE', #141817, 'mechanical' ) ;
#8106 = EDGE_CURVE ( 'NONE', #179696, #186824, #27111, .T. ) ;
#8105 = CARTESIAN_POINT ( 'NONE',  ( 0.5922524703982982031, -1.911778602531236215, -0.2371815352125578036 ) ) ;
#8104 = CARTESIAN_POINT ( 'NONE',  ( -8.154339323615371171, 11.60081407993821045, 1.199719254218453823 ) ) ;
#8107 = CARTESIAN_POINT ( 'NONE',  ( -5.815521545619021460, 5.749472989502435460, -0.7998128361456362523 ) ) ;
#8108 = CARTESIAN_POINT ( 'NONE',  ( 8.127223016387999266, 11.56917838817298616, 1.199719254218460707 ) ) ;
#8109 = CARTESIAN_POINT ( 'NONE',  ( 6.197485614778188712, 6.403023770095574108, -0.7216878364870458196 ) ) ;
#8110 = CARTESIAN_POINT ( 'NONE',  ( 4.768780016659259324, 6.770301073365750710, 1.244442160714388068 ) ) ;
#8111 = CARTESIAN_POINT ( 'NONE',  ( -3.475000000000000533, -0.6854166657107528815, -2.006292185433948827 ) ) ;
#8112 = CARTESIAN_POINT ( 'NONE',  ( -4.939248034080176097, 4.656877549381960080, 1.214306433183764966E-14 ) ) ;
#8113 = CARTESIAN_POINT ( 'NONE',  ( 0.2818602545999105424, 0.2096452599892709712, -2.211486639639495433 ) ) ;
#8114 = CARTESIAN_POINT ( 'NONE',  ( 2.081218647941612154, -0.1023907900198107734, -2.103586654547675128 ) ) ;
#8115 = CARTESIAN_POINT ( 'NONE',  ( -3.494969737272722643, 7.299491470118629088, -0.7998128361456481317 ) ) ;
#8116 = CARTESIAN_POINT ( 'NONE',  ( 8.749089199520284410, 9.101692242395490240, 0.7998128361456481317 ) ) ;
#8117 = CARTESIAN_POINT ( 'NONE',  ( 6.034019871906543209, 1.107478494666002344, 1.495390754572333725 ) ) ;
#8118 = CARTESIAN_POINT ( 'NONE',  ( 8.125414133291656071, 8.374071331795406081, -0.7998128361456291469 ) ) ;
#8119 = CARTESIAN_POINT ( 'NONE',  ( 3.449547071718269020, 5.499999999999998224, 2.024999999999999023 ) ) ;
#8120 = CARTESIAN_POINT ( 'NONE',  ( -5.750066545971566079, 8.762142499391876171, 1.082531754730550855 ) ) ;
#8121 = CARTESIAN_POINT ( 'NONE',  ( -8.351459436338030784, 11.72682452816096976, -1.082531754730543971 ) ) ;
#8122 =( BOUNDED_SURFACE ( )  B_SPLINE_SURFACE ( 3, 2, ( 
 ( #131936, #98333, #148159 ),
 ( #78865, #114648, #214160 ),
 ( #64754, #17050, #182766 ),
 ( #48528, #130896, #180641 ) ),
 .UNSPECIFIED., .F., .F., .T. ) 
 B_SPLINE_SURFACE_WITH_KNOTS ( ( 4, 4 ),
 ( 3, 3 ),
 ( 0.000000000000000000, 9.170893476602704462E-05 ),
 ( 0.000000000000000000, 1.000000000000000000 ),
 .UNSPECIFIED. ) 
 GEOMETRIC_REPRESENTATION_ITEM ( )  RATIONAL_B_SPLINE_SURFACE ( (
 ( 1.000000000000000000, 0.7100530722026798802, 1.000000000000000000),
 ( 1.000000000000000000, 0.6998898451682473709, 1.000000000000000000),
 ( 1.000000000000000000, 0.6894756946157520883, 1.000000000000000000),
 ( 1.000000000000000000, 0.6787756258918292707, 1.000000000000000000) ) ) 
 REPRESENTATION_ITEM ( '' )  SURFACE ( )  );
#8123 = CARTESIAN_POINT ( 'NONE',  ( -0.03470293633787284449, -1.699275230904277789, 1.268407768021381221 ) ) ;
#8124 = CARTESIAN_POINT ( 'NONE',  ( -7.774674742793745708, 8.035151719539642912, 0.7998128361456341429 ) ) ;
#8126 = CARTESIAN_POINT ( 'NONE',  ( 3.807043925254738781, -1.605251362286563177, 1.127602784832412386 ) ) ;
#8125 = CARTESIAN_POINT ( 'NONE',  ( -0.6125000000000001554, -0.4583333333332967330, 1.060881119635912029 ) ) ;
#8127 = CARTESIAN_POINT ( 'NONE',  ( 2.588937169860201504, -0.3686131662095324946, -2.129881858774537395 ) ) ;
#8129 = CARTESIAN_POINT ( 'NONE',  ( -4.639453055371920875, 6.917948375795638150, -1.210149155198399828 ) ) ;
#8128 = CARTESIAN_POINT ( 'NONE',  ( -4.553559489343377287, 6.405848385690952718, -1.599625672291271394 ) ) ;
#8130 = CARTESIAN_POINT ( 'NONE',  ( -0.6823417656250212460, 1.301041667008083547, 1.181850606188755259 ) ) ;
#8131 = CARTESIAN_POINT ( 'NONE',  ( 2.976183818757103250, -0.1284355763333933920, -1.735648432857107126 ) ) ;
#8132 = CARTESIAN_POINT ( 'NONE',  ( 5.002595493762530765, 8.780185809457538681, 1.040834085586084257E-14 ) ) ;
#8133 = CARTESIAN_POINT ( 'NONE',  ( -10.83922355283164229, 5.627439893072521571, -6.488667358217314884 ) ) ;
#8134 = VERTEX_POINT ( 'NONE', #207931 ) ;
#8135 = AXIS2_PLACEMENT_3D ( 'NONE', #26444, #24290, #92554 ) ;
#8136 = CARTESIAN_POINT ( 'NONE',  ( 2.653672528425448540, -0.3418824089525332455, -1.986742401007553172 ) ) ;
#8137 = FACE_OUTER_BOUND ( 'NONE', #57716, .T. ) ;
#8139 = PRESENTATION_LAYER_ASSIGNMENT (  '', '', ( #46201 ) ) ;
#8138 = CARTESIAN_POINT ( 'NONE',  ( 0.2687375195599971400, -1.410744835756465365, 1.637978619736128127 ) ) ;
#8140 = EDGE_CURVE ( 'NONE', #170253, #33524, #144837, .T. ) ;
#8141 = CARTESIAN_POINT ( 'NONE',  ( 2.078924955456124657, -0.09500079177627264448, -1.969288250925634642 ) ) ;
#8142 = CIRCLE ( 'NONE', #91200, 6.959052028703005099 ) ;
#8145 = ORIENTED_EDGE ( 'NONE', *, *, #159414, .F. ) ;
#8144 = CARTESIAN_POINT ( 'NONE',  ( -6.156811154381562012, 6.355570232966157640, 0.7216878364870257245 ) ) ;
#8143 = CARTESIAN_POINT ( 'NONE',  ( 6.521744167503259249, -0.4122283346772101509, 1.874327247564554266 ) ) ;
#8146 = CARTESIAN_POINT ( 'NONE',  ( -6.590672069574513792, 6.861741300691274859, 0.000000000000000000 ) ) ;
#8147 = CARTESIAN_POINT ( 'NONE',  ( 5.091969210384201361, 8.098325291160362482, 1.199719254218452047 ) ) ;
#8148 = CARTESIAN_POINT ( 'NONE',  ( -5.306037014901836990, 7.283738832175834510, 1.599625672291263179 ) ) ;
#8149 = CARTESIAN_POINT ( 'NONE',  ( 2.824872690137433029, 1.461285568133148693, -1.394416722739227898 ) ) ;
#8150 = CARTESIAN_POINT ( 'NONE',  ( 0.000000000000000000, 0.000000000000000000, 0.000000000000000000 ) ) ;
#8151 = CARTESIAN_POINT ( 'NONE',  ( 6.212023164884419302, -2.291203086667678690, 0.2740844210103609568 ) ) ;
#8152 = CARTESIAN_POINT ( 'NONE',  ( -4.559605246071192219, 3.300000000000025135, -0.7749999999999935829 ) ) ;
#8153 = CARTESIAN_POINT ( 'NONE',  ( 2.571086506140254357, 1.750134206675527437, 0.8865088104979682582 ) ) ;
#8154 = CARTESIAN_POINT ( 'NONE',  ( 9.935427640716063991, 10.48575375712389679, -0.7998128361456281477 ) ) ;
#8155 = CARTESIAN_POINT ( 'NONE',  ( 0.4225002777262388265, -1.427939226333583500, -1.423959630194884696 ) ) ;
#8156 = ORIENTED_EDGE ( 'NONE', *, *, #203953, .T. ) ;
#8157 = CARTESIAN_POINT ( 'NONE',  ( 2.167340134605561630, 1.933669477944195636, -0.8630234182349978411 ) ) ;
#8159 = CARTESIAN_POINT ( 'NONE',  ( -7.206322340863467346, 8.366129804884193888, 1.199719254218450271 ) ) ;
#8158 = SURFACE_STYLE_USAGE ( .BOTH. , #72072 ) ;
#8160 = CARTESIAN_POINT ( 'NONE',  ( 1.780954670855667388, 1.268887097626215876, 1.334285251370644021 ) ) ;
#8161 = ORIENTED_EDGE ( 'NONE', *, *, #209369, .T. ) ;
#8162 = CARTESIAN_POINT ( 'NONE',  ( -7.811469059767924605, 12.26513100303794168, -0.7998128361456281477 ) ) ;
#8163 = CARTESIAN_POINT ( 'NONE',  ( -1.468321960012643590, 7.242494692102438236, 4.289992922803264719 ) ) ;
#8164 = CARTESIAN_POINT ( 'NONE',  ( 3.955424862866574021, -1.843446357660895041, 1.048082435718917571 ) ) ;
#8165 = CARTESIAN_POINT ( 'NONE',  ( 6.685517510867199142, -0.8268063683338886527, 1.755141085440144355 ) ) ;
#8166 = FACE_OUTER_BOUND ( 'NONE', #138541, .T. ) ;
#8167 = CARTESIAN_POINT ( 'NONE',  ( 6.265839547809997079, 10.46189657242035587, 0.7998128361456462443 ) ) ;
#8168 = CARTESIAN_POINT ( 'NONE',  ( 5.515134625708930649, 9.656350506627580543, 0.000000000000000000 ) ) ;
#8169 = CARTESIAN_POINT ( 'NONE',  ( 4.710263567924342532, -0.8773996900517248010, -1.864791387430650094 ) ) ;
#8171 = CARTESIAN_POINT ( 'NONE',  ( 0.9074547957551477584, -0.8278116715597811925, -1.644758345054016191 ) ) ;
#8170 = CARTESIAN_POINT ( 'NONE',  ( -6.714312387265696458, 8.856450423275211037, 1.599625672291283607 ) ) ;
#8172 = CARTESIAN_POINT ( 'NONE',  ( -1.364683531250010295, 5.030208333674757171, 0.7879004041258379498 ) ) ;
#8173 = FACE_BOUND ( 'NONE', #130131, .T. ) ;
#8174 = CARTESIAN_POINT ( 'NONE',  ( -9.499607930503637832, -9.902952869712851935, 0.08630915044580420026 ) ) ;
#8175 = CARTESIAN_POINT ( 'NONE',  ( 2.889785579457926801, 6.440540434672812786, -0.3822207396134719715 ) ) ;
#8176 = CARTESIAN_POINT ( 'NONE',  ( 1.172829962703396456, -1.397616723802884708, 1.707921395779465890 ) ) ;
#8177 = CARTESIAN_POINT ( 'NONE',  ( 4.130342294306089457, 1.214786636354926452, -1.908452007788311366 ) ) ;
#8178 = CARTESIAN_POINT ( 'NONE',  ( -8.866669273657352690, 9.446795028796142191, 0.7216878364870438212 ) ) ;
#8179 = CARTESIAN_POINT ( 'NONE',  ( 3.656362025717549535, 1.803379273073001388, 0.1719060212231597329 ) ) ;
#8180 = CARTESIAN_POINT ( 'NONE',  ( 3.590956263468424225, 1.645886154840708659, 0.9800325279442632098 ) ) ;
#8181 = CARTESIAN_POINT ( 'NONE',  ( 3.701679681979888503, -1.565833156357125278, -1.354537944502069102 ) ) ;
#8182 = CARTESIAN_POINT ( 'NONE',  ( -1.364683531249997417, 4.071875000341417028, 1.214306433183764966E-14 ) ) ;
#8183 = CARTESIAN_POINT ( 'NONE',  ( 3.045733664408939223, 0.7109379216812520275, -1.838982635421481993 ) ) ;
#8184 = CARTESIAN_POINT ( 'NONE',  ( 0.7274102002729305738, -1.830281784476958773, 0.6011100631785198933 ) ) ;
#8185 = CARTESIAN_POINT ( 'NONE',  ( 3.748781033766034998, -1.529746656882627454, 1.076398355447941491 ) ) ;
#8186 = CARTESIAN_POINT ( 'NONE',  ( 1.999037954658490213, -0.6180237258119178900, -2.223338030673171151 ) ) ;
#8187 = CARTESIAN_POINT ( 'NONE',  ( 4.176097997218494839, -0.9553649929725913648, -1.596950837584124816 ) ) ;
#8188 = CARTESIAN_POINT ( 'NONE',  ( 1.364683531249988535, 4.113541667008088432, 0.7879004041258500513 ) ) ;
#8189 = CARTESIAN_POINT ( 'NONE',  ( -3.249150368769345043, 6.942425863539538611, 0.7998128361456341429 ) ) ;
#8190 = CARTESIAN_POINT ( 'NONE',  ( 7.298366762858032430, 7.409182732956175244, 1.040834085586084257E-14 ) ) ;
#8191 = CARTESIAN_POINT ( 'NONE',  ( 6.734029298721180723, -7.783114986501015409, 6.778728372092625243 ) ) ;
#8192 = CARTESIAN_POINT ( 'NONE',  ( 0.3816453311432427831, 1.964265557344764712, -0.7602060659359122230 ) ) ;
#8193 = CARTESIAN_POINT ( 'NONE',  ( 3.836594282542914236, 5.499112634431936542, 1.443375672974062551 ) ) ;
#8195 = CARTESIAN_POINT ( 'NONE',  ( 0.000000000000000000, -6.583980363594990948, 0.000000000000000000 ) ) ;
#8194 = CARTESIAN_POINT ( 'NONE',  ( 1.364683531249988535, 3.926041667008087543, 0.7879004041258500513 ) ) ;
#8196 = CARTESIAN_POINT ( 'NONE',  ( 2.426173717206762781, -2.096881089210366422, 0.3156149858808757203 ) ) ;
#8197 = CARTESIAN_POINT ( 'NONE',  ( 0.2815179179852530522, 0.1935487615560542163, -2.010460980806235920 ) ) ;
#8198 = CARTESIAN_POINT ( 'NONE',  ( -1.364683531250014514, 0.2385416670080863499, -0.7879004041258359514 ) ) ;
#8199 = CARTESIAN_POINT ( 'NONE',  ( -5.585596099150199834, 5.618876325204420930, -0.7216878364870207285 ) ) ;
#8200 = CARTESIAN_POINT ( 'NONE',  ( 4.313465427442102929, 8.184126765324453601, 0.7998128361456462443 ) ) ;
#8201 = CARTESIAN_POINT ( 'NONE',  ( 1.458524589769864210, 0.8745999688587955401, 1.976921506453344080 ) ) ;
#8204 = CARTESIAN_POINT ( 'NONE',  ( 3.714570900464274850, 6.317121236308204324, 1.082531754730558626 ) ) ;
#8203 = CARTESIAN_POINT ( 'NONE',  ( 2.273349394227877074, 5.683342515206170731, 0.4597581080974435519 ) ) ;
#8202 = CARTESIAN_POINT ( 'NONE',  ( 5.737035277238070385, 6.722237907313067140, -1.199719254218452047 ) ) ;
#8205 = CARTESIAN_POINT ( 'NONE',  ( -2.830620210203090181, 6.524417021870718258, 0.000000000000000000 ) ) ;
#8206 = CARTESIAN_POINT ( 'NONE',  ( 5.630092293170263495, 2.014432788975322630, 0.09412139267171715229 ) ) ;
#8208 = CARTESIAN_POINT ( 'NONE',  ( -4.895902867866254837, 7.765618208269001066, 1.082531754730549967 ) ) ;
#8207 = CARTESIAN_POINT ( 'NONE',  ( -7.185458225562757484, 11.32685899655781903, 0.7216878364870458196 ) ) ;
#8209 = CARTESIAN_POINT ( 'NONE',  ( -10.50000000000000000, 10.89999999999998259, 3.599999999999999201 ) ) ;
#8211 = CARTESIAN_POINT ( 'NONE',  ( 1.364683531249996529, 10.21354166700806587, 0.7879004041258403923 ) ) ;
#8210 = CARTESIAN_POINT ( 'NONE',  ( 0.5150084580479041829, 1.557691122620246116, -1.641117935488043633 ) ) ;
#8212 = CARTESIAN_POINT ( 'NONE',  ( -8.272446282632566650, 12.80293776304669962, 0.7998128361456481317 ) ) ;
#8214 = CARTESIAN_POINT ( 'NONE',  ( 1.194790368808082759, 1.690169533058868190, 0.9015364962996033071 ) ) ;
#8213 = CARTESIAN_POINT ( 'NONE',  ( -4.839897649954225223, 7.630002444046455778, 1.082531754730560403 ) ) ;
#8215 = CARTESIAN_POINT ( 'NONE',  ( -1.201851678989727383E-14, 1.384375000341419693, 1.575800808251672791 ) ) ;
#8216 = DIRECTION ( 'NONE',  ( 3.330669073875479482E-16, -3.330669073875479482E-16, -1.000000000000000000 ) ) ;
#8217 = CARTESIAN_POINT ( 'NONE',  ( -1.500000000000008216, 8.500000000000000000, 3.469446951953614189E-15 ) ) ;
#8218 = CARTESIAN_POINT ( 'NONE',  ( 2.384998569339055408, 1.577468512335476358, -0.6981430484895093658 ) ) ;
#8219 = CARTESIAN_POINT ( 'NONE',  ( 4.085803189671889157, 5.860132702740892263, -1.599625672291273171 ) ) ;
#8220 = CARTESIAN_POINT ( 'NONE',  ( 4.044074958626150185, 7.940114228364351767, 0.7998128361456271485 ) ) ;
#8221 = CARTESIAN_POINT ( 'NONE',  ( 1.352431244980515146, -1.399367522912741135, 1.083307108726710100 ) ) ;
#8222 = AXIS2_PLACEMENT_3D ( 'NONE', #178795, #80206, #210196 ) ;
#8223 = CARTESIAN_POINT ( 'NONE',  ( 2.385404357411140541, 0.09669159202466531822, -2.010876702762071311 ) ) ;
#8224 = SURFACE_SIDE_STYLE ('',( #191232 ) ) ;
#8225 = CARTESIAN_POINT ( 'NONE',  ( 9.642873567817520808, 12.27310513391906532, 1.599625672291279388 ) ) ;
#8226 = CARTESIAN_POINT ( 'NONE',  ( 3.698430944683338328, -2.204125419102770600, -0.1106900096672913392 ) ) ;
#8227 = AXIS2_PLACEMENT_3D ( 'NONE', #91337, #213301, #126026 ) ;
#8228 = ORIENTED_EDGE ( 'NONE', *, *, #1351, .F. ) ;
#8229 = CARTESIAN_POINT ( 'NONE',  ( 8.934460041281305109, 10.48625347199211966, -1.082531754730543083 ) ) ;
#8231 = CARTESIAN_POINT ( 'NONE',  ( 3.304314702139679039, 1.277028363417181289, -1.560513873864778578 ) ) ;
#8230 = CARTESIAN_POINT ( 'NONE',  ( 3.914780425095893968, -0.6665358524936614293, -2.013057630646164942 ) ) ;
#8233 = ORIENTED_EDGE ( 'NONE', *, *, #206552, .T. ) ;
#8232 = CARTESIAN_POINT ( 'NONE',  ( 3.339928375916663139, -1.083189831351333954, -1.451890931963683684 ) ) ;
#8234 = CARTESIAN_POINT ( 'NONE',  ( 5.143339171537801846, 7.093924681584509173, 1.599625672291269396 ) ) ;
#8235 = ORIENTED_EDGE ( 'NONE', *, *, #138098, .F. ) ;
#8236 = EDGE_CURVE ( 'NONE', #60515, #145094, #31973, .T. ) ;
#8237 = CARTESIAN_POINT ( 'NONE',  ( 1.024039198018782626, 1.117340804906666873, -1.500143343703803422 ) ) ;
#8238 = CARTESIAN_POINT ( 'NONE',  ( 6.234959169399230561, 0.1841439077357870380, 1.816378869960999509 ) ) ;
#8239 = CARTESIAN_POINT ( 'NONE',  ( -2.656508033273816238, 5.186677574539687363, -1.199719254218446718 ) ) ;
#8240 = DIRECTION ( 'NONE',  ( 0.000000000000000000, 8.546850786086437571E-32, 1.000000000000000000 ) ) ;
#8241 = CARTESIAN_POINT ( 'NONE',  ( -15.75000000000000000, 13.39999999999998259, 1.799999999999999600 ) ) ;
#8242 = CARTESIAN_POINT ( 'NONE',  ( -1.364683531250000748, 1.321875000341421469, 0.000000000000000000 ) ) ;
#8243 = CARTESIAN_POINT ( 'NONE',  ( 11.94105721237523277, 13.40000000000000036, -1.187919463087249827 ) ) ;
#8244 = CARTESIAN_POINT ( 'NONE',  ( 7.024532985656136930, 8.328281583754568729, 1.082531754730549967 ) ) ;
#8245 = CARTESIAN_POINT ( 'NONE',  ( -5.492461627311929995, 5.580495784718250363, 0.000000000000000000 ) ) ;
#8246 = CARTESIAN_POINT ( 'NONE',  ( -6.882699257592852504, 8.058845884393651460, -1.199719254218452047 ) ) ;
#8247 = CARTESIAN_POINT ( 'NONE',  ( 4.482752736079084421, -1.382999391253452615, 1.607682512923855445 ) ) ;
#8249 = CARTESIAN_POINT ( 'NONE',  ( -10.07169253693141897, 5.946554136026001913, 5.792750394403223702 ) ) ;
#8248 = CARTESIAN_POINT ( 'NONE',  ( -0.02968770228137587730, 2.889947918782026726, -2.315223470976325526 ) ) ;
#8250 = CARTESIAN_POINT ( 'NONE',  ( 4.200430055897656167, -0.6152532741215356316, -1.872979577440760046 ) ) ;
#8251 = CARTESIAN_POINT ( 'NONE',  ( -0.6823417656250003738, 1.717708333674752730, -1.181850606188749264 ) ) ;
#8252 = CARTESIAN_POINT ( 'NONE',  ( 6.398695753475230674, -1.876852914212179035, -0.3660984893600614520 ) ) ;
#8253 = VERTEX_POINT ( 'NONE', #161341 ) ;
#8254 = CARTESIAN_POINT ( 'NONE',  ( 0.2283145101530216492, 2.111890517744571927, 0.1509969543822299032 ) ) ;
#8255 = CARTESIAN_POINT ( 'NONE',  ( 6.928203230275514990, 14.48195938056239385, 9.797958971132711525 ) ) ;
#8256 = CARTESIAN_POINT ( 'NONE',  ( 1.258353326579707776, -2.070544811992577561, -0.001879966208345739808 ) ) ;
#8257 = CARTESIAN_POINT ( 'NONE',  ( 5.332099551924443404, 9.442809587212341427, 0.000000000000000000 ) ) ;
#8258 = CARTESIAN_POINT ( 'NONE',  ( 6.690022453700429139, 6.769724048930809701, 0.7998128361456331437 ) ) ;
#8259 = CARTESIAN_POINT ( 'NONE',  ( 7.201315867513990554, 8.430565262634994284, -1.199719254218452047 ) ) ;
#8261 = CARTESIAN_POINT ( 'NONE',  ( 4.330940004561544043, 7.140181541042074365, -1.199719254218452047 ) ) ;
#8260 = CARTESIAN_POINT ( 'NONE',  ( 3.486350522754261494, -0.4081323730865527577, -2.050228346494194831 ) ) ;
#8262 = CARTESIAN_POINT ( 'NONE',  ( 5.840530312436913007, 10.03597880781023299, 0.000000000000000000 ) ) ;
#8265 = ORIENTED_EDGE ( 'NONE', *, *, #28369, .T. ) ;
#8264 = CARTESIAN_POINT ( 'NONE',  ( 1.172180985828397581, 0.7336035429467204771, 1.656470807091579900 ) ) ;
#8263 = CARTESIAN_POINT ( 'NONE',  ( 1.852308540880560850, 0.5694407911355814367, 1.734573797025913189 ) ) ;
#8266 = CARTESIAN_POINT ( 'NONE',  ( 6.041676539500916654, -1.595688354349385607, -1.524751901930617715 ) ) ;
#8267 = CARTESIAN_POINT ( 'NONE',  ( 4.650083499807235121, 5.295740330745369207, 1.082471891955963716 ) ) ;
#8268 = CARTESIAN_POINT ( 'NONE',  ( 4.260898339918250066, -1.637375743694971408, 1.479669880875638777 ) ) ;
#8269 = CARTESIAN_POINT ( 'NONE',  ( 8.457588896826466751, 8.761608555919362828, 1.040834085586084257E-14 ) ) ;
#8270 = CARTESIAN_POINT ( 'NONE',  ( 1.364683531249996529, 8.526041667008065872, 0.7879004041258403923 ) ) ;
#8271 = CARTESIAN_POINT ( 'NONE',  ( 2.473184984502617478, -1.664690511387197702, -0.9409074295685518896 ) ) ;
#8272 = CARTESIAN_POINT ( 'NONE',  ( 7.425061681778431399, 11.81432239538354345, 0.7998128361456462443 ) ) ;
#8273 = CARTESIAN_POINT ( 'NONE',  ( 5.793440749948310042, -1.873300974885267589, 0.8818263447485861217 ) ) ;
#8275 = FACE_OUTER_BOUND ( 'NONE', #127862, .T. ) ;
#8274 = CARTESIAN_POINT ( 'NONE',  ( 1.530444406200885954, 8.694995975526813581, -2.517029436271772003 ) ) ;
#8276 = CARTESIAN_POINT ( 'NONE',  ( 5.776942576169182608, 2.025397260235710206, -0.8375503648087383457 ) ) ;
#8277 = ORIENTED_EDGE ( 'NONE', *, *, #163792, .T. ) ;
#8278 = ORIENTED_EDGE ( 'NONE', *, *, #199264, .F. ) ;
#8279 = CARTESIAN_POINT ( 'NONE',  ( 3.475000000000000533, -2.202083332377416713, -2.006292185433951047 ) ) ;
#8280 = CARTESIAN_POINT ( 'NONE',  ( 0.000000000000000000, 4.000000000000003553, 0.000000000000000000 ) ) ;
#8281 = CARTESIAN_POINT ( 'NONE',  ( 4.655245641445829641, 6.524482229810530498, 1.599625672291269396 ) ) ;
#8282 = DIRECTION ( 'NONE',  ( 0.000000000000000000, 1.000000000000000000, 0.000000000000000000 ) ) ;
#8283 = CIRCLE ( 'NONE', #77555, 0.7499999999999997780 ) ;
#8284 = CARTESIAN_POINT ( 'NONE',  ( -7.537970219518075332, 10.77775377520434574, -1.082531754730543971 ) ) ;
#8285 = CARTESIAN_POINT ( 'NONE',  ( 5.585032934186686226, 5.480569609498057382, 0.000000000000000000 ) ) ;
#8286 = CARTESIAN_POINT ( 'NONE',  ( 5.260626886859606444, -0.6923115906582855139, -1.951227211109484383 ) ) ;
#8288 = EDGE_CURVE ( 'NONE', #112905, #202900, #86587, .T. ) ;
#8287 = CARTESIAN_POINT ( 'NONE',  ( 4.231024032915966515, 0.09596189134018082156, 1.924231256547383362 ) ) ;
#8289 = CARTESIAN_POINT ( 'NONE',  ( 6.433232048832024930, -1.700592621796994441, -1.261046147972416875 ) ) ;
#8290 = VECTOR ( 'NONE', #86267, 1000.000000000000000 ) ;
#8291 = CYLINDRICAL_SURFACE ( 'NONE', #128927, 0.3999999999999997446 ) ;
#8292 = CARTESIAN_POINT ( 'NONE',  ( 7.828907357248368726, 8.098423103070084395, 0.7998128361456281477 ) ) ;
#8293 = CARTESIAN_POINT ( 'NONE',  ( 6.580031643469963498, -2.246689805010111396, -0.4540597329640746471 ) ) ;
#8294 = CARTESIAN_POINT ( 'NONE',  ( 4.898959864523320107, 1.516061528642864253, -1.016892643307308441 ) ) ;
#8295 = CARTESIAN_POINT ( 'NONE',  ( 6.536439455564168277, 6.798469917679251573, 0.7216878364870328300 ) ) ;
#8296 = CARTESIAN_POINT ( 'NONE',  ( 2.670593071767634719, 6.059516317130127838, -0.7216878364870267237 ) ) ;
#8297 = CARTESIAN_POINT ( 'NONE',  ( -6.981522756394290319, 7.109807735406931783, 0.7998128361456341429 ) ) ;
#8298 = CARTESIAN_POINT ( 'NONE',  ( 5.138703914779377158, 5.953908307786102583, 1.199719254218462483 ) ) ;
#8299 = CARTESIAN_POINT ( 'NONE',  ( 5.727393547130178675, 5.646656991265468939, 0.000000000000000000 ) ) ;
#8300 =( BOUNDED_SURFACE ( )  B_SPLINE_SURFACE ( 3, 2, ( 
 ( #163682, #110725, #210271 ),
 ( #197221, #15264, #132268 ),
 ( #114976, #194027, #129132 ),
 ( #113930, #146383, #97624 ),
 ( #61909, #195108, #30484 ),
 ( #46744, #81351, #131233 ) ),
 .UNSPECIFIED., .F., .F., .F. ) 
 B_SPLINE_SURFACE_WITH_KNOTS ( ( 4, 2, 4 ),
 ( 3, 3 ),
 ( 0.000000000000000000, 0.0003754691837024766443, 0.0007509383674049532886 ),
 ( 0.000000000000000000, 1.000000000000000000 ),
 .UNSPECIFIED. ) 
 GEOMETRIC_REPRESENTATION_ITEM ( )  RATIONAL_B_SPLINE_SURFACE ( (
 ( 1.000000000000000000, 0.6711954675835484219, 1.000000000000000000),
 ( 1.000000000000000000, 0.6709646295272747585, 1.000000000000000000),
 ( 1.000000000000000000, 0.6771840716652173242, 1.000000000000000000),
 ( 1.000000000000000000, 0.6927481755874340674, 1.000000000000000000),
 ( 1.000000000000000000, 0.7017972101304913446, 1.000000000000000000),
 ( 1.000000000000000000, 0.7071067811865399122, 1.000000000000000000) ) ) 
 REPRESENTATION_ITEM ( '' )  SURFACE ( )  );
#8301 = VERTEX_POINT ( 'NONE', #127865 ) ;
#8303 = CARTESIAN_POINT ( 'NONE',  ( 6.486586620031766337, -1.235515937849906321, 1.590312944162165287 ) ) ;
#8302 = CARTESIAN_POINT ( 'NONE',  ( 2.436835438956724165, -1.365703447793526371, -1.235134912642745775 ) ) ;
#8304 = CARTESIAN_POINT ( 'NONE',  ( 0.8787516259003292918, -0.3353366030727308877, 2.273710652787809039 ) ) ;
#8305 = CARTESIAN_POINT ( 'NONE',  ( 6.368018226480639754, -1.947316962026977682, 0.2367824842242904348 ) ) ;
#8306 = CARTESIAN_POINT ( 'NONE',  ( -5.850506979496850057, 6.784345216623154151, -1.199719254218446718 ) ) ;
#8307 = CARTESIAN_POINT ( 'NONE',  ( -4.073660332270687690, 7.638349725183815053, -0.4663290683490532995 ) ) ;
#8308 = CARTESIAN_POINT ( 'NONE',  ( -4.135400547368138113, 4.783387712472935149, 1.199719254218462483 ) ) ;
#8309 = CARTESIAN_POINT ( 'NONE',  ( 0.6607010325807397555, -0.6960017893198193750, -1.950014918625786020 ) ) ;
#8310 = CARTESIAN_POINT ( 'NONE',  ( -3.149236820124241110, 6.896136400112061970, -0.7998128361456481317 ) ) ;
#8312 = CARTESIAN_POINT ( 'NONE',  ( 1.621729638615863944, -1.036547396872866678, -1.557007864774778705 ) ) ;
#8311 = CARTESIAN_POINT ( 'NONE',  ( 3.017214641935324071, -2.014214092474704731, 0.5601794093188486867 ) ) ;
#8313 = CARTESIAN_POINT ( 'NONE',  ( 2.108749758911751204, 0.7741990562295970602, -1.861730988020185329 ) ) ;
#8314 = CARTESIAN_POINT ( 'NONE',  ( 9.571693261567965294, 10.26932301469188857, 0.7216878364870438212 ) ) ;
#8315 = ORIENTED_EDGE ( 'NONE', *, *, #92877, .F. ) ;
#8316 = CARTESIAN_POINT ( 'NONE',  ( -1.364683531250012516, 4.051041667008088432, -0.7879004041258300672 ) ) ;
#8317 = CARTESIAN_POINT ( 'NONE',  ( 2.507021497916587460, -1.721230695331811722, 0.2570161617474544524 ) ) ;
#8318 = CARTESIAN_POINT ( 'NONE',  ( 4.852928918687680948, 7.749168607522574526, 1.199719254218462483 ) ) ;
#8320 = CARTESIAN_POINT ( 'NONE',  ( 0.3548627404530421137, 3.214704059642509826, -1.969391935101212576 ) ) ;
#8319 = CARTESIAN_POINT ( 'NONE',  ( 0.000000000000000000, -2.859583229930517945E-15, 6.399999999999999467 ) ) ;
#8321 = CARTESIAN_POINT ( 'NONE',  ( 3.000334558935643603, -0.5012536917932303160, -1.650428355875031228 ) ) ;
#8322 = CARTESIAN_POINT ( 'NONE',  ( 3.087623348389135547, -0.8860277256741244667, 2.004638750299721828 ) ) ;
#8323 = CARTESIAN_POINT ( 'NONE',  ( 0.1758332513315676859, 1.282751065617006248, 1.167194905859494591 ) ) ;
#8324 = CARTESIAN_POINT ( 'NONE',  ( 5.426482453889071245, 1.317083479513626587, -1.770629405693980640 ) ) ;
#8325 = CARTESIAN_POINT ( 'NONE',  ( -9.541882734523161602, 5.027466607964795386, -6.730450668810338044 ) ) ;
#8326 = CARTESIAN_POINT ( 'NONE',  ( 2.008858235458183650, 0.6779177425604805407, 2.062613225174831921 ) ) ;
#8327 = CARTESIAN_POINT ( 'NONE',  ( 1.558932953716257730, -1.564965500463588732, -0.9399777662534372080 ) ) ;
#8328 = CARTESIAN_POINT ( 'NONE',  ( 4.786377933101198856, -0.7163331637287263520, -1.992584184115009149 ) ) ;
#8329 = CARTESIAN_POINT ( 'NONE',  ( 6.539320575229287336, 7.629137130509086262, 2.596737603865982624 ) ) ;
#8330 = ORIENTED_EDGE ( 'NONE', *, *, #26436, .T. ) ;
#8332 = CARTESIAN_POINT ( 'NONE',  ( 1.364683531249988535, 1.426041667008083991, 0.7879004041258500513 ) ) ;
#8331 = CARTESIAN_POINT ( 'NONE',  ( 4.230218865515364968, 2.248128804489764043, 0.4474220685124987162 ) ) ;
#8333 = DIRECTION ( 'NONE',  ( -1.000000000000000000, -1.725633230170963762E-31, -8.638326563840814399E-31 ) ) ;
#8334 = CARTESIAN_POINT ( 'NONE',  ( 3.785751206713845018, 5.439795712631356750, 1.599625672291267398 ) ) ;
#8335 = CARTESIAN_POINT ( 'NONE',  ( 0.7156801077207708417, 1.735845614737155707, 1.217653249118654468 ) ) ;
#8336 = CARTESIAN_POINT ( 'NONE',  ( -4.419594888374909658, 8.100018436505289188, 0.7216878364870458196 ) ) ;
#8337 = CARTESIAN_POINT ( 'NONE',  ( 2.548569689688999329, 5.917155704705049146, -0.7216878364870267237 ) ) ;
#8338 = CARTESIAN_POINT ( 'NONE',  ( -6.521108698048783126, 7.670676904887464786, -1.082531754730543083 ) ) ;
#8339 = CARTESIAN_POINT ( 'NONE',  ( 3.119784744920330422, 6.653849612466795627, 0.7216878364870257245 ) ) ;
#8340 = AXIS2_PLACEMENT_3D ( 'NONE', #99507, #202026, #32373 ) ;
#8341 = VERTEX_POINT ( 'NONE', #45463 ) ;
#8342 = CARTESIAN_POINT ( 'NONE',  ( 5.449842333688053486, -1.824117940560719298, -0.8596331684956670660 ) ) ;
#8344 = CARTESIAN_POINT ( 'NONE',  ( 3.502832280938583676, 0.4964207669093263497, 2.001847840641638232 ) ) ;
#8343 = CARTESIAN_POINT ( 'NONE',  ( 4.476163270806094552, 8.373940915915776273, 0.7998128361456462443 ) ) ;
#8345 = CARTESIAN_POINT ( 'NONE',  ( 6.749980374757213575, 8.968339418673846097, 1.599625672291268286 ) ) ;
#8346 = CARTESIAN_POINT ( 'NONE',  ( 3.228249973385329596, 6.780392379009261283, -1.734723475976807094E-15 ) ) ;
#8347 = CARTESIAN_POINT ( 'NONE',  ( 3.285556943750000514, -3.813541666188710710, 1.896917185911906500 ) ) ;
#8348 = FACE_OUTER_BOUND ( 'NONE', #113636, .T. ) ;
#8349 = CARTESIAN_POINT ( 'NONE',  ( 6.439412520197737244, 0.8424478218750917069, -2.023249321508275855 ) ) ;
#8350 = CARTESIAN_POINT ( 'NONE',  ( 3.375625116643202972, -0.3961014713874110305, -1.976955985980306307 ) ) ;
#8351 = CARTESIAN_POINT ( 'NONE',  ( 3.052128622409277181, -1.392423357299840792, 1.204796875372941667 ) ) ;
#8352 = CARTESIAN_POINT ( 'NONE',  ( 6.500244582748090139, 9.671036882259738121, 1.199719254218460707 ) ) ;
#8353 = CARTESIAN_POINT ( 'NONE',  ( 6.827182134110196365, 0.003888933837258023128, 1.810856214465895508 ) ) ;
#8354 = CARTESIAN_POINT ( 'NONE',  ( 0.2648075084464130979, 2.141788565065712913, -0.8351287359565621182 ) ) ;
#8355 = CARTESIAN_POINT ( 'NONE',  ( -5.703176172842872482, 9.805455968292021041, 0.000000000000000000 ) ) ;
#8356 = CARTESIAN_POINT ( 'NONE',  ( 6.403223674518304875, 1.876769595090790554, 1.263360297164903168 ) ) ;
#8357 = CARTESIAN_POINT ( 'NONE',  ( 1.524195097446314318, -1.171203135327163913, -1.750160316008353201 ) ) ;
#8358 = CARTESIAN_POINT ( 'NONE',  ( -5.367048706163331850, 7.354919138647580290, -1.599625672291271394 ) ) ;
#8359 = CARTESIAN_POINT ( 'NONE',  ( 9.101601193475611140, 9.512956235343358102, -0.7998128361456221525 ) ) ;
#8360 = CARTESIAN_POINT ( 'NONE',  ( 8.136301581532414673, 8.664975731308866003, 0.000000000000000000 ) ) ;
#8361 = DIRECTION ( 'NONE',  ( -0.8516084350226855726, 0.000000000000000000, 0.5241784747566542446 ) ) ;
#8363 = ADVANCED_FACE ( 'NONE', ( #62749 ), #34073, .T. ) ;
#8362 = CARTESIAN_POINT ( 'NONE',  ( -5.551173829791513192, 8.563787670477010394, 1.199719254218452047 ) ) ;
#8364 = CARTESIAN_POINT ( 'NONE',  ( 7.090551149822728938, 10.25576486055978442, 1.082531754730558626 ) ) ;
#8365 = CARTESIAN_POINT ( 'NONE',  ( 4.051511279158463985, 7.758049153162790645, -0.5006740859710266944 ) ) ;
#8366 = CARTESIAN_POINT ( 'NONE',  ( -4.761938266897808525, 6.578680616179308771, 1.599625672291267398 ) ) ;
#8367 = CARTESIAN_POINT ( 'NONE',  ( 3.937882119624159127, -2.125045857649208614, 0.6470787896058221023 ) ) ;
#8368 = CARTESIAN_POINT ( 'NONE',  ( 1.693587955360946529, -0.7361150630936144079, 2.064250245950305374 ) ) ;
#8369 = CARTESIAN_POINT ( 'NONE',  ( 0.3994152196779980346, 1.832435997337564348, -1.229551327501000380 ) ) ;
#8370 = CARTESIAN_POINT ( 'NONE',  ( -3.800028193580205382, 7.655393002477360653, -0.7998128361456481317 ) ) ;
#8371 = CARTESIAN_POINT ( 'NONE',  ( 4.510177812457000002, 1.961482754637720927, -0.04604004567236585910 ) ) ;
#8372 = CARTESIAN_POINT ( 'NONE',  ( 8.757677159423465696, 12.30470822171437284, 1.199719254218450271 ) ) ;
#8373 = FACE_OUTER_BOUND ( 'NONE', #100184, .T. ) ;
#8374 = CARTESIAN_POINT ( 'NONE',  ( 1.364683531249986537, 0.3635416670080869328, 0.7879004041258500513 ) ) ;
#8375 = CARTESIAN_POINT ( 'NONE',  ( 6.610000000000001208, 3.709748940453510446, 2.234587373521100151 ) ) ;
#8377 = EDGE_LOOP ( 'NONE', ( #172657, #93375, #55514, #112718 ) ) ;
#8376 = CARTESIAN_POINT ( 'NONE',  ( -4.772106882330223954, 8.511282429453158827, -0.7216878364870267237 ) ) ;
#8378 = CARTESIAN_POINT ( 'NONE',  ( 3.006218798242997980, -0.8556837461295877523, 1.940463308995137526 ) ) ;
#8379 = CARTESIAN_POINT ( 'NONE',  ( -3.311934663488232733, 7.085950550703385531, -0.7998128361456481317 ) ) ;
#8380 = CARTESIAN_POINT ( 'NONE',  ( 5.190363053866647647, -2.144918610114197488, -0.2683968819863768451 ) ) ;
#8381 = CARTESIAN_POINT ( 'NONE',  ( 4.194743914777058436, 1.481411246205705412, 1.093257649623424754 ) ) ;
#8382 = B_SPLINE_CURVE_WITH_KNOTS ( 'NONE', 3,
 ( #145180, #14041, #78000, #111641, #62810, #60680, #163527, #178716 ),
 .UNSPECIFIED., .F., .F.,
 ( 4, 2, 2, 4 ),
 ( 1.064888869118105810E-15, 0.0004636157603174413970, 0.0006954236404756280717, 0.0009272315206338146380 ),
 .UNSPECIFIED. ) ;
#8383 = CARTESIAN_POINT ( 'NONE',  ( -5.911556925646939575, 6.000462466000660022, -0.05029327469607651480 ) ) ;
#8384 = CARTESIAN_POINT ( 'NONE',  ( -0.6823417656250212460, 0.8635416670080899859, 1.181850606188755259 ) ) ;
#8385 = CARTESIAN_POINT ( 'NONE',  ( 0.4854153416827499679, -1.726952712381021326, -0.2154422717644439433 ) ) ;
#8386 = CARTESIAN_POINT ( 'NONE',  ( 6.827182134110209688, 6.038954451951505042, 2.405852596708078384 ) ) ;
#8387 = CARTESIAN_POINT ( 'NONE',  ( 2.223174002961016082, 5.537527403522402025, -0.7216878364870267237 ) ) ;
#8388 = CARTESIAN_POINT ( 'NONE',  ( 11.78331023100045627, 13.79999999999999893, -1.800000000000001155 ) ) ;
#8389 = CARTESIAN_POINT ( 'NONE',  ( 4.610339536224768331, -0.9213992672730475508, -1.955631277330005968 ) ) ;
#8390 = CARTESIAN_POINT ( 'NONE',  ( -5.434120640978981065, 5.234228924097238611, -0.7998128361456221525 ) ) ;
#8391 = CARTESIAN_POINT ( 'NONE',  ( 5.606796008369615336, 0.8196459417171353401, -1.842166028910074527 ) ) ;
#8392 = CARTESIAN_POINT ( 'NONE',  ( -8.798878505144665851, 9.367705798864669475, -0.7216878364870267237 ) ) ;
#8393 = CARTESIAN_POINT ( 'NONE',  ( 3.608425205800522839, -0.8741791752944136906, -1.977237025433141504 ) ) ;
#8394 = CARTESIAN_POINT ( 'NONE',  ( 4.007068486172041588, 1.689080509644375505, 1.016306131198143836 ) ) ;
#8395 = CARTESIAN_POINT ( 'NONE',  ( -0.09540182900466381843, -7.837949925775446580, 10.99983588129881618 ) ) ;
#8396 = CARTESIAN_POINT ( 'NONE',  ( 0.5523711044835468709, 0.7197940642212009577, -2.192503933474987843 ) ) ;
#8397 = CARTESIAN_POINT ( 'NONE',  ( 3.321608758505911307, -1.986990267296639745, 0.5463351552400242950 ) ) ;
#8398 = CARTESIAN_POINT ( 'NONE',  ( 5.724156413028869572, 1.872829174467111946, 0.5137480774947185136 ) ) ;
#8399 = CARTESIAN_POINT ( 'NONE',  ( -6.832946231163084860, 10.91559500309152675, 0.000000000000000000 ) ) ;
#8400 = CARTESIAN_POINT ( 'NONE',  ( -5.498713818794216834, 8.572860667638675380, -1.199719254218452047 ) ) ;
#8401 = DIRECTION ( 'NONE',  ( 0.000000000000000000, 0.000000000000000000, 1.000000000000000000 ) ) ;
#8403 = ORIENTED_EDGE ( 'NONE', *, *, #134540, .F. ) ;
#8402 = CARTESIAN_POINT ( 'NONE',  ( -2.979759899953417612, 6.698413326579433225, 0.7998128361456352531 ) ) ;
#8404 = CARTESIAN_POINT ( 'NONE',  ( -8.310784975052685652, 9.758632561392040827, -1.082531754730543083 ) ) ;
#8405 = CARTESIAN_POINT ( 'NONE',  ( 2.555956245031346885, 0.5892994983645870599, -2.126554282292691500 ) ) ;
#8406 = CARTESIAN_POINT ( 'NONE',  ( -3.285556943750000514, -3.376041666188708490, -1.896917185911906500 ) ) ;
#8407 = ORIENTED_EDGE ( 'NONE', *, *, #80469, .T. ) ;
#8408 = CARTESIAN_POINT ( 'NONE',  ( 6.578960362708798471, 1.829258725439562916, 0.7091506158454219388 ) ) ;
#8409 = CARTESIAN_POINT ( 'NONE',  ( 6.539320575229281118, 7.629137130509070275, 2.703262396134015866 ) ) ;
#8410 = CARTESIAN_POINT ( 'NONE',  ( 1.499999999999989120, 5.327083334016152527, -0.8660254037844323793 ) ) ;
#8411 = SURFACE_STYLE_USAGE ( .BOTH. , #141670 ) ;
#8413 = CARTESIAN_POINT ( 'NONE',  ( 0.4019237886466814902, 12.60491455036742892, 1.499999999999999334 ) ) ;
#8412 = CARTESIAN_POINT ( 'NONE',  ( 1.499999999999964695, 5.077083334016150751, -0.8660254037844461461 ) ) ;
#8414 = CARTESIAN_POINT ( 'NONE',  ( 5.244037021109955177, 0.5378974813256987009, 1.760811445753920568 ) ) ;
#8415 = ORIENTED_EDGE ( 'NONE', *, *, #18341, .T. ) ;
#8416 = CARTESIAN_POINT ( 'NONE',  ( 2.149359023125880341, -1.654445155856735905, -1.228624528962230400 ) ) ;
#8417 = CARTESIAN_POINT ( 'NONE',  ( 1.360316468750000896, 0.7656250003413994643, 0.000000000000000000 ) ) ;
#8418 = CARTESIAN_POINT ( 'NONE',  ( -5.845536785786364931, 9.971543350059432598, 0.000000000000000000 ) ) ;
#8419 = CARTESIAN_POINT ( 'NONE',  ( 7.013428937081386927, 5.939655416065874327, 2.436399677959149468 ) ) ;
#8420 = VECTOR ( 'NONE', #46689, 1000.000000000000000 ) ;
#8421 = CARTESIAN_POINT ( 'NONE',  ( 4.364835388595708743, 7.179726155748598515, 1.199719254218462483 ) ) ;
#8422 = CARTESIAN_POINT ( 'NONE',  ( 0.5321925127804688627, 1.059884587108523402, -1.767317575122410167 ) ) ;
#8424 = CARTESIAN_POINT ( 'NONE',  ( 4.774869596704574448, 1.716175909155163382, -0.6674964387535023969 ) ) ;
#8423 = DIRECTION ( 'NONE',  ( -0.000000000000000000, 1.000000000000000000, -0.000000000000000000 ) ) ;
#8425 = CARTESIAN_POINT ( 'NONE',  ( 7.121056995675668411, 9.330985799753529264, -1.599625672291262513 ) ) ;
#8426 = CARTESIAN_POINT ( 'NONE',  ( -6.981522756394290319, 7.109807735406931783, 0.7998128361456341429 ) ) ;
#8427 = ORIENTED_EDGE ( 'NONE', *, *, #18617, .F. ) ;
#8428 = CARTESIAN_POINT ( 'NONE',  ( 4.248781725523794073, 0.5872999373685274804, 2.127227798101683387 ) ) ;
#8429 = CARTESIAN_POINT ( 'NONE',  ( 0.5796411875719498230, 2.017120475678677582, -0.7774783797904263327 ) ) ;
#8430 = CARTESIAN_POINT ( 'NONE',  ( -4.270455198624581783, 7.926022131796578662, 1.040834085586084257E-14 ) ) ;
#8431 = CARTESIAN_POINT ( 'NONE',  ( 0.03522015555855115276, -0.09184495783944729430, 1.910282976853895587 ) ) ;
#8432 = CARTESIAN_POINT ( 'NONE',  ( 6.403544266003773799, -1.856299428965903164, 0.4729442951737494183 ) ) ;
#8433 = CARTESIAN_POINT ( 'NONE',  ( 6.495764994278795612, 9.632124022417032805, 1.082531754730549078 ) ) ;
#8434 = DIRECTION ( 'NONE',  ( 0.000000000000000000, 0.000000000000000000, 1.000000000000000000 ) ) ;
#8435 = CARTESIAN_POINT ( 'NONE',  ( 6.340485057729076779, 1.096952271789692901, -1.566184530335120950 ) ) ;
#8436 =( LENGTH_UNIT ( ) NAMED_UNIT ( * ) SI_UNIT ( .MILLI., .METRE. ) );
#8437 = VECTOR ( 'NONE', #174577, 1000.000000000000000 ) ;
#8438 = CARTESIAN_POINT ( 'NONE',  ( 1.076777757339364205, -0.04213119042271313425, -1.870346338061685154 ) ) ;
#8439 = CARTESIAN_POINT ( 'NONE',  ( 2.395720570290179374, -1.993893129684479293, 0.3006499569925198956 ) ) ;
#8441 = CARTESIAN_POINT ( 'NONE',  ( -5.515163814073178905, 6.606792650666174715, 1.108724247552300701 ) ) ;
#8440 = CARTESIAN_POINT ( 'NONE',  ( -1.364683531250012516, 1.280208333674755172, 0.7879004041258379498 ) ) ;
#8443 = CARTESIAN_POINT ( 'NONE',  ( 4.125680639212436773, -2.015421878069530326, 0.6112012065569141228 ) ) ;
#8442 = CARTESIAN_POINT ( 'NONE',  ( -8.422639742587602285, 10.84949900448412841, -1.599625672291263179 ) ) ;
#8444 = AXIS2_PLACEMENT_3D ( 'NONE', #3451, #103118, #83650 ) ;
#8445 = CARTESIAN_POINT ( 'NONE',  ( 8.959240580532112475, 9.346868853575953651, -0.7998128361456221525 ) ) ;
#8447 = CARTESIAN_POINT ( 'NONE',  ( -9.352427035328430449, 9.805586384171650849, 1.040834085586084257E-14 ) ) ;
#8446 = CARTESIAN_POINT ( 'NONE',  ( 4.329849954717849947, 6.144853928627882489, 1.599625672291262513 ) ) ;
#8448 = CARTESIAN_POINT ( 'NONE',  ( 11.33772465723237666, 10.09131699265169146, 3.600000000000073364 ) ) ;
#8449 = CARTESIAN_POINT ( 'NONE',  ( 4.623309962349557267, 1.759429041943610716, 0.9917458525283324722 ) ) ;
#8450 = CARTESIAN_POINT ( 'NONE',  ( 1.364683531249990311, 5.113541667008084879, 0.7879004041258500513 ) ) ;
#8451 = CARTESIAN_POINT ( 'NONE',  ( 8.242994207428692377, 12.56065097540143327, -0.7216878364870328300 ) ) ;
#8452 = CARTESIAN_POINT ( 'NONE',  ( 4.640002929648442631, 0.9288797265196678810, -1.951996720969489951 ) ) ;
#8453 = CARTESIAN_POINT ( 'NONE',  ( 6.713222337422018349, 7.861122810861019161, -1.199719254218452047 ) ) ;
#8454 = CARTESIAN_POINT ( 'NONE',  ( 0.6823417656249864960, -0.5114583329919111243, -1.181850606188749264 ) ) ;
#8456 = FILL_AREA_STYLE_COLOUR ( '', #110720 ) ;
#8455 = CARTESIAN_POINT ( 'NONE',  ( 6.554440917563797875, 6.611545590104705994, -0.7998128361456481317 ) ) ;
#8457 = CARTESIAN_POINT ( 'NONE',  ( 9.042925270190638187, 9.652427024751663254, 0.7216878364870458196 ) ) ;
#8459 = CARTESIAN_POINT ( 'NONE',  ( -0.4382560683119280931, -7.666862915010161039, 10.99126615174920651 ) ) ;
#8458 = CARTESIAN_POINT ( 'NONE',  ( 1.504584854702104124, 2.168655969765376224, 0.1073316571278438991 ) ) ;
#8460 = AXIS2_PLACEMENT_3D ( 'NONE', #77835, #191573, #142885 ) ;
#8462 = CARTESIAN_POINT ( 'NONE',  ( 0.5382993156314471728, -1.579489783069366604, 0.9460463261394758128 ) ) ;
#8461 = CARTESIAN_POINT ( 'NONE',  ( -5.260200412422200600, 8.120355666925794580, -1.082531754730544860 ) ) ;
#8463 = CARTESIAN_POINT ( 'NONE',  ( 1.364683531249986537, 1.655208333674748955, -0.7879004041258239610 ) ) ;
#8464 = CARTESIAN_POINT ( 'NONE',  ( 3.017305944477025825, -2.111434807548946857, 0.5868732223921411251 ) ) ;
#8465 = FACE_OUTER_BOUND ( 'NONE', #74080, .T. ) ;
#8466 = CARTESIAN_POINT ( 'NONE',  ( 4.083118212167598848, -0.2185186360062584821, -2.251932414709489905 ) ) ;
#8467 = CARTESIAN_POINT ( 'NONE',  ( -8.179646747746328828, 8.437342715325849341, -0.7998128361456291469 ) ) ;
#8468 = CARTESIAN_POINT ( 'NONE',  ( -1.201851678989727383E-14, 5.009375000341421469, -1.575800808251660134 ) ) ;
#8469 = CARTESIAN_POINT ( 'NONE',  ( 6.474762296362193581, 6.758873339713582062, -0.2294044474360455721 ) ) ;
#8470 = CARTESIAN_POINT ( 'NONE',  ( 1.499999999999993117, 12.35416666666666785, 0.8660254037844409281 ) ) ;
#8471 = CARTESIAN_POINT ( 'NONE',  ( 5.072158865288233898, 7.971250205261355859, 1.082531754730549078 ) ) ;
#8472 = CARTESIAN_POINT ( 'NONE',  ( 4.182668740906975380, -0.1716826142807558186, -1.761352938113736277 ) ) ;
#8473 = CARTESIAN_POINT ( 'NONE',  ( 7.099665995050449041, 11.43469409420089455, 0.7998128361456462443 ) ) ;
#8475 = AXIS2_PLACEMENT_3D ( 'NONE', #93523, #110881, #193126 ) ;
#8474 = CARTESIAN_POINT ( 'NONE',  ( 1.202331507228219243, -2.106147100265920002, -0.0002331622408376087278 ) ) ;
#8477 = CARTESIAN_POINT ( 'NONE',  ( -1.500000000000013101, 1.170833333333352710, 0.8660254037844403729 ) ) ;
#8476 = CARTESIAN_POINT ( 'NONE',  ( -1.364683531250000748, 10.60937500034139802, 0.000000000000000000 ) ) ;
#8478 = CARTESIAN_POINT ( 'NONE',  ( 1.381238074367253876, -0.05158952566820934615, 1.969057209924016227 ) ) ;
#8479 = CARTESIAN_POINT ( 'NONE',  ( -3.311934663488232733, 7.085950550703385531, -0.7998128361456481317 ) ) ;
#8480 = CARTESIAN_POINT ( 'NONE',  ( -0.4241069589250067162, 7.990617654048622676, -1.998204128839461191 ) ) ;
#8482 = EDGE_LOOP ( 'NONE', ( #56450, #139771, #96590, #210350 ) ) ;
#8481 = CARTESIAN_POINT ( 'NONE',  ( 5.168131652730963310, 1.809155975298855523, -0.09671077906142805380 ) ) ;
#8483 = CARTESIAN_POINT ( 'NONE',  ( 7.348156068926750883, 8.635565504245116486, -1.082531754730537976 ) ) ;
#8484 = EDGE_CURVE ( 'NONE', #199128, #100096, #140417, .T. ) ;
#8485 = CARTESIAN_POINT ( 'NONE',  ( 10.07100917685271035, 10.64393221595000938, 0.7998128361456462443 ) ) ;
#8486 = CARTESIAN_POINT ( 'NONE',  ( 5.084763247618332649, -0.2297073032716222263, -1.856415652357709778 ) ) ;
#8487 = VERTEX_POINT ( 'NONE', #210057 ) ;
#8488 = CARTESIAN_POINT ( 'NONE',  ( 4.803616497939601437, -1.596918191575154911, -1.317456641179854504 ) ) ;
#8489 = CARTESIAN_POINT ( 'NONE',  ( -3.956095110007852622E-14, 1.437500000000030864, -1.414508159514597407 ) ) ;
#8490 = CARTESIAN_POINT ( 'NONE',  ( -6.577113915960849155, 6.845923454808663600, -0.7216878364870338292 ) ) ;
#8492 = PRESENTATION_LAYER_ASSIGNMENT (  '', '', ( #39728 ) ) ;
#8491 = CARTESIAN_POINT ( 'NONE',  ( 0.4437927792854980402, -0.8979896776215845478, -3.297249098415093282 ) ) ;
#8493 = CARTESIAN_POINT ( 'NONE',  ( 8.646349277213076334, 11.11049346154719508, 1.599625672291281386 ) ) ;
#8494 = CARTESIAN_POINT ( 'NONE',  ( -9.992522908471816123, 11.61669713376064372, 1.199719254218462483 ) ) ;
#8495 = CARTESIAN_POINT ( 'NONE',  ( 5.806634928402749196, 9.996434193103704402, -0.7998128361456481317 ) ) ;
#8496 = CARTESIAN_POINT ( 'NONE',  ( -4.570876033279031248, 6.929166027572136954, -1.217404184480129326 ) ) ;
#8497 = CARTESIAN_POINT ( 'NONE',  ( -1.402160292154681736E-14, 0.5718750003414239114, 1.575800808251672791 ) ) ;
#8500 = ADVANCED_FACE ( 'NONE', ( #44395 ), #96127, .F. ) ;
#8499 = CIRCLE ( 'NONE', #181367, 0.07999999999999998779 ) ;
#8498 = CARTESIAN_POINT ( 'NONE',  ( -1.402160292154681736E-14, 0.4625000000000214495, 1.732050807568877637 ) ) ;
#8501 = CARTESIAN_POINT ( 'NONE',  ( 3.877359892829432386, -0.1466975079335990917, 1.956454564409334296 ) ) ;
#8502 = CARTESIAN_POINT ( 'NONE',  ( 1.932970024460831882, 1.034005469613193062, 1.730602090182407959 ) ) ;
#8503 = FACE_OUTER_BOUND ( 'NONE', #85978, .T. ) ;
#8504 = LINE ( 'NONE', #60453, #143679 ) ;
#8505 = CARTESIAN_POINT ( 'NONE',  ( -11.81907076198591966, 9.842687754035246428, 1.592066415281218505 ) ) ;
#8506 = CARTESIAN_POINT ( 'NONE',  ( 1.581098268704693055, 1.730367963306264301, -0.7109649657882493035 ) ) ;
#8507 = CARTESIAN_POINT ( 'NONE',  ( -1.201851678989727383E-14, 4.696875000341419693, -1.575800808251660134 ) ) ;
#8508 = CARTESIAN_POINT ( 'NONE',  ( 3.111590725901419940, 1.589763268213672420, 1.235112918372171187 ) ) ;
#8510 = CARTESIAN_POINT ( 'NONE',  ( 3.743865479105834559, 2.100983596406953424, -0.2614307623071217557 ) ) ;
#8509 = CARTESIAN_POINT ( 'NONE',  ( -5.856759171423528088, 8.816340885760650892, 1.082531754730548412 ) ) ;
#8511 = CARTESIAN_POINT ( 'NONE',  ( 0.000000000000000000, 3.599999999999999201, 0.000000000000000000 ) ) ;
#8512 = CARTESIAN_POINT ( 'NONE',  ( 4.896967953096117654, 0.3505727482827174502, 2.040303948762006492 ) ) ;
#8513 = CARTESIAN_POINT ( 'NONE',  ( 5.773793314573267388, 7.829454515125894964, 1.599625672291268286 ) ) ;
#8515 = CARTESIAN_POINT ( 'NONE',  ( 6.720655732516648051, 1.999557737031621540, 2.575425662770465252 ) ) ;
#8514 = CARTESIAN_POINT ( 'NONE',  ( 0.08173368997131927327, -0.9817114319007680390, 1.845913477919949086 ) ) ;
#8517 = ORIENTED_EDGE ( 'NONE', *, *, #186328, .T. ) ;
#8516 = CARTESIAN_POINT ( 'NONE',  ( 5.614214418409627427, -0.8227427255552112184, -1.629729119005427496 ) ) ;
#8518 = CARTESIAN_POINT ( 'NONE',  ( 9.237182729612253951, 9.671134694169463586, 0.7998128361456462443 ) ) ;
#8519 = CARTESIAN_POINT ( 'NONE',  ( -6.080807945883922372, 5.988697446486341391, 0.1578021610283755760 ) ) ;
#8520 = PRESENTATION_STYLE_ASSIGNMENT (( #171025 ) ) ;
#8521 = CARTESIAN_POINT ( 'NONE',  ( -11.38450596090590849, 3.710255710271473273, 5.708599601896569453 ) ) ;
#8522 = CARTESIAN_POINT ( 'NONE',  ( 0.6823417656249969321, 12.58854166700806942, -1.181850606188757036 ) ) ;
#8523 = CARTESIAN_POINT ( 'NONE',  ( 6.094389051209717856, -1.018956457145767436, 1.618003106988876283 ) ) ;
#8524 = CARTESIAN_POINT ( 'NONE',  ( -7.133561379084627063, 11.47423870890741782, 0.7998128361456481317 ) ) ;
#8525 = CARTESIAN_POINT ( 'NONE',  ( 5.147291874682557555, 9.156924287104992288, 0.7998128361456462443 ) ) ;
#8526 = CARTESIAN_POINT ( 'NONE',  ( 0.007473969438204840048, 8.279395425053873936, 1.999986034896453324 ) ) ;
#8527 = CARTESIAN_POINT ( 'NONE',  ( 3.511198595814932766, 5.119484333249288532, 1.443375672974066548 ) ) ;
#8528 = EDGE_CURVE ( 'NONE', #45649, #29327, #145119, .T. ) ;
#8529 = FACE_OUTER_BOUND ( 'NONE', #166307, .T. ) ;
#8530 = CARTESIAN_POINT ( 'NONE',  ( 3.985207087413062066, 6.736826471035503694, -1.199719254218452047 ) ) ;
#8531 = VERTEX_POINT ( 'NONE', #179724 ) ;
#8532 = CARTESIAN_POINT ( 'NONE',  ( -6.882699257592852504, 8.058845884393651460, -1.199719254218452047 ) ) ;
#8533 = CARTESIAN_POINT ( 'NONE',  ( 5.431267612114304200, -1.591330327768199382, -1.238307421737715019 ) ) ;
#8534 = DIRECTION ( 'NONE',  ( 0.000000000000000000, -1.000000000000000000, 0.000000000000000000 ) ) ;
#8535 = CARTESIAN_POINT ( 'NONE',  ( -0.1399997263889559695, 7.629137130509076492, -2.600276787041354343 ) ) ;
#8536 = CARTESIAN_POINT ( 'NONE',  ( -4.880572111239580124, 7.677455982212699759, 1.082531754730560403 ) ) ;
#8537 = CARTESIAN_POINT ( 'NONE',  ( 10.38518247838791986, 11.21839376764850726, 0.7216878364870438212 ) ) ;
#8538 = CARTESIAN_POINT ( 'NONE',  ( 2.254690153889327586, -0.5205305878250593432, -1.899364841092534339 ) ) ;
#8539 = ADVANCED_FACE ( 'NONE', ( #97418 ), #108799, .F. ) ;
#8540 = CARTESIAN_POINT ( 'NONE',  ( 3.550407796516129366, -1.352142120786763213, 1.496064415113136592 ) ) ;
#8541 = CARTESIAN_POINT ( 'NONE',  ( -7.694415870955439551, 8.935572256658169010, 1.199719254218462483 ) ) ;
#8542 = CARTESIAN_POINT ( 'NONE',  ( 6.827182134110157286, 6.032625672350935275, 2.883942191975923830 ) ) ;
#8543 = CARTESIAN_POINT ( 'NONE',  ( 3.380998015235132215, 1.981133383611884735, -0.9370748116589098231 ) ) ;
#8544 = DIRECTION ( 'NONE',  ( 0.000000000000000000, 1.000000000000000000, 0.000000000000000000 ) ) ;
#8545 = CARTESIAN_POINT ( 'NONE',  ( 2.801685564775885595, -0.6058112460363762608, 1.828711369353401617 ) ) ;
#8546 = CARTESIAN_POINT ( 'NONE',  ( -6.984421689334302741, 11.30024240419870374, 0.000000000000000000 ) ) ;
#8547 = ADVANCED_FACE ( 'NONE', ( #163769 ), #81440, .F. ) ;
#8548 = CARTESIAN_POINT ( 'NONE',  ( -0.1296875068448159751, 0.001480089298542403009, -1.826395826379861864 ) ) ;
#8549 = CARTESIAN_POINT ( 'NONE',  ( 0.1333542156527295908, 7.629137130509112907, -2.645925523406994717 ) ) ;
#8550 = DIRECTION ( 'NONE',  ( 0.000000000000000000, 0.000000000000000000, -1.000000000000000000 ) ) ;
#8551 = CARTESIAN_POINT ( 'NONE',  ( 1.364683531249996529, 12.71354166700806232, 0.7879004041258403923 ) ) ;
#8552 = CARTESIAN_POINT ( 'NONE',  ( 4.741601036477289810, 6.554953847355395880, 1.599625672291267398 ) ) ;
#8553 = FACE_OUTER_BOUND ( 'NONE', #10677, .T. ) ;
#8554 = CARTESIAN_POINT ( 'NONE',  ( 4.909461021924240498, 7.781436054670031410, 1.082531754730549078 ) ) ;
#8555 = ORIENTED_EDGE ( 'NONE', *, *, #39340, .F. ) ;
#8557 = CARTESIAN_POINT ( 'NONE',  ( 3.404942666290892817, -0.3948933297331903014, -1.973820178108119272 ) ) ;
#8556 = CARTESIAN_POINT ( 'NONE',  ( 5.688959394570705541, 1.398425918548395153, 1.197878823674280779 ) ) ;
#8558 = CARTESIAN_POINT ( 'NONE',  ( 5.079617024973425821, 1.589842341716392493, -1.660015637060639371 ) ) ;
#8559 = CARTESIAN_POINT ( 'NONE',  ( 3.186215892106421421, 1.037744835847534741, -1.544512256342661427 ) ) ;
#8560 = CARTESIAN_POINT ( 'NONE',  ( -1.642778471874998480, -0.7510416661887092671, 2.845375778867863303 ) ) ;
#8561 = CARTESIAN_POINT ( 'NONE',  ( -0.1290005225502398323, 0.2247172878383028038, -2.207197350255707402 ) ) ;
#8562 = CARTESIAN_POINT ( 'NONE',  ( -11.84668730067608600, 10.19999999999999929, -1.400000000000001910 ) ) ;
#8563 = CARTESIAN_POINT ( 'NONE',  ( -6.008234629150358330, 10.16135750065076060, 0.000000000000000000 ) ) ;
#8564 = CARTESIAN_POINT ( 'NONE',  ( -3.797692425603673705, 6.484372692295976570, 1.082531754730549967 ) ) ;
#8565 = CARTESIAN_POINT ( 'NONE',  ( 6.374567656919228220, -0.1030857042376011334, -2.088345373630628554 ) ) ;
#8566 = CARTESIAN_POINT ( 'NONE',  ( 6.317736394288140822, 7.433409217166723870, 1.082531754730558626 ) ) ;
#8567 = ORIENTED_EDGE ( 'NONE', *, *, #191657, .T. ) ;
#8568 = CARTESIAN_POINT ( 'NONE',  ( -1.436717746206722213, 7.422220963915807879, 4.237135035833794916 ) ) ;
#8570 = CARTESIAN_POINT ( 'NONE',  ( 5.352771719296971042, 5.139321848801576387, 0.7998128361456341429 ) ) ;
#8569 = DIRECTION ( 'NONE',  ( 1.000000000000000000, 0.000000000000000000, 0.000000000000000000 ) ) ;
#8571 = CARTESIAN_POINT ( 'NONE',  ( 5.813083859329478464, 1.524454967706680319, 0.8070229810451818864 ) ) ;
#8572 = CARTESIAN_POINT ( 'NONE',  ( -6.247609857798938293, 6.183299677053865295, -0.7998128361456291469 ) ) ;
#8573 = CARTESIAN_POINT ( 'NONE',  ( 1.828352651294574249, 0.6632370903016276964, -1.602517542597500455 ) ) ;
#8574 = CARTESIAN_POINT ( 'NONE',  ( -5.249999999999987566, 1.374772708486751593, 1.000000000000000888 ) ) ;
#8575 = CARTESIAN_POINT ( 'NONE',  ( 11.86145016429272836, 10.90000000000000036, -1.180000000000002158 ) ) ;
#8576 = FILL_AREA_STYLE_COLOUR ( '', #160658 ) ;
#8577 = CARTESIAN_POINT ( 'NONE',  ( 5.893482054836863604, -1.966010524246808666, 0.9213097603111667366 ) ) ;
#8578 = CARTESIAN_POINT ( 'NONE',  ( 4.828627627824715773, 1.747987318788373656, 0.5269492854979712648 ) ) ;
#8579 = CARTESIAN_POINT ( 'NONE',  ( 1.973419848571813295, -0.2453196125269933581, 1.946320556625024345 ) ) ;
#8580 = CARTESIAN_POINT ( 'NONE',  ( 9.601932019700244680, 4.115787151892719820, 7.121345993713853240 ) ) ;
#8581 = CARTESIAN_POINT ( 'NONE',  ( -9.642873567817536795, 12.27310513391906532, 1.599625672291281386 ) ) ;
#8582 = CARTESIAN_POINT ( 'NONE',  ( 7.564559641420864899, 10.91273778404466199, -1.199719254218446718 ) ) ;
#8583 = CARTESIAN_POINT ( 'NONE',  ( 3.334745777049468618, 1.343786929377327466, -1.640352557257473309 ) ) ;
#8584 = CARTESIAN_POINT ( 'NONE',  ( -2.168941388506379742, 5.474256019991960542, -0.7216878364870267237 ) ) ;
#8585 = CARTESIAN_POINT ( 'NONE',  ( 0.4373225248172820656, -7.723431457505077979, -10.96785329849813273 ) ) ;
#8586 = CARTESIAN_POINT ( 'NONE',  ( -4.822091459260241741, 6.758233420496813082, -1.248138317850192580 ) ) ;
#8587 = CARTESIAN_POINT ( 'NONE',  ( 1.428671948192638208, -1.316369429293560156, 1.597808059233512656 ) ) ;
#8588 = CARTESIAN_POINT ( 'NONE',  ( 2.280903940472752467, 5.594607745005274246, -0.6109567437776646237 ) ) ;
#8590 = ORIENTED_EDGE ( 'NONE', *, *, #71115, .F. ) ;
#8589 = CARTESIAN_POINT ( 'NONE',  ( 3.914843843660667400, -0.6973054565188941956, -2.109062029434173535 ) ) ;
#8591 = CARTESIAN_POINT ( 'NONE',  ( 1.319383182065179128, 1.127869332580781148, -2.002907031218110312 ) ) ;
#8593 = CARTESIAN_POINT ( 'NONE',  ( 6.209847231236663490, 0.6040719066883664112, -1.972102366942799945 ) ) ;
#8592 = CARTESIAN_POINT ( 'NONE',  ( 8.215877900201359552, 11.56864606933486606, -1.082531754730543083 ) ) ;
#8595 = CARTESIAN_POINT ( 'NONE',  ( 2.960183410750786059, -4.109567543049581495, -1.425552035297093623 ) ) ;
#8594 = CARTESIAN_POINT ( 'NONE',  ( 3.040771591214902259, 6.769593633051179005, -0.7998128361456362523 ) ) ;
#8596 = CARTESIAN_POINT ( 'NONE',  ( -6.042630808230841359E-15, -1.662500000000000533, 3.474999999999999645 ) ) ;
#8597 = CARTESIAN_POINT ( 'NONE',  ( 6.585540641348407220, -0.7802508550805786758, 1.666130356082275998 ) ) ;
#8598 = SURFACE_STYLE_FILL_AREA ( #41135 ) ;
#8599 = CARTESIAN_POINT ( 'NONE',  ( -0.1104750535120268828, 5.720715034752038797, -2.697548938405624597 ) ) ;
#8600 = CARTESIAN_POINT ( 'NONE',  ( 2.625662686473359653, -0.9909224867145174365, -1.411489731159983219 ) ) ;
#8601 = CARTESIAN_POINT ( 'NONE',  ( 2.167204200501818612, 1.841733140229084853, -0.8216742516050158374 ) ) ;
#8602 = CARTESIAN_POINT ( 'NONE',  ( 3.287964078406432566, 1.811126957681759908, -1.415446460160358688 ) ) ;
#8603 = TOROIDAL_SURFACE ( 'NONE', #129777, 2.349999999999999645, 0.1000000000000000056 ) ;
#8604 = CARTESIAN_POINT ( 'NONE',  ( 3.620660229735796154, 1.438486863682734818, -1.746180642158390084 ) ) ;
#8605 = CARTESIAN_POINT ( 'NONE',  ( 5.426436078920066741, 1.255580583125959437, -1.690716914145540040 ) ) ;
#8606 = CARTESIAN_POINT ( 'NONE',  ( -7.268579750702160780, 8.613002809641560731, -1.082531754730549967 ) ) ;
#8607 = CARTESIAN_POINT ( 'NONE',  ( 3.866244329565728943, -1.190307266767919536, 1.309773914726497734 ) ) ;
#8609 = CARTESIAN_POINT ( 'NONE',  ( 6.409759596795807646, -1.076414324555999391, -2.023967322820482639 ) ) ;
#8608 = CARTESIAN_POINT ( 'NONE',  ( 3.241808126998965811, 6.796210224891872542, 0.7216878364870257245 ) ) ;
#8610 = CARTESIAN_POINT ( 'NONE',  ( 6.035073252477260120, -1.336788798515762489, -1.266260169258619284 ) ) ;
#8612 = EDGE_CURVE ( 'NONE', #129277, #92086, #212458, .T. ) ;
#8611 = CARTESIAN_POINT ( 'NONE',  ( -2.923754682041362241, 6.562797562356882608, 0.7998128361456341429 ) ) ;
#8613 = CARTESIAN_POINT ( 'NONE',  ( -1.500000000000011324, 3.670833333333356485, 0.8660254037844403729 ) ) ;
#8614 = CARTESIAN_POINT ( 'NONE',  ( 6.123007039855313138, -2.064672272812938747, 0.7349105657750015785 ) ) ;
#8615 = CARTESIAN_POINT ( 'NONE',  ( -3.460355519985875983, 5.060167411448709629, 1.599625672291267398 ) ) ;
#8616 = CARTESIAN_POINT ( 'NONE',  ( -5.577074488906905714, 15.46905280921072467, 10.63472345728874835 ) ) ;
#8617 = CARTESIAN_POINT ( 'NONE',  ( 6.338344951546218908, -1.110931056888088353, 1.746890944850580052 ) ) ;
#8618 = CARTESIAN_POINT ( 'NONE',  ( 0.3918150239524306189, -2.006371095615328226, 0.2024682584410575914 ) ) ;
#8619 = CARTESIAN_POINT ( 'NONE',  ( 0.6823417656249917140, 5.092708333674749177, 1.181850606188765695 ) ) ;
#8620 = CARTESIAN_POINT ( 'NONE',  ( 4.336495953379083446, 1.889596944713485049, 0.3744603196194126182 ) ) ;
#8621 = CARTESIAN_POINT ( 'NONE',  ( -8.012344526598182026E-15, 10.04687500034140335, -1.575800808251669460 ) ) ;
#8623 = CARTESIAN_POINT ( 'NONE',  ( -2.304522924643024773, 5.632434478818063361, 0.7216878364870317197 ) ) ;
#8622 = AXIS2_PLACEMENT_3D ( 'NONE', #210944, #14869, #130846 ) ;
#8624 = CARTESIAN_POINT ( 'NONE',  ( 0.5455723692351510667, 0.1713331888719657747, 2.214891930232844253 ) ) ;
#8626 = ORIENTED_EDGE ( 'NONE', *, *, #1482, .T. ) ;
#8625 = CARTESIAN_POINT ( 'NONE',  ( 4.577813143269636065, 5.369812084349879555, -1.199719254218450271 ) ) ;
#8628 = CARTESIAN_POINT ( 'NONE',  ( -10.95308175811721085, 13.79999999999999893, -1.800000000000001155 ) ) ;
#8627 = CARTESIAN_POINT ( 'NONE',  ( 6.966220764712143243, 6.002124920821316323, -2.420000000000000373 ) ) ;
#8629 = CARTESIAN_POINT ( 'NONE',  ( 2.218730694130720771, 5.740269576461138890, 0.7998128361456462443 ) ) ;
#8630 = CARTESIAN_POINT ( 'NONE',  ( 7.962224162659105708, -5.254973434576991842, -7.552496594302672506 ) ) ;
#8631 = PLANE ( 'NONE',  #28342 ) ;
#8632 = CARTESIAN_POINT ( 'NONE',  ( 10.80547401163854460, 9.581360759087717227, 5.116132519491706887 ) ) ;
#8633 = CARTESIAN_POINT ( 'NONE',  ( 9.205623113554612047, 12.72334881824701469, 1.082531754730546636 ) ) ;
#8634 = CARTESIAN_POINT ( 'NONE',  ( 1.785527960060459440, -1.848404783191982315, 0.6579185095809261252 ) ) ;
#8635 = CARTESIAN_POINT ( 'NONE',  ( -1.364683531250014514, 1.801041667008085767, -0.7879004041258289570 ) ) ;
#8636 = CARTESIAN_POINT ( 'NONE',  ( 1.419999999999990603, 6.280000000000042881, 2.873333333333337070 ) ) ;
#8637 = EDGE_CURVE ( 'NONE', #190586, #5554, #143562, .T. ) ;
#8638 = CARTESIAN_POINT ( 'NONE',  ( 5.266048140081638351, -1.952571265509401854, 0.1905133553196102503 ) ) ;
#8639 = CARTESIAN_POINT ( 'NONE',  ( -8.402302512167102222, 10.82577223566020841, -1.599625672291263179 ) ) ;
#8640 = CARTESIAN_POINT ( 'NONE',  ( -5.463572716182839351, 7.397254140345190798, 1.443375672974064550 ) ) ;
#8641 = AXIS2_PLACEMENT_3D ( 'NONE', #31169, #131895, #29033 ) ;
#8642 = CARTESIAN_POINT ( 'NONE',  ( 6.473507614529132148, 2.070149491355821159, -0.6224772505839873959 ) ) ;
#8644 = ORIENTED_EDGE ( 'NONE', *, *, #64428, .T. ) ;
#8643 = CARTESIAN_POINT ( 'NONE',  ( -0.2104748580754183807, 2.005809028216706924, -2.517884123765606663 ) ) ;
#8645 = CARTESIAN_POINT ( 'NONE',  ( -1.402160292154681736E-14, -1.006249999317181620, 1.732050807568877637 ) ) ;
#8646 = CARTESIAN_POINT ( 'NONE',  ( 0.8252170375972631700, -1.778153878779257901, 0.5809004490327505099 ) ) ;
#8647 = CARTESIAN_POINT ( 'NONE',  ( 6.274686883491842337, -1.720241393171379363, 0.2158021260532434760 ) ) ;
#8649 = CARTESIAN_POINT ( 'NONE',  ( 3.034921719543516971, -1.931671641359738567, 1.035203715903771915 ) ) ;
#8648 = CARTESIAN_POINT ( 'NONE',  ( -0.6801582343750403048, 1.598958333674738164, -1.178068619123869398 ) ) ;
#8650 = CARTESIAN_POINT ( 'NONE',  ( 4.946439154741203659, 2.300974901101384695, 0.1755221459238848203 ) ) ;
#8651 = CARTESIAN_POINT ( 'NONE',  ( 0.1454761644432709389, -1.592655978506152703, -1.307672486379028332 ) ) ;
#8652 = CARTESIAN_POINT ( 'NONE',  ( 2.132666086734685162, -1.734545437858775463, 0.8733739462151270949 ) ) ;
#8653 = CARTESIAN_POINT ( 'NONE',  ( -4.514501963226242864, 7.250374142863800664, 1.082531754730560403 ) ) ;
#8654 = AXIS2_PLACEMENT_3D ( 'NONE', #50930, #51999, #37875 ) ;
#8655 = CARTESIAN_POINT ( 'NONE',  ( -0.4644214298786696893, 7.369507887681775671, -4.459343850242297513 ) ) ;
#8656 = CARTESIAN_POINT ( 'NONE',  ( 4.781546299372162245, 0.2051969522943071500, -2.110614603223801122 ) ) ;
#8657 = FILL_AREA_STYLE_COLOUR ( '', #167590 ) ;
#8658 = CARTESIAN_POINT ( 'NONE',  ( 3.639296212489909532, 0.7283784247123014088, 1.880435045658496618 ) ) ;
#8659 = CARTESIAN_POINT ( 'NONE',  ( -3.917943204224914933, 6.554388924028945240, -1.082531754730548412 ) ) ;
#8660 = CARTESIAN_POINT ( 'NONE',  ( -7.469616286486262524, 7.679250187180907794, 0.7998128361456341429 ) ) ;
#8661 = CARTESIAN_POINT ( 'NONE',  ( 8.940712233207955606, 12.51824914112961729, 1.199719254218450271 ) ) ;
#8662 = CARTESIAN_POINT ( 'NONE',  ( 1.242498012622397674, 0.3540479964400863877, 1.790853789395550955 ) ) ;
#8663 = CARTESIAN_POINT ( 'NONE',  ( -6.622231685632140596, 6.690634819517756959, 0.000000000000000000 ) ) ;
#8664 = CARTESIAN_POINT ( 'NONE',  ( -6.479871072688648148, 6.524547437750345402, 0.000000000000000000 ) ) ;
#8665 = CARTESIAN_POINT ( 'NONE',  ( 10.91970695577495754, -6.134628647623513231, 0.08000000000000194456 ) ) ;
#8666 = VERTEX_POINT ( 'NONE', #162705 ) ;
#8667 = CARTESIAN_POINT ( 'NONE',  ( 5.911025222378588850, 1.816451602635826612, 0.9735456368637726010 ) ) ;
#8668 = CARTESIAN_POINT ( 'NONE',  ( -6.794044373779495771, 8.059378203231773341, 1.082531754730549078 ) ) ;
#8669 = CARTESIAN_POINT ( 'NONE',  ( -3.255929445576174697, 6.950334786480840243, -0.7998128361456281477 ) ) ;
#8670 = CARTESIAN_POINT ( 'NONE',  ( -6.114675100508033978, 6.010327456751344499, 0.3238074992715953559 ) ) ;
#8671 = CARTESIAN_POINT ( 'NONE',  ( 4.846356044401274765, 1.036295046036241674, -1.733382803446526621 ) ) ;
#8673 = ORIENTED_EDGE ( 'NONE', *, *, #183782, .T. ) ;
#8672 = CARTESIAN_POINT ( 'NONE',  ( 5.971364366153397718, -1.903789954562478792, -1.144205655003695643 ) ) ;
#8675 = CARTESIAN_POINT ( 'NONE',  ( 7.592202833972727660, 11.80139437303613015, -0.7216878364870267237 ) ) ;
#8674 = CARTESIAN_POINT ( 'NONE',  ( -6.291865805193673111, 9.498204651771386509, -1.199719254218452047 ) ) ;
#8676 = CARTESIAN_POINT ( 'NONE',  ( 5.133733721068893807, 9.141106441222381918, 1.040834085586084257E-14 ) ) ;
#8677 = CARTESIAN_POINT ( 'NONE',  ( 3.889569955515647326, 1.491445920024776051, 1.422513881352378107 ) ) ;
#8678 = CARTESIAN_POINT ( 'NONE',  ( 4.184220324914634581, 1.621181886760931778, 1.198861198883696799 ) ) ;
#8679 = VERTEX_POINT ( 'NONE', #29497 ) ;
#8680 = FACE_OUTER_BOUND ( 'NONE', #108782, .T. ) ;
#8681 = CARTESIAN_POINT ( 'NONE',  ( 5.190073875932979419, 4.949507698210251938, 0.7998128361456341429 ) ) ;
#8683 = ORIENTED_EDGE ( 'NONE', *, *, #9580, .T. ) ;
#8682 = CARTESIAN_POINT ( 'NONE',  ( -7.944151662964566540, 8.232874793072271657, 0.000000000000000000 ) ) ;
#8684 = CARTESIAN_POINT ( 'NONE',  ( 5.504185490526544378, 7.460110003252303557, -1.249659907641489820 ) ) ;
#8685 = CARTESIAN_POINT ( 'NONE',  ( 3.462267382487670631, 1.587593928739635896, 1.242537129137813556 ) ) ;
#8686 = CARTESIAN_POINT ( 'NONE',  ( 2.888418961059231904, 1.578855305991919478, -0.9468669452540460219 ) ) ;
#8687 = CARTESIAN_POINT ( 'NONE',  ( 0.6457025891282016650, -1.976290545051001768, 1.191322501153786906 ) ) ;
#8688 = CARTESIAN_POINT ( 'NONE',  ( 3.088225128862704949, 6.824956093640315302, 0.7998128361456281477 ) ) ;
#8689 = CARTESIAN_POINT ( 'NONE',  ( 3.462350783624254191, 0.9684823049558517472, 1.932541222812742987 ) ) ;
#8690 = CARTESIAN_POINT ( 'NONE',  ( 8.127223016387999266, 11.56917838817298616, 1.199719254218460707 ) ) ;
#8691 = CARTESIAN_POINT ( 'NONE',  ( -6.413170354464012846, 7.440785820751486312, 1.199719254218450271 ) ) ;
#8692 = ADVANCED_FACE ( 'NONE', ( #31634 ), #41057, .T. ) ;
#8693 = CARTESIAN_POINT ( 'NONE',  ( 3.409784427348498070, 0.5549599139818006677, 2.230294995599948926 ) ) ;
#8694 = ORIENTED_EDGE ( 'NONE', *, *, #200691, .F. ) ;
#8695 = DIRECTION ( 'NONE',  ( 0.000000000000000000, 8.546850786086437571E-32, 1.000000000000000000 ) ) ;
#8696 = CARTESIAN_POINT ( 'NONE',  ( 2.869827659178546764, 0.9992216309704025079, 1.581230272166146644 ) ) ;
#8697 = CARTESIAN_POINT ( 'NONE',  ( 5.770382930017874834, -1.251004719971451795, 1.523686133408495236 ) ) ;
#8699 = CARTESIAN_POINT ( 'NONE',  ( 8.717529583462646059, 11.19353715217169309, 1.443375672974076540 ) ) ;
#8698 = CARTESIAN_POINT ( 'NONE',  ( 1.364683531249990311, 4.384375000341417028, 1.214306433183764966E-14 ) ) ;
#8701 = CARTESIAN_POINT ( 'NONE',  ( 0.4170028235400899397, 1.518763190251697370, -1.601383572969114599 ) ) ;
#8700 = CARTESIAN_POINT ( 'NONE',  ( -5.388475986427523345, 8.373973519885682393, 1.199719254218452047 ) ) ;
#8702 = CARTESIAN_POINT ( 'NONE',  ( 10.39230484541318589, 3.447199233515649386, -6.000000000000107470 ) ) ;
#8703 = CARTESIAN_POINT ( 'NONE',  ( 3.994848817520957773, 7.812407387083109001, 1.040834085586084257E-14 ) ) ;
#8704 = CARTESIAN_POINT ( 'NONE',  ( -5.762378981008047241, 6.681529218386182301, 1.199719254218450271 ) ) ;
#8705 = CARTESIAN_POINT ( 'NONE',  ( -8.016215341155614738, -5.223177556212601047, 7.499070966594912235 ) ) ;
#8706 = CARTESIAN_POINT ( 'NONE',  ( 6.262572880032761802, -1.394454384559177695, 1.393866484745357459 ) ) ;
#8707 = CARTESIAN_POINT ( 'NONE',  ( 5.971339433669736962, 0.1760496889521658836, -2.301030538967073991 ) ) ;
#8708 = CARTESIAN_POINT ( 'NONE',  ( 5.828513650932020340, -1.180329482691832244, 1.438830759754748723 ) ) ;
#8709 = CARTESIAN_POINT ( 'NONE',  ( 3.485269120655315689, 0.04592427588026624929, 2.062205569330832766 ) ) ;
#8710 = CARTESIAN_POINT ( 'NONE',  ( 6.155038550924144758, 8.203964280876741455, 1.443375672974076540 ) ) ;
#8711 = CARTESIAN_POINT ( 'NONE',  ( 5.833751235630055376, 10.02806988486892514, 0.7998128361456331437 ) ) ;
#8712 = CARTESIAN_POINT ( 'NONE',  ( 6.927853306458743532, 9.105581495667113501, 1.443375672974076540 ) ) ;
#8713 = CARTESIAN_POINT ( 'NONE',  ( 0.6823417656249899377, 3.988541667008085767, -1.181850606188754593 ) ) ;
#8714 = DIRECTION ( 'NONE',  ( 0.000000000000000000, 0.000000000000000000, 1.000000000000000000 ) ) ;
#8715 = CARTESIAN_POINT ( 'NONE',  ( 4.460269348771534581, 8.147471973634706544, -0.7216878364870207285 ) ) ;
#8716 = CARTESIAN_POINT ( 'NONE',  ( 5.336453890206420247, -1.210535830701382709, 1.802210774359000567 ) ) ;
#8717 = CARTESIAN_POINT ( 'NONE',  ( 0.4214947629261721618, 3.038568440852233987, -0.4183962726263586451 ) ) ;
#8719 = CARTESIAN_POINT ( 'NONE',  ( 4.018977146631536712, -1.760761141180338774, 0.5383908109771737838 ) ) ;
#8718 = CARTESIAN_POINT ( 'NONE',  ( -4.148431816101615155, 3.942184661647709198, 0.7216878364870317197 ) ) ;
#8720 = B_SPLINE_CURVE_WITH_KNOTS ( 'NONE', 3,
 ( #172114, #101773, #68180, #20504, #106092, #71377, #167841 ),
 .UNSPECIFIED., .F., .F.,
 ( 4, 3, 4 ),
 ( 0.0001932293135873436221, 0.0009000000018422016053, 0.002089330742406769661 ),
 .UNSPECIFIED. ) ;
#8721 = AXIS2_PLACEMENT_3D ( 'NONE', #55363, #53229, #151811 ) ;
#8723 = CARTESIAN_POINT ( 'NONE',  ( 6.720655732516653380, 6.038084619979597001, 2.521169617733058477 ) ) ;
#8722 = CARTESIAN_POINT ( 'NONE',  ( -1.499999999999960476, 6.999999999999999112, 10.89724735885168982 ) ) ;
#8724 = CARTESIAN_POINT ( 'NONE',  ( 6.480031355044912900, -2.148842909532014289, -0.4297212958329286736 ) ) ;
#8725 = CARTESIAN_POINT ( 'NONE',  ( 0.1452347671247937455, 3.480000000000001759, 2.000000000000002220 ) ) ;
#8726 = CARTESIAN_POINT ( 'NONE',  ( 0.8435138722653515719, -1.939887490614403687, 1.163926157780611925 ) ) ;
#8727 = ADVANCED_FACE ( 'NONE', ( #169414 ), #209905, .T. ) ;
#8728 = CARTESIAN_POINT ( 'NONE',  ( -4.212224785787594961, 7.548845203666256332, -0.9872405639642158892 ) ) ;
#8729 = DIRECTION ( 'NONE',  ( -0.06263215618328135670, 1.613675268591885659E-12, -0.9980366791916183145 ) ) ;
#8730 = CARTESIAN_POINT ( 'NONE',  ( 6.090086331970060662, 7.118959255344424086, 1.132899493623270359 ) ) ;
#8731 = CARTESIAN_POINT ( 'NONE',  ( -4.123088111887291518, 7.824370207261548416, 0.000000000000000000 ) ) ;
#8732 = CARTESIAN_POINT ( 'NONE',  ( 0.2231138172586397683, 1.663799575440491285, 0.9424754157791456199 ) ) ;
#8733 =( BOUNDED_CURVE ( )  B_SPLINE_CURVE ( 2, ( #87070, #206147, #153140, #74030, #169388, #57775, #72940, #140121, #156355 ),
 .UNSPECIFIED., .F., .T. ) 
 B_SPLINE_CURVE_WITH_KNOTS ( ( 3, 2, 2, 2, 3 ),
 ( 0.3593749999999999445, 0.3645833333333333148, 0.3750000000000000000, 0.3854166666666666852, 0.3906250000000001665 ),
 .UNSPECIFIED. ) 
 CURVE ( )  GEOMETRIC_REPRESENTATION_ITEM ( )  RATIONAL_B_SPLINE_CURVE ( ( 0.9330127018922194093, 0.9330127018922186322, 1.000000000000000000, 0.8660254037844387076, 1.000000000000000000, 0.8660254037844387076, 1.000000000000000000, 0.9330127018922171889, 0.9330127018922194093 ) ) 
 REPRESENTATION_ITEM ( '' )  );
#8734 = CARTESIAN_POINT ( 'NONE',  ( 1.902845806929494232, 1.469307612142495723, 0.9863148084752764166 ) ) ;
#8735 = CARTESIAN_POINT ( 'NONE',  ( 5.637363213272434059, -0.04718591601137950980, 2.012692011999743791 ) ) ;
#8736 = CARTESIAN_POINT ( 'NONE',  ( 5.464099601507359516, 6.333536608968757697, 1.199719254218462483 ) ) ;
#8737 = CARTESIAN_POINT ( 'NONE',  ( 3.715936783694527179, -2.075135040979354528, 0.3580079364009710052 ) ) ;
#8739 = CARTESIAN_POINT ( 'NONE',  ( 3.532743792504475788, -1.564076696776861120, 1.105682177958314583 ) ) ;
#8738 = CARTESIAN_POINT ( 'NONE',  ( -3.050221372950322252, 5.542046787541873520, 1.082531754730560403 ) ) ;
#8740 = CARTESIAN_POINT ( 'NONE',  ( -0.02244404828160087226, 6.946777552644228138, -2.784171975256703124 ) ) ;
#8741 = CARTESIAN_POINT ( 'NONE',  ( 3.754321382136751595, -1.967203782747016128, -0.09899598954335629697 ) ) ;
#8742 = CARTESIAN_POINT ( 'NONE',  ( 0.4047333657465709278, -2.105317319661216047, -0.2534319464195868843 ) ) ;
#8743 = CARTESIAN_POINT ( 'NONE',  ( 2.360033908006432757, 0.7977434165707707470, 1.692156362554583460 ) ) ;
#8745 = ORIENTED_EDGE ( 'NONE', *, *, #133776, .F. ) ;
#8744 = CARTESIAN_POINT ( 'NONE',  ( 5.619686913847246501, -1.681401280226066941, 0.3840984716911073349 ) ) ;
#8747 = CARTESIAN_POINT ( 'NONE',  ( 3.714570900464269076, 7.277490450609545469, 0.7216878364870298324 ) ) ;
#8746 = CARTESIAN_POINT ( 'NONE',  ( 2.666872310945223923, -1.521158656661812714, 1.599105504226288499 ) ) ;
#8748 = CARTESIAN_POINT ( 'NONE',  ( 1.364683531249988535, 2.926041667008082658, 0.7879004041258500513 ) ) ;
#8749 = CARTESIAN_POINT ( 'NONE',  ( 6.549272904993657995, 1.707534169505098953, -0.9658701945045378157 ) ) ;
#8750 = CARTESIAN_POINT ( 'NONE',  ( 7.832860060393120882, 10.16142270859057462, 1.599625672291281386 ) ) ;
#8751 = CARTESIAN_POINT ( 'NONE',  ( -10.15522075183580419, 11.80651128435196462, 1.199719254218462483 ) ) ;
#8752 = CARTESIAN_POINT ( 'NONE',  ( 0.000000000000000000, 19.00000000000000000, 0.000000000000000000 ) ) ;
#8753 = CARTESIAN_POINT ( 'NONE',  ( -1.299038105676657340, 5.999999999999998224, 0.7500000000000006661 ) ) ;
#8754 = DIRECTION ( 'NONE',  ( -0.000000000000000000, -1.000000000000000000, -0.000000000000000000 ) ) ;
#8755 = ORIENTED_EDGE ( 'NONE', *, *, #207217, .T. ) ;
#8756 = CARTESIAN_POINT ( 'NONE',  ( 2.576698201331685922, 1.354182300986291887, -1.566139152919379107 ) ) ;
#8758 = CARTESIAN_POINT ( 'NONE',  ( 1.499999999999989120, 2.775000000000020339, 1.214306433183764966E-14 ) ) ;
#8757 = MECHANICAL_DESIGN_GEOMETRIC_PRESENTATION_REPRESENTATION (  '', ( #195542 ), #98904 ) ;
#8759 = CARTESIAN_POINT ( 'NONE',  ( 5.099838337034727331, 9.101561826515851550, -0.7998128361456281477 ) ) ;
#8760 = CARTESIAN_POINT ( 'NONE',  ( 5.076602173674213070, 4.887400388900169368, 0.000000000000000000 ) ) ;
#8761 = CARTESIAN_POINT ( 'NONE',  ( 6.604144390287855160, -0.9070803646254663732, 1.914764756563241965 ) ) ;
#8762 = DIRECTION ( 'NONE',  ( -3.330669073875472579E-16, 1.665334536937734318E-16, 1.000000000000000000 ) ) ;
#8763 = CARTESIAN_POINT ( 'NONE',  ( 1.364683531249988535, 3.405208333674749621, -0.7879004041258239610 ) ) ;
#8764 = ADVANCED_FACE ( 'NONE', ( #64489 ), #70099, .F. ) ;
#8766 = CARTESIAN_POINT ( 'NONE',  ( 7.944714827928033962, 12.21265836598400689, 0.7216878364870438212 ) ) ;
#8765 = CARTESIAN_POINT ( 'NONE',  ( 6.877413162628407406, -0.1429737755889188000, 1.930079329684093237 ) ) ;
#8767 = CARTESIAN_POINT ( 'NONE',  ( 5.431017465639029318, 0.9912489969874547224, 1.755499476546865445 ) ) ;
#8768 = CARTESIAN_POINT ( 'NONE',  ( 4.909359874374886523, -1.816983420234472790, 0.6072180050544163654 ) ) ;
#8769 = CARTESIAN_POINT ( 'NONE',  ( 2.349409277133751139, 0.5813161652389825518, -2.113004480973964760 ) ) ;
#8770 = CARTESIAN_POINT ( 'NONE',  ( 1.499999999999987121, 1.827083334016151861, -0.8660254037844253849 ) ) ;
#8771 = CARTESIAN_POINT ( 'NONE',  ( 2.584119536544440265, 1.026460374567798484, 1.613398670029235538 ) ) ;
#8772 = CARTESIAN_POINT ( 'NONE',  ( -6.742482464697739708, 6.760651051769146491, 0.7998128361456341429 ) ) ;
#8774 = CARTESIAN_POINT ( 'NONE',  ( 0.4742327405582689170, -2.001515332587662233, -0.2440062454662216829 ) ) ;
#8773 = CARTESIAN_POINT ( 'NONE',  ( -4.148431816101615155, 3.942184661647709198, 0.7216878364870317197 ) ) ;
#8775 = CARTESIAN_POINT ( 'NONE',  ( -1.402160292154681736E-14, 9.734375000341399797, 1.575800808251682339 ) ) ;
#8777 = CARTESIAN_POINT ( 'NONE',  ( -5.769876891067536206, 8.889217585290882795, 1.199719254218454489 ) ) ;
#8776 = CARTESIAN_POINT ( 'NONE',  ( 3.210569733434172512, 1.891194753341999935, 0.8916721373675460249 ) ) ;
#8779 = ORIENTED_EDGE ( 'NONE', *, *, #18478, .T. ) ;
#8778 = CARTESIAN_POINT ( 'NONE',  ( 2.397083457474056267, 1.331176160016230847, 1.096701253500545148 ) ) ;
#8780 = DIRECTION ( 'NONE',  ( -0.000000000000000000, -1.000000000000000000, -0.000000000000000000 ) ) ;
#8781 = CARTESIAN_POINT ( 'NONE',  ( 6.484877546038077867, 6.460111979999551224, 1.040834085586084257E-14 ) ) ;
#8782 = DIRECTION ( 'NONE',  ( 4.462851221005182648E-16, 0.7999999999999986011, 0.6000000000000019762 ) ) ;
#8783 = FACE_OUTER_BOUND ( 'NONE', #35541, .T. ) ;
#8784 = EDGE_CURVE ( 'NONE', #69383, #90338, #199976, .T. ) ;
#8785 = DIRECTION ( 'NONE',  ( 0.000000000000000000, 0.000000000000000000, 1.000000000000000000 ) ) ;
#8786 = CARTESIAN_POINT ( 'NONE',  ( 6.681470773436232413, 6.689470745297396270, -0.7998128361456281477 ) ) ;
#8787 = ORIENTED_EDGE ( 'NONE', *, *, #101370, .F. ) ;
#8788 = CARTESIAN_POINT ( 'NONE',  ( -0.5000000000000091038, 3.999999999999948042, -0.5000000000000368594 ) ) ;
#8789 = VERTEX_POINT ( 'NONE', #79668 ) ;
#8790 = CARTESIAN_POINT ( 'NONE',  ( 2.631291878999729938, -0.1756591012599724722, 1.802909387868474766 ) ) ;
#8791 = AXIS2_PLACEMENT_3D ( 'NONE', #173451, #56481, #6635 ) ;
#8792 = ORIENTED_EDGE ( 'NONE', *, *, #52063, .F. ) ;
#8793 = CARTESIAN_POINT ( 'NONE',  ( 4.227444969362701421, 3.826440640544909400, 1.214306433183764966E-14 ) ) ;
#8794 = CARTESIAN_POINT ( 'NONE',  ( 4.573896719763862251, 6.429575154514868274, -1.599625672291273171 ) ) ;
#8795 = CARTESIAN_POINT ( 'NONE',  ( 3.738735263490736926, 1.721172062854194218, 0.5650376532472713986 ) ) ;
#8796 = CARTESIAN_POINT ( 'NONE',  ( 6.539320575229255361, 3.697401852651286180, 2.511149361313206096 ) ) ;
#8797 = CARTESIAN_POINT ( 'NONE',  ( -10.99943592164172834, -8.407420853759269619, 0.1113975120798851026 ) ) ;
#8798 = CARTESIAN_POINT ( 'NONE',  ( 5.702249273124194495, 6.094009171513759426, 0.7094654760324905496 ) ) ;
#8800 = CARTESIAN_POINT ( 'NONE',  ( 0.6823417656249969321, 14.52604166700806410, -1.181850606188757036 ) ) ;
#8799 = CARTESIAN_POINT ( 'NONE',  ( 4.017883236588020601, 1.847182159994051442, -0.2260418734564421939 ) ) ;
#8801 = CARTESIAN_POINT ( 'NONE',  ( 1.317839660544089853, 0.9426401379578488449, -1.667518220840451981 ) ) ;
#8802 = CARTESIAN_POINT ( 'NONE',  ( 1.184280053745472738, -1.780106929851841491, -0.4042017716930704219 ) ) ;
#8803 = FILL_AREA_STYLE_COLOUR ( '', #35287 ) ;
#8804 = FACE_OUTER_BOUND ( 'NONE', #114369, .T. ) ;
#8805 = CIRCLE ( 'NONE', #154154, 0.2000000000000005107 ) ;
#8806 = CARTESIAN_POINT ( 'NONE',  ( 5.448178351099921102, 7.506598249424609293, 1.250114376932524252 ) ) ;
#8807 = CARTESIAN_POINT ( 'NONE',  ( -11.48243876534946217, 13.79999999999998295, 3.199999999999997957 ) ) ;
#8808 = CARTESIAN_POINT ( 'NONE',  ( -1.519470924986878968, 8.761764328395900137, -2.483655442635856136 ) ) ;
#8809 = CARTESIAN_POINT ( 'NONE',  ( 1.737500000000001155, -2.639583332377418046, 3.009438278150922130 ) ) ;
#8810 = CARTESIAN_POINT ( 'NONE',  ( 5.992340707560141588, 9.934888558888093968, 0.7216878364870438212 ) ) ;
#8811 = CARTESIAN_POINT ( 'NONE',  ( 5.981301965652664698, -0.05197358493889753933, 1.968944643851434639 ) ) ;
#8812 = EDGE_CURVE ( 'NONE', #82411, #72492, #145783, .T. ) ;
#8813 = CARTESIAN_POINT ( 'NONE',  ( -2.428882075142555497, 5.985446187641602300, 1.040834085586084257E-14 ) ) ;
#8814 =( LENGTH_UNIT ( ) NAMED_UNIT ( * ) SI_UNIT ( .MILLI., .METRE. ) );
#8815 = VECTOR ( 'NONE', #127497, 1000.000000000000000 ) ;
#8816 = CARTESIAN_POINT ( 'NONE',  ( 0.9200049341780929257, 1.243975779098299927, -1.680105788963416780 ) ) ;
#8817 = CARTESIAN_POINT ( 'NONE',  ( 6.545928648987922038, 0.7364953880720639390, -1.780233924599901929 ) ) ;
#8818 = CARTESIAN_POINT ( 'NONE',  ( -5.368138756007025947, 8.350246751061767725, 1.199719254218452047 ) ) ;
#8819 = EDGE_CURVE ( 'NONE', #78057, #12050, #73389, .T. ) ;
#8820 = CARTESIAN_POINT ( 'NONE',  ( 1.606192798902779328, -0.6535759462080005244, -1.704761432720684144 ) ) ;
#8821 = CARTESIAN_POINT ( 'NONE',  ( 2.948105999307056635, 0.7938017206191756436, -2.059354589195587337 ) ) ;
#8822 = CARTESIAN_POINT ( 'NONE',  ( 0.5449873876890098945, 0.1430962203496731200, 1.907122450762772647 ) ) ;
#8823 = CARTESIAN_POINT ( 'NONE',  ( 1.451539297965124264, 1.489159454907125646, 1.289083465231783299 ) ) ;
#8824 = CARTESIAN_POINT ( 'NONE',  ( 3.122533544175498221, 0.05045625456868290531, 1.941573572215535393 ) ) ;
#8825 = ORIENTED_EDGE ( 'NONE', *, *, #7969, .T. ) ;
#8826 = DIRECTION ( 'NONE',  ( -0.01043841336116890263, 0.000000000000000000, -0.9999455182791217034 ) ) ;
#8828 = CARTESIAN_POINT ( 'NONE',  ( 6.297681919442434939, -1.347125180836796998, -1.284110876681610725 ) ) ;
#8827 = CARTESIAN_POINT ( 'NONE',  ( -5.276058054373441664, 6.184431147304315424, -1.199719254218453823 ) ) ;
#8829 = CARTESIAN_POINT ( 'NONE',  ( 3.725458348705031231, 7.568394850123006279, -1.734723475976807094E-15 ) ) ;
#8830 = CARTESIAN_POINT ( 'NONE',  ( -11.44786932348563901, 13.79999999999999893, -3.303370173849772051 ) ) ;
#8831 = LINE ( 'NONE', #74908, #60216 ) ;
#8832 = CARTESIAN_POINT ( 'NONE',  ( -4.762657100150483380, 8.778460060142702304, 0.000000000000000000 ) ) ;
#8833 = CARTESIAN_POINT ( 'NONE',  ( 2.103317784989285677, -0.4765762082987561321, 2.138964651187735821 ) ) ;
#8834 = CARTESIAN_POINT ( 'NONE',  ( 7.472478939787284169, 8.746922180287201698, 1.199719254218452935 ) ) ;
#8835 = CARTESIAN_POINT ( 'NONE',  ( 0.2026985623045176044, -4.140708350189164832, 1.000000000000004441 ) ) ;
#8836 = CARTESIAN_POINT ( 'NONE',  ( 2.701551412915685457, -0.5726843992823158480, 1.733614832724015731 ) ) ;
#8837 = CARTESIAN_POINT ( 'NONE',  ( -2.819205876637805641, 5.376491725131008259, -1.199719254218446718 ) ) ;
#8838 = CARTESIAN_POINT ( 'NONE',  ( -4.979135478818752958, 8.054126424104152804, -1.119915745145182440 ) ) ;
#8839 = CARTESIAN_POINT ( 'NONE',  ( 6.925078400183550364, 2.460400685555228950, 2.239421262742965268 ) ) ;
#8840 = CARTESIAN_POINT ( 'NONE',  ( 9.023114925094663619, 10.48572115315399245, 1.199719254218453823 ) ) ;
#8841 = CARTESIAN_POINT ( 'NONE',  ( 1.576654987853912449, -1.829214484822901055, -0.6046830185306437677 ) ) ;
#8842 = CARTESIAN_POINT ( 'NONE',  ( 5.576992410575341452, 1.811172876804711507, 0.7542287045681007607 ) ) ;
#8843 = CARTESIAN_POINT ( 'NONE',  ( -0.7500000000000179856, 14.79166666666666785, 1.299038105676658228 ) ) ;
#8844 = CARTESIAN_POINT ( 'NONE',  ( -7.202405917357668663, 9.425892875049191488, 1.599625672291295375 ) ) ;
#8845 = CARTESIAN_POINT ( 'NONE',  ( 5.169736645512481132, 4.925780929386339935, 0.7998128361456341429 ) ) ;
#8846 = CARTESIAN_POINT ( 'NONE',  ( -3.784134271545645412, 7.428924060196286483, 0.7216878364870338292 ) ) ;
#8847 = CARTESIAN_POINT ( 'NONE',  ( 3.323720213644492993, 7.029424015893889433, 1.040834085586084257E-14 ) ) ;
#8848 = CARTESIAN_POINT ( 'NONE',  ( -2.304522924643024773, 5.632434478818063361, 0.7216878364870317197 ) ) ;
#8849 = CARTESIAN_POINT ( 'NONE',  ( 5.629760504653214426, 1.996728726787128538, -0.5467053113129491937 ) ) ;
#8851 = CARTESIAN_POINT ( 'NONE',  ( -0.6823417656250003738, 2.280208333674753174, -1.181850606188749264 ) ) ;
#8850 = CARTESIAN_POINT ( 'NONE',  ( 0.000000000000000000, 9.719999999999982876, 0.000000000000000000 ) ) ;
#8852 = VERTEX_POINT ( 'NONE', #183553 ) ;
#8853 = CARTESIAN_POINT ( 'NONE',  ( 4.834794202738506463, 0.7220915915403209873, -2.182417960738481710 ) ) ;
#8854 = CARTESIAN_POINT ( 'NONE',  ( 5.829642864196151741, 9.745074408296771296, 0.7216878364870438212 ) ) ;
#8856 = CARTESIAN_POINT ( 'NONE',  ( 1.255262969126035860E-15, 7.849261790823902629, -10.24999999999998934 ) ) ;
#8855 = CARTESIAN_POINT ( 'NONE',  ( 5.316205630334249754, 7.295602216847000498, -1.443375672974078761 ) ) ;
#8857 = CARTESIAN_POINT ( 'NONE',  ( 0.1118211671861284034, -2.246746504121981403, 0.4537721782011410188 ) ) ;
#8858 = CARTESIAN_POINT ( 'NONE',  ( -0.005636796283178119316, -9.933099634201859374, -9.579656484007937678 ) ) ;
#8859 = CARTESIAN_POINT ( 'NONE',  ( -5.237192476628793614, 9.332084666034067055, 0.7998128361456291469 ) ) ;
#8860 = CARTESIAN_POINT ( 'NONE',  ( 4.400292492776470610, 1.500370014523371154, -1.232902440404326727 ) ) ;
#8861 = ORIENTED_EDGE ( 'NONE', *, *, #44771, .T. ) ;
#8862 = CARTESIAN_POINT ( 'NONE',  ( 7.727784369665023689, 11.95957283134381477, 1.040834085586084257E-14 ) ) ;
#8863 = ORIENTED_EDGE ( 'NONE', *, *, #42520, .F. ) ;
#8864 = CARTESIAN_POINT ( 'NONE',  ( 5.783449990912790106, 0.1341079605299954347, -1.907733270042926810 ) ) ;
#8865 = CARTESIAN_POINT ( 'NONE',  ( -0.02338929933905826986, 0.006294950389555685130, -1.710968156697996401 ) ) ;
#8866 = CARTESIAN_POINT ( 'NONE',  ( 5.331267653506235327, -1.592659417495114083, -1.236803018183525449 ) ) ;
#8868 = CARTESIAN_POINT ( 'NONE',  ( -4.177320726786328819, 5.966903162707725805, -1.443375672974066548 ) ) ;
#8867 = CARTESIAN_POINT ( 'NONE',  ( -7.883176251342026042, 11.28445716228600126, -1.199719254218446718 ) ) ;
#8869 = CARTESIAN_POINT ( 'NONE',  ( 1.001543065824772753E-15, -1.159374999522043481, 3.793834371823811669 ) ) ;
#8871 = CARTESIAN_POINT ( 'NONE',  ( 6.907488038778298645, -0.3811802009726448226, 1.734239976993730670 ) ) ;
#8870 = CARTESIAN_POINT ( 'NONE',  ( 1.464907584622468173, 0.1521959979720881595, -2.085151142678423497 ) ) ;
#8872 = CARTESIAN_POINT ( 'NONE',  ( 5.695935454815424848, 1.779625283580280382, 0.9480427965274510482 ) ) ;
#8874 = CARTESIAN_POINT ( 'NONE',  ( 2.625266749315146253, -2.138330473123546405, 0.8262727722977771805 ) ) ;
#8873 = CARTESIAN_POINT ( 'NONE',  ( 3.237364818613055473, 6.998952398349030268, -1.734723475976807094E-15 ) ) ;
#8875 = CARTESIAN_POINT ( 'NONE',  ( 2.009305037403839922, -0.8189296680943327633, -1.535607775426613086 ) ) ;
#8876 = CARTESIAN_POINT ( 'NONE',  ( 2.672263739372262137, 2.109986773948614225, -0.2121620573234672125 ) ) ;
#8877 = CARTESIAN_POINT ( 'NONE',  ( 1.500000000000035971, 7.750000000000000000, 10.86128356754324109 ) ) ;
#8878 = CARTESIAN_POINT ( 'NONE',  ( 2.143477642578191844, -0.07974179160761747653, -1.732128062886995057 ) ) ;
#8879 = CARTESIAN_POINT ( 'NONE',  ( -1.360316468750004448, 1.671875000341424666, -8.673617379884035472E-15 ) ) ;
#8880 = CARTESIAN_POINT ( 'NONE',  ( 2.049040314030759369, 1.621234533420016888, -0.9136741289750174300 ) ) ;
#8881 = CARTESIAN_POINT ( 'NONE',  ( 2.242849641980674491, -2.128998374728574117, -0.4250897845002408193 ) ) ;
#8882 = CARTESIAN_POINT ( 'NONE',  ( 3.485564796978508184, -0.5807542032013839339, 1.931124776463407189 ) ) ;
#8883 = CARTESIAN_POINT ( 'NONE',  ( 5.125000000000002665, -2.052068128417943171, 3.046444613966958600E-13 ) ) ;
#8884 = CARTESIAN_POINT ( 'NONE',  ( -0.7500000000000006661, 3.139583334016149418, -1.299038105676652011 ) ) ;
#8885 = CARTESIAN_POINT ( 'NONE',  ( 0.6043602652519001195, -0.6458173669235712788, -1.815047198766789327 ) ) ;
#8886 = CARTESIAN_POINT ( 'NONE',  ( 0.6823417656249934904, 14.44270833367473195, 1.181850606188764807 ) ) ;
#8887 = CARTESIAN_POINT ( 'NONE',  ( 3.955514033904330873, -1.931546270572735979, 1.097109147590840550 ) ) ;
#8888 = EDGE_LOOP ( 'NONE', ( #204730, #101929, #36498, #178099 ) ) ;
#8889 = CARTESIAN_POINT ( 'NONE',  ( 11.86239285000045740, 11.37999999999998302, 1.812080536912751061 ) ) ;
#8890 = CARTESIAN_POINT ( 'NONE',  ( 0.7499999999999885647, 0.7333333333333567072, 1.299038105676657340 ) ) ;
#8891 = CARTESIAN_POINT ( 'NONE',  ( 8.749089199520284410, 9.101692242395490240, 0.7998128361456481317 ) ) ;
#8892 = CARTESIAN_POINT ( 'NONE',  ( 0.6823417656249864960, -0.5739583329919112353, -1.181850606188749264 ) ) ;
#8893 = CARTESIAN_POINT ( 'NONE',  ( 6.135052730014136202, 2.072377209612641824, 0.8004311911904669063 ) ) ;
#8894 = CARTESIAN_POINT ( 'NONE',  ( 4.879329150013382410, -0.09822140645733207220, 1.959542894978071992 ) ) ;
#8896 = CARTESIAN_POINT ( 'NONE',  ( -6.155038550924159857, 8.203964280876741455, 1.443375672974078761 ) ) ;
#8895 = CARTESIAN_POINT ( 'NONE',  ( 9.734391104931951588, 11.41950637958454706, 1.082531754730548412 ) ) ;
#8897 = PRESENTATION_STYLE_ASSIGNMENT (( #158372 ) ) ;
#8898 = CARTESIAN_POINT ( 'NONE',  ( 5.923173471921922228, -0.06425113298673529316, 2.261675518886300473 ) ) ;
#8899 = CARTESIAN_POINT ( 'NONE',  ( -6.956742217587851052, 7.288823140040177506, 0.000000000000000000 ) ) ;
#8900 = CARTESIAN_POINT ( 'NONE',  ( 2.031754214314248408, 1.974575511506712289, -0.5964607296059397656 ) ) ;
#8901 = CARTESIAN_POINT ( 'NONE',  ( -5.392392409933270514, 7.314210449720692786, 1.599625672291269396 ) ) ;
#8902 = AXIS2_PLACEMENT_3D ( 'NONE', #55554, #61679, #171434 ) ;
#8903 = ORIENTED_EDGE ( 'NONE', *, *, #141806, .F. ) ;
#8904 = CARTESIAN_POINT ( 'NONE',  ( -0.7500000000000006661, 3.139583334016149418, -1.299038105676652011 ) ) ;
#8905 = CARTESIAN_POINT ( 'NONE',  ( 1.364683531249988535, 3.967708333674751842, -0.7879004041258239610 ) ) ;
#8906 = CARTESIAN_POINT ( 'NONE',  ( 4.428871017648271291, 0.08965458760558722706, 1.868499062828571367 ) ) ;
#8907 = CARTESIAN_POINT ( 'NONE',  ( 3.129275142338799665, 0.4248101585269374869, 1.681139380183617194 ) ) ;
#8908 = CARTESIAN_POINT ( 'NONE',  ( 2.559766225087984903, -1.198919528351283681, 1.261881593406234403 ) ) ;
#8909 = CARTESIAN_POINT ( 'NONE',  ( 1.294905083876269236, 1.870644729521577565, -1.324771388537665961 ) ) ;
#8910 = CARTESIAN_POINT ( 'NONE',  ( 0.9564373720404686363, 2.204146663617879476, -0.1098798544595935567 ) ) ;
#8911 = CARTESIAN_POINT ( 'NONE',  ( 4.458587642939345841, -1.868375113230103857, -0.9383987773294580892 ) ) ;
#8912 = CARTESIAN_POINT ( 'NONE',  ( 5.736261908918430130, 0.3809393362203088440, 1.904059320497718089 ) ) ;
#8914 = ORIENTED_EDGE ( 'NONE', *, *, #31028, .T. ) ;
#8913 = LINE ( 'NONE', #74994, #118908 ) ;
#8915 = CARTESIAN_POINT ( 'NONE',  ( 0.1412502902482688505, 0.7743183493036235321, 1.862015731718666078 ) ) ;
#8916 = PRESENTATION_STYLE_ASSIGNMENT (( #125961 ) ) ;
#8917 = DIRECTION ( 'NONE',  ( 0.000000000000000000, 1.000000000000000000, 0.000000000000000000 ) ) ;
#8918 = CARTESIAN_POINT ( 'NONE',  ( -9.826962411806732689, 10.35921099006301382, -0.7998128361456291469 ) ) ;
#8919 =( BOUNDED_CURVE ( )  B_SPLINE_CURVE ( 2, ( #6174, #187074, #72243, #201173, #52812, #36553, #70102, #204367, #193214 ),
 .UNSPECIFIED., .F., .T. ) 
 B_SPLINE_CURVE_WITH_KNOTS ( ( 3, 2, 2, 2, 3 ),
 ( 0.8482142857142856984, 0.8511904761904761640, 0.8571428571428570953, 0.8630952380952381375, 0.8660714285714286031 ),
 .UNSPECIFIED. ) 
 CURVE ( )  GEOMETRIC_REPRESENTATION_ITEM ( )  RATIONAL_B_SPLINE_CURVE ( ( 0.9330127018922194093, 0.9330127018922194093, 1.000000000000000000, 0.8660254037844387076, 1.000000000000000000, 0.8660254037844387076, 1.000000000000000000, 0.9330127018922194093, 0.9330127018922194093 ) ) 
 REPRESENTATION_ITEM ( '' )  );
#8920 = CARTESIAN_POINT ( 'NONE',  ( 7.806797523370503811, 8.002351953554066810, 1.040834085586084257E-14 ) ) ;
#8921 = CARTESIAN_POINT ( 'NONE',  ( 1.419999999999999485, 7.140846818246212813, 4.154462424328221104 ) ) ;
#8922 = CARTESIAN_POINT ( 'NONE',  ( 4.705575438601840688, -0.4840451379145363497, 1.760283039881085809 ) ) ;
#8923 = CARTESIAN_POINT ( 'NONE',  ( 1.659489206604364941, -1.893029981318217647, -1.133929415002648655 ) ) ;
#8924 = EDGE_LOOP ( 'NONE', ( #165319, #163579, #64494, #119140, #135611 ) ) ;
#8925 = CARTESIAN_POINT ( 'NONE',  ( -3.309598895067336510, 6.875299454304925284, 0.000000000000000000 ) ) ;
#8926 = CARTESIAN_POINT ( 'NONE',  ( -1.642778471874998480, -2.588541666188707957, 2.845375778867863303 ) ) ;
#8927 = CARTESIAN_POINT ( 'NONE',  ( -8.616370316684697883, 10.01118577667568132, -1.199719254218446718 ) ) ;
#8928 = CARTESIAN_POINT ( 'NONE',  ( 0.8615889817988997557, -1.594800366461980756, -1.239340803694780835 ) ) ;
#8930 = ADVANCED_FACE ( 'NONE', ( #200843 ), #104458, .F. ) ;
#8929 = CARTESIAN_POINT ( 'NONE',  ( -7.247736482493301047, 14.00000000000600231, -10.57961706324514850 ) ) ;
#8931 = CARTESIAN_POINT ( 'NONE',  ( -3.135678666510573365, 6.880318554229450712, 0.000000000000000000 ) ) ;
#8932 = CARTESIAN_POINT ( 'NONE',  ( 3.379601846096703888, -1.794663673993960540, 0.4920686967917423105 ) ) ;
#8933 = CARTESIAN_POINT ( 'NONE',  ( 2.205172540517054802, 5.724451730578533848, 1.040834085586084257E-14 ) ) ;
#8934 = DIRECTION ( 'NONE',  ( 0.000000000000000000, 0.000000000000000000, -1.000000000000000000 ) ) ;
#8935 = VERTEX_POINT ( 'NONE', #69782 ) ;
#8936 = ORIENTED_EDGE ( 'NONE', *, *, #6348, .T. ) ;
#8937 = CARTESIAN_POINT ( 'NONE',  ( -5.440899717785814715, 5.242137847038546461, 0.7998128361456341429 ) ) ;
#8938 = CARTESIAN_POINT ( 'NONE',  ( -8.188234707649510113, 11.64035869464474082, -1.199719254218446718 ) ) ;
#8939 = CARTESIAN_POINT ( 'NONE',  ( 3.773894676421325478, 1.015518775504126614, 1.516979517045339509 ) ) ;
#8941 = CARTESIAN_POINT ( 'NONE',  ( 1.737500000000001155, -3.033333333333332327, 3.009438278150922130 ) ) ;
#8940 = CARTESIAN_POINT ( 'NONE',  ( -3.546339698426324460, 6.295090860542775779, -1.199719254218450271 ) ) ;
#8942 = CARTESIAN_POINT ( 'NONE',  ( 6.512538272292041519, 6.827515365185738538, -0.5364851146780359459 ) ) ;
#8943 = CARTESIAN_POINT ( 'NONE',  ( 6.872432811717262169, -0.4447407475622888740, 1.973694069355651282 ) ) ;
#8944 = CARTESIAN_POINT ( 'NONE',  ( 6.175717916360309090, -0.9808100270635997653, 1.557957644481674730 ) ) ;
#8945 = CARTESIAN_POINT ( 'NONE',  ( 4.336755680664809098, 2.262710760593138470, 0.4526611301470875870 ) ) ;
#8946 = CARTESIAN_POINT ( 'NONE',  ( 4.472210567661338843, 6.310941310395290493, 1.599625672291261402 ) ) ;
#8947 = CARTESIAN_POINT ( 'NONE',  ( 0.4564140224992017658, 0.7863226074062683590, 1.905069713448727775 ) ) ;
#8948 = CARTESIAN_POINT ( 'NONE',  ( 5.147291874682557555, 9.156924287104992288, 0.7998128361456462443 ) ) ;
#8949 = EDGE_CURVE ( 'NONE', #43706, #168291, #35160, .T. ) ;
#8950 = ADVANCED_FACE ( 'NONE', ( #72994 ), #17597, .T. ) ;
#8951 = CARTESIAN_POINT ( 'NONE',  ( 5.343244854357415363, -1.283103863925443955, 1.906741504182138502 ) ) ;
#8952 = CARTESIAN_POINT ( 'NONE',  ( -1.020158943445720556, -3.232243495192077987, 3.126638183162731899 ) ) ;
#8953 = CARTESIAN_POINT ( 'NONE',  ( -3.546339698426324460, 6.295090860542775779, -1.199719254218450271 ) ) ;
#8954 = STYLED_ITEM ( 'NONE', ( #189453 ), #7720 ) ;
#8955 = CARTESIAN_POINT ( 'NONE',  ( 6.244977087980838171, -1.579202250953464670, 1.002420361074819688 ) ) ;
#8957 = ORIENTED_EDGE ( 'NONE', *, *, #129734, .T. ) ;
#8956 = CIRCLE ( 'NONE', #115848, 0.09999999999999982514 ) ;
#8959 = CARTESIAN_POINT ( 'NONE',  ( -4.122561227007127016, 6.967349310553715647, 1.199719254218452935 ) ) ;
#8958 = CARTESIAN_POINT ( 'NONE',  ( 2.724755696555291262, 1.382288352666941389, -1.321784923088549446 ) ) ;
#8960 = CARTESIAN_POINT ( 'NONE',  ( 3.967548030458594166, 0.2710504330169676845, -2.190103208553782821 ) ) ;
#8961 = CARTESIAN_POINT ( 'NONE',  ( 4.733676700703519202, 0.6609272643324247687, -2.011644693266708916 ) ) ;
#8962 = CARTESIAN_POINT ( 'NONE',  ( 1.224999999999961009, 0.9583333340161364067, -0.7072540797573237947 ) ) ;
#8963 = CARTESIAN_POINT ( 'NONE',  ( 6.883263157960373135, 0.5713788194823016253, 2.097868537683903245 ) ) ;
#8964 = CARTESIAN_POINT ( 'NONE',  ( -0.2110808730067326444, 2.048707873362776599, -2.213945011526836204 ) ) ;
#8965 = CARTESIAN_POINT ( 'NONE',  ( 4.706088717274896638, 7.544168365912456764, 1.082531754730548412 ) ) ;
#8966 = CIRCLE ( 'NONE', #12352, 0.08000000000000020983 ) ;
#8967 = CARTESIAN_POINT ( 'NONE',  ( -5.790741006368224753, 5.928488393617260321, 0.7216878364870257245 ) ) ;
#8968 = CARTESIAN_POINT ( 'NONE',  ( 2.854834436329793057, 0.7764391075696615019, 2.173172238055173455 ) ) ;
#8969 = CARTESIAN_POINT ( 'NONE',  ( 3.156644782993088150, -0.5669402238272451822, -1.878178299617596192 ) ) ;
#8970 = CARTESIAN_POINT ( 'NONE',  ( -5.472651281771599763, 6.413789912602166687, 1.199719254218452935 ) ) ;
#8971 = CARTESIAN_POINT ( 'NONE',  ( 6.948098685450462497, -0.8862217868219750549, 1.860397500250488001 ) ) ;
#8972 = CARTESIAN_POINT ( 'NONE',  ( 4.690757960648234359, 4.574898496952131133, 0.7216878364870317197 ) ) ;
#8973 = CARTESIAN_POINT ( 'NONE',  ( 4.309512724297349884, 6.121127159803966933, 1.599625672291261402 ) ) ;
#8974 = ORIENTED_EDGE ( 'NONE', *, *, #170968, .F. ) ;
#8975 = CARTESIAN_POINT ( 'NONE',  ( 5.067592334412735156, 1.357865985192594271, 1.490972259599515848 ) ) ;
#8976 = CARTESIAN_POINT ( 'NONE',  ( -9.982881178363895103, 10.54111621771303753, 1.040834085586084257E-14 ) ) ;
#8977 = CARTESIAN_POINT ( 'NONE',  ( 11.80248046418316044, 13.79999999999998295, 1.695421849633139466 ) ) ;
#8978 = CARTESIAN_POINT ( 'NONE',  ( -11.52570357830391323, 8.091488070261075194, -2.173620758456770830 ) ) ;
#8979 = CARTESIAN_POINT ( 'NONE',  ( 9.368847842243145152, 10.88907622316056312, 1.199719254218453823 ) ) ;
#8980 = CARTESIAN_POINT ( 'NONE',  ( 1.516727516949545107, 0.8775410692131856427, 1.985969635014148915 ) ) ;
#8981 = FACE_OUTER_BOUND ( 'NONE', #67316, .T. ) ;
#8982 = CARTESIAN_POINT ( 'NONE',  ( -7.093660771577591895, 14.55189863974096554, -9.633804998953056753 ) ) ;
#8983 = CARTESIAN_POINT ( 'NONE',  ( 5.096922329222960180, 6.645262723539179461, 1.370935683266294003 ) ) ;
#8984 = CARTESIAN_POINT ( 'NONE',  ( 4.690754089986846509, 8.373302309308519042, 0.6171781843518510113 ) ) ;
#8985 = CARTESIAN_POINT ( 'NONE',  ( 0.6673476085290538373, 0.2044725723429566266, -2.050631486922994906 ) ) ;
#8987 = CARTESIAN_POINT ( 'NONE',  ( 4.363950690066983107, 4.004001632660354915, -0.1812806842866887536 ) ) ;
#8986 = CARTESIAN_POINT ( 'NONE',  ( 0.07775346131142897577, 1.984126704040774181, -2.702190870904349840 ) ) ;
#8988 = CARTESIAN_POINT ( 'NONE',  ( -1.364683531250014514, 0.2802083336747505649, 0.7879004041258379498 ) ) ;
#8989 = FILL_AREA_STYLE ('',( #43654 ) ) ;
#8990 = ORIENTED_EDGE ( 'NONE', *, *, #65446, .T. ) ;
#8991 = CARTESIAN_POINT ( 'NONE',  ( 3.668532269402470458, 0.6909111621477401766, 1.783275653667259597 ) ) ;
#8992 = CARTESIAN_POINT ( 'NONE',  ( 5.172599881030584434, -1.667270648082047835, -0.5941068299562983768 ) ) ;
#8993 = CARTESIAN_POINT ( 'NONE',  ( 7.062871678076271920, 7.204714810702593120, -0.7998128361456341429 ) ) ;
#8994 = CARTESIAN_POINT ( 'NONE',  ( -5.278201874421821316, 5.052323696447222900, 0.7998128361456341429 ) ) ;
#8996 = CARTESIAN_POINT ( 'NONE',  ( -0.2236198635829286518, -0.4190533842500678841, -1.875677477222786438 ) ) ;
#8995 = CARTESIAN_POINT ( 'NONE',  ( 0.000000000000000000, 0.5000000000000004441, 0.000000000000000000 ) ) ;
#8997 = CARTESIAN_POINT ( 'NONE',  ( -1.402160292154681736E-14, 0.2125000000000202283, 1.732050807568877637 ) ) ;
#8998 = CARTESIAN_POINT ( 'NONE',  ( 0.9946828900261883710, 2.039433816042154124, 0.3556643922909968891 ) ) ;
#8999 = CARTESIAN_POINT ( 'NONE',  ( 0.7499999999999920064, 5.733333333333353821, 1.299038105676669330 ) ) ;
#9000 = CARTESIAN_POINT ( 'NONE',  ( 6.227412191919261986, -1.760757567598171480, 0.6321290105378990498 ) ) ;
#9001 = CARTESIAN_POINT ( 'NONE',  ( 2.068725586703868746, -1.668841220716179130, -0.7407507213199536755 ) ) ;
#9003 = CARTESIAN_POINT ( 'NONE',  ( 5.148720134264945791, 7.772403765597828418, 1.171659602702241676 ) ) ;
#9002 = CARTESIAN_POINT ( 'NONE',  ( 5.514374426699260923, -0.9893691592960799364, -1.972764877262770833 ) ) ;
#9004 = CARTESIAN_POINT ( 'NONE',  ( 1.364683531249986537, 0.6135416670080880985, 0.7879004041258500513 ) ) ;
#9005 = CARTESIAN_POINT ( 'NONE',  ( 3.367685602802727551, -0.4050715705573506575, 2.022353529335896294 ) ) ;
#9006 = CARTESIAN_POINT ( 'NONE',  ( -7.335124800193271177, 8.516399340768996851, -1.199719254218452935 ) ) ;
#9007 = CARTESIAN_POINT ( 'NONE',  ( 7.404724451357931336, 11.79059562655963056, 0.7998128361456462443 ) ) ;
#9008 = DIRECTION ( 'NONE',  ( 1.276756478318932585E-15, -1.000000000000000000, 1.665334536937738262E-16 ) ) ;
#9009 = CARTESIAN_POINT ( 'NONE',  ( 0.7730135719010817752, -2.035059957909639561, -0.7290066412228360937 ) ) ;
#9010 = CARTESIAN_POINT ( 'NONE',  ( 7.205232291019763480, 7.370802192470005565, -0.7998128361456341429 ) ) ;
#9011 = CARTESIAN_POINT ( 'NONE',  ( 5.793440749948310042, -1.873300974885267589, 0.8818263447485861217 ) ) ;
#9012 = CARTESIAN_POINT ( 'NONE',  ( 1.364683531249986537, -0.5739583329919174526, 0.7879004041258500513 ) ) ;
#9013 = CARTESIAN_POINT ( 'NONE',  ( 3.761131992884462871, -1.904433681825665969, -1.022602951024270679 ) ) ;
#9014 = CARTESIAN_POINT ( 'NONE',  ( -4.784432227305938312, 8.165582598138012571, -0.7895561949947740299 ) ) ;
#9016 = CARTESIAN_POINT ( 'NONE',  ( 2.242563829109287088, -1.923402688547710904, -0.3857071251459272543 ) ) ;
#9015 = CARTESIAN_POINT ( 'NONE',  ( 3.123699121837515413, -0.3918110498563053268, 1.981120561552232262 ) ) ;
#9017 = CARTESIAN_POINT ( 'NONE',  ( 6.720655732516655156, 7.629137130509086262, 2.673739711112704143 ) ) ;
#9018 = B_SPLINE_CURVE_WITH_KNOTS ( 'NONE', 3,
 ( #144578, #146697, #210592, #48129 ),
 .UNSPECIFIED., .F., .F.,
 ( 4, 4 ),
 ( 0.000000000000000000, 2.032232339058191815E-05 ),
 .UNSPECIFIED. ) ;
#9019 = PRODUCT_DEFINITION_SHAPE ( 'NONE', 'NONE',  #214428 ) ;
#9020 = EDGE_CURVE ( 'NONE', #80420, #5098, #197284, .T. ) ;
#9023 = CARTESIAN_POINT ( 'NONE',  ( 7.646435448427411963, 8.023188899361205273, -0.7216878364870257245 ) ) ;
#9022 = CARTESIAN_POINT ( 'NONE',  ( 3.475000000000000533, -2.304166666666668473, 2.006292185433948827 ) ) ;
#9021 = CARTESIAN_POINT ( 'NONE',  ( -0.4465194593918104249, 3.080450244942127380, 0.4155024747329021939 ) ) ;
#9024 = CARTESIAN_POINT ( 'NONE',  ( -7.930593509350902792, 8.217056947189661287, -0.7998128361456362523 ) ) ;
#9025 = CARTESIAN_POINT ( 'NONE',  ( 1.622280145275534435, 1.995268681201247452, 0.2910785328335343536 ) ) ;
#9027 = CARTESIAN_POINT ( 'NONE',  ( 6.251546423958430410, 2.185849743821382862, -0.1592787069685034917 ) ) ;
#9026 = CARTESIAN_POINT ( 'NONE',  ( -5.362413449404877852, 6.214902764849178141, -1.199719254218446718 ) ) ;
#9029 = AXIS2_PLACEMENT_3D ( 'NONE', #126335, #173967, #90573 ) ;
#9028 = CARTESIAN_POINT ( 'NONE',  ( 0.2999999999999999334, 3.950000000000001954, -1.007084189318397938 ) ) ;
#9030 = CARTESIAN_POINT ( 'NONE',  ( 6.099862406061942188, 1.323743610676546334, 1.380425988546908567 ) ) ;
#9031 = CARTESIAN_POINT ( 'NONE',  ( -2.103486388414573138, 5.605817886458954291, 1.040834085586084257E-14 ) ) ;
#9032 = CARTESIAN_POINT ( 'NONE',  ( 4.473827502385202770, 8.163289819517311585, 1.040834085586084257E-14 ) ) ;
#9034 = CARTESIAN_POINT ( 'NONE',  ( 3.269157808572686896, 1.821735364950356484, -0.8647411805496332260 ) ) ;
#9033 = CARTESIAN_POINT ( 'NONE',  ( -7.497295758232712437, 11.69066945133944380, -0.7216878364870267237 ) ) ;
#9035 = CARTESIAN_POINT ( 'NONE',  ( 0.7499999999999902300, 3.816666666666690411, -1.299038105676658228 ) ) ;
#9036 = CARTESIAN_POINT ( 'NONE',  ( 1.364683531249997417, 14.04687500034140157, 2.602085213965210642E-15 ) ) ;
#9037 = CARTESIAN_POINT ( 'NONE',  ( -0.02338929933905826986, 0.006294950389555685130, -1.710968156697996401 ) ) ;
#9038 = CARTESIAN_POINT ( 'NONE',  ( 6.851666526859736983, 9.086973262793417661, -1.599625672291269396 ) ) ;
#9039 = CARTESIAN_POINT ( 'NONE',  ( 9.259855728453651125, 9.905512559391842942, 1.040834085586084257E-14 ) ) ;
#9040 = CARTESIAN_POINT ( 'NONE',  ( -0.4032277238576902900, 3.019957635004387075, 0.4115402804778086621 ) ) ;
#9041 = CARTESIAN_POINT ( 'NONE',  ( 4.253091631423633778, -1.553859266942819284, -1.041061106808522929 ) ) ;
#9042 = ADVANCED_FACE ( 'NONE', ( #44812 ), #63180, .T. ) ;
#9043 = CARTESIAN_POINT ( 'NONE',  ( -11.48243876534946217, 9.799999999999982947, 3.199999999999997957 ) ) ;
#9044 = CARTESIAN_POINT ( 'NONE',  ( 0.6903901511902330590, 1.067356595782501749, -1.773781848916009096 ) ) ;
#9045 = CARTESIAN_POINT ( 'NONE',  ( 0.4366903032816606411, -8.287795860939844772, -10.40306649911374670 ) ) ;
#9046 = ORIENTED_EDGE ( 'NONE', *, *, #41548, .F. ) ;
#9047 = CARTESIAN_POINT ( 'NONE',  ( 4.095444919779759552, 6.935713618788495793, 1.199719254218451159 ) ) ;
#9048 = PRESENTATION_STYLE_ASSIGNMENT (( #7964 ) ) ;
#9049 = CARTESIAN_POINT ( 'NONE',  ( 0.1580966392830873424, 1.806712829659435027, 0.1331060069221217668 ) ) ;
#9050 = CARTESIAN_POINT ( 'NONE',  ( 3.390947816749319443, 6.970206529600588397, -1.734723475976807094E-15 ) ) ;
#9051 = CARTESIAN_POINT ( 'NONE',  ( 1.815167269671989603, 0.3943365573011955449, 0.6613654005181966999 ) ) ;
#9052 = ORIENTED_EDGE ( 'NONE', *, *, #21416, .F. ) ;
#9053 = CARTESIAN_POINT ( 'NONE',  ( 7.849807752188022292, 11.14156422998596696, -1.082531754730543083 ) ) ;
#9054 = STYLED_ITEM ( 'NONE', ( #63098 ), #125431 ) ;
#9056 = CARTESIAN_POINT ( 'NONE',  ( 8.697719238366680372, 10.10609285197134533, 1.199719254218462483 ) ) ;
#9055 = CARTESIAN_POINT ( 'NONE',  ( 1.680054527999317759, -1.087118939145682583, -1.632918184844594611 ) ) ;
#9057 = CARTESIAN_POINT ( 'NONE',  ( 6.591422782704708716, -0.4110296003016626898, 1.877638232857116174 ) ) ;
#9058 = CARTESIAN_POINT ( 'NONE',  ( -11.41381676900475917, 13.53041960022397916, 3.704697931490214646 ) ) ;
#9059 = CARTESIAN_POINT ( 'NONE',  ( -2.200353596358113339, -3.182436278638796523, 2.524625639462166671 ) ) ;
#9061 = ORIENTED_EDGE ( 'NONE', *, *, #16612, .F. ) ;
#9060 = CARTESIAN_POINT ( 'NONE',  ( 4.609409038966229666, 6.400729850259146758, -1.443375672974051449 ) ) ;
#9062 = ADVANCED_FACE ( 'NONE', ( #24091 ), #141106, .F. ) ;
#9063 = CARTESIAN_POINT ( 'NONE',  ( -7.375272376154081932, 10.58793962461302485, -1.082531754730543971 ) ) ;
#9064 = CARTESIAN_POINT ( 'NONE',  ( 2.641676655999642076, -1.601130012699041982, -1.452526871000489495 ) ) ;
#9065 = CARTESIAN_POINT ( 'NONE',  ( -3.772911886352873445, 7.623757310712140800, 0.7998128361456352531 ) ) ;
#9066 = CARTESIAN_POINT ( 'NONE',  ( 7.675324359112103423, 8.127168971818530707, 0.7216878364870267237 ) ) ;
#9067 = CARTESIAN_POINT ( 'NONE',  ( -3.521367211247373508, 5.131347717920458962, -1.599625672291256295 ) ) ;
#9068 = ADVANCED_FACE ( 'NONE', ( #11036 ), #120962, .T. ) ;
#9069 = CARTESIAN_POINT ( 'NONE',  ( 6.036143291503483610, 0.8974207610169572247, -1.589712159477923992 ) ) ;
#9070 = CARTESIAN_POINT ( 'NONE',  ( 11.30883932465314601, 7.475091753786390569, 3.226902027701133324 ) ) ;
#9071 = CARTESIAN_POINT ( 'NONE',  ( 1.387891646316425476, -0.8902153388929586741, 1.759007621864362214 ) ) ;
#9072 = CARTESIAN_POINT ( 'NONE',  ( 4.060738401289211374, 0.5150538496448524572, 1.841637258418599155 ) ) ;
#9073 = VERTEX_POINT ( 'NONE', #124895 ) ;
#9074 = CARTESIAN_POINT ( 'NONE',  ( -11.45842088241054135, 10.00693529122955283, -3.566211699757781073 ) ) ;
#9075 = CARTESIAN_POINT ( 'NONE',  ( 5.389095231685527843, 0.1428881311146198430, 1.964408359074652388 ) ) ;
#9076 = EDGE_LOOP ( 'NONE', ( #141587, #36747, #27725, #90938, #169125, #107784 ) ) ;
#9077 = CARTESIAN_POINT ( 'NONE',  ( 6.269086997039995168, 1.857158234874217939, -0.5679118324898363435 ) ) ;
#9078 = VERTEX_POINT ( 'NONE', #179964 ) ;
#9079 = CARTESIAN_POINT ( 'NONE',  ( -5.098748287191073203, 8.106234214101666780, 1.199719254218452935 ) ) ;
#9081 = CARTESIAN_POINT ( 'NONE',  ( 6.818239715405162826, -6.631671885545136647, -6.594971855056806831 ) ) ;
#9080 = CARTESIAN_POINT ( 'NONE',  ( -5.255720823952942489, 6.160704378480398979, -1.199719254218453823 ) ) ;
#9082 = CARTESIAN_POINT ( 'NONE',  ( 7.309254211098767051, 7.700087132469628948, 0.7216878364870267237 ) ) ;
#9084 = ORIENTED_EDGE ( 'NONE', *, *, #112034, .F. ) ;
#9083 = CARTESIAN_POINT ( 'NONE',  ( 4.107995242876061326, -0.7289348763114507079, 1.768098669557085056 ) ) ;
#9085 = CARTESIAN_POINT ( 'NONE',  ( 0.09513611692719620150, -0.4880922032983874281, -2.160105283315366442 ) ) ;
#9086 = CARTESIAN_POINT ( 'NONE',  ( 9.534866695232221190, 3.538528462892257309, -7.286654780214764315 ) ) ;
#9087 = CARTESIAN_POINT ( 'NONE',  ( 6.252595736715376162, 1.991502868314236174, 0.2931975281106109499 ) ) ;
#9088 = DIRECTION ( 'NONE',  ( -0.9446243521954068578, 3.252606517456503205E-14, -0.3281536732072456997 ) ) ;
#9089 = CARTESIAN_POINT ( 'NONE',  ( 6.305291373979138747, 1.520805759102667132, 1.009792402853857407 ) ) ;
#9090 = CARTESIAN_POINT ( 'NONE',  ( 1.732962091629593804, -1.965256999408044436, -0.6514315320021792921 ) ) ;
#9091 = CARTESIAN_POINT ( 'NONE',  ( -7.549192604710863286, 7.701812881784464437, -0.7998128361456291469 ) ) ;
#9092 = CIRCLE ( 'NONE', #5650, 0.1599999999999999756 ) ;
#9093 = CARTESIAN_POINT ( 'NONE',  ( -5.764421489320544545, 7.269302474779911982, -1.197982331091128616 ) ) ;
#9094 = CARTESIAN_POINT ( 'NONE',  ( 1.257518954444996062, 2.841479010054028365, -0.7749999999999926947 ) ) ;
#9095 = CARTESIAN_POINT ( 'NONE',  ( 6.244977087980838171, -1.579202250953464670, 1.002420361074819688 ) ) ;
#9096 = CARTESIAN_POINT ( 'NONE',  ( 5.799137018343234473, 7.788745826199009237, -1.599625672291262513 ) ) ;
#9097 = FILL_AREA_STYLE ('',( #178013 ) ) ;
#9098 = CARTESIAN_POINT ( 'NONE',  ( 5.072158865288243668, 6.050511776658669127, 1.082531754730549078 ) ) ;
#9099 = DIRECTION ( 'NONE',  ( 0.000000000000000000, 0.000000000000000000, 1.000000000000000000 ) ) ;
#9100 = CARTESIAN_POINT ( 'NONE',  ( 0.6823417656249969321, 12.33854166700806765, -1.181850606188757036 ) ) ;
#9102 = CARTESIAN_POINT ( 'NONE',  ( -6.444921918449773024, 8.612437886315108315, 1.599625672291269396 ) ) ;
#9101 = CARTESIAN_POINT ( 'NONE',  ( 6.825078400183581806, 2.095667212029386661, 2.065897939415714646 ) ) ;
#9103 = CARTESIAN_POINT ( 'NONE',  ( 5.010307813345768579, -1.644221866518974728, 0.5513857468827707553 ) ) ;
#9104 = CARTESIAN_POINT ( 'NONE',  ( -5.590039407536138150, 5.416134151747256986, 0.000000000000000000 ) ) ;
#9105 = CARTESIAN_POINT ( 'NONE',  ( 2.747004861044194612, -0.3495022371792326221, -2.040372298647576965 ) ) ;
#9106 = CARTESIAN_POINT ( 'NONE',  ( 3.216528272283057710, 2.066224784428410732, 0.4612988732951432969 ) ) ;
#9107 = CARTESIAN_POINT ( 'NONE',  ( 6.938021921891177612, 9.117444880338284818, -1.599625672291262513 ) ) ;
#9108 = CARTESIAN_POINT ( 'NONE',  ( 6.520158902582592120, 5.290451655907108197, -2.438235897557449849 ) ) ;
#9109 = CARTESIAN_POINT ( 'NONE',  ( 2.026157484158600752, 1.007934145216189625, 1.691802187876802810 ) ) ;
#9110 = CARTESIAN_POINT ( 'NONE',  ( 5.577782935947014131, 6.368007920784547693, 1.193350709755973682 ) ) ;
#9112 = CARTESIAN_POINT ( 'NONE',  ( -0.4648879685169910458, -7.768188185258928513, -9.920930332858617362 ) ) ;
#9111 = CARTESIAN_POINT ( 'NONE',  ( -3.475000000000000533, -1.779166666666666785, -2.006292185433948827 ) ) ;
#9113 = CARTESIAN_POINT ( 'NONE',  ( 3.925942518080671739, 1.227467849647005282, -1.935749465030587313 ) ) ;
#9114 = CARTESIAN_POINT ( 'NONE',  ( 2.332394550857110893, 1.770734860448031300, 0.4440693575865002907 ) ) ;
#9115 = AXIS2_PLACEMENT_3D ( 'NONE', #185231, #165004, #168998 ) ;
#9116 = CARTESIAN_POINT ( 'NONE',  ( 6.052789233858158369, 6.026285292448116948, 0.000000000000000000 ) ) ;
#9117 = CARTESIAN_POINT ( 'NONE',  ( 5.734735788456138295, 8.673980272298743799, -1.082531754730537976 ) ) ;
#9118 = CARTESIAN_POINT ( 'NONE',  ( -7.212047647465563038, 10.50147379109678880, -1.199719254218446718 ) ) ;
#9119 = CARTESIAN_POINT ( 'NONE',  ( 2.812746579430201788, -0.5882912493809470122, -1.925304731621484633 ) ) ;
#9120 = CARTESIAN_POINT ( 'NONE',  ( 2.553501467334079678, 1.513274546892771966, 1.248348448719404757 ) ) ;
#9121 = CARTESIAN_POINT ( 'NONE',  ( -7.320512876374914768, 10.62801655815766999, 1.199719254218453823 ) ) ;
#9122 = CARTESIAN_POINT ( 'NONE',  ( -6.358937740009323214, 7.377514437221045718, -1.199719254218446718 ) ) ;
#9123 = DIRECTION ( 'NONE',  ( 1.000000000000000000, -0.000000000000000000, -0.000000000000000000 ) ) ;
#9125 = CARTESIAN_POINT ( 'NONE',  ( 4.522157790900214636, 1.087963700580677484, -1.395837783952274647 ) ) ;
#9124 = CARTESIAN_POINT ( 'NONE',  ( 4.541018360983569480, -1.615799657739678263, -1.326631217474142366 ) ) ;
#9126 = CARTESIAN_POINT ( 'NONE',  ( -8.752560967067513076, 14.99999998465384365, 9.356054886187056496 ) ) ;
#9127 = B_SPLINE_CURVE_WITH_KNOTS ( 'NONE', 3,
 ( #10160, #28559, #94648, #126138 ),
 .UNSPECIFIED., .F., .F.,
 ( 4, 4 ),
 ( 0.000000000000000000, 0.0007717018656778090215 ),
 .UNSPECIFIED. ) ;
#9128 = CARTESIAN_POINT ( 'NONE',  ( 0.4983068789779531160, -0.7420642642406435341, -2.062120472104383317 ) ) ;
#9129 = CARTESIAN_POINT ( 'NONE',  ( 5.525286087770139964, -1.108758243214434724, -1.341423578285575235 ) ) ;
#9130 = CARTESIAN_POINT ( 'NONE',  ( 7.995557903757111617, 10.35123685918189729, 1.599625672291281386 ) ) ;
#9131 = DIRECTION ( 'NONE',  ( -0.000000000000000000, -1.000000000000000000, 0.000000000000000000 ) ) ;
#9132 = CARTESIAN_POINT ( 'NONE',  ( 6.012345284929816458, -2.165844811509042511, 0.7704031996330994447 ) ) ;
#9133 = CARTESIAN_POINT ( 'NONE',  ( 2.970447988400423789, 6.576210002780722874, 0.4422704740705263871 ) ) ;
#9134 = CARTESIAN_POINT ( 'NONE',  ( 6.046190555029876457, 1.600718489819895174, -0.6667736897630163195 ) ) ;
#9135 = CARTESIAN_POINT ( 'NONE',  ( 6.385953923436008317, -2.015982004707029596, 0.05432014494890363698 ) ) ;
#9136 = CARTESIAN_POINT ( 'NONE',  ( 6.268071979561871565, -2.155543878041016992, 0.2595383615264702515 ) ) ;
#9137 = DIRECTION ( 'NONE',  ( -0.2684563758389304500, -0.000000000000000000, -0.9632918427306581544 ) ) ;
#9138 = CARTESIAN_POINT ( 'NONE',  ( 0.4798920220053382590, -0.7558346266652364864, 1.978032726644059158 ) ) ;
#9139 = CARTESIAN_POINT ( 'NONE',  ( 4.031250000000002665, -0.7852924748301974844, -1.895863743163994863 ) ) ;
#9140 = DIRECTION ( 'NONE',  ( 1.000000000000000000, 0.000000000000000000, 0.000000000000000000 ) ) ;
#9141 = CARTESIAN_POINT ( 'NONE',  ( 4.788067677947292822, -0.9085903742032475083, 1.698673095886160000 ) ) ;
#9142 = CARTESIAN_POINT ( 'NONE',  ( -0.7500000000000006661, 11.73958333401613174, -1.299038105676657340 ) ) ;
#9143 = CARTESIAN_POINT ( 'NONE',  ( 1.032228388637240313, -2.166051452891520679, 0.4916964420428306948 ) ) ;
#9144 = ORIENTED_EDGE ( 'NONE', *, *, #76230, .F. ) ;
#9145 = CARTESIAN_POINT ( 'NONE',  ( -1.499999999999997780, 4.400000000000021672, 1.214306433183764966E-14 ) ) ;
#9146 = CARTESIAN_POINT ( 'NONE',  ( 5.996784015946103885, 5.890669528225568996, 1.040834085586084257E-14 ) ) ;
#9147 = CARTESIAN_POINT ( 'NONE',  ( 5.296431564432884542, 9.330920591813708143, 1.040834085586084257E-14 ) ) ;
#9148 = CARTESIAN_POINT ( 'NONE',  ( 3.159039748919801216, 0.5414197367904579616, 2.154182169225922205 ) ) ;
#9149 = CARTESIAN_POINT ( 'NONE',  ( 6.073689629242148058, 8.109057205581079231, -1.443375672974057666 ) ) ;
#9150 = CARTESIAN_POINT ( 'NONE',  ( -8.473482818416670170, 10.90881592628469932, -1.443375672974058777 ) ) ;
#9151 = CARTESIAN_POINT ( 'NONE',  ( 6.699137298928145690, 8.909022496873262753, 1.443375672974065660 ) ) ;
#9152 = CARTESIAN_POINT ( 'NONE',  ( 0.6334356698059575574, 0.5880228326464317368, 1.928751028484784413 ) ) ;
#9154 = CARTESIAN_POINT ( 'NONE',  ( 0.4970291366834606039, 0.3490122959711927098, 2.032667101136710563 ) ) ;
#9153 = CARTESIAN_POINT ( 'NONE',  ( 8.890396042259068210, 11.39521468743417998, -1.599625672291257406 ) ) ;
#9155 = CARTESIAN_POINT ( 'NONE',  ( -10.85353573482940881, -6.836568542494932288, 0.4635785636673760979 ) ) ;
#9156 = CARTESIAN_POINT ( 'NONE',  ( 7.485510208076452621, 7.905719128943566432, 0.000000000000000000 ) ) ;
#9157 = CARTESIAN_POINT ( 'NONE',  ( 0.000000000000000000, 0.5000000000000004441, 0.000000000000000000 ) ) ;
#9158 = CARTESIAN_POINT ( 'NONE',  ( -1.201851678989727383E-14, 0.8218750003414171390, 1.575800808251672791 ) ) ;
#9159 = CARTESIAN_POINT ( 'NONE',  ( 0.8777613430710672349, -0.9896981104785051997, 1.466914328529956180 ) ) ;
#9160 = CARTESIAN_POINT ( 'NONE',  ( 0.3346115673153668424, 0.6298721381652396811, -1.915601020889952322 ) ) ;
#9161 = CARTESIAN_POINT ( 'NONE',  ( 5.319757424029775805, 1.030549729363830158, -1.402388650165889095 ) ) ;
#9162 = CARTESIAN_POINT ( 'NONE',  ( 4.441175045773351648, -1.771670475836329306, -1.454733398674179945 ) ) ;
#9163 = CARTESIAN_POINT ( 'NONE',  ( -0.6823417656250246877, -0.6989583329919113464, 1.181850606188755259 ) ) ;
#9164 = CARTESIAN_POINT ( 'NONE',  ( 1.904012794591736668, 1.364881752761820222, -1.235849761865935870 ) ) ;
#9165 = CARTESIAN_POINT ( 'NONE',  ( 10.55910270694468345, 11.21337466772398095, 0.7998128361456462443 ) ) ;
#9166 = CARTESIAN_POINT ( 'NONE',  ( 9.086253353280449474, 13.40000000000000036, 7.838367176906169576 ) ) ;
#9167 = CARTESIAN_POINT ( 'NONE',  ( 2.801551268311212262, -0.5745519774189576934, 1.732868645247707562 ) ) ;
#9168 = CARTESIAN_POINT ( 'NONE',  ( 4.096327398540238640, -0.3419367296172080017, 1.987046374476949095 ) ) ;
#9169 = CARTESIAN_POINT ( 'NONE',  ( -8.371269781434001800, 11.85389961405997816, -1.199719254218446718 ) ) ;
#9171 = CARTESIAN_POINT ( 'NONE',  ( 0.07680821025393690105, 0.005952109439256307241, -1.810863387344714193 ) ) ;
#9170 = CARTESIAN_POINT ( 'NONE',  ( 1.780510834742056847, -1.209543565243664798, 1.911899112700167880 ) ) ;
#9172 = CARTESIAN_POINT ( 'NONE',  ( 5.983450976520548359, 1.947180606154915727, -0.8027177699698545554 ) ) ;
#9173 = CARTESIAN_POINT ( 'NONE',  ( 8.788338075491303414, 15.71983230968314871, 9.216794715973650298 ) ) ;
#9174 = CARTESIAN_POINT ( 'NONE',  ( 2.277862540309500083, -2.008769142935047380, 0.5008063122204224893 ) ) ;
#9175 = CARTESIAN_POINT ( 'NONE',  ( 4.891794496432329886, 4.601515088792824670, -0.7998128361456211532 ) ) ;
#9176 = CARTESIAN_POINT ( 'NONE',  ( -0.6801582343750334214, 0.3802083336747336118, -1.178068619123869398 ) ) ;
#9177 = CARTESIAN_POINT ( 'NONE',  ( 4.389387035479824561, -0.001039498178659337352, -2.120667954306009406 ) ) ;
#9179 = AXIS2_PLACEMENT_3D ( 'NONE', #210281, #64048, #29426 ) ;
#9178 = ITEM_DEFINED_TRANSFORMATION ( 'NONE', 'NONE', #100542,  #200407 ) ;
#9180 = B_SPLINE_CURVE_WITH_KNOTS ( 'NONE', 3,
 ( #116797, #165484, #67950, #813, #1890, #66881, #86378, #133025, #33348, #17081 ),
 .UNSPECIFIED., .F., .F.,
 ( 4, 2, 2, 2, 4 ),
 ( 0.000000000000000000, 0.0005402298572614764672, 0.001080459714522952934, 0.001620689571784429510, 0.002160919429045905869 ),
 .UNSPECIFIED. ) ;
#9182 = CARTESIAN_POINT ( 'NONE',  ( 1.260239703848411441, 0.7801416839768731126, 1.761649912542123664 ) ) ;
#9181 = CARTESIAN_POINT ( 'NONE',  ( -4.134873662043608178, 4.886736029548026217, 1.082531754730558626 ) ) ;
#9183 = CARTESIAN_POINT ( 'NONE',  ( -5.354544322754380303, 5.211666229493680191, 0.7998128361456281477 ) ) ;
#9184 = CARTESIAN_POINT ( 'NONE',  ( 9.935427640716063991, 10.48575375712389679, -0.7998128361456281477 ) ) ;
#9185 = CARTESIAN_POINT ( 'NONE',  ( 5.682275777458846377, 7.722684055159064975, 1.443375672974064550 ) ) ;
#9186 = CARTESIAN_POINT ( 'NONE',  ( 4.285325189395043033, 7.238007417033815116, 0.9681492361576886641 ) ) ;
#9187 = CARTESIAN_POINT ( 'NONE',  ( 0.000000000000000000, -0.3937499990440834763, -4.012584370867899430 ) ) ;
#9188 = CARTESIAN_POINT ( 'NONE',  ( -5.413783410558481002, 5.210502155273325720, -0.7998128361456221525 ) ) ;
#9189 = CARTESIAN_POINT ( 'NONE',  ( 5.906510592826289319, -2.110524776404258507, -0.2060971850248518311 ) ) ;
#9190 = CARTESIAN_POINT ( 'NONE',  ( 2.344876439239967247, 0.4604487725310001389, 2.054841016598129233 ) ) ;
#9191 = CARTESIAN_POINT ( 'NONE',  ( -5.666381855868691808, 5.575476684793721383, 0.000000000000000000 ) ) ;
#9192 = CARTESIAN_POINT ( 'NONE',  ( 6.428537391173986038, 10.65171072301167854, 0.7998128361456462443 ) ) ;
#9193 = CARTESIAN_POINT ( 'NONE',  ( 6.702007135557183304, 0.7127468228822000373, -1.719244972783180225 ) ) ;
#9194 = CARTESIAN_POINT ( 'NONE',  ( 7.775764792637399836, 9.030479331953833011, -1.199719254218441611 ) ) ;
#9195 = CARTESIAN_POINT ( 'NONE',  ( 1.499999999999959588, 6.999999999999999112, -10.89724735885168805 ) ) ;
#9196 = CARTESIAN_POINT ( 'NONE',  ( -5.093022980588950865, 5.970890227889075419, -1.199719254218453823 ) ) ;
#9197 = CARTESIAN_POINT ( 'NONE',  ( -8.188761592974040937, 11.53701037756964887, -1.082531754730543971 ) ) ;
#9198 = CARTESIAN_POINT ( 'NONE',  ( 0.3871773095200456982, -1.998849835692744659, -0.7086421328065874992 ) ) ;
#9199 = FACE_OUTER_BOUND ( 'NONE', #151864, .T. ) ;
#9201 = CARTESIAN_POINT ( 'NONE',  ( 3.701569118832209515, -1.483977648892897960, -1.283320388228793130 ) ) ;
#9200 = CARTESIAN_POINT ( 'NONE',  ( -1.225000000000038058, -0.7291666666666354324, 0.7072540797572717253 ) ) ;
#9202 = CARTESIAN_POINT ( 'NONE',  ( 1.938557520917514987, 2.138169252768943984, 0.3173444169591658204 ) ) ;
#9204 = CARTESIAN_POINT ( 'NONE',  ( -5.077710034904439951, 6.555083676148210081, -1.223860624452234980 ) ) ;
#9203 = CARTESIAN_POINT ( 'NONE',  ( -5.469788628470539926, 5.346117919495872783, -0.7998128361456362523 ) ) ;
#9205 = CARTESIAN_POINT ( 'NONE',  ( -1.402160292154681736E-14, 1.446875000341420137, -1.575800808251659024 ) ) ;
#9206 = CARTESIAN_POINT ( 'NONE',  ( 3.046520963529773862, -1.423092868940859956, -1.001465238821471315 ) ) ;
#9207 = CARTESIAN_POINT ( 'NONE',  ( 6.100805936469477331, 9.101062111647635788, -1.082531754730537088 ) ) ;
#9208 = CARTESIAN_POINT ( 'NONE',  ( -12.36781821011106963, 9.649948393628900334, 1.413879826568002152 ) ) ;
#9209 = EDGE_CURVE ( 'NONE', #142998, #75662, #83746, .T. ) ;
#9210 = CIRCLE ( 'NONE', #175283, 11.95586206896552284 ) ;
#9211 = CARTESIAN_POINT ( 'NONE',  ( 1.880232294074701604, -0.2495702131940503166, 2.000550610736757218 ) ) ;
#9212 = CARTESIAN_POINT ( 'NONE',  ( -0.08058608058609216529, -9.902238891812018551, -10.99970480893080271 ) ) ;
#9213 = CARTESIAN_POINT ( 'NONE',  ( -2.986538976760251263, 6.706322249520737522, -0.7998128361456481317 ) ) ;
#9214 = CARTESIAN_POINT ( 'NONE',  ( 2.588696453722662660, -0.3354253448964693574, -1.942569732146891770 ) ) ;
#9216 = CARTESIAN_POINT ( 'NONE',  ( -4.163762573172648196, 7.871823745427799501, 0.000000000000000000 ) ) ;
#9215 = CARTESIAN_POINT ( 'NONE',  ( 5.713130151434068438, 1.559639147136464343, -1.106415316399149473 ) ) ;
#9217 = CARTESIAN_POINT ( 'NONE',  ( -5.058600711230246461, 7.955432358860325515, 1.082531754730549967 ) ) ;
#9218 = CARTESIAN_POINT ( 'NONE',  ( 5.040599249230596435, 9.102725900736217568, 0.7998128361456341429 ) ) ;
#9219 = CARTESIAN_POINT ( 'NONE',  ( -6.954406449166956605, 7.078172043641714595, -0.7998128361456362523 ) ) ;
#9220 = CARTESIAN_POINT ( 'NONE',  ( 2.455728411619819251, -1.498007593246965419, -1.354850333784217709 ) ) ;
#9221 = CARTESIAN_POINT ( 'NONE',  ( -10.15469386651127515, 11.90985960142705657, 1.082531754730558626 ) ) ;
#9222 = CARTESIAN_POINT ( 'NONE',  ( 5.667085135620930636, -2.082984650255703230, -0.9933455750401504192 ) ) ;
#9223 = CARTESIAN_POINT ( 'NONE',  ( 6.637165056451467038, -0.09505199798197358496, -1.959668910398344233 ) ) ;
#9224 = EDGE_CURVE ( 'NONE', #208182, #71097, #179294, .T. ) ;
#9225 = CARTESIAN_POINT ( 'NONE',  ( 3.450005804356533812, -0.7992637590314204399, 1.791754569076028147 ) ) ;
#9226 = CARTESIAN_POINT ( 'NONE',  ( 8.772289083241844310, 10.19309100432570148, -1.199719254218446718 ) ) ;
#9227 = CARTESIAN_POINT ( 'NONE',  ( 0.5982800022500452952, -0.2930678230431381648, 1.994870242743536304 ) ) ;
#9228 = ORIENTED_EDGE ( 'NONE', *, *, #160649, .T. ) ;
#9229 = CARTESIAN_POINT ( 'NONE',  ( 2.220046512049120846, 0.9935532346000598425, -1.869724544471425665 ) ) ;
#9231 = CARTESIAN_POINT ( 'NONE',  ( -5.845536785786364931, 9.971543350059432598, 0.000000000000000000 ) ) ;
#9230 = CARTESIAN_POINT ( 'NONE',  ( -4.647747731386360215, 4.316793862905830892, 0.7998128361456341429 ) ) ;
#9232 = CARTESIAN_POINT ( 'NONE',  ( 2.431387202150553151, 0.8680758514147070004, -1.623638265414374171 ) ) ;
#9233 = ORIENTED_EDGE ( 'NONE', *, *, #114075, .F. ) ;
#9234 = CARTESIAN_POINT ( 'NONE',  ( -9.001723924469462901, 12.58942944760136484, -1.199719254218446718 ) ) ;
#9235 = CARTESIAN_POINT ( 'NONE',  ( 10.65509502169168776, 9.862988198964483644, 5.421291348111367370 ) ) ;
#9236 = CARTESIAN_POINT ( 'NONE',  ( 3.392942708002244068, -2.044739723715986113, -0.5619712599038150236 ) ) ;
#9237 = CARTESIAN_POINT ( 'NONE',  ( -0.7500000000000215383, 4.222916667349481123, 1.299038105676671107 ) ) ;
#9238 = CARTESIAN_POINT ( 'NONE',  ( 8.101160479365381306, 9.410107633136481908, -1.199719254218446718 ) ) ;
#9239 = CARTESIAN_POINT ( 'NONE',  ( 5.501576472095266901, 9.640532660744973725, -0.7998128361456481317 ) ) ;
#9240 = CARTESIAN_POINT ( 'NONE',  ( 3.989569841107299286, 1.489977244407629131, 1.423887585670815747 ) ) ;
#9242 = CARTESIAN_POINT ( 'NONE',  ( 1.469984750362408388, -1.748608032326857353, -0.5769476384821782267 ) ) ;
#9241 = CARTESIAN_POINT ( 'NONE',  ( -7.690499447449645309, 9.995335326823163058, 1.599625672291295375 ) ) ;
#9243 = CARTESIAN_POINT ( 'NONE',  ( -0.6823417656249969321, 4.467708333674755394, -1.181850606188749264 ) ) ;
#9244 = CARTESIAN_POINT ( 'NONE',  ( -0.02224634325197898804, 1.983040877609225872, -2.702260234736663325 ) ) ;
#9245 = CARTESIAN_POINT ( 'NONE',  ( -1.495221130952461897, 8.717880658893493617, 2.557745341056316679 ) ) ;
#9246 = CARTESIAN_POINT ( 'NONE',  ( 11.04536101718726115, 13.50457272964008482, 1.099999999999998979 ) ) ;
#9247 = CIRCLE ( 'NONE', #151046, 0.08000000000000041800 ) ;
#9248 = CARTESIAN_POINT ( 'NONE',  ( 1.032169062358662348, -1.402649970393770484, -1.703791656331831605 ) ) ;
#9249 = CARTESIAN_POINT ( 'NONE',  ( 2.372703478119597698, -1.393307465234068898, 1.782356930206913770 ) ) ;
#9250 = CARTESIAN_POINT ( 'NONE',  ( -7.049876689426097798, 11.16868053773170821, -0.7216878364870267237 ) ) ;
#9251 = CARTESIAN_POINT ( 'NONE',  ( 4.007922362044618048, -0.6876924770315288038, 1.676191166192544157 ) ) ;
#9252 = CARTESIAN_POINT ( 'NONE',  ( 3.221808243886138179, 0.8566008913209141040, -1.713579649959365403 ) ) ;
#9253 = CARTESIAN_POINT ( 'NONE',  ( 4.123533666479628046, 0.2564666318346648377, -2.054367117340555549 ) ) ;
#9254 = CARTESIAN_POINT ( 'NONE',  ( -1.364683531250012516, 2.842708333674754506, 0.7879004041258379498 ) ) ;
#9255 = AXIS2_PLACEMENT_3D ( 'NONE', #116887, #182886, #34503 ) ;
#9256 = CARTESIAN_POINT ( 'NONE',  ( 3.291827724629258434, -0.8003651471039547882, 1.801871540228771273 ) ) ;
#9257 = CARTESIAN_POINT ( 'NONE',  ( 0.5340448022827409824, 0.9932739084477918423, -1.650449964952714454 ) ) ;
#9258 = CARTESIAN_POINT ( 'NONE',  ( 4.240975883383619305, -1.627667033997456381, 0.9218181776217827528 ) ) ;
#9259 = CARTESIAN_POINT ( 'NONE',  ( 2.807580367715529324, 1.950013211217585196, 1.233794411958085036 ) ) ;
#9260 = CARTESIAN_POINT ( 'NONE',  ( 3.455356687279837136, 1.465577529964179115, 1.146850193174092203 ) ) ;
#9261 = CARTESIAN_POINT ( 'NONE',  ( 1.364683531249990311, 4.384375000341417028, 1.214306433183764966E-14 ) ) ;
#9262 = CARTESIAN_POINT ( 'NONE',  ( -4.355193658487827690, 6.104145239700998538, -1.599625672291256295 ) ) ;
#9263 = CARTESIAN_POINT ( 'NONE',  ( 6.799577732453452761, 7.891594428405881878, -1.199719254218446718 ) ) ;
#9264 = DIRECTION ( 'NONE',  ( -1.000000000000000000, -2.168404344971003504E-14, 0.000000000000000000 ) ) ;
#9265 = CARTESIAN_POINT ( 'NONE',  ( 1.119907265981748168, -2.054334215221398807, 0.4631877017708794231 ) ) ;
#9267 = CARTESIAN_POINT ( 'NONE',  ( 5.076871660599175051, 4.912164349150736520, 0.2100609765546117280 ) ) ;
#9266 = CARTESIAN_POINT ( 'NONE',  ( -0.6823417656250212460, 4.363541667008085767, 1.181850606188767472 ) ) ;
#9268 = CARTESIAN_POINT ( 'NONE',  ( 1.346456596051760490, 4.237728335763024212, -0.3357819570988694324 ) ) ;
#9269 = CARTESIAN_POINT ( 'NONE',  ( 2.355864820516640812, -1.574449018071517825, -1.420800595792824028 ) ) ;
#9270 = CARTESIAN_POINT ( 'NONE',  ( 6.235022398275627431, 1.885252722396244085, 0.7250032809389771460 ) ) ;
#9271 = CARTESIAN_POINT ( 'NONE',  ( -1.402160292154681736E-14, -0.4281249996585808071, 1.575800808251672791 ) ) ;
#9272 = AXIS2_PLACEMENT_3D ( 'NONE', #124069, #91501, #54704 ) ;
#9273 = CARTESIAN_POINT ( 'NONE',  ( -4.067082894419624672, 6.728385229256075739, 1.082531754730560403 ) ) ;
#9274 = CARTESIAN_POINT ( 'NONE',  ( 3.825371897350130723, 7.614684313550482031, 0.7998128361456321445 ) ) ;
#9275 = CARTESIAN_POINT ( 'NONE',  ( 1.370646902836635261, -1.372427557409527488, 1.669970663979184256 ) ) ;
#9276 = ADVANCED_FACE ( 'NONE', ( #31587 ), #175178, .T. ) ;
#9279 = CARTESIAN_POINT ( 'NONE',  ( 3.470524135418292300, 5.072030796119872953, -1.443375672974057666 ) ) ;
#9278 = CARTESIAN_POINT ( 'NONE',  ( 6.925078400183523719, 3.697131557392329348, 2.469975972695995559 ) ) ;
#9277 = CARTESIAN_POINT ( 'NONE',  ( 5.794130544993763898, 7.853181283949808744, 1.599625672291269396 ) ) ;
#9280 = CARTESIAN_POINT ( 'NONE',  ( -3.923105346307911745, 5.670318552149568703, -1.599625672291283607 ) ) ;
#9281 = CARTESIAN_POINT ( 'NONE',  ( 4.751185534883737738, 0.1928377863454934504, -2.007255887737584121 ) ) ;
#9283 = CARTESIAN_POINT ( 'NONE',  ( -4.787437638956920871, 8.599444655509458357, -0.7216878364870338292 ) ) ;
#9282 = CARTESIAN_POINT ( 'NONE',  ( -8.337901282724359930, 12.67137589657970409, 1.040834085586084257E-14 ) ) ;
#9284 = FILL_AREA_STYLE ('',( #106842 ) ) ;
#9286 = CARTESIAN_POINT ( 'NONE',  ( -1.364683531250000748, 10.10937500034139802, 0.000000000000000000 ) ) ;
#9285 = CARTESIAN_POINT ( 'NONE',  ( 0.4622851218389683603, 2.237382594954186565, -0.3354954470186234383 ) ) ;
#9287 = CARTESIAN_POINT ( 'NONE',  ( -10.63367255181986160, 11.30037282007833532, 1.040834085586084257E-14 ) ) ;
#9289 = CARTESIAN_POINT ( 'NONE',  ( 0.4213150654816185114, -1.355317750890722595, -1.354022888547769421 ) ) ;
#9288 = CARTESIAN_POINT ( 'NONE',  ( -6.087247782411500552, 7.164505836643929371, 1.082531754730549967 ) ) ;
#9290 = CARTESIAN_POINT ( 'NONE',  ( 1.364683531249988535, 1.426041667008083991, 0.7879004041258500513 ) ) ;
#9291 = LINE ( 'NONE', #50065, #127123 ) ;
#9292 = CARTESIAN_POINT ( 'NONE',  ( 1.500000000000001332, 8.625000000000000000, 0.000000000000000000 ) ) ;
#9293 = CARTESIAN_POINT ( 'NONE',  ( 2.929983995618768322, 0.9579465210916816575, -1.434183166407378307 ) ) ;
#9294 = CARTESIAN_POINT ( 'NONE',  ( 5.246079093845007257, 5.085123462432798114, 0.7998128361456352531 ) ) ;
#9295 = CARTESIAN_POINT ( 'NONE',  ( 4.518610335104485287, 8.493738834255713854, 0.000000000000000000 ) ) ;
#9296 = CARTESIAN_POINT ( 'NONE',  ( 1.457869587114325460, 0.7109265171535653627, 1.620852848218183873 ) ) ;
#9297 = CARTESIAN_POINT ( 'NONE',  ( 1.963540897105001459, -1.618223010570983611, -1.197281337589267247 ) ) ;
#9298 = CARTESIAN_POINT ( 'NONE',  ( 8.669853050660773164, 2.974000657017433102, 7.806370750281344861 ) ) ;
#9299 = CARTESIAN_POINT ( 'NONE',  ( 4.647634198631804381, -1.703412986257560879, -1.402924735643434673 ) ) ;
#9300 = ORIENTED_EDGE ( 'NONE', *, *, #159807, .T. ) ;
#9301 = CARTESIAN_POINT ( 'NONE',  ( 4.004454267989866700, 5.765225627445230927, 1.599625672291262513 ) ) ;
#9302 = CARTESIAN_POINT ( 'NONE',  ( 7.551528372687370094, 11.75394083486988528, -0.7216878364870267237 ) ) ;
#9304 = CARTESIAN_POINT ( 'NONE',  ( 2.671500097371417137, 1.427951006967288272, 1.423949442620517480 ) ) ;
#9303 = CARTESIAN_POINT ( 'NONE',  ( 4.090573159264241809, -1.219870178150096462, 1.734285844867427651 ) ) ;
#9306 = ORIENTED_EDGE ( 'NONE', *, *, #154040, .F. ) ;
#9305 = CARTESIAN_POINT ( 'NONE',  ( 3.480526544955347301, -1.212856340575025005, 1.345865543471187253 ) ) ;
#9307 = CARTESIAN_POINT ( 'NONE',  ( 5.357406976055401948, 6.279338222599979424, 1.199719254218452935 ) ) ;
#9308 = EDGE_LOOP ( 'NONE', ( #171057, #177648 ) ) ;
#9309 = CARTESIAN_POINT ( 'NONE',  ( 0.4791068267422092797, 1.747065859276742072, -0.6691465683838908607 ) ) ;
#9310 = CARTESIAN_POINT ( 'NONE',  ( 2.869522067586683711, 6.499526178826442013, 0.7998128361456362523 ) ) ;
#9311 = CARTESIAN_POINT ( 'NONE',  ( 6.076747101522134820, -1.735163100867884500, -0.5679748894881069265 ) ) ;
#9313 = CARTESIAN_POINT ( 'NONE',  ( 2.852642732684606663, -1.771934378248109399, -0.7286688389312511172 ) ) ;
#9312 = CARTESIAN_POINT ( 'NONE',  ( -2.578021764892882040, 6.159442492350315490, 0.7998128361456341429 ) ) ;
#9314 = CARTESIAN_POINT ( 'NONE',  ( 1.150196859685076012, 3.185958678954800227, 0.7750000000000135669 ) ) ;
#9315 = CARTESIAN_POINT ( 'NONE',  ( -1.500000000000001110, 8.552083334016133520, 0.8660254037844418162 ) ) ;
#9316 = CARTESIAN_POINT ( 'NONE',  ( -1.364683531250012516, 1.092708333674754506, 0.7879004041258379498 ) ) ;
#9317 = VERTEX_POINT ( 'NONE', #118900 ) ;
#9318 = EDGE_CURVE ( 'NONE', #14390, #90767, #24263, .T. ) ;
#9319 = CARTESIAN_POINT ( 'NONE',  ( 6.373741612200160667, 9.489763409991955001, 1.082531754730549078 ) ) ;
#9320 = CARTESIAN_POINT ( 'NONE',  ( -4.014622883422336308, 5.777089012116397804, -1.443375672974066548 ) ) ;
#9321 = CARTESIAN_POINT ( 'NONE',  ( -5.803772275101700906, 8.928762199997411386, -1.199719254218452047 ) ) ;
#9322 = CARTESIAN_POINT ( 'NONE',  ( 3.463236921083117537, -1.731491641549892213, 1.224000437801610941 ) ) ;
#9324 = CARTESIAN_POINT ( 'NONE',  ( -10.99318506637795956, 6.209869560752310669, 6.173358988436974393 ) ) ;
#9323 = CARTESIAN_POINT ( 'NONE',  ( -0.1294898018152357000, 1.363479816416721446, -2.179679775322340696 ) ) ;
#9325 = CARTESIAN_POINT ( 'NONE',  ( 4.868415619454742327, -1.289772430030609707, 1.490937899079747497 ) ) ;
#9326 =( BOUNDED_CURVE ( )  B_SPLINE_CURVE ( 2, ( #61882, #147407, #146360, #179903, #211315, #78123, #80261 ),
 .UNSPECIFIED., .F., .T. ) 
 B_SPLINE_CURVE_WITH_KNOTS ( ( 3, 2, 2, 3 ),
 ( 0.2125000000000000222, 0.2166666666666667573, 0.2208333333333334647, 0.2250000000000001998 ),
 .UNSPECIFIED. ) 
 CURVE ( )  GEOMETRIC_REPRESENTATION_ITEM ( )  RATIONAL_B_SPLINE_CURVE ( ( 0.9999999999999991118, 0.8660254037844395958, 1.000000000000000000, 0.8660254037844387076, 1.000000000000000000, 0.8660254037844324904, 1.000000000000006217 ) ) 
 REPRESENTATION_ITEM ( '' )  );
#9327 = CARTESIAN_POINT ( 'NONE',  ( -0.03490996608559569087, -1.614503017106348581, 1.202435150695363664 ) ) ;
#9328 = ORIENTED_EDGE ( 'NONE', *, *, #198303, .F. ) ;
#9329 = AXIS2_PLACEMENT_3D ( 'NONE', #5948, #104562, #101340 ) ;
#9330 = CARTESIAN_POINT ( 'NONE',  ( 6.280470216940358341, -0.5666190470481970998, -2.040018813895160044 ) ) ;
#9331 = EDGE_CURVE ( 'NONE', #83117, #147564, #190323, .T. ) ;
#9332 = CARTESIAN_POINT ( 'NONE',  ( 1.557173632797459684, 1.693725193156172315, -1.190412882225246438 ) ) ;
#9333 = CARTESIAN_POINT ( 'NONE',  ( 2.185399619353834311, -0.8303394849570409075, 1.755606585091240568 ) ) ;
#9334 = CARTESIAN_POINT ( 'NONE',  ( 4.505052181490820651, 8.477920988373101707, -0.7998128361456381397 ) ) ;
#9335 = CARTESIAN_POINT ( 'NONE',  ( 5.525830126021535449, 8.604496359403894346, -1.199719254218452047 ) ) ;
#9337 = CARTESIAN_POINT ( 'NONE',  ( 6.993308306550549247, 7.053281200597435685, 1.040834085586084257E-14 ) ) ;
#9336 = CARTESIAN_POINT ( 'NONE',  ( 3.292999148915674468, 1.648261854606505983, 1.285964787075925431 ) ) ;
#9338 = CARTESIAN_POINT ( 'NONE',  ( 3.065552130021340194, 6.590578228417936835, 0.000000000000000000 ) ) ;
#9340 = ORIENTED_EDGE ( 'NONE', *, *, #45325, .T. ) ;
#9339 = CARTESIAN_POINT ( 'NONE',  ( 0.9436867518335406713, -1.148578278726499757, -1.400746029399003501 ) ) ;
#9341 = CARTESIAN_POINT ( 'NONE',  ( 5.444034239667132624, 0.8972360612293399651, -2.016436982482258333 ) ) ;
#9342 = CARTESIAN_POINT ( 'NONE',  ( -0.4635785636673774857, -6.836568542494932288, -10.85353573482939460 ) ) ;
#9343 = CARTESIAN_POINT ( 'NONE',  ( 4.594872931952145301, -0.4798491958124780910, -2.153818993410236970 ) ) ;
#9344 = CARTESIAN_POINT ( 'NONE',  ( 8.118635056484817980, 8.366162408854107113, 0.7998128361456481317 ) ) ;
#9346 =( BOUNDED_SURFACE ( )  B_SPLINE_SURFACE ( 3, 2, ( 
 ( #194969, #212265, #161421 ),
 ( #144142, #159268, #210134 ),
 ( #62830, #10868, #131102 ),
 ( #197091, #78017, #63899 ),
 ( #163545, #45544, #110594 ),
 ( #13004, #30350, #61777 ) ),
 .UNSPECIFIED., .F., .F., .F. ) 
 B_SPLINE_SURFACE_WITH_KNOTS ( ( 4, 2, 4 ),
 ( 3, 3 ),
 ( 0.000000000000000000, 0.0003831327362561333209, 0.0007662654725122666419 ),
 ( 0.000000000000000000, 1.000000000000000000 ),
 .UNSPECIFIED. ) 
 GEOMETRIC_REPRESENTATION_ITEM ( )  RATIONAL_B_SPLINE_SURFACE ( (
 ( 1.000000000000000000, 0.5879095031487548972, 1.000000000000000000),
 ( 1.000000000000000000, 0.5873691247580644648, 1.000000000000000000),
 ( 1.000000000000000000, 0.6054349545494872586, 1.000000000000000000),
 ( 1.000000000000000000, 0.6533334602768978705, 1.000000000000000000),
 ( 1.000000000000000000, 0.6828746263149305662, 1.000000000000000000),
 ( 1.000000000000000000, 0.7071067811865475727, 1.000000000000000000) ) ) 
 REPRESENTATION_ITEM ( '' )  SURFACE ( )  );
#9345 = CARTESIAN_POINT ( 'NONE',  ( 0.000000000000000000, 6.999999999999999112, 0.000000000000000000 ) ) ;
#9347 = CARTESIAN_POINT ( 'NONE',  ( 2.842330330863319876, 1.060513762474508015, -1.591057744338888913 ) ) ;
#9348 = CARTESIAN_POINT ( 'NONE',  ( 8.992082194361556091, 11.51384853155376220, 1.599625672291279388 ) ) ;
#9349 = CARTESIAN_POINT ( 'NONE',  ( 5.635237798060349412, -0.04710594754482424346, -2.069988403558701062 ) ) ;
#9351 = CARTESIAN_POINT ( 'NONE',  ( 2.448304249002517974, 2.161202317112873139, 0.05382173394478938222 ) ) ;
#9350 = CARTESIAN_POINT ( 'NONE',  ( 0.000000000000000000, 0.000000000000000000, 0.000000000000000000 ) ) ;
#9352 = CARTESIAN_POINT ( 'NONE',  ( 4.845371438081495619, 0.6875289519675978900, -2.081009137124201658 ) ) ;
#9353 = ORIENTED_EDGE ( 'NONE', *, *, #105154, .F. ) ;
#9354 = CARTESIAN_POINT ( 'NONE',  ( 9.579764304849247125, -9.999999999999998224, -0.06720017513376763674 ) ) ;
#9355 = CARTESIAN_POINT ( 'NONE',  ( 4.817943484809818600, 6.714296380401858499, 1.599625672291269396 ) ) ;
#9356 = CARTESIAN_POINT ( 'NONE',  ( -0.6823417656250039265, 15.13020833367473372, -1.181850606188755259 ) ) ;
#9357 = CARTESIAN_POINT ( 'NONE',  ( 6.661184041420940005, -7.246166700180828535, -6.773376349083132908 ) ) ;
#9358 = EDGE_CURVE ( 'NONE', #125304, #179210, #165876, .T. ) ;
#9359 = CARTESIAN_POINT ( 'NONE',  ( -7.348156068926747331, 11.51667314714914347, 0.7216878364870458196 ) ) ;
#9361 = CARTESIAN_POINT ( 'NONE',  ( 6.073126464278658432, 6.050012061272033392, 0.000000000000000000 ) ) ;
#9360 = AXIS2_PLACEMENT_3D ( 'NONE', #50594, #83082, #82023 ) ;
#9362 = CARTESIAN_POINT ( 'NONE',  ( 6.157099584139436033, 1.695871835526874483, -1.187180358042688511 ) ) ;
#9363 = CARTESIAN_POINT ( 'NONE',  ( 4.652910101842601343, -1.546415465631932884, 1.148725279867918170 ) ) ;
#9364 = CARTESIAN_POINT ( 'NONE',  ( -0.1351500440973339712, -0.1486198258836557429, -1.983738523497140305 ) ) ;
#9365 = SURFACE_STYLE_USAGE ( .BOTH. , #41894 ) ;
#9366 = CARTESIAN_POINT ( 'NONE',  ( 7.180978637093494044, 8.406838493811077839, -1.199719254218452047 ) ) ;
#9367 = DIRECTION ( 'NONE',  ( -0.000000000000000000, 0.000000000000000000, -1.000000000000000000 ) ) ;
#9368 = CARTESIAN_POINT ( 'NONE',  ( 5.436368237181718577, -1.097297496841664444, 1.635214795183062675 ) ) ;
#9369 = CARTESIAN_POINT ( 'NONE',  ( 0.02373106683711476844, -1.352142385343929387, -1.725327757841053078 ) ) ;
#9370 = CARTESIAN_POINT ( 'NONE',  ( 5.232948167349782409, 0.1380416123818763163, 1.820529236867339584 ) ) ;
#9371 = CARTESIAN_POINT ( 'NONE',  ( 5.045042558060919724, 8.899983727797476263, -0.7216878364870458196 ) ) ;
#9372 = CARTESIAN_POINT ( 'NONE',  ( 2.521453382017309952, 5.885520012421409319, 0.000000000000000000 ) ) ;
#9373 = CARTESIAN_POINT ( 'NONE',  ( -6.656127069666307072, 6.730179434224282886, 0.7998128361456341429 ) ) ;
#9374 = CARTESIAN_POINT ( 'NONE',  ( 3.867818961648523235, 7.734482231890414283, 1.040834085586084257E-14 ) ) ;
#9375 = EDGE_LOOP ( 'NONE', ( #56325, #99381, #111070, #54880, #69649, #141268 ) ) ;
#9377 = CARTESIAN_POINT ( 'NONE',  ( 6.533470335063485734, -0.1341179537190802518, 1.982235210812468340 ) ) ;
#9376 = CARTESIAN_POINT ( 'NONE',  ( 3.034521004542716227, -1.622529355458858236, 0.8704296449140033198 ) ) ;
#9378 = CARTESIAN_POINT ( 'NONE',  ( 0.5975257653535933633, 1.179397575757964001, -1.972621981072789410 ) ) ;
#9379 = CARTESIAN_POINT ( 'NONE',  ( 6.912952593004609625, -1.518390278170888008, 1.241885805282373134 ) ) ;
#9380 = CARTESIAN_POINT ( 'NONE',  ( -4.855791571988752331, 8.816840600628864877, 0.7998128361456481317 ) ) ;
#9381 = CARTESIAN_POINT ( 'NONE',  ( -5.807383341681398470, 6.267539566907733395, -0.6908299548700506110 ) ) ;
#9382 = CARTESIAN_POINT ( 'NONE',  ( -3.327636637150278798, 5.969660945728899826, -1.199719254218452935 ) ) ;
#9383 = CARTESIAN_POINT ( 'NONE',  ( -5.000000000000009770, 3.850000000000006306, 6.071532165918824830E-15 ) ) ;
#9384 = CARTESIAN_POINT ( 'NONE',  ( -3.962726036944197894, 7.845207153068690431, -0.7998128361456481317 ) ) ;
#9386 = CARTESIAN_POINT ( 'NONE',  ( 1.059204734455133412, 0.3686402435371800013, -1.833797362824276078 ) ) ;
#9385 = CARTESIAN_POINT ( 'NONE',  ( 3.140259756110568734, 0.5104685904834010968, 2.027328384984484533 ) ) ;
#9387 = CARTESIAN_POINT ( 'NONE',  ( 1.458361007166041334, 1.524808354686446821, 1.319028796778199730 ) ) ;
#9388 = ORIENTED_EDGE ( 'NONE', *, *, #127726, .F. ) ;
#9389 = CARTESIAN_POINT ( 'NONE',  ( 1.364683531249990311, 3.696875000341416584, 1.214306433183764966E-14 ) ) ;
#9390 = CARTESIAN_POINT ( 'NONE',  ( 2.032363155619838935, -1.554395792557780487, 0.7831100076771575491 ) ) ;
#9391 = CARTESIAN_POINT ( 'NONE',  ( 6.159481859310094620, 6.080483678816896109, 1.040834085586084257E-14 ) ) ;
#9393 = FACE_OUTER_BOUND ( 'NONE', #101495, .T. ) ;
#9392 = DIRECTION ( 'NONE',  ( 0.000000000000000000, 1.000000000000000000, 0.000000000000000000 ) ) ;
#9394 = CARTESIAN_POINT ( 'NONE',  ( 3.281609485064349130, 1.095178418435642120, 1.332575575002497681 ) ) ;
#9395 = CARTESIAN_POINT ( 'NONE',  ( 3.245827600587628758, 2.191739723504753101, -0.002129563554123526260 ) ) ;
#9396 = CARTESIAN_POINT ( 'NONE',  ( 5.127635347277352373, -2.096377701570474539, 0.6897739467496829535 ) ) ;
#9397 = CARTESIAN_POINT ( 'NONE',  ( -10.36744940472232379, 5.031894517187950555, -7.294791872146300982 ) ) ;
#9398 = AXIS2_PLACEMENT_3D ( 'NONE', #1181, #31593, #131278 ) ;
#9399 =( BOUNDED_CURVE ( )  B_SPLINE_CURVE ( 2, ( #114988, #98683, #151706, #164739, #69342, #50995, #198285 ),
 .UNSPECIFIED., .F., .T. ) 
 B_SPLINE_CURVE_WITH_KNOTS ( ( 3, 2, 2, 3 ),
 ( 0.3750000000000000000, 0.3833333333333335258, 0.3916666666666670515, 0.4000000000000005773 ),
 .UNSPECIFIED. ) 
 CURVE ( )  GEOMETRIC_REPRESENTATION_ITEM ( )  RATIONAL_B_SPLINE_CURVE ( ( 1.000000000000000000, 0.8660254037844387076, 1.000000000000000000, 0.8660254037844387076, 1.000000000000000000, 0.8660254037844298258, 1.000000000000008882 ) ) 
 REPRESENTATION_ITEM ( '' )  );
#9400 = CARTESIAN_POINT ( 'NONE',  ( 2.694371920525945097, 1.027083080403013993, -1.912793749723267211 ) ) ;
#9401 = CARTESIAN_POINT ( 'NONE',  ( 0.9788029507734037349, -0.04229004422508231970, -1.825371421953936757 ) ) ;
#9402 = CARTESIAN_POINT ( 'NONE',  ( 3.573546900796530146, 1.536558363836796337, 1.457006447099787882 ) ) ;
#9403 = DIRECTION ( 'NONE',  ( 1.000000000000000000, -0.000000000000000000, -0.000000000000000000 ) ) ;
#9404 = ORIENTED_EDGE ( 'NONE', *, *, #80728, .T. ) ;
#9406 = CARTESIAN_POINT ( 'NONE',  ( 1.364683531249986537, 0.7177083336747527298, -0.7879004041258239610 ) ) ;
#9405 = CARTESIAN_POINT ( 'NONE',  ( 3.773197156129989516, 2.158245952819247471, -0.7729258541082913991 ) ) ;
#9407 = CARTESIAN_POINT ( 'NONE',  ( 1.224999999999995204, 0.1249999999999862332, -6.938893903907228378E-15 ) ) ;
#9408 = CARTESIAN_POINT ( 'NONE',  ( 4.192495815123822744, 5.914331089109666983, -1.599625672291255185 ) ) ;
#9409 = CIRCLE ( 'NONE', #158169, 0.07999999999999993228 ) ;
#9410 = CARTESIAN_POINT ( 'NONE',  ( 5.496814983966967993, -2.166796134289544984, -0.4884321829702345519 ) ) ;
#9411 = CARTESIAN_POINT ( 'NONE',  ( -5.260200412422200600, 8.120355666925794580, -1.082531754730544860 ) ) ;
#9412 = CARTESIAN_POINT ( 'NONE',  ( 4.717874267875568961, 4.606534188717351874, -0.7216878364870188411 ) ) ;
#9413 = CARTESIAN_POINT ( 'NONE',  ( -5.517805330637490790, 9.381263952478319013, 0.7216878364870458196 ) ) ;
#9414 = CARTESIAN_POINT ( 'NONE',  ( 0.005636871015585881439, -9.933099847254503345, 10.91969863820290421 ) ) ;
#9415 = ORIENTED_EDGE ( 'NONE', *, *, #36946, .F. ) ;
#9416 = CARTESIAN_POINT ( 'NONE',  ( 4.307267641921147749, 1.238321930042911578, -1.591317616567271775 ) ) ;
#9418 = CARTESIAN_POINT ( 'NONE',  ( 3.590735542246026313, 2.011259174285257689, 0.4565010432640480564 ) ) ;
#9417 = CARTESIAN_POINT ( 'NONE',  ( 6.368579470117202490, 8.453095353268645695, 1.599625672291281386 ) ) ;
#9419 = CARTESIAN_POINT ( 'NONE',  ( 8.005163354226054295, 8.304055099544019214, 0.000000000000000000 ) ) ;
#9420 = CARTESIAN_POINT ( 'NONE',  ( 5.989670002187236442, 10.20997511251894529, -0.7998128361456481317 ) ) ;
#9421 = CARTESIAN_POINT ( 'NONE',  ( 0.000000000000000000, -2.296874999522042327, -3.793834371823813001 ) ) ;
#9422 = CARTESIAN_POINT ( 'NONE',  ( 2.325000000000005063, -1.380506584136773637E-31, 3.455330625536333992E-31 ) ) ;
#9423 = CARTESIAN_POINT ( 'NONE',  ( 5.912113082354764515, 1.474260358680115068, -1.621598248542432064 ) ) ;
#9424 = CARTESIAN_POINT ( 'NONE',  ( 3.305314717767214638, 1.277042846462652204, -1.560500556308255238 ) ) ;
#9425 = CARTESIAN_POINT ( 'NONE',  ( 2.331387312403776946, 0.8663521307504215008, -1.624669977836174839 ) ) ;
#9426 = VECTOR ( 'NONE', #174333, 1000.000000000000000 ) ;
#9427 = CARTESIAN_POINT ( 'NONE',  ( 5.147291874682557555, 9.156924287104992288, 0.7998128361456462443 ) ) ;
#9428 = CARTESIAN_POINT ( 'NONE',  ( 6.440460073785046369, 1.806197173870389694, 0.2645596887278709453 ) ) ;
#9429 = CARTESIAN_POINT ( 'NONE',  ( 0.3526649539562948243, 0.2173941373411722999, -2.288394520000771148 ) ) ;
#9430 = CARTESIAN_POINT ( 'NONE',  ( -5.364222332501225488, 9.410009821226765325, 0.7998128361456481317 ) ) ;
#9431 = CARTESIAN_POINT ( 'NONE',  ( 6.819229412991756334, -0.1648141603832406210, 2.226593352680195537 ) ) ;
#9432 = CARTESIAN_POINT ( 'NONE',  ( 2.033940956955893498, -1.376631898319637726, -1.593950314443808969 ) ) ;
#9433 = CARTESIAN_POINT ( 'NONE',  ( -6.448838341955544173, 7.552674816150118708, 1.199719254218452047 ) ) ;
#9434 = CARTESIAN_POINT ( 'NONE',  ( 8.320953590485093088, 10.73086516036454618, 1.599625672291281386 ) ) ;
#9435 = CARTESIAN_POINT ( 'NONE',  ( 6.007671464186812749, 10.02305078494439883, 0.7216878364870317197 ) ) ;
#9436 = CARTESIAN_POINT ( 'NONE',  ( -7.365103760721662951, 9.615707025640515937, 1.599625672291295375 ) ) ;
#9437 = CYLINDRICAL_SURFACE ( 'NONE', #140955, 1.500000000000000222 ) ;
#9438 = CARTESIAN_POINT ( 'NONE',  ( 8.066738210006686671, 9.473911335505048825, 1.082531754730558626 ) ) ;
#9439 = CARTESIAN_POINT ( 'NONE',  ( 4.000033042702237474, 7.827758669039140749, -0.08873751906842038129 ) ) ;
#9440 = CARTESIAN_POINT ( 'NONE',  ( -4.843287188579803448, 6.673587691474970107, -1.599625672291256295 ) ) ;
#9441 = CARTESIAN_POINT ( 'NONE',  ( 4.412477314457364130, -2.220925182493800776, -0.05286738749475486387 ) ) ;
#9442 = CARTESIAN_POINT ( 'NONE',  ( 0.2587985324217950689, 0.8487602207661277820, 2.037339956011212649 ) ) ;
#9443 = CARTESIAN_POINT ( 'NONE',  ( -6.310394152517827315, 6.326824364217716656, 0.7998128361456281477 ) ) ;
#9444 = CARTESIAN_POINT ( 'NONE',  ( 4.123651276850781144, 7.962676922967908411, -0.7998128361456221525 ) ) ;
#9445 = CARTESIAN_POINT ( 'NONE',  ( 4.246505328441081417, -1.940195102956907336, -0.2900488188990399396 ) ) ;
#9446 = CARTESIAN_POINT ( 'NONE',  ( 8.540746701604824409, 12.05162268759261224, -1.199719254218446718 ) ) ;
#9447 = CARTESIAN_POINT ( 'NONE',  ( -5.028543871580710700, 6.592580098690584478, 1.235119876028653918 ) ) ;
#9448 = CARTESIAN_POINT ( 'NONE',  ( -3.913718639709061087, 2.801499522163740430, -0.7749999999999944711 ) ) ;
#9449 = CARTESIAN_POINT ( 'NONE',  ( 1.364683531249986537, 0.4052083336747511200, -0.7879004041258309554 ) ) ;
#9450 = CARTESIAN_POINT ( 'NONE',  ( -3.851925040058345573, 5.587274861525073355, -1.443375672974078761 ) ) ;
#9452 = ORIENTED_EDGE ( 'NONE', *, *, #128228, .T. ) ;
#9451 = CARTESIAN_POINT ( 'NONE',  ( -6.588899466561478846, 6.789396920517583922, 0.7216878364870317197 ) ) ;
#9453 = CARTESIAN_POINT ( 'NONE',  ( 3.551138032611600437, 0.3147205237276836653, 2.097014573754731881 ) ) ;
#9454 = CARTESIAN_POINT ( 'NONE',  ( -3.786470039966538970, 7.639575156594750283, 0.000000000000000000 ) ) ;
#9455 = CARTESIAN_POINT ( 'NONE',  ( 5.225516498768126183, -2.053876642077703707, 0.6744380372525200507 ) ) ;
#9456 = CARTESIAN_POINT ( 'NONE',  ( 3.895923546780861724, -0.5813109859279728120, -1.747131793041277970 ) ) ;
#9457 = CARTESIAN_POINT ( 'NONE',  ( 5.173064673083394460, 1.776168143800487043, -0.9548534231369476544 ) ) ;
#9458 = CARTESIAN_POINT ( 'NONE',  ( -5.532833371615617502, 6.236068886146576951, 0.9535701153140889730 ) ) ;
#9459 = CARTESIAN_POINT ( 'NONE',  ( 1.364683531249986537, 1.176041667008082658, 0.7879004041258500513 ) ) ;
#9460 = CARTESIAN_POINT ( 'NONE',  ( 6.714805129994689814, -0.1247508129638870145, 1.711716247594262441 ) ) ;
#9461 = CARTESIAN_POINT ( 'NONE',  ( 6.727182134110180733, 7.053024033604696541, 2.509100769544295950 ) ) ;
#9462 = CARTESIAN_POINT ( 'NONE',  ( 2.711267533052988732, 6.106969855296372707, -0.7216878364870267237 ) ) ;
#9463 = CARTESIAN_POINT ( 'NONE',  ( -1.772826578343107640, 3.949999999999974420, 0.4499999999999487188 ) ) ;
#9464 = ADVANCED_FACE ( 'NONE', ( #163329 ), #14909, .F. ) ;
#9465 = CARTESIAN_POINT ( 'NONE',  ( 3.661132068870280420, -1.905464569931826446, -1.020879743040298271 ) ) ;
#9466 = CARTESIAN_POINT ( 'NONE',  ( 5.554064478179312481, 1.779353385700060075, -0.9478964821433707444 ) ) ;
#9467 = CARTESIAN_POINT ( 'NONE',  ( -9.151390499099978371, 9.778969791812544443, 0.7216878364870438212 ) ) ;
#9468 = CARTESIAN_POINT ( 'NONE',  ( 3.274459119871219848, -1.289031633699176949, 1.735169069618908821 ) ) ;
#9469 = CARTESIAN_POINT ( 'NONE',  ( 3.567610853275906546, 1.924076846980572464, -0.4285291244595054727 ) ) ;
#9470 = FACE_OUTER_BOUND ( 'NONE', #120220, .T. ) ;
#9471 = CARTESIAN_POINT ( 'NONE',  ( 1.413547897872836856, 2.036140070965312354, 1.085889434398391584 ) ) ;
#9472 = CARTESIAN_POINT ( 'NONE',  ( 3.075518034276482293, 1.957894989606956182, -0.6432953703794060951 ) ) ;
#9473 = CARTESIAN_POINT ( 'NONE',  ( 5.144061591681034606, 0.5672955765679200679, 1.857344180792292354 ) ) ;
#9476 = ORIENTED_EDGE ( 'NONE', *, *, #200174, .F. ) ;
#9475 = CARTESIAN_POINT ( 'NONE',  ( -1.150222622689996532, 3.108395032273046255, 0.7749999999993751887 ) ) ;
#9474 = CARTESIAN_POINT ( 'NONE',  ( -8.812436658758329600, 9.383523644747281622, 1.040834085586084257E-14 ) ) ;
#9477 = CARTESIAN_POINT ( 'NONE',  ( -6.363572996767778100, 8.517530811019446091, -1.599625672291271394 ) ) ;
#9478 = DIRECTION ( 'NONE',  ( 1.000000000000000000, 0.000000000000000000, 0.000000000000000000 ) ) ;
#9480 = VERTEX_POINT ( 'NONE', #213114 ) ;
#9479 = CARTESIAN_POINT ( 'NONE',  ( -4.736594563127865420, 6.619389305106191834, -1.599625672291271394 ) ) ;
#9481 = CARTESIAN_POINT ( 'NONE',  ( -7.985389288324710400, 8.418635045908049008, -0.7216878364870267237 ) ) ;
#9482 = CARTESIAN_POINT ( 'NONE',  ( 2.626236979526615389, -1.269917727785064843, -1.804575601930514139 ) ) ;
#9483 = CARTESIAN_POINT ( 'NONE',  ( 3.285556943750000514, -3.901041666188710177, 1.896917185911906500 ) ) ;
#9484 = CARTESIAN_POINT ( 'NONE',  ( 6.034033239799157400, 1.165729394902741189, 1.577711426528668692 ) ) ;
#9485 = CARTESIAN_POINT ( 'NONE',  ( 6.539320575229278454, 0.5749733277502915296, 2.156147827957733742 ) ) ;
#9486 = CARTESIAN_POINT ( 'NONE',  ( 1.499999999999990896, 4.806250000682819490, 1.214306433183764966E-14 ) ) ;
#9487 = CARTESIAN_POINT ( 'NONE',  ( -9.367496997608871112, 15.42330868759649043, 7.413898975919298806 ) ) ;
#9490 = CONICAL_SURFACE ( 'NONE', #120261, 10.99999999999999112, 0.7853981633974425058 ) ;
#9489 = CARTESIAN_POINT ( 'NONE',  ( 1.499999999999996891, 12.67708333401612819, -0.8660254037844378194 ) ) ;
#9488 = CARTESIAN_POINT ( 'NONE',  ( -6.285146472706256482, 6.979120928820362835, -0.9578508296879204575 ) ) ;
#9491 = CARTESIAN_POINT ( 'NONE',  ( 5.771403949166884040, 1.100151190403714452, 1.476150860297697154 ) ) ;
#9492 = ORIENTED_EDGE ( 'NONE', *, *, #132683, .T. ) ;
#9493 = CARTESIAN_POINT ( 'NONE',  ( 2.500915792353772815, 1.655931770628838784, -1.226644000274518476 ) ) ;
#9494 = CARTESIAN_POINT ( 'NONE',  ( -1.360316468750032870, 0.6614583336747411613, 0.7853790794158620470 ) ) ;
#9495 = CARTESIAN_POINT ( 'NONE',  ( -6.938021921891187382, 9.117444880338284818, -1.599625672291263179 ) ) ;
#9496 = CARTESIAN_POINT ( 'NONE',  ( 10.91838098853855321, -9.962496060591742975, -0.1694417511252848119 ) ) ;
#9497 = CARTESIAN_POINT ( 'NONE',  ( 11.97178994924802353, 11.37999993797205178, 0.8322011300497306197 ) ) ;
#9498 = CARTESIAN_POINT ( 'NONE',  ( 9.006795113616758996, 12.35945717444475278, -7.859917408111167347 ) ) ;
#9499 = CARTESIAN_POINT ( 'NONE',  ( 4.473300617505036492, 7.306268922809479704, -1.199719254218452047 ) ) ;
#9500 = CARTESIAN_POINT ( 'NONE',  ( 1.129840139894950246, -1.306895429219852467, -1.593522927358894004 ) ) ;
#9503 = CARTESIAN_POINT ( 'NONE',  ( 4.370544011308346910, -0.004580445953385886559, -1.841430844414258861 ) ) ;
#9502 = CARTESIAN_POINT ( 'NONE',  ( 2.031498134000471190, 1.782053568523461751, -0.5365169527500669444 ) ) ;
#9501 = DIRECTION ( 'NONE',  ( 0.000000000000000000, 0.000000000000000000, -1.000000000000000000 ) ) ;
#9504 = CARTESIAN_POINT ( 'NONE',  ( 8.308449207076147758, 8.587612251210650527, -0.7998128361456281477 ) ) ;
#9505 = DIRECTION ( 'NONE',  ( 0.7613463080411785322, -0.000000000000000000, 0.6483454320283801309 ) ) ;
#9506 = CARTESIAN_POINT ( 'NONE',  ( -5.794130544993808307, 7.853181283949808744, 1.599625672291263179 ) ) ;
#9508 = ORIENTED_EDGE ( 'NONE', *, *, #119125, .T. ) ;
#9507 = CARTESIAN_POINT ( 'NONE',  ( -11.24798771954519871, -6.442483420751891288, 0.4630894006630780213 ) ) ;
#9509 = CARTESIAN_POINT ( 'NONE',  ( 4.143358556170802842, -1.920740624720223666, 1.086653567583625746 ) ) ;
#9510 = CARTESIAN_POINT ( 'NONE',  ( 0.7378453340087381962, -1.528073262844112268, -1.529135702860604074 ) ) ;
#9511 = CARTESIAN_POINT ( 'NONE',  ( -6.588899466561478846, 6.789396920517583922, 0.7216878364870317197 ) ) ;
#9512 = CARTESIAN_POINT ( 'NONE',  ( -0.1757481403069499348, -0.8193859263425256056, -1.726394157293544840 ) ) ;
#9513 = CARTESIAN_POINT ( 'NONE',  ( -0.1003747550864658999, -1.976661868047492998, 0.3981153667176607902 ) ) ;
#9514 = LINE ( 'NONE', #210899, #29991 ) ;
#9515 = DIRECTION ( 'NONE',  ( 5.551115123125764829E-17, 0.000000000000000000, -1.000000000000000000 ) ) ;
#9516 = CARTESIAN_POINT ( 'NONE',  ( 5.285773936917006921, 1.841837585529454202, -0.5139651673399318055 ) ) ;
#9517 = CARTESIAN_POINT ( 'NONE',  ( 1.234984068473435892, -1.692697435815498919, 0.7966027930108383615 ) ) ;
#9518 = MECHANICAL_DESIGN_GEOMETRIC_PRESENTATION_REPRESENTATION (  '', ( #33791 ), #2672 ) ;
#9519 = CARTESIAN_POINT ( 'NONE',  ( 2.272673044126482189, -0.3494851828299732621, -1.985868527484459634 ) ) ;
#9521 = CARTESIAN_POINT ( 'NONE',  ( 3.756553094297815143, 0.7580258897690328457, 1.965105124105433809 ) ) ;
#9520 = CARTESIAN_POINT ( 'NONE',  ( -9.027031348600448979, 9.425958082989001952, 1.040834085586084257E-14 ) ) ;
#9522 = CARTESIAN_POINT ( 'NONE',  ( 8.932124273304774320, 9.315233161810734686, 0.7998128361456462443 ) ) ;
#9524 = CARTESIAN_POINT ( 'NONE',  ( -6.991200766141138168, 11.30815132714001159, 0.7998128361456481317 ) ) ;
#9523 = CARTESIAN_POINT ( 'NONE',  ( -1.402160292154681736E-14, -0.2874999999999741096, 1.732050807568877637 ) ) ;
#9525 = CARTESIAN_POINT ( 'NONE',  ( -15.75000000000000000, 9.799999999999982947, 1.799999999999999600 ) ) ;
#9526 = CARTESIAN_POINT ( 'NONE',  ( 4.095966777872499520, 1.322572826423114911, 1.526597406435834081 ) ) ;
#9527 = CARTESIAN_POINT ( 'NONE',  ( 1.364683531249988535, 4.363541667008090208, 0.7879004041258500513 ) ) ;
#9528 = CARTESIAN_POINT ( 'NONE',  ( 8.866669273657322492, 12.32790267170016207, -1.082531754730543083 ) ) ;
#9529 = CARTESIAN_POINT ( 'NONE',  ( 4.341216920475977403, -1.883070171734081200, 1.061215411333437109 ) ) ;
#9530 = DIRECTION ( 'NONE',  ( -1.000000000000000000, 7.771561172376097755E-16, 4.440892098500627148E-16 ) ) ;
#9531 = CARTESIAN_POINT ( 'NONE',  ( -1.500000000000011324, 5.629166666666693963, -0.8660254037844313801 ) ) ;
#9532 = CARTESIAN_POINT ( 'NONE',  ( 5.987861119090863049, 7.014868056141362551, 1.199719254218452047 ) ) ;
#9533 = CARTESIAN_POINT ( 'NONE',  ( 8.229436053370669413, 10.62409470039771442, 1.443375672974076540 ) ) ;
#9535 = CARTESIAN_POINT ( 'NONE',  ( -2.265491011392835929, 2.737016401661231502, -2.500000000000000444 ) ) ;
#9534 = CARTESIAN_POINT ( 'NONE',  ( 1.996751263802678533, 2.147379752972265354, 0.3199099038852480370 ) ) ;
#9537 = CARTESIAN_POINT ( 'NONE',  ( 1.135996871135702024, 0.3593859243370273182, 1.805655672011026391 ) ) ;
#9536 = CARTESIAN_POINT ( 'NONE',  ( -6.317736394288148816, 8.393778431468064127, 1.443375672974078761 ) ) ;
#9538 = CARTESIAN_POINT ( 'NONE',  ( 1.364683531249988535, 1.363541667008083769, 0.7879004041258500513 ) ) ;
#9539 = CARTESIAN_POINT ( 'NONE',  ( 3.685266855566126321, 1.588411730319793769, 1.510178839762461811 ) ) ;
#9540 = FACE_OUTER_BOUND ( 'NONE', #165967, .T. ) ;
#9541 = CARTESIAN_POINT ( 'NONE',  ( 4.188523121243816760, -2.237390873258153778, -0.3355513299154490592 ) ) ;
#9543 = CARTESIAN_POINT ( 'NONE',  ( -5.669280788808708671, 9.765911353585494226, 0.7998128361456481317 ) ) ;
#9542 = B_SPLINE_CURVE_WITH_KNOTS ( 'NONE', 3,
 ( #97006, #175048, #144706, #145774, #208567, #176109, #11446, #178242, #179309, #194473 ),
 .UNSPECIFIED., .F., .F.,
 ( 4, 3, 3, 4 ),
 ( 0.000000000000000000, 4.379906072315623141E-05, 0.0001100530589225749337, 0.0001772280998810008272 ),
 .UNSPECIFIED. ) ;
#9544 = CARTESIAN_POINT ( 'NONE',  ( 1.364683531249990311, 5.196875000341417916, 1.214306433183764966E-14 ) ) ;
#9545 = CARTESIAN_POINT ( 'NONE',  ( 5.997574213172828905, 7.082153300894140635, -1.064076030282636420 ) ) ;
#9546 = CARTESIAN_POINT ( 'NONE',  ( -1.402160292154681736E-14, 12.06250000000000000, 1.732050807568881190 ) ) ;
#9547 = CARTESIAN_POINT ( 'NONE',  ( 5.397554552016204710, 9.311247720745345902, 0.7216878364870317197 ) ) ;
#9548 = CARTESIAN_POINT ( 'NONE',  ( 4.850734264762338377, -1.421546097138610243, 1.053919008203674013 ) ) ;
#9549 = AXIS2_PLACEMENT_3D ( 'NONE', #7335, #73412, #156826 ) ;
#9550 = CARTESIAN_POINT ( 'NONE',  ( 8.235688245297327015, 11.69572115523387268, -1.199719254218446718 ) ) ;
#9551 = CARTESIAN_POINT ( 'NONE',  ( 1.149603698739794400, -1.659950780972534012, -1.295870271070469260 ) ) ;
#9553 = CARTESIAN_POINT ( 'NONE',  ( 0.7499999999999902300, 1.733333333333357595, 1.299038105676657340 ) ) ;
#9552 = CARTESIAN_POINT ( 'NONE',  ( -0.6823417656250003738, 10.40104166700806587, 1.181850606188754593 ) ) ;
#9554 = CARTESIAN_POINT ( 'NONE',  ( 0.7308274648059713829, -1.853293357156562404, -0.6670056901108140091 ) ) ;
#9555 = CARTESIAN_POINT ( 'NONE',  ( -4.176793841461789114, 7.030620694084159794, -1.199719254218455378 ) ) ;
#9556 = CARTESIAN_POINT ( 'NONE',  ( -0.3124725659140401568, 7.215207000027771045, -2.082817582596259154 ) ) ;
#9557 = EDGE_LOOP ( 'NONE', ( #101500, #18562 ) ) ;
#9558 = CARTESIAN_POINT ( 'NONE',  ( 5.992340707560141588, 9.934888558888093968, 0.7216878364870438212 ) ) ;
#9559 = AXIS2_PLACEMENT_3D ( 'NONE', #91102, #41288, #177671 ) ;
#9560 = CARTESIAN_POINT ( 'NONE',  ( 4.961713530105988923, 1.850188064717460223, -0.2750520410098392654 ) ) ;
#9561 = CARTESIAN_POINT ( 'NONE',  ( 4.434477146351770926, -1.196200190851111511, 1.689492296227592893 ) ) ;
#9562 = CARTESIAN_POINT ( 'NONE',  ( 1.224999999999947020, 2.354166666666675400, 0.7072540797573036997 ) ) ;
#9563 = CARTESIAN_POINT ( 'NONE',  ( -6.766928066552171828, 7.067373297165212342, 0.7216878364870317197 ) ) ;
#9564 = CARTESIAN_POINT ( 'NONE',  ( 2.055513515747692921, -0.9138922176956919552, -2.615695235488095349 ) ) ;
#9565 = CARTESIAN_POINT ( 'NONE',  ( 7.404724451357931336, 11.79059562655963056, 0.7998128361456462443 ) ) ;
#9566 = CARTESIAN_POINT ( 'NONE',  ( -10.47775378526269918, 11.11846759242831872, -0.7998128361456221525 ) ) ;
#9567 = DIRECTION ( 'NONE',  ( 0.000000000000000000, 0.000000000000000000, 1.000000000000000000 ) ) ;
#9568 = DIRECTION ( 'NONE',  ( 0.000000000000000000, -1.000000000000000000, 0.000000000000000000 ) ) ;
#9569 = CARTESIAN_POINT ( 'NONE',  ( 0.6823417656249882723, -1.157291666325249713, 1.181850606188755259 ) ) ;
#9570 = CARTESIAN_POINT ( 'NONE',  ( 3.894932841003693191, 0.2855096342280309396, 1.940843471192068570 ) ) ;
#9571 = CARTESIAN_POINT ( 'NONE',  ( 2.073592080879012478, 1.495823877299466087, -1.351946161731142126 ) ) ;
#9572 = CARTESIAN_POINT ( 'NONE',  ( -3.363304624641834106, 6.081549941127532222, -1.199719254218452047 ) ) ;
#9573 = CARTESIAN_POINT ( 'NONE',  ( 0.000000000000000000, 3.799999999999998046, 0.000000000000000000 ) ) ;
#9574 = CARTESIAN_POINT ( 'NONE',  ( 0.8427765623921362748, -1.607460297381148928, 0.9563107477488577146 ) ) ;
#9575 = CARTESIAN_POINT ( 'NONE',  ( -0.6823417656250212460, 4.051041667008085767, 1.181850606188767472 ) ) ;
#9576 = CARTESIAN_POINT ( 'NONE',  ( 3.463142787923169763, -1.643428793820296718, 1.162544664348450496 ) ) ;
#9578 = CARTESIAN_POINT ( 'NONE',  ( 3.216528272283057710, 2.066224784428410732, 0.4612988732951432969 ) ) ;
#9577 = CARTESIAN_POINT ( 'NONE',  ( -5.097502569058210753, 7.930541516334467467, -1.082531754730549967 ) ) ;
#9580 = EDGE_CURVE ( 'NONE', #114068, #56213, #3541, .T. ) ;
#9579 = CARTESIAN_POINT ( 'NONE',  ( -6.069210040772897052, 7.109775131437022999, -1.199719254218453823 ) ) ;
#9581 = CARTESIAN_POINT ( 'NONE',  ( 4.984861949208964305, 1.980195279717174905, 0.6042863919064264122 ) ) ;
#9582 = CARTESIAN_POINT ( 'NONE',  ( 8.154303043976348420, 8.478051404252736845, 0.7998128361456281477 ) ) ;
#9584 = CARTESIAN_POINT ( 'NONE',  ( 6.620655732516650183, 4.692022689331314389, 2.636326274693585159 ) ) ;
#9583 = CARTESIAN_POINT ( 'NONE',  ( 6.703094305332148117, -0.4564761572844484028, 2.047479069123214757 ) ) ;
#9586 = ORIENTED_EDGE ( 'NONE', *, *, #71473, .T. ) ;
#9585 = CARTESIAN_POINT ( 'NONE',  ( 5.350558509363329662, 0.5315954154057299652, 1.746479326997903092 ) ) ;
#9587 = CARTESIAN_POINT ( 'NONE',  ( 7.727257484784855635, 11.10255193463598111, -1.199719254218446718 ) ) ;
#9588 = CARTESIAN_POINT ( 'NONE',  ( 6.471393748265519719, 5.229711127717882491, -2.499999999999995115 ) ) ;
#9589 = CARTESIAN_POINT ( 'NONE',  ( 5.299301323368958094, 6.361497809228795930, -1.122821758042211959 ) ) ;
#9590 = CARTESIAN_POINT ( 'NONE',  ( -10.21581353488473987, 4.000000000000001776, 7.512123095767014647 ) ) ;
#9591 = CARTESIAN_POINT ( 'NONE',  ( 1.364683531249997417, 12.29687500034139980, 2.602085213965210642E-15 ) ) ;
#9592 = CARTESIAN_POINT ( 'NONE',  ( 6.217437059193511750, 1.592560689453832001, 1.058264445519964125 ) ) ;
#9593 = CARTESIAN_POINT ( 'NONE',  ( -8.158255747121117452, 10.54105100977322174, 1.599625672291295375 ) ) ;
#9594 = CARTESIAN_POINT ( 'NONE',  ( 7.156006149914539982, 7.243095351188763686, 1.040834085586084257E-14 ) ) ;
#9595 = FACE_OUTER_BOUND ( 'NONE', #5456, .T. ) ;
#9596 = CARTESIAN_POINT ( 'NONE',  ( -11.41381675112453387, 10.90000000000000036, -3.704697986577184299 ) ) ;
#9597 = CARTESIAN_POINT ( 'NONE',  ( 3.714044015139744914, 6.420469553383295391, 1.199719254218462483 ) ) ;
#9598 = ORIENTED_EDGE ( 'NONE', *, *, #62818, .F. ) ;
#9599 = CARTESIAN_POINT ( 'NONE',  ( -5.427006627220116286, 9.553534508390610469, -0.7998128361456362523 ) ) ;
#9600 = CARTESIAN_POINT ( 'NONE',  ( 5.150017624212761547, 0.9963180513538304472, 1.753022482293864481 ) ) ;
#9602 = CARTESIAN_POINT ( 'NONE',  ( 7.354371980770088690, 7.544798497178720531, 0.000000000000000000 ) ) ;
#9601 = CARTESIAN_POINT ( 'NONE',  ( -4.143499164831425219, 7.564990639293021957, -0.8130116771524699137 ) ) ;
#9603 = CARTESIAN_POINT ( 'NONE',  ( 0.1394461523057137220, 2.891244824116427470, -2.208899952336295325 ) ) ;
#9604 = EDGE_CURVE ( 'NONE', #110599, #80954, #96640, .T. ) ;
#9605 = CARTESIAN_POINT ( 'NONE',  ( -5.151735183512911043, 6.073074471262228435, 1.082531754730548412 ) ) ;
#9606 = CARTESIAN_POINT ( 'NONE',  ( 4.521807925357579805, 5.234196320127330715, -1.199719254218452047 ) ) ;
#9607 = CARTESIAN_POINT ( 'NONE',  ( 2.412896334679739851, -1.525488895468416706, 1.245673054583651407 ) ) ;
#9608 = CARTESIAN_POINT ( 'NONE',  ( 3.673453983005552814, 1.462458373076291673, 1.388474078538141754 ) ) ;
#9609 = CARTESIAN_POINT ( 'NONE',  ( -8.206763054973658100, 8.468978407091068306, 0.7998128361456602331 ) ) ;
#9610 = CARTESIAN_POINT ( 'NONE',  ( 6.727182134110234024, -0.002100931800118072384, 2.089081857379895268 ) ) ;
#9611 = CARTESIAN_POINT ( 'NONE',  ( 3.996163734398257894, -0.6867376513691285655, -2.081127982183433645 ) ) ;
#9612 = DIRECTION ( 'NONE',  ( 0.000000000000000000, 0.000000000000000000, 1.000000000000000000 ) ) ;
#9613 = CARTESIAN_POINT ( 'NONE',  ( 2.221590912301483645, -1.869112302256823011, 0.4658275329730912628 ) ) ;
#9614 = CARTESIAN_POINT ( 'NONE',  ( -7.808606406466886973, 11.19745900993164511, 1.199719254218453823 ) ) ;
#9615 = CARTESIAN_POINT ( 'NONE',  ( 0.1333542156527113831, 2.876250315000815405, -2.534448870308704915 ) ) ;
#9616 =( LENGTH_UNIT ( ) NAMED_UNIT ( * ) SI_UNIT ( .MILLI., .METRE. ) );
#9617 = CARTESIAN_POINT ( 'NONE',  ( 8.229962938695207342, 9.560377169021284871, 1.199719254218462483 ) ) ;
#9618 = CARTESIAN_POINT ( 'NONE',  ( 5.769158057814842699, 6.689438141327490150, 1.199719254218462483 ) ) ;
#9619 = CARTESIAN_POINT ( 'NONE',  ( -2.440293211016301606E-15, 1.187499999999993117, -1.225000000000025624 ) ) ;
#9620 = CARTESIAN_POINT ( 'NONE',  ( 5.343321937561575474, 8.287607122913563273, -1.082531754730548412 ) ) ;
#9622 = CARTESIAN_POINT ( 'NONE',  ( 2.789700014133191797, 1.910882804325767070, -0.6334545493084097201 ) ) ;
#9621 = CARTESIAN_POINT ( 'NONE',  ( 5.636236351835953506, 0.3653394402399374741, 1.804471444190151930 ) ) ;
#9623 = CARTESIAN_POINT ( 'NONE',  ( 4.517165314107184138, 2.297965829929650372, -0.05084271438157876577 ) ) ;
#9625 = CARTESIAN_POINT ( 'NONE',  ( 3.520197291191272448, 0.8326901208413343136, 1.664296038758736440 ) ) ;
#9624 = CARTESIAN_POINT ( 'NONE',  ( -0.02900071798685524560, -0.004641455105012376459, -2.173770343569726649 ) ) ;
#9626 = CARTESIAN_POINT ( 'NONE',  ( 8.174640274396848483, 8.501778173076651512, 0.7998128361456291469 ) ) ;
#9627 = DIRECTION ( 'NONE',  ( 0.000000000000000000, 1.000000000000000000, 0.000000000000000000 ) ) ;
#9628 = DIRECTION ( 'NONE',  ( 0.000000000000000000, 0.000000000000000000, -1.000000000000000000 ) ) ;
#9629 = CARTESIAN_POINT ( 'NONE',  ( -8.681298431451969222, 9.022603012982438386, 1.040834085586084257E-14 ) ) ;
#9630 = CARTESIAN_POINT ( 'NONE',  ( -4.340018570150306232, 8.077455741901736985, -0.7216878364870338292 ) ) ;
#9631 = CARTESIAN_POINT ( 'NONE',  ( 5.970280646434825478, -1.985518398909513982, -0.6551979098984096472 ) ) ;
#9632 = CARTESIAN_POINT ( 'NONE',  ( 5.450014563013511726, 8.341805509282339770, -1.082531754730543083 ) ) ;
#9633 = EDGE_LOOP ( 'NONE', ( #44582, #185136, #40205, #131913 ) ) ;
#9634 = CARTESIAN_POINT ( 'NONE',  ( -1.440240048133426987, 7.355731858844955617, 4.317885097512588644 ) ) ;
#9635 = DIRECTION ( 'NONE',  ( 0.9999580691339164940, -1.693994860858438588E-16, -0.009157509157509135383 ) ) ;
#9636 = CARTESIAN_POINT ( 'NONE',  ( 6.217413168894407427, -0.2034119912461933299, 1.712789424573582409 ) ) ;
#9637 = CARTESIAN_POINT ( 'NONE',  ( -5.168682875307782254, 7.053215992657626110, -1.599625672291256295 ) ) ;
#9638 = CARTESIAN_POINT ( 'NONE',  ( 1.318582137269165733, 0.8549262331399180015, -1.508633131004229133 ) ) ;
#9639 = DIRECTION ( 'NONE',  ( 1.276756478318932585E-15, -1.000000000000000000, 1.665334536937738262E-16 ) ) ;
#9640 = DIRECTION ( 'NONE',  ( 0.000000000000000000, -1.000000000000000000, 0.000000000000000000 ) ) ;
#9641 = VECTOR ( 'NONE', #41368, 1000.000000000000000 ) ;
#9642 = FACE_OUTER_BOUND ( 'NONE', #37583, .T. ) ;
#9643 = CARTESIAN_POINT ( 'NONE',  ( 5.700102493039955753, 0.8868678402436469543, -1.981866098488117789 ) ) ;
#9644 = CARTESIAN_POINT ( 'NONE',  ( 4.143042835627613663, -1.587387879459275286, 0.9017181768668989239 ) ) ;
#9645 = CARTESIAN_POINT ( 'NONE',  ( 2.746866186719683967, -0.3305370478365337039, -1.933541032166598894 ) ) ;
#9646 = SURFACE_SIDE_STYLE ('',( #25890 ) ) ;
#9647 = CARTESIAN_POINT ( 'NONE',  ( -8.455481356417053007, 13.01647868246193518, 0.7998128361456341429 ) ) ;
#9648 = CARTESIAN_POINT ( 'NONE',  ( 7.130698725783555680, 10.40656671580112658, 1.199719254218460707 ) ) ;
#9649 = CARTESIAN_POINT ( 'NONE',  ( 3.651137946248568689, 0.3127203024623700367, 2.097190470537732221 ) ) ;
#9650 = CARTESIAN_POINT ( 'NONE',  ( -4.311129659465605002, 4.131998812239033647, 0.7216878364870317197 ) ) ;
#9651 = CARTESIAN_POINT ( 'NONE',  ( -15.75000000000000000, 10.90000000000000036, -3.200000000000001510 ) ) ;
#9652 = CARTESIAN_POINT ( 'NONE',  ( -5.312752313518235958, 6.384578190230367767, -1.125208257168613502 ) ) ;
#9654 = CIRCLE ( 'NONE', #130808, 0.07999999999999933553 ) ;
#9653 = AXIS2_PLACEMENT_3D ( 'NONE', #148467, #183078, #34690 ) ;
#9655 = CARTESIAN_POINT ( 'NONE',  ( 0.8310238944931707117, -1.948087850137161459, -0.7009411469260096172 ) ) ;
#9657 = CARTESIAN_POINT ( 'NONE',  ( -1.500000000000015099, 15.01041666734946745, -0.8660254037844309360 ) ) ;
#9656 = CARTESIAN_POINT ( 'NONE',  ( -10.52647613395849646, 3.958815601275306406, 5.762288996714484135 ) ) ;
#9659 = VERTEX_POINT ( 'NONE', #188094 ) ;
#9658 = CARTESIAN_POINT ( 'NONE',  ( 3.422728177422405871, -0.9015832817733639981, -2.030284994954335787 ) ) ;
#9660 = CARTESIAN_POINT ( 'NONE',  ( 0.8976324851915818970, -1.040256531696292397, -2.049935236865876309 ) ) ;
#9662 = CARTESIAN_POINT ( 'NONE',  ( 6.614137777011339203, 2.057435194276434842, -0.1460075293888435377 ) ) ;
#9661 = CARTESIAN_POINT ( 'NONE',  ( 10.54788032175191326, 11.40820791823982994, 0.7216878364870317197 ) ) ;
#9664 = CARTESIAN_POINT ( 'NONE',  ( -3.285556943750000514, -3.988541666188710089, -1.896917185911906500 ) ) ;
#9663 = CARTESIAN_POINT ( 'NONE',  ( 4.472210567661338843, 6.310941310395290493, 1.599625672291261402 ) ) ;
#9665 = FACE_OUTER_BOUND ( 'NONE', #177141, .T. ) ;
#9666 = CARTESIAN_POINT ( 'NONE',  ( -11.04536101718726293, 11.00581235719507411, 1.099999999999996536 ) ) ;
#9667 = CARTESIAN_POINT ( 'NONE',  ( 3.929058411375439874, 5.999999999999998224, 0.7500000000000006661 ) ) ;
#9668 = CARTESIAN_POINT ( 'NONE',  ( -0.2106725631050020975, 7.629137130509112907, -2.603678913577145426 ) ) ;
#9669 = CARTESIAN_POINT ( 'NONE',  ( 3.522183196695947593, 1.094745356718468399, -1.332776395737497399 ) ) ;
#9670 = CARTESIAN_POINT ( 'NONE',  ( 1.411342602523329992, -1.897109289313267944, 0.6839406069230755669 ) ) ;
#9671 = CARTESIAN_POINT ( 'NONE',  ( 2.461953032136819264, -2.200924886027255667, -0.6633417334961901890 ) ) ;
#9672 = CARTESIAN_POINT ( 'NONE',  ( 3.023041696300738934, 2.129209760986842781, 0.7651156340112361676 ) ) ;
#9673 = CARTESIAN_POINT ( 'NONE',  ( 5.531892221078217098, -1.335191642697653336, -1.628727054747380887 ) ) ;
#9674 = CARTESIAN_POINT ( 'NONE',  ( -5.478903473698241378, 9.406154796041011679, -0.7216878364870338292 ) ) ;
#9675 = ORIENTED_EDGE ( 'NONE', *, *, #16450, .T. ) ;
#9676 = CARTESIAN_POINT ( 'NONE',  ( 3.584973236653755002, 1.601158291227417152, -0.7540797108817003380 ) ) ;
#9678 = CARTESIAN_POINT ( 'NONE',  ( 0.1997390566700393277, -0.6049713359795177992, 2.210933144166931985 ) ) ;
#9677 = CARTESIAN_POINT ( 'NONE',  ( 3.228249973385329596, 6.780392379009261283, -1.734723475976807094E-15 ) ) ;
#9679 = CARTESIAN_POINT ( 'NONE',  ( 5.331922971087851515, 1.814509544241477146, 0.3110680438872318043 ) ) ;
#9680 = CARTESIAN_POINT ( 'NONE',  ( -3.653032323878261600, 6.349289246911547835, -1.199719254218452047 ) ) ;
#9681 = CARTESIAN_POINT ( 'NONE',  ( 4.812781342726855982, 7.598366752281232372, 1.082531754730558626 ) ) ;
#9682 = CARTESIAN_POINT ( 'NONE',  ( -1.201851678989727383E-14, 4.087500000000022560, -1.732050807568863648 ) ) ;
#9683 = CARTESIAN_POINT ( 'NONE',  ( 4.400438482046089561, 1.694813852089768869, -1.389250428430639950 ) ) ;
#9684 = CARTESIAN_POINT ( 'NONE',  ( -2.625475302540713152, 6.214804952939456228, -0.7998128361456281477 ) ) ;
#9685 = FACE_OUTER_BOUND ( 'NONE', #36607, .T. ) ;
#9686 = CARTESIAN_POINT ( 'NONE',  ( 5.389151899530504330, 0.1487064154041470299, 2.065066873896327593 ) ) ;
#9687 = CARTESIAN_POINT ( 'NONE',  ( 0.005092704479254389627, -0.09411098085002241043, 2.014433268766747887 ) ) ;
#9688 =( GEOMETRIC_REPRESENTATION_CONTEXT ( 3 ) GLOBAL_UNCERTAINTY_ASSIGNED_CONTEXT ( ( #174663 ) ) GLOBAL_UNIT_ASSIGNED_CONTEXT ( ( #124382, #209785, #28930 ) ) REPRESENTATION_CONTEXT ( 'NONE', 'WORKASPACE' ) );
#9689 = CARTESIAN_POINT ( 'NONE',  ( 1.364683531249988535, 5.155208333674749177, -0.7879004041258300672 ) ) ;
#9690 = CARTESIAN_POINT ( 'NONE',  ( 2.807156881705831442, 1.627618881652561411, 1.030384643589934646 ) ) ;
#9691 = CARTESIAN_POINT ( 'NONE',  ( 1.364683531249996529, 10.96354166700806942, 0.7879004041258405033 ) ) ;
#9692 = CARTESIAN_POINT ( 'NONE',  ( -3.470524135418306511, 5.072030796119872953, -1.443375672974053447 ) ) ;
#9693 = CARTESIAN_POINT ( 'NONE',  ( -0.05205951232617207075, -2.027416208471942038, 0.9083432681902519068 ) ) ;
#9694 = ORIENTED_EDGE ( 'NONE', *, *, #165975, .F. ) ;
#9696 = DIRECTION ( 'NONE',  ( 0.000000000000000000, 0.000000000000000000, 1.000000000000000000 ) ) ;
#9695 = CARTESIAN_POINT ( 'NONE',  ( -4.828112100242294424, 5.765790550771681566, -1.082531754730549967 ) ) ;
#9697 = CARTESIAN_POINT ( 'NONE',  ( 5.678167406024951624, 5.518950149984223508, 0.7998128361456341429 ) ) ;
#9698 = FILL_AREA_STYLE_COLOUR ( '', #180717 ) ;
#9699 = CYLINDRICAL_SURFACE ( 'NONE', #69895, 0.08000000000000041800 ) ;
#9700 = CARTESIAN_POINT ( 'NONE',  ( 11.75999501215279963, 7.882567973567104147, -2.166920717415847353 ) ) ;
#9701 = CARTESIAN_POINT ( 'NONE',  ( 10.37162432432990755, 11.20257592124748136, -0.7216878364870257245 ) ) ;
#9703 = CARTESIAN_POINT ( 'NONE',  ( 1.750371521623844462, -1.952110535733902585, -0.1955497077021361163 ) ) ;
#9702 = CIRCLE ( 'NONE', #123918, 0.08000000000000014044 ) ;
#9704 = CARTESIAN_POINT ( 'NONE',  ( -1.364683531250000748, 1.071875000341421247, 0.000000000000000000 ) ) ;
#9705 = EDGE_CURVE ( 'NONE', #116397, #209056, #27484, .T. ) ;
#9706 = CARTESIAN_POINT ( 'NONE',  ( 0.3999999999999889200, 3.372708439410121439, -0.5000000000000368594 ) ) ;
#9707 = CARTESIAN_POINT ( 'NONE',  ( 5.652778587040098834, -0.4750822840141955550, -1.903360745478323679 ) ) ;
#9708 = CARTESIAN_POINT ( 'NONE',  ( -8.296699936558862731, 11.76690146170562201, 1.199719254218453823 ) ) ;
#9709 = CARTESIAN_POINT ( 'NONE',  ( -4.378920427089552092, 8.052564898339037214, 0.7216878364870317197 ) ) ;
#9710 = CARTESIAN_POINT ( 'NONE',  ( 6.491117449447131982, 1.883434485765375310, -1.060826435891427666 ) ) ;
#9712 = EDGE_LOOP ( 'NONE', ( #175488, #136539, #193559, #70664 ) ) ;
#9711 = CARTESIAN_POINT ( 'NONE',  ( -0.3617173305618593959, -5.199791778942955744, -10.99431798667224136 ) ) ;
#9713 = CARTESIAN_POINT ( 'NONE',  ( -1.402160292154681736E-14, -0.8812499993171809543, -1.732050807568870754 ) ) ;
#9714 = CARTESIAN_POINT ( 'NONE',  ( 0.2802489257003986656, -1.812731005579379051, -0.4610361243657657981 ) ) ;
#9715 = CARTESIAN_POINT ( 'NONE',  ( 6.731818218530718489, -1.587343137472529309, -0.6980196547925822115 ) ) ;
#9717 = CARTESIAN_POINT ( 'NONE',  ( 3.017305944477025825, -2.111434807548946857, 0.5868732223921411251 ) ) ;
#9716 = CARTESIAN_POINT ( 'NONE',  ( -1.360316468749999119, 0.3906250003414130090, -8.673617379884035472E-15 ) ) ;
#9718 = CARTESIAN_POINT ( 'NONE',  ( 4.278580467222413475, -1.332036844872594994, 1.884138376372360479 ) ) ;
#9719 = CARTESIAN_POINT ( 'NONE',  ( 0.4267267499857710367, 1.971919523859454237, 0.5989439635904010295 ) ) ;
#9720 = CARTESIAN_POINT ( 'NONE',  ( 1.974458820771322953, -0.09541523299517583323, -1.939727210137192737 ) ) ;
#9721 = CARTESIAN_POINT ( 'NONE',  ( -5.870317324592829067, 5.951051088220814300, -0.7216878364870197293 ) ) ;
#9722 = EDGE_CURVE ( 'NONE', #171541, #162523, #121062, .T. ) ;
#9723 = DIRECTION ( 'NONE',  ( 0.000000000000000000, 1.000000000000000000, 0.000000000000000000 ) ) ;
#9724 = CARTESIAN_POINT ( 'NONE',  ( 5.502226937873657242, -0.9515977829631333540, 1.895136135177949877 ) ) ;
#9725 = CARTESIAN_POINT ( 'NONE',  ( 3.041638857185970046, -1.525043868314728934, 1.319228477497782714 ) ) ;
#9726 = CARTESIAN_POINT ( 'NONE',  ( -3.890826896997578999, 7.483122446565064756, 0.7216878364870317197 ) ) ;
#9727 = CARTESIAN_POINT ( 'NONE',  ( -6.583366107887490770, 9.838288338247510367, 1.199719254218452935 ) ) ;
#9728 = CARTESIAN_POINT ( 'NONE',  ( 9.480175724453529185, 12.08329098332774265, 1.599625672291279388 ) ) ;
#9729 = DIRECTION ( 'NONE',  ( 1.039099362110107450E-15, 1.000000000000000000, -4.583713267641621330E-32 ) ) ;
#9730 = CARTESIAN_POINT ( 'NONE',  ( -5.641074431737709283, 8.738948049406083385, -1.199719254218452047 ) ) ;
#9731 = LINE ( 'NONE', #193810, #64732 ) ;
#9732 = CARTESIAN_POINT ( 'NONE',  ( -10.30047605039691128, 4.688744718740807116, 5.507884344589919934 ) ) ;
#9733 = EDGE_LOOP ( 'NONE', ( #177182, #32572, #185276, #212455 ) ) ;
#9734 = CARTESIAN_POINT ( 'NONE',  ( 5.207911835226475716, -2.051185258288893198, 0.1996322284415520676 ) ) ;
#9735 = CARTESIAN_POINT ( 'NONE',  ( -7.729556973122450714, 8.190440354830551328, 0.000000000000000000 ) ) ;
#9736 = CARTESIAN_POINT ( 'NONE',  ( 7.634649897826744080, 9.040084647953621655, 1.082531754730549078 ) ) ;
#9737 = CARTESIAN_POINT ( 'NONE',  ( -4.925689880466507908, 4.641059703499347044, -0.7998128361456221525 ) ) ;
#9738 = CARTESIAN_POINT ( 'NONE',  ( -6.025283891683315574, 6.066383424671776936, 0.6274445299816646671 ) ) ;
#9739 = CARTESIAN_POINT ( 'NONE',  ( 4.389322685995568740, -0.002182162029157329840, -2.019862493239577894 ) ) ;
#9741 = ORIENTED_EDGE ( 'NONE', *, *, #193016, .T. ) ;
#9740 = CARTESIAN_POINT ( 'NONE',  ( 6.164703477482621707, 0.6939275443377226349, 2.110173311658748663 ) ) ;
#9742 = COLOUR_RGB ( '', 0.40784314, 0.44705882, 0.49803922) ;
#9744 = CARTESIAN_POINT ( 'NONE',  ( 7.782016984564043227, 12.02284421539267356, 0.7216878364870438212 ) ) ;
#9743 = CARTESIAN_POINT ( 'NONE',  ( -5.029148636026397945, 4.832037928311032182, 0.7998128361456281477 ) ) ;
#9745 = CARTESIAN_POINT ( 'NONE',  ( 5.795220594837462436, 8.848508896363995291, -1.199719254218440723 ) ) ;
#9746 = CARTESIAN_POINT ( 'NONE',  ( 4.065347389730957772, 0.2539501645208458447, -2.045120066754711363 ) ) ;
#9747 = CARTESIAN_POINT ( 'NONE',  ( 3.393204081532863459, -0.8197727808607684352, -1.842447475547980495 ) ) ;
#9748 = ORIENTED_EDGE ( 'NONE', *, *, #70626, .T. ) ;
#9749 = CARTESIAN_POINT ( 'NONE',  ( 4.192495815123822744, 5.914331089109666983, -1.599625672291255185 ) ) ;
#9751 = ORIENTED_EDGE ( 'NONE', *, *, #107896, .F. ) ;
#9750 = CARTESIAN_POINT ( 'NONE',  ( -0.3138284133838390444, 8.211984188054007205, -1.978018658440992006 ) ) ;
#9752 = CARTESIAN_POINT ( 'NONE',  ( 5.726091835933811325, 7.283405380927965744, -1.209259067671350163 ) ) ;
#9753 = CARTESIAN_POINT ( 'NONE',  ( 3.005232341680406094, 2.000550758621592706, 0.2495690156183311137 ) ) ;
#9754 = CARTESIAN_POINT ( 'NONE',  ( 2.062219658421380775, -1.683061746929171321, -0.7467898329211534181 ) ) ;
#9755 = EDGE_CURVE ( 'NONE', #136413, #160735, #153595, .T. ) ;
#9756 = CARTESIAN_POINT ( 'NONE',  ( 1.067484182866541564, -2.088262569869667740, -0.9824423588734966239 ) ) ;
#9757 = CARTESIAN_POINT ( 'NONE',  ( 6.235824307642648279, 6.239826211863360506, 0.000000000000000000 ) ) ;
#9758 = CARTESIAN_POINT ( 'NONE',  ( 3.690839692606663558, -0.4176960054509891163, -2.120685484085436112 ) ) ;
#9759 = VECTOR ( 'NONE', #150361, 1000.000000000000000 ) ;
#9760 = CARTESIAN_POINT ( 'NONE',  ( -6.847031270101295419, 7.946956888995021728, -1.199719254218446718 ) ) ;
#9761 = CARTESIAN_POINT ( 'NONE',  ( 3.251609920728415037, -2.263897172838242877, -0.3959942320375854918 ) ) ;
#9762 = ORIENTED_EDGE ( 'NONE', *, *, #15859, .F. ) ;
#9763 = CARTESIAN_POINT ( 'NONE',  ( 2.550000000000000266, 2.499999999999998668, 1.849324200890695824 ) ) ;
#9764 = CARTESIAN_POINT ( 'NONE',  ( 1.340467186903429253, 0.3614942610149494695, 1.835218787103513050 ) ) ;
#9765 = CARTESIAN_POINT ( 'NONE',  ( 6.209841870239331207, -1.956602576295646490, 0.2410399859902948028 ) ) ;
#9768 = EDGE_CURVE ( 'NONE', #193157, #142998, #159977, .T. ) ;
#9767 = CARTESIAN_POINT ( 'NONE',  ( 9.205623113554628034, 9.842241175342985926, 0.7216878364870458196 ) ) ;
#9766 = CARTESIAN_POINT ( 'NONE',  ( 1.364683531249988535, 4.905208333674756283, -0.7879004041258300672 ) ) ;
#9770 = CARTESIAN_POINT ( 'NONE',  ( 1.084930333755677045, -2.153824616689365978, -0.4803136671489223741 ) ) ;
#9769 = CARTESIAN_POINT ( 'NONE',  ( -7.061099074618889304, 7.132370430010492868, -0.7998128361456291469 ) ) ;
#9771 = DIRECTION ( 'NONE',  ( -0.5000000000000102141, 0.000000000000000000, -0.8660254037844328234 ) ) ;
#9772 = CARTESIAN_POINT ( 'NONE',  ( 4.171104814498611368, 8.018039383557042044, 0.7998128361456321445 ) ) ;
#9773 = CARTESIAN_POINT ( 'NONE',  ( -4.737684612971557740, 7.614716917520386374, 1.199719254218464037 ) ) ;
#9774 = CARTESIAN_POINT ( 'NONE',  ( 6.639320575229255894, 7.629137130509070275, 2.703262396134015866 ) ) ;
#9775 = CARTESIAN_POINT ( 'NONE',  ( 4.610209453490740295, -0.8421727957172200352, -1.782655373600953386 ) ) ;
#9776 = ADVANCED_FACE ( 'NONE', ( #174025 ), #151965, .F. ) ;
#9777 = CARTESIAN_POINT ( 'NONE',  ( 6.199901738523720951, -0.7837251098280417771, 2.170682987836409783 ) ) ;
#9778 = CARTESIAN_POINT ( 'NONE',  ( 5.547250370032299038, 1.641257983771953866, -0.8773172063531119447 ) ) ;
#9779 = CARTESIAN_POINT ( 'NONE',  ( 2.606363979242664719, 2.062007909489747881, 0.05513178878350195877 ) ) ;
#9780 = CARTESIAN_POINT ( 'NONE',  ( 5.002595493762530765, 8.780185809457538681, 1.040834085586084257E-14 ) ) ;
#9781 = CARTESIAN_POINT ( 'NONE',  ( 3.923105346307896202, 5.670318552149568703, -1.599625672291269396 ) ) ;
#9782 = CARTESIAN_POINT ( 'NONE',  ( 0.6823417656249882723, 1.488541667008083547, -1.181850606188749264 ) ) ;
#9783 = CARTESIAN_POINT ( 'NONE',  ( 0.08058608058607134861, -6.271284633940159559, -10.99970480893079916 ) ) ;
#9784 = CARTESIAN_POINT ( 'NONE',  ( 5.409340101728155936, 8.294351971116089572, -1.082531754730543971 ) ) ;
#9785 = CARTESIAN_POINT ( 'NONE',  ( 5.160662515399747186, -0.7266353732918430230, -2.046117350891932141 ) ) ;
#9787 = CARTESIAN_POINT ( 'NONE',  ( 4.036529152626888717, -1.599951230533543267, 0.9111318136766360931 ) ) ;
#9786 = CARTESIAN_POINT ( 'NONE',  ( -2.331639231870358930, 5.664070170583284103, -0.7216878364870267237 ) ) ;
#9789 = CARTESIAN_POINT ( 'NONE',  ( 6.720655732516655156, 7.629137130509086262, 2.526260288887293814 ) ) ;
#9788 = CARTESIAN_POINT ( 'NONE',  ( -9.946057155611605083, 2.515145635913770494, -6.189092007093218051 ) ) ;
#9790 = CARTESIAN_POINT ( 'NONE',  ( 6.181208317857348256, 1.509947553572440704, 1.588605474358975478 ) ) ;
#9791 = CARTESIAN_POINT ( 'NONE',  ( 0.2458944382301266607, -1.750094391731635168, -1.433289930825008218 ) ) ;
#9792 = CARTESIAN_POINT ( 'NONE',  ( -3.975603406396657213, 7.849426279905078019, -0.02588959144292704573 ) ) ;
#9793 = DIRECTION ( 'NONE',  ( -0.000000000000000000, -1.000000000000000000, -0.000000000000000000 ) ) ;
#9794 = CARTESIAN_POINT ( 'NONE',  ( 6.472394699177205446, 6.854181287346997387, 0.6349317888264572884 ) ) ;
#9795 = CARTESIAN_POINT ( 'NONE',  ( -3.919715807682309094, 6.626733304721049933, 1.082531754730549967 ) ) ;
#9796 = CARTESIAN_POINT ( 'NONE',  ( 0.1352199593073095951, -0.09384731153385186819, 1.910084486482076294 ) ) ;
#9797 = CARTESIAN_POINT ( 'NONE',  ( 0.2327837997007513038, -1.621012357304358220, 0.7108589729635225174 ) ) ;
#9798 = CARTESIAN_POINT ( 'NONE',  ( 5.813144886445268611, 1.644464822582414332, -1.160890557811714352 ) ) ;
#9799 = CARTESIAN_POINT ( 'NONE',  ( 6.817052309572890323, 6.847649204123507083, 0.7998128361456341429 ) ) ;
#9800 = CARTESIAN_POINT ( 'NONE',  ( 4.067482540003349634, 0.2598354432931935243, -2.089805856947650309 ) ) ;
#9801 = CARTESIAN_POINT ( 'NONE',  ( 2.794441263998331149, 1.385543030692138133, -1.323043162562879349 ) ) ;
#9802 = CARTESIAN_POINT ( 'NONE',  ( -0.02244404828157658613, 0.6916080914694566761, -2.270927585766496559 ) ) ;
#9803 = CARTESIAN_POINT ( 'NONE',  ( 4.826587240018016089, -1.288162778474700287, 1.489951593160773635 ) ) ;
#9804 = CARTESIAN_POINT ( 'NONE',  ( 5.695571270406009745, 1.864622851205568699, -0.7768453975713036641 ) ) ;
#9805 = CARTESIAN_POINT ( 'NONE',  ( 3.186256133050053840, -1.842714570631575510, -0.3211874441736498054 ) ) ;
#9808 = ORIENTED_EDGE ( 'NONE', *, *, #78734, .F. ) ;
#9807 = CARTESIAN_POINT ( 'NONE',  ( 1.757924209179074770, 0.7287868685415777037, -1.768279316124596878 ) ) ;
#9806 = CARTESIAN_POINT ( 'NONE',  ( 4.723137274085514647, -0.08022016869785492110, 1.723147214940720762 ) ) ;
#9810 = CARTESIAN_POINT ( 'NONE',  ( 4.853455804012228647, 4.764712647543454693, 0.7216878364870317197 ) ) ;
#9809 = CARTESIAN_POINT ( 'NONE',  ( 1.963769682107346037, 0.3752889857368995608, -2.174583152744386627 ) ) ;
#9811 = CARTESIAN_POINT ( 'NONE',  ( -1.364683531250012516, 2.551041667008089320, -0.7879004041258289570 ) ) ;
#9812 = CARTESIAN_POINT ( 'NONE',  ( 6.531700620877029628, 1.877769495358465157, -0.5682946464737671510 ) ) ;
#9813 = CARTESIAN_POINT ( 'NONE',  ( 8.101160479365381306, 9.410107633136481908, -1.199719254218446718 ) ) ;
#9814 = CARTESIAN_POINT ( 'NONE',  ( -10.65400978224035811, 11.32409958890225710, 1.040834085586084257E-14 ) ) ;
#9815 = FACE_OUTER_BOUND ( 'NONE', #133822, .T. ) ;
#9816 = CARTESIAN_POINT ( 'NONE',  ( 3.008927249609713250, 6.454239524612553680, -0.03298405530798137475 ) ) ;
#9817 = FACE_OUTER_BOUND ( 'NONE', #2900, .T. ) ;
#9819 = CIRCLE ( 'NONE', #151612, 3.100000000000000089 ) ;
#9818 = CIRCLE ( 'NONE', #44481, 0.7500000000000011102 ) ;
#9820 = CARTESIAN_POINT ( 'NONE',  ( 2.242711981562468093, -2.029969483702593003, -0.4061203719310027549 ) ) ;
#9821 = CARTESIAN_POINT ( 'NONE',  ( -1.499999999999997780, 3.150000000000020783, 1.214306433183764966E-14 ) ) ;
#9822 = CARTESIAN_POINT ( 'NONE',  ( 6.986529229743720926, 7.045372277656132276, -0.7998128361456281477 ) ) ;
#9823 = CARTESIAN_POINT ( 'NONE',  ( -7.874588291438845644, 8.081441182967111558, -0.7998128361456291469 ) ) ;
#9824 = CARTESIAN_POINT ( 'NONE',  ( 4.415115299905642665, 5.179997933758551554, -1.199719254218450271 ) ) ;
#9825 = CARTESIAN_POINT ( 'NONE',  ( -0.1048592448738161903, -0.1538584160990438265, -1.986454975908092058 ) ) ;
#9826 = CARTESIAN_POINT ( 'NONE',  ( -9.499700864329909678, -7.154544010627095219, -0.07538891330675229208 ) ) ;
#9827 = CARTESIAN_POINT ( 'NONE',  ( 0.6823417656249882723, 2.426041667008084435, -1.181850606188749264 ) ) ;
#9829 = CARTESIAN_POINT ( 'NONE',  ( 3.195971524519376494, 4.751719416737803847, -1.599625672291262513 ) ) ;
#9828 = DIRECTION ( 'NONE',  ( -0.08676574618400526018, 0.9962285034897238045, -0.0006885664517735924335 ) ) ;
#9830 = CARTESIAN_POINT ( 'NONE',  ( 5.606796008369615336, 0.8196459417171354511, -1.842166028910074527 ) ) ;
#9831 = CARTESIAN_POINT ( 'NONE',  ( 4.786306776965392196, -0.6515362397919061133, -1.801638605214391342 ) ) ;
#9832 = SURFACE_SIDE_STYLE ('',( #145216 ) ) ;
#9833 = CARTESIAN_POINT ( 'NONE',  ( 2.120887600855193345, 0.003649250790785373531, 2.191739723551556551 ) ) ;
#9834 = CARTESIAN_POINT ( 'NONE',  ( -3.294268138440636928, 6.787137228248626641, 1.040834085586084257E-14 ) ) ;
#9835 = CARTESIAN_POINT ( 'NONE',  ( 1.499999999999989120, 2.056250000682817269, 1.214306433183764966E-14 ) ) ;
#9836 = CARTESIAN_POINT ( 'NONE',  ( 4.957293921627444533, -1.724444360862188885, 1.038707789177233831 ) ) ;
#9837 = CARTESIAN_POINT ( 'NONE',  ( 1.722773492080275748, 1.414811824084385883, -1.286832238068566392 ) ) ;
#9838 = CARTESIAN_POINT ( 'NONE',  ( -6.501298352952815662, 7.543601818988450169, -1.199719254218446718 ) ) ;
#9840 = CARTESIAN_POINT ( 'NONE',  ( 0.3687678296072604556, -0.2496303596870551866, -2.000855358883571800 ) ) ;
#9839 = CARTESIAN_POINT ( 'NONE',  ( -4.284013352238274841, 4.100363120473813794, -0.7216878364870207285 ) ) ;
#9842 = ADVANCED_FACE ( 'NONE', ( #11482 ), #92316, .T. ) ;
#9841 = CARTESIAN_POINT ( 'NONE',  ( -1.364683531250000748, 10.17187500034139802, 0.000000000000000000 ) ) ;
#9844 = CARTESIAN_POINT ( 'NONE',  ( -5.119085517611572378, 8.129960982925583224, 1.199719254218452935 ) ) ;
#9843 = CARTESIAN_POINT ( 'NONE',  ( 3.702747019872438372, 1.794327276830971707, 1.072858563533698018 ) ) ;
#9846 = ORIENTED_EDGE ( 'NONE', *, *, #44338, .F. ) ;
#9845 = CARTESIAN_POINT ( 'NONE',  ( 1.852176121455822777, 0.5370312411601232405, 1.639109186831126053 ) ) ;
#9847 = DIRECTION ( 'NONE',  ( 1.224646799147353454E-16, 0.000000000000000000, -1.000000000000000000 ) ) ;
#9848 = CARTESIAN_POINT ( 'NONE',  ( 6.311484202361478779, 7.322151976631905868, -1.199719254218446718 ) ) ;
#9849 = CARTESIAN_POINT ( 'NONE',  ( -7.709579522695857001, -6.700642373080281544, -7.846302513400019940 ) ) ;
#9850 = DIRECTION ( 'NONE',  ( 0.000000000000000000, 0.000000000000000000, -1.000000000000000000 ) ) ;
#9851 = DIRECTION ( 'NONE',  ( 0.000000000000000000, -1.000000000000000000, 0.000000000000000000 ) ) ;
#9852 = CARTESIAN_POINT ( 'NONE',  ( 5.789495288235341874, 6.713164910151406595, 1.199719254218462483 ) ) ;
#9853 = ORIENTED_EDGE ( 'NONE', *, *, #12404, .F. ) ;
#9854 = DIRECTION ( 'NONE',  ( 0.000000000000000000, 0.000000000000000000, -1.000000000000000000 ) ) ;
#9855 = CARTESIAN_POINT ( 'NONE',  ( 2.420317109208899531, -0.6946167411978272366, -1.673203699974361580 ) ) ;
#9856 = ORIENTED_EDGE ( 'NONE', *, *, #139194, .T. ) ;
#9857 = CARTESIAN_POINT ( 'NONE',  ( 4.729096653068339151, 4.411700938201493116, -0.7998128361456211532 ) ) ;
#9858 = CARTESIAN_POINT ( 'NONE',  ( 4.278479993564246797, 7.149254538203735798, 1.199719254218452047 ) ) ;
#9859 = CARTESIAN_POINT ( 'NONE',  ( 4.178215122889179511, 0.8575144648667647473, 1.595655492163786437 ) ) ;
#9860 = CARTESIAN_POINT ( 'NONE',  ( 0.000000000000000000, -6.532648833121157850, 0.000000000000000000 ) ) ;
#9861 = CARTESIAN_POINT ( 'NONE',  ( 5.726377019126981160, 6.078880280049443918, 0.6665230057388837892 ) ) ;
#9862 = CIRCLE ( 'NONE', #82522, 1.250000000000000222 ) ;
#9863 = CARTESIAN_POINT ( 'NONE',  ( 4.439814405351947713, 1.214877501302736862, 1.409928613244580742 ) ) ;
#9864 = EDGE_CURVE ( 'NONE', #11502, #91840, #197304, .T. ) ;
#9865 = CARTESIAN_POINT ( 'NONE',  ( 2.020959903547480341, -1.710230010390185296, 0.8631189023672394267 ) ) ;
#9866 = CARTESIAN_POINT ( 'NONE',  ( 0.5162701059127188241, 1.262803565755654001, -1.318596375272471199 ) ) ;
#9867 = CARTESIAN_POINT ( 'NONE',  ( 4.728828643816226140, 8.210394131765152537, 0.6915292512235807765 ) ) ;
#9868 = CARTESIAN_POINT ( 'NONE',  ( -0.4205927090898516907, 3.223357252100233605, 1.955451565440526007 ) ) ;
#9869 = CARTESIAN_POINT ( 'NONE',  ( 4.816695983655697511, 8.110494931179941247, 0.8576603160085185529 ) ) ;
#9870 = CARTESIAN_POINT ( 'NONE',  ( 4.876338901402099246, 8.164033411617232616, 0.9883146796138141399 ) ) ;
#9871 = CARTESIAN_POINT ( 'NONE',  ( -3.650099463454746118, 7.352759259900637723, 0.1599090995409638560 ) ) ;
#9872 = CARTESIAN_POINT ( 'NONE',  ( -4.140316941461365197, 3.976524957527992843, 0.4412079600669023272 ) ) ;
#9873 = CARTESIAN_POINT ( 'NONE',  ( 7.293923454472080792, 9.532663335016016148, 1.443375672974076540 ) ) ;
#9874 = CARTESIAN_POINT ( 'NONE',  ( 5.524252356588593926, 0.9672068372908498857, 1.715464803677963834 ) ) ;
#9875 = CARTESIAN_POINT ( 'NONE',  ( -3.730464822054482710, 7.503959392372201442, 1.040834085586084257E-14 ) ) ;
#9876 = CARTESIAN_POINT ( 'NONE',  ( -0.4786071537202271076, 6.664221364234077960, 3.365248248540958276 ) ) ;
#9877 = CARTESIAN_POINT ( 'NONE',  ( 0.7266515212380560973, 0.1555473773823950467, 2.084908828405390491 ) ) ;
#9878 = CARTESIAN_POINT ( 'NONE',  ( 8.281332899848809603, 8.555976559445431562, 0.7998128361456481317 ) ) ;
#9879 = CARTESIAN_POINT ( 'NONE',  ( 5.297847195631281814, -0.6933188941696236673, 1.797466220796402725 ) ) ;
#9880 = CARTESIAN_POINT ( 'NONE',  ( -5.473741331615264549, 7.409117525016355010, -1.599625672291256295 ) ) ;
#9881 = EDGE_CURVE ( 'NONE', #124240, #145532, #176599, .T. ) ;
#9882 = CARTESIAN_POINT ( 'NONE',  ( 1.641335390984842491, -1.319735721761399638, -1.261605215524951085 ) ) ;
#9883 = CARTESIAN_POINT ( 'NONE',  ( 1.998912159191484905, -0.5904864226158462737, -2.126349760018491963 ) ) ;
#9884 = CARTESIAN_POINT ( 'NONE',  ( -2.788906526875773208E-15, 10.43750000000000000, -1.499999999999998446 ) ) ;
#9885 = CARTESIAN_POINT ( 'NONE',  ( 1.265713261412576562, 0.5522810963098608861, -1.830935845731461953 ) ) ;
#9886 = CARTESIAN_POINT ( 'NONE',  ( 6.930521655090660538, -1.214226768402311363, 1.551031149239000761 ) ) ;
#9887 = CARTESIAN_POINT ( 'NONE',  ( 2.366656106817651040, 0.09313060749883492195, -1.939932752287050199 ) ) ;
#9888 = CARTESIAN_POINT ( 'NONE',  ( 1.317732270343049406, -1.591076063098846749, 1.238129638497114771 ) ) ;
#9890 = CARTESIAN_POINT ( 'NONE',  ( 6.157066405694873623, 1.522017207847397469, -1.070502804743376668 ) ) ;
#9889 = CARTESIAN_POINT ( 'NONE',  ( -5.173318132066234476, 8.193232366456022930, -1.199719254218453823 ) ) ;
#9891 = CARTESIAN_POINT ( 'NONE',  ( 6.073126464278658432, 6.050012061272033392, 0.000000000000000000 ) ) ;
#9892 = CARTESIAN_POINT ( 'NONE',  ( -11.43195036480942051, 13.65524496285257783, -3.649565797774410036 ) ) ;
#9893 = CARTESIAN_POINT ( 'NONE',  ( 9.480175724453529185, 12.08329098332774265, 1.599625672291279388 ) ) ;
#9894 = CARTESIAN_POINT ( 'NONE',  ( -3.958090780185743451, 6.705190779270287393, -1.199719254218452047 ) ) ;
#9895 = CARTESIAN_POINT ( 'NONE',  ( -5.773793314573309132, 7.829454515125894964, 1.599625672291263179 ) ) ;
#9896 = CARTESIAN_POINT ( 'NONE',  ( 2.472451708263478931, -2.098117355222902436, -0.6331711661175795092 ) ) ;
#9897 = CARTESIAN_POINT ( 'NONE',  ( 3.063779527008304360, 6.518233848244248563, 0.7216878364870317197 ) ) ;
#9898 = AXIS2_PLACEMENT_3D ( 'NONE', #102502, #183747, #6042 ) ;
#9899 = DIRECTION ( 'NONE',  ( -0.9446243521954068578, 0.000000000000000000, 0.3281536732072456997 ) ) ;
#9900 = DIRECTION ( 'NONE',  ( -4.462851221005182648E-16, -0.7999999999999986011, 0.6000000000000019762 ) ) ;
#9901 = CARTESIAN_POINT ( 'NONE',  ( 2.508196354075361789, -0.6984789837382252564, -1.686990664346368796 ) ) ;
#9902 = CARTESIAN_POINT ( 'NONE',  ( -0.7500000000000006661, 12.98958333401613352, -1.299038105676657340 ) ) ;
#9903 = CARTESIAN_POINT ( 'NONE',  ( -2.927671105547157371, 5.503034492191895666, 1.199719254218462483 ) ) ;
#9904 = CARTESIAN_POINT ( 'NONE',  ( -4.684263184503158151, 8.377143357790286515, -0.6327197186303500365 ) ) ;
#9905 = CARTESIAN_POINT ( 'NONE',  ( 0.000000000000000000, 8.920000000000001705, 0.000000000000000000 ) ) ;
#9906 = CARTESIAN_POINT ( 'NONE',  ( 7.456094412511537151, 10.78619501698377370, 1.199719254218460707 ) ) ;
#9907 = CARTESIAN_POINT ( 'NONE',  ( 0.8735101492000696410, 1.856966920605634508, -0.5126664406217595893 ) ) ;
#9908 = CARTESIAN_POINT ( 'NONE',  ( 6.069191303861535935, 1.728486752094374967, 0.9278679456784576507 ) ) ;
#9909 = AXIS2_PLACEMENT_3D ( 'NONE', #174462, #92151, #26038 ) ;
#9910 = CARTESIAN_POINT ( 'NONE',  ( -0.7500000000000179856, 15.29166666666666785, 1.299038105676658228 ) ) ;
#9911 = CARTESIAN_POINT ( 'NONE',  ( -8.376239975144482486, 8.666701480623698828, 1.040834085586084257E-14 ) ) ;
#9912 = CARTESIAN_POINT ( 'NONE',  ( 5.847644326195776010, 5.716673223516856694, -0.7998128361456281477 ) ) ;
#9913 = EDGE_CURVE ( 'NONE', #150798, #157913, #117534, .T. ) ;
#9914 = CARTESIAN_POINT ( 'NONE',  ( 4.950807510372833065, -1.851323926424643274, -1.172527737679923465 ) ) ;
#9915 =( BOUNDED_SURFACE ( )  B_SPLINE_SURFACE ( 1, 2, ( 
 ( #122541, #6533, #136575, #154949, #20650, #72612, #138711, #56378, #185290, #35848, #156016, #36913, #135505, #188502, #202596, #151757, #106244, #203663, #105148, #170114, #137644, #169053, #172270, #23856, #89964, #7603, #186361, #54248, #52115, #55314, #118242, #184225, #19598, #167993, #101927, #86740, #70459, #3328, #201528, #171188, #152809, #4388, #120386, #5454, #37996, #104068, #21701, #87813, #153885, #121463, #187433, #22777, #39062, #27062, #75823, #10805, #177602, #110529, #76879, #109467, #24927, #159204, #144074, #210069, #43347, #74763, #61709, #175474, #95304, #91031, #108394, #8681, #205813, #143000, #123605, #9749, #57445, #25994, #208998, #92103, #140865, #191687, #206878, #125726, #124665, #127877, #190622, #157092, #58510, #193827, #189570, #42281, #60634, #59566, #28141, #192752, #174418, #41215, #158157, #141932, #126797, #45476, #207945, #93167, #44409, #161353, #176529, #94236, #160274, #11877, #77953, #111592, #29214, #173346, #12935, #139786, #107322, #211138, #30281, #212199, #147239, #164538, #15062, #16124, #62760, #163480, #145131, #179734, #98473, #31352, #13998, #131041, #146184, #64894, #63836, #83267, #129994, #96368, #195983, #935, #128920, #47615, #82207, #213267, #181831, #132080, #113729, #194901, #97427, #80083, #214298, #67002, #81154, #197030, #48667, #100599, #114784, #180782, #162421, #32407, #148301, #65931, #198089, #112660, #149355, #99539, #49716, #46539, #115845, #33464, #165603, #17192, #133139, #199138, #50783, #116911, #182911, #34527, #166675, #79015, #178669, #121209, #52915, #38806, #187178, #170930, #85416, #68066, #188241, #151499, #101668, #22527, #168798, #117986, #88636, #21452, #137389, #202337, #169863, #135262, #104888, #154694, #6277, #72349, #4138, #86486, #138451, #87560, #204472, #56125, #51864, #200212, #122283, #3069, #102743, #134202, #105992, #203405, #150438, #18265, #183978, #37738, #84349, #35589, #167737, #39881, #2001, #153628, #20405, #55058, #19337, #120130, #152551, #103814, #69139, #201275, #5200, #53989, #119048, #71275, #185032, #36658, #136319, #70206, #186106, #207698, #127619, #57192, #140615, #40957, #23604, #77699, #205553, #139527, #11625, #156838, #42031, #73426, #45227, #142745, #89713, #172012, #123352, #191436, #155763, #7347, #189319, #209817, #107065, #26813, #108143, #208753, #143820, #59319, #174169, #43103, #61452, #60379, #109217, #141685, #173090, #175228, #176285, #27887, #75576, #24671, #93984, #125476, #193583, #90777, #206627, #8425, #74511, #92915, #58257, #25741, #124413, #190371, #158961, #91852, #157909, #9504, #10556, #76630, #126542, #160026, #192504, #44155, #110276, #33212, #28959, #13756, #114539, #31106, #214054, #164288, #96113, #95044, #79830, #112407, #32155, #99296, #113477, #63587, #145940, #132883, #47363, #179484, #128679, #194648, #46290, #64650, #195727, #144883, #115589, #131829, #178418, #161094, #62514, #30028, #97179, #196785, #163233, #49470, #15876, #81961, #14815, #180533, #165343, #197838, #80906, #65682, #211952, #181583, #16938, #83019, #162169, #12683, #66740, #129744, #146997, #149092, #213014, #210889, #674, #98233, #148046, #130790, #48426, #198885, #111342, #177347, #78759, #137125, #36401, #118789, #4936, #119863, #203154, #41505, #54798, #102479, #184775, #71012, #185841, #120947, #173650, #84094, #18004, #107619, #35332, #135003, #166409, #141167, #21193, #182651, #50531, #150181, #69946, #116654, #100345, #67806, #91327, #34273, #37473, #201014, #87296, #25224, #152300, #52661, #136058, #157387, #153365, #202071, #20142, #1749, #53731, #189862, #8979, #168545, #199962, #75053, #86229, #133955, #51610, #19079, #117734, #183723, #103551, #101411, #3873, #167484, #151243, #169611, #2812, #85160, #68884, #59866, #193055, #191978, #211436, #43645, #10042, #126018, #129235, #124955, #109759, #210370, #127092, #95604, #45777, #175768, #190917, #27361, #208234, #128166, #195207, #209288, #159501, #93462, #14290, #143297, #60935, #76116, #142221, #11099, #160567, #77175, #26288, #63067, #13247, #44709, #42581, #158441, #110816, #176821, #78247, #28436, #145436, #111894, #177898 ),
 ( #62010, #30584, #46844, #112958, #94529, #12175, #29511, #108685, #144370, #194127, #161652, #58800, #79320, #80385, #178969, #96666, #162718, #207176, #174714, #92402, #81454, #82503, #64141, #181078, #83571, #212500, #134502, #213552, #1234, #149653, #132373, #148590, #164833, #184262, #130285, #116140, #97724, #68370, #31647, #196273, #114032, #99835, #100888, #98778, #65175, #47920, #117210, #67296, #35888, #200506, #150733, #163782, #165901, #199442, #180026, #182129, #48964, #133435, #15361, #115082, #198375, #52149, #159, #118277, #147531, #131330, #18566, #183207, #33758, #101964, #34813, #17485, #197324, #84642, #16423, #168030, #32696, #2293, #19634, #146481, #66226, #50016, #51085, #166975, #203700, #169089, #138745, #5490, #135542, #56415, #204763, #36954, #201567, #152850, #171221, #188538, #173380, #4425, #89998, #106282, #87849, #137679, #202636, #70495, #71571, #55346, #3367, #54286, #41250, #73723, #103034, #53213, #22816, #172303, #121498, #139819, #122576, #153920, #104104, #69436, #186397, #151793, #88929, #38034, #154984, #20688, #40168, #86779, #23892, #85705, #170154, #156049, #7638, #205849, #187470, #120423, #136611, #21740, #57482, #185331, #6569, #119344, #123641, #39100, #72649, #189604, #105185, #107358, #43379, #62795, #157126, #209031, #190655, #161390, #124697, #91066, #206912, #192786, #193862, #191723, #158193, #8715, #210103, #94269, #128957, #12973, #29248, #42316, #44444, #77986, #74800, #60666, #141964, #160309, #140901, #207976, #10836, #145165, #27097, #211170, #174452, #26028, #111627, #61743, #126829, #79049, #127910, #110562, #92138, #177640, #109500, #194936, #108432, #95340, #46573, #112692, #9784, #58542, #144109, #45511, #143036, #75856, #24964, #159235, #59603, #125761, #175507, #93204, #76910, #176564, #28173, #11913, #51894, #97459, #182943, #199171, #180813, #16155, #81189, #163514, #164570, #82240, #96402, #147267, #134236, #166706, #130025, #80114, #49751, #50817, #98508, #18297, #969, #32440, #197063, #162452, #64926, #30317, #115878, #131075, #33499, #196016, #67034, #113763, #133171, #178703, #48701, #116943, #149386, #34559, #148331, #213299, #179767, #31383, #100629, #63870, #114815, #14028, #15101, #132112, #84383, #150470, #214331, #2031, #65963, #198120, #146219, #181863, #99572, #165636, #47652, #17224, #83301, #68100, #200244, #212237, #122318, #138484, #52944, #35620, #69170, #36687, #186135, #203437, #54021, #56155, #22563, #170963, #202372, #187210, #39915, #204506, #120160, #6311, #152581, #188275, #72385, #106024, #185062, #167769, #73460, #102773, #201304, #172046, #37770, #3099, #23639, #121240, #88669, #87590, #55091, #20433, #89747, #155796, #7380, #139561, #103844, #169892, #205588, #38839, #118017, #184006, #151531, #85446, #101699, #168829, #21481, #19366, #135290, #154728, #119082, #86516, #4167, #137418, #70237, #136352, #153662, #5230, #71305, #104922, #141718, #27921, #177378, #158992, #207727, #142777, #95078, #94016, #208783, #26843, #156871, #76663, #61485, #127650, #175258, #206657, #193614, #92947, #12714, #8457, #25773, #140644, #123385, #60413, #40990, #59350, #189350, #157941, #126574, #9533, #58290, #109250, #124446, #43136, #42061, #45255, #108175, #74545, #190405, #111374, #107101, #174201, #192534, #191469, #160055, #110308, #91886, #173124, #75607, #125506, #44188, #28992, #10588, #176316, #11659, #78788, #77732, #24705, #57225, #90807, #143854, #144911, #209846, #161127, #34304, #62544, #65712, #80934, #181615, #116685, #98261, #147024, #81991, #100378, #33244, #148079, #180563, #96147, #15908, #708, #66772, #114571, #145968, #132913, #32185, #166449, #162198, #179515, #79859, #128707, #214084, #194676, #213048, #46320, #97210, #131860, #163262, #211980, #48458, #63619, #196815, #195756, #198918, #47394, #13785, #129774, #50564, #112436, #113507, #197867, #130823, #99326, #49499, #31135, #178449, #14844, #64676, #115619, #182684, #164318, #165377, #16970, #18040, #83051, #149126, #84127, #210918, #30057, #103588, #20176, #183759, #154476, #170710, #85192, #67842, #101443, #68917, #3911, #21230, #86263, #88408 ) ),
 .UNSPECIFIED., .F., .F., .T. ) 
 B_SPLINE_SURFACE_WITH_KNOTS ( ( 2, 2 ),
 ( 3, 2, 2, 2, 2, 2, 2, 2, 2, 2, 2, 2, 2, 2, 2, 2, 2, 2, 2, 2, 2, 2, 2, 2, 2, 2, 2, 2, 2, 2, 2, 2, 2, 2, 2, 2, 2, 2, 2, 2, 2, 2, 2, 2, 2, 2, 2, 2, 2, 2, 2, 2, 2, 2, 2, 2, 2, 2, 2, 2, 2, 2, 2, 2, 2, 2, 2, 2, 2, 2, 2, 2, 2, 2, 2, 2, 2, 2, 2, 2, 2, 2, 2, 2, 2, 2, 2, 2, 2, 2, 2, 2, 2, 2, 2, 2, 2, 2, 2, 2, 2, 2, 2, 2, 2, 2, 2, 2, 2, 2, 2, 2, 2, 2, 2, 2, 2, 2, 2, 2, 2, 2, 2, 2, 2, 2, 2, 2, 2, 2, 2, 2, 2, 2, 2, 2, 2, 2, 2, 2, 2, 2, 2, 2, 2, 2, 2, 2, 2, 2, 2, 2, 2, 2, 2, 2, 2, 2, 2, 2, 2, 2, 2, 2, 2, 2, 2, 2, 2, 2, 2, 2, 2, 2, 2, 2, 2, 2, 2, 2, 2, 2, 2, 2, 2, 2, 2, 2, 2, 2, 2, 2, 2, 2, 2, 2, 2, 2, 2, 2, 2, 2, 2, 2, 2, 2, 2, 2, 2, 2, 2, 2, 2, 2, 2, 2, 2, 2, 2, 2, 2, 2, 2, 2, 2, 2, 2, 2, 2, 2, 2, 2, 2, 2, 2, 2, 2, 2, 2, 2, 3 ),
 ( 0.000000000000000000, 1.000000000000000000 ),
 ( 0.000000000000000000, 0.004166666666666666609, 0.008333333333333333218, 0.01250000000000000069, 0.01666666666666666644, 0.02083333333333333218, 0.02500000000000000139, 0.02916666666666666713, 0.03333333333333333287, 0.03749999999999999861, 0.04166666666666666435, 0.04583333333333333010, 0.05000000000000000278, 0.05416666666666666852, 0.05833333333333333426, 0.06250000000000000000, 0.06666666666666666574, 0.07083333333333333148, 0.07499999999999999722, 0.07916666666666666297, 0.08333333333333332871, 0.08749999999999999445, 0.09166666666666666019, 0.09583333333333333981, 0.1000000000000000056, 0.1041666666666666713, 0.1083333333333333370, 0.1125000000000000028, 0.1166666666666666685, 0.1208333333333333343, 0.1250000000000000000, 0.1291666666666666796, 0.1333333333333333315, 0.1375000000000000111, 0.1416666666666666630, 0.1458333333333333426, 0.1499999999999999944, 0.1541666666666666741, 0.1583333333333333259, 0.1625000000000000056, 0.1666666666666666574, 0.1708333333333333370, 0.1749999999999999889, 0.1791666666666666685, 0.1833333333333333204, 0.1875000000000000000, 0.1916666666666666796, 0.1958333333333333315, 0.2000000000000000111, 0.2041666666666666630, 0.2083333333333333426, 0.2124999999999999944, 0.2166666666666666741, 0.2208333333333333259, 0.2250000000000000056, 0.2291666666666666574, 0.2333333333333333370, 0.2374999999999999889, 0.2416666666666666685, 0.2458333333333333204, 0.2500000000000000000, 0.2541666666666666519, 0.2583333333333333592, 0.2625000000000000111, 0.2666666666666666630, 0.2708333333333333148, 0.2750000000000000222, 0.2791666666666666741, 0.2833333333333333259, 0.2874999999999999778, 0.2916666666666666852, 0.2958333333333333370, 0.2999999999999999889, 0.3041666666666666408, 0.3083333333333333481, 0.3125000000000000000, 0.3166666666666666519, 0.3208333333333333592, 0.3250000000000000111, 0.3291666666666666630, 0.3333333333333333148, 0.3375000000000000222, 0.3416666666666666741, 0.3458333333333333259, 0.3499999999999999778, 0.3541666666666666852, 0.3583333333333333370, 0.3624999999999999889, 0.3666666666666666408, 0.3708333333333333481, 0.3750000000000000000, 0.3791666666666666519, 0.3833333333333333592, 0.3875000000000000111, 0.3916666666666666630, 0.3958333333333333148, 0.4000000000000000222, 0.4041666666666666741, 0.4083333333333333259, 0.4124999999999999778, 0.4166666666666666852, 0.4208333333333333370, 0.4249999999999999889, 0.4291666666666666408, 0.4333333333333333481, 0.4375000000000000000, 0.4416666666666666519, 0.4458333333333333592, 0.4500000000000000111, 0.4541666666666666630, 0.4583333333333333148, 0.4625000000000000222, 0.4666666666666666741, 0.4708333333333333259, 0.4749999999999999778, 0.4791666666666666852, 0.4833333333333333370, 0.4874999999999999889, 0.4916666666666666408, 0.4958333333333333481, 0.5000000000000000000, 0.5041666666666666519, 0.5083333333333333037, 0.5124999999999999556, 0.5166666666666667185, 0.5208333333333333703, 0.5250000000000000222, 0.5291666666666666741, 0.5333333333333333259, 0.5374999999999999778, 0.5416666666666666297, 0.5458333333333332815, 0.5500000000000000444, 0.5541666666666666963, 0.5583333333333333481, 0.5625000000000000000, 0.5666666666666666519, 0.5708333333333333037, 0.5749999999999999556, 0.5791666666666667185, 0.5833333333333333703, 0.5875000000000000222, 0.5916666666666666741, 0.5958333333333333259, 0.5999999999999999778, 0.6041666666666666297, 0.6083333333333332815, 0.6125000000000000444, 0.6166666666666666963, 0.6208333333333333481, 0.6250000000000000000, 0.6291666666666666519, 0.6333333333333333037, 0.6374999999999999556, 0.6416666666666667185, 0.6458333333333333703, 0.6500000000000000222, 0.6541666666666666741, 0.6583333333333333259, 0.6624999999999999778, 0.6666666666666666297, 0.6708333333333332815, 0.6750000000000000444, 0.6791666666666666963, 0.6833333333333333481, 0.6875000000000000000, 0.6916666666666666519, 0.6958333333333333037, 0.6999999999999999556, 0.7041666666666667185, 0.7083333333333333703, 0.7125000000000000222, 0.7166666666666666741, 0.7208333333333333259, 0.7249999999999999778, 0.7291666666666666297, 0.7333333333333332815, 0.7375000000000000444, 0.7416666666666666963, 0.7458333333333333481, 0.7500000000000000000, 0.7541666666666666519, 0.7583333333333333037, 0.7624999999999999556, 0.7666666666666667185, 0.7708333333333333703, 0.7750000000000000222, 0.7791666666666666741, 0.7833333333333333259, 0.7874999999999999778, 0.7916666666666666297, 0.7958333333333332815, 0.8000000000000000444, 0.8041666666666666963, 0.8083333333333333481, 0.8125000000000000000, 0.8166666666666666519, 0.8208333333333333037, 0.8249999999999999556, 0.8291666666666667185, 0.8333333333333333703, 0.8375000000000000222, 0.8416666666666666741, 0.8458333333333333259, 0.8499999999999999778, 0.8541666666666666297, 0.8583333333333332815, 0.8625000000000000444, 0.8666666666666666963, 0.8708333333333333481, 0.8750000000000000000, 0.8791666666666666519, 0.8833333333333333037, 0.8874999999999999556, 0.8916666666666667185, 0.8958333333333333703, 0.9000000000000000222, 0.9041666666666666741, 0.9083333333333333259, 0.9124999999999999778, 0.9166666666666666297, 0.9208333333333332815, 0.9250000000000000444, 0.9291666666666666963, 0.9333333333333333481, 0.9375000000000000000, 0.9416666666666666519, 0.9458333333333333037, 0.9499999999999999556, 0.9541666666666667185, 0.9583333333333333703, 0.9625000000000000222, 0.9666666666666666741, 0.9708333333333333259, 0.9749999999999999778, 0.9791666666666666297, 0.9833333333333332815, 0.9875000000000000444, 0.9916666666666666963, 0.9958333333333333481, 1.000000000000000000 ),
 .UNSPECIFIED. ) 
 GEOMETRIC_REPRESENTATION_ITEM ( )  RATIONAL_B_SPLINE_SURFACE ( (
 ( 1.000000000000000000, 0.8660254037844387076, 1.000000000000000000, 0.8660254037844387076, 1.000000000000000000, 0.8660254037844387076, 1.000000000000000000, 0.8660254037844387076, 1.000000000000000000, 0.8660254037844387076, 1.000000000000000000, 0.8660254037844387076, 1.000000000000000000, 0.8660254037844387076, 1.000000000000000000, 0.8660254037844387076, 1.000000000000000000, 0.8660254037844387076, 1.000000000000000000, 0.8660254037844387076, 1.000000000000000000, 0.8660254037844387076, 1.000000000000000000, 0.8660254037844387076, 1.000000000000000000, 0.8660254037844387076, 1.000000000000000000, 0.8660254037844387076, 1.000000000000000000, 0.8660254037844387076, 1.000000000000000000, 0.8660254037844387076, 1.000000000000000000, 0.8660254037844387076, 1.000000000000000000, 0.8660254037844387076, 1.000000000000000000, 0.8660254037844387076, 1.000000000000000000, 0.8660254037844387076, 1.000000000000000000, 0.8660254037844387076, 1.000000000000000000, 0.8660254037844387076, 1.000000000000000000, 0.8660254037844387076, 1.000000000000000000, 0.8660254037844387076, 1.000000000000000000, 0.8660254037844387076, 1.000000000000000000, 0.8660254037844387076, 1.000000000000000000, 0.8660254037844387076, 1.000000000000000000, 0.8660254037844387076, 1.000000000000000000, 0.8660254037844387076, 1.000000000000000000, 0.8660254037844387076, 1.000000000000000000, 0.8660254037844387076, 1.000000000000000000, 0.8660254037844387076, 1.000000000000000000, 0.8660254037844387076, 1.000000000000000000, 0.8660254037844387076, 1.000000000000000000, 0.8660254037844387076, 1.000000000000000000, 0.8660254037844387076, 1.000000000000000000, 0.8660254037844387076, 1.000000000000000000, 0.8660254037844387076, 1.000000000000000000, 0.8660254037844387076, 1.000000000000000000, 0.8660254037844387076, 1.000000000000000000, 0.8660254037844387076, 1.000000000000000000, 0.8660254037844387076, 1.000000000000000000, 0.8660254037844387076, 1.000000000000000000, 0.8660254037844387076, 1.000000000000000000, 0.8660254037844387076, 1.000000000000000000, 0.8660254037844387076, 1.000000000000000000, 0.8660254037844387076, 1.000000000000000000, 0.8660254037844387076, 1.000000000000000000, 0.8660254037844387076, 1.000000000000000000, 0.8660254037844387076, 1.000000000000000000, 0.8660254037844387076, 1.000000000000000000, 0.8660254037844387076, 1.000000000000000000, 0.8660254037844387076, 1.000000000000000000, 0.8660254037844387076, 1.000000000000000000, 0.8660254037844387076, 1.000000000000000000, 0.8660254037844387076, 1.000000000000000000, 0.8660254037844387076, 1.000000000000000000, 0.8660254037844387076, 1.000000000000000000, 0.8660254037844387076, 1.000000000000000000, 0.8660254037844387076, 1.000000000000000000, 0.8660254037844387076, 1.000000000000000000, 0.8660254037844387076, 1.000000000000000000, 0.8660254037844387076, 1.000000000000000000, 0.8660254037844387076, 1.000000000000000000, 0.8660254037844387076, 1.000000000000000000, 0.8660254037844387076, 1.000000000000000000, 0.8660254037844387076, 1.000000000000000000, 0.8660254037844387076, 1.000000000000000000, 0.8660254037844387076, 1.000000000000000000, 0.8660254037844387076, 1.000000000000000000, 0.8660254037844387076, 1.000000000000000000, 0.8660254037844387076, 1.000000000000000000, 0.8660254037844387076, 1.000000000000000000, 0.8660254037844387076, 1.000000000000000000, 0.8660254037844387076, 1.000000000000000000, 0.8660254037844387076, 1.000000000000000000, 0.8660254037844387076, 1.000000000000000000, 0.8660254037844387076, 1.000000000000000000, 0.8660254037844387076, 1.000000000000000000, 0.8660254037844387076, 1.000000000000000000, 0.8660254037844387076, 1.000000000000000000, 0.8660254037844387076, 1.000000000000000000, 0.8660254037844387076, 1.000000000000000000, 0.8660254037844387076, 1.000000000000000000, 0.8660254037844387076, 1.000000000000000000, 0.8660254037844387076, 1.000000000000000000, 0.8660254037844387076, 1.000000000000000000, 0.8660254037844387076, 1.000000000000000000, 0.8660254037844387076, 1.000000000000000000, 0.8660254037844387076, 1.000000000000000000, 0.8660254037844387076, 1.000000000000000000, 0.8660254037844387076, 1.000000000000000000, 0.8660254037844387076, 1.000000000000000000, 0.8660254037844387076, 1.000000000000000000, 0.8660254037844387076, 1.000000000000000000, 0.8660254037844387076, 1.000000000000000000, 0.8660254037844387076, 1.000000000000000000, 0.8660254037844387076, 1.000000000000000000, 0.8660254037844387076, 1.000000000000000000, 0.8660254037844387076, 1.000000000000000000, 0.8660254037844387076, 1.000000000000000000, 0.8660254037844387076, 1.000000000000000000, 0.8660254037844387076, 1.000000000000000000, 0.8660254037844387076, 1.000000000000000000, 0.8660254037844387076, 1.000000000000000000, 0.8660254037844387076, 1.000000000000000000, 0.8660254037844387076, 1.000000000000000000, 0.8660254037844387076, 1.000000000000000000, 0.8660254037844387076, 1.000000000000000000, 0.8660254037844387076, 1.000000000000000000, 0.8660254037844387076, 1.000000000000000000, 0.8660254037844387076, 1.000000000000000000, 0.8660254037844387076, 1.000000000000000000, 0.8660254037844387076, 1.000000000000000000, 0.8660254037844387076, 1.000000000000000000, 0.8660254037844387076, 1.000000000000000000, 0.8660254037844387076, 1.000000000000000000, 0.8660254037844387076, 1.000000000000000000, 0.8660254037844387076, 1.000000000000000000, 0.8660254037844387076, 1.000000000000000000, 0.8660254037844387076, 1.000000000000000000, 0.8660254037844387076, 1.000000000000000000, 0.8660254037844387076, 1.000000000000000000, 0.8660254037844387076, 1.000000000000000000, 0.8660254037844387076, 1.000000000000000000, 0.8660254037844387076, 1.000000000000000000, 0.8660254037844387076, 1.000000000000000000, 0.8660254037844387076, 1.000000000000000000, 0.8660254037844387076, 1.000000000000000000, 0.8660254037844387076, 1.000000000000000000, 0.8660254037844387076, 1.000000000000000000, 0.8660254037844387076, 1.000000000000000000, 0.8660254037844387076, 1.000000000000000000, 0.8660254037844387076, 1.000000000000000000, 0.8660254037844387076, 1.000000000000000000, 0.8660254037844387076, 1.000000000000000000, 0.8660254037844387076, 1.000000000000000000, 0.8660254037844387076, 1.000000000000000000, 0.8660254037844387076, 1.000000000000000000, 0.8660254037844387076, 1.000000000000000000, 0.8660254037844387076, 1.000000000000000000, 0.8660254037844387076, 1.000000000000000000, 0.8660254037844387076, 1.000000000000000000, 0.8660254037844387076, 1.000000000000000000, 0.8660254037844387076, 1.000000000000000000, 0.8660254037844387076, 1.000000000000000000, 0.8660254037844387076, 1.000000000000000000, 0.8660254037844387076, 1.000000000000000000, 0.8660254037844387076, 1.000000000000000000, 0.8660254037844387076, 1.000000000000000000, 0.8660254037844387076, 1.000000000000000000, 0.8660254037844387076, 1.000000000000000000, 0.8660254037844387076, 1.000000000000000000, 0.8660254037844387076, 1.000000000000000000, 0.8660254037844387076, 1.000000000000000000, 0.8660254037844387076, 1.000000000000000000, 0.8660254037844387076, 1.000000000000000000, 0.8660254037844387076, 1.000000000000000000, 0.8660254037844387076, 1.000000000000000000, 0.8660254037844387076, 1.000000000000000000, 0.8660254037844387076, 1.000000000000000000, 0.8660254037844387076, 1.000000000000000000, 0.8660254037844387076, 1.000000000000000000, 0.8660254037844387076, 1.000000000000000000, 0.8660254037844387076, 1.000000000000000000, 0.8660254037844387076, 1.000000000000000000, 0.8660254037844387076, 1.000000000000000000, 0.8660254037844387076, 1.000000000000000000, 0.8660254037844387076, 1.000000000000000000, 0.8660254037844387076, 1.000000000000000000, 0.8660254037844387076, 1.000000000000000000, 0.8660254037844387076, 1.000000000000000000, 0.8660254037844387076, 1.000000000000000000, 0.8660254037844387076, 1.000000000000000000, 0.8660254037844387076, 1.000000000000000000, 0.8660254037844387076, 1.000000000000000000, 0.8660254037844387076, 1.000000000000000000, 0.8660254037844387076, 1.000000000000000000, 0.8660254037844387076, 1.000000000000000000, 0.8660254037844387076, 1.000000000000000000, 0.8660254037844387076, 1.000000000000000000, 0.8660254037844387076, 1.000000000000000000, 0.8660254037844387076, 1.000000000000000000, 0.8660254037844387076, 1.000000000000000000, 0.8660254037844387076, 1.000000000000000000, 0.8660254037844387076, 1.000000000000000000, 0.8660254037844387076, 1.000000000000000000, 0.8660254037844387076, 1.000000000000000000, 0.8660254037844387076, 1.000000000000000000, 0.8660254037844387076, 1.000000000000000000, 0.8660254037844387076, 1.000000000000000000, 0.8660254037844387076, 1.000000000000000000, 0.8660254037844387076, 1.000000000000000000, 0.8660254037844387076, 1.000000000000000000, 0.8660254037844387076, 1.000000000000000000, 0.8660254037844387076, 1.000000000000000000, 0.8660254037844387076, 1.000000000000000000, 0.8660254037844387076, 1.000000000000000000, 0.8660254037844387076, 1.000000000000000000, 0.8660254037844387076, 1.000000000000000000, 0.8660254037844387076, 1.000000000000000000, 0.8660254037844387076, 1.000000000000000000, 0.8660254037844387076, 1.000000000000000000, 0.8660254037844387076, 1.000000000000000000, 0.8660254037844387076, 1.000000000000000000, 0.8660254037844387076, 1.000000000000000000, 0.8660254037844387076, 1.000000000000000000, 0.8660254037844387076, 1.000000000000000000, 0.8660254037844387076, 1.000000000000000000, 0.8660254037844387076, 1.000000000000000000, 0.8660254037844387076, 1.000000000000000000, 0.8660254037844387076, 1.000000000000000000, 0.8660254037844387076, 1.000000000000000000, 0.8660254037844387076, 1.000000000000000000, 0.8660254037844387076, 1.000000000000000000, 0.8660254037844387076, 1.000000000000000000, 0.8660254037844387076, 1.000000000000000000, 0.8660254037844387076, 1.000000000000000000, 0.8660254037844387076, 1.000000000000000000, 0.8660254037844387076, 1.000000000000000000, 0.8660254037844387076, 1.000000000000000000, 0.8660254037844387076, 1.000000000000000000, 0.8660254037844387076, 1.000000000000000000, 0.8660254037844387076, 1.000000000000000000, 0.8660254037844387076, 1.000000000000000000, 0.8660254037844387076, 1.000000000000000000, 0.8660254037844387076, 1.000000000000000000, 0.8660254037844387076, 1.000000000000000000, 0.8660254037844387076, 1.000000000000000000, 0.8660254037844387076, 1.000000000000000000, 0.8660254037844387076, 1.000000000000000000, 0.8660254037844387076, 1.000000000000000000, 0.8660254037844387076, 1.000000000000000000, 0.8660254037844387076, 1.000000000000000000, 0.8660254037844387076, 1.000000000000000000, 0.8660254037844387076, 1.000000000000000000, 0.8660254037844387076, 1.000000000000000000, 0.8660254037844387076, 1.000000000000000000, 0.8660254037844387076, 1.000000000000000000, 0.8660254037844387076, 1.000000000000000000),
 ( 1.000000000000000000, 0.8660254037844387076, 1.000000000000000000, 0.8660254037844387076, 1.000000000000000000, 0.8660254037844387076, 1.000000000000000000, 0.8660254037844387076, 1.000000000000000000, 0.8660254037844387076, 1.000000000000000000, 0.8660254037844387076, 1.000000000000000000, 0.8660254037844387076, 1.000000000000000000, 0.8660254037844387076, 1.000000000000000000, 0.8660254037844387076, 1.000000000000000000, 0.8660254037844387076, 1.000000000000000000, 0.8660254037844387076, 1.000000000000000000, 0.8660254037844387076, 1.000000000000000000, 0.8660254037844387076, 1.000000000000000000, 0.8660254037844387076, 1.000000000000000000, 0.8660254037844387076, 1.000000000000000000, 0.8660254037844387076, 1.000000000000000000, 0.8660254037844387076, 1.000000000000000000, 0.8660254037844387076, 1.000000000000000000, 0.8660254037844387076, 1.000000000000000000, 0.8660254037844387076, 1.000000000000000000, 0.8660254037844387076, 1.000000000000000000, 0.8660254037844387076, 1.000000000000000000, 0.8660254037844387076, 1.000000000000000000, 0.8660254037844387076, 1.000000000000000000, 0.8660254037844387076, 1.000000000000000000, 0.8660254037844387076, 1.000000000000000000, 0.8660254037844387076, 1.000000000000000000, 0.8660254037844387076, 1.000000000000000000, 0.8660254037844387076, 1.000000000000000000, 0.8660254037844387076, 1.000000000000000000, 0.8660254037844387076, 1.000000000000000000, 0.8660254037844387076, 1.000000000000000000, 0.8660254037844387076, 1.000000000000000000, 0.8660254037844387076, 1.000000000000000000, 0.8660254037844387076, 1.000000000000000000, 0.8660254037844387076, 1.000000000000000000, 0.8660254037844387076, 1.000000000000000000, 0.8660254037844387076, 1.000000000000000000, 0.8660254037844387076, 1.000000000000000000, 0.8660254037844387076, 1.000000000000000000, 0.8660254037844387076, 1.000000000000000000, 0.8660254037844387076, 1.000000000000000000, 0.8660254037844387076, 1.000000000000000000, 0.8660254037844387076, 1.000000000000000000, 0.8660254037844387076, 1.000000000000000000, 0.8660254037844387076, 1.000000000000000000, 0.8660254037844387076, 1.000000000000000000, 0.8660254037844387076, 1.000000000000000000, 0.8660254037844387076, 1.000000000000000000, 0.8660254037844387076, 1.000000000000000000, 0.8660254037844387076, 1.000000000000000000, 0.8660254037844387076, 1.000000000000000000, 0.8660254037844387076, 1.000000000000000000, 0.8660254037844387076, 1.000000000000000000, 0.8660254037844387076, 1.000000000000000000, 0.8660254037844387076, 1.000000000000000000, 0.8660254037844387076, 1.000000000000000000, 0.8660254037844387076, 1.000000000000000000, 0.8660254037844387076, 1.000000000000000000, 0.8660254037844387076, 1.000000000000000000, 0.8660254037844387076, 1.000000000000000000, 0.8660254037844387076, 1.000000000000000000, 0.8660254037844387076, 1.000000000000000000, 0.8660254037844387076, 1.000000000000000000, 0.8660254037844387076, 1.000000000000000000, 0.8660254037844387076, 1.000000000000000000, 0.8660254037844387076, 1.000000000000000000, 0.8660254037844387076, 1.000000000000000000, 0.8660254037844387076, 1.000000000000000000, 0.8660254037844387076, 1.000000000000000000, 0.8660254037844387076, 1.000000000000000000, 0.8660254037844387076, 1.000000000000000000, 0.8660254037844387076, 1.000000000000000000, 0.8660254037844387076, 1.000000000000000000, 0.8660254037844387076, 1.000000000000000000, 0.8660254037844387076, 1.000000000000000000, 0.8660254037844387076, 1.000000000000000000, 0.8660254037844387076, 1.000000000000000000, 0.8660254037844387076, 1.000000000000000000, 0.8660254037844387076, 1.000000000000000000, 0.8660254037844387076, 1.000000000000000000, 0.8660254037844387076, 1.000000000000000000, 0.8660254037844387076, 1.000000000000000000, 0.8660254037844387076, 1.000000000000000000, 0.8660254037844387076, 1.000000000000000000, 0.8660254037844387076, 1.000000000000000000, 0.8660254037844387076, 1.000000000000000000, 0.8660254037844387076, 1.000000000000000000, 0.8660254037844387076, 1.000000000000000000, 0.8660254037844387076, 1.000000000000000000, 0.8660254037844387076, 1.000000000000000000, 0.8660254037844387076, 1.000000000000000000, 0.8660254037844387076, 1.000000000000000000, 0.8660254037844387076, 1.000000000000000000, 0.8660254037844387076, 1.000000000000000000, 0.8660254037844387076, 1.000000000000000000, 0.8660254037844387076, 1.000000000000000000, 0.8660254037844387076, 1.000000000000000000, 0.8660254037844387076, 1.000000000000000000, 0.8660254037844387076, 1.000000000000000000, 0.8660254037844387076, 1.000000000000000000, 0.8660254037844387076, 1.000000000000000000, 0.8660254037844387076, 1.000000000000000000, 0.8660254037844387076, 1.000000000000000000, 0.8660254037844387076, 1.000000000000000000, 0.8660254037844387076, 1.000000000000000000, 0.8660254037844387076, 1.000000000000000000, 0.8660254037844387076, 1.000000000000000000, 0.8660254037844387076, 1.000000000000000000, 0.8660254037844387076, 1.000000000000000000, 0.8660254037844387076, 1.000000000000000000, 0.8660254037844387076, 1.000000000000000000, 0.8660254037844387076, 1.000000000000000000, 0.8660254037844387076, 1.000000000000000000, 0.8660254037844387076, 1.000000000000000000, 0.8660254037844387076, 1.000000000000000000, 0.8660254037844387076, 1.000000000000000000, 0.8660254037844387076, 1.000000000000000000, 0.8660254037844387076, 1.000000000000000000, 0.8660254037844387076, 1.000000000000000000, 0.8660254037844387076, 1.000000000000000000, 0.8660254037844387076, 1.000000000000000000, 0.8660254037844387076, 1.000000000000000000, 0.8660254037844387076, 1.000000000000000000, 0.8660254037844387076, 1.000000000000000000, 0.8660254037844387076, 1.000000000000000000, 0.8660254037844387076, 1.000000000000000000, 0.8660254037844387076, 1.000000000000000000, 0.8660254037844387076, 1.000000000000000000, 0.8660254037844387076, 1.000000000000000000, 0.8660254037844387076, 1.000000000000000000, 0.8660254037844387076, 1.000000000000000000, 0.8660254037844387076, 1.000000000000000000, 0.8660254037844387076, 1.000000000000000000, 0.8660254037844387076, 1.000000000000000000, 0.8660254037844387076, 1.000000000000000000, 0.8660254037844387076, 1.000000000000000000, 0.8660254037844387076, 1.000000000000000000, 0.8660254037844387076, 1.000000000000000000, 0.8660254037844387076, 1.000000000000000000, 0.8660254037844387076, 1.000000000000000000, 0.8660254037844387076, 1.000000000000000000, 0.8660254037844387076, 1.000000000000000000, 0.8660254037844387076, 1.000000000000000000, 0.8660254037844387076, 1.000000000000000000, 0.8660254037844387076, 1.000000000000000000, 0.8660254037844387076, 1.000000000000000000, 0.8660254037844387076, 1.000000000000000000, 0.8660254037844387076, 1.000000000000000000, 0.8660254037844387076, 1.000000000000000000, 0.8660254037844387076, 1.000000000000000000, 0.8660254037844387076, 1.000000000000000000, 0.8660254037844387076, 1.000000000000000000, 0.8660254037844387076, 1.000000000000000000, 0.8660254037844387076, 1.000000000000000000, 0.8660254037844387076, 1.000000000000000000, 0.8660254037844387076, 1.000000000000000000, 0.8660254037844387076, 1.000000000000000000, 0.8660254037844387076, 1.000000000000000000, 0.8660254037844387076, 1.000000000000000000, 0.8660254037844387076, 1.000000000000000000, 0.8660254037844387076, 1.000000000000000000, 0.8660254037844387076, 1.000000000000000000, 0.8660254037844387076, 1.000000000000000000, 0.8660254037844387076, 1.000000000000000000, 0.8660254037844387076, 1.000000000000000000, 0.8660254037844387076, 1.000000000000000000, 0.8660254037844387076, 1.000000000000000000, 0.8660254037844387076, 1.000000000000000000, 0.8660254037844387076, 1.000000000000000000, 0.8660254037844387076, 1.000000000000000000, 0.8660254037844387076, 1.000000000000000000, 0.8660254037844387076, 1.000000000000000000, 0.8660254037844387076, 1.000000000000000000, 0.8660254037844387076, 1.000000000000000000, 0.8660254037844387076, 1.000000000000000000, 0.8660254037844387076, 1.000000000000000000, 0.8660254037844387076, 1.000000000000000000, 0.8660254037844387076, 1.000000000000000000, 0.8660254037844387076, 1.000000000000000000, 0.8660254037844387076, 1.000000000000000000, 0.8660254037844387076, 1.000000000000000000, 0.8660254037844387076, 1.000000000000000000, 0.8660254037844387076, 1.000000000000000000, 0.8660254037844387076, 1.000000000000000000, 0.8660254037844387076, 1.000000000000000000, 0.8660254037844387076, 1.000000000000000000, 0.8660254037844387076, 1.000000000000000000, 0.8660254037844387076, 1.000000000000000000, 0.8660254037844387076, 1.000000000000000000, 0.8660254037844387076, 1.000000000000000000, 0.8660254037844387076, 1.000000000000000000, 0.8660254037844387076, 1.000000000000000000, 0.8660254037844387076, 1.000000000000000000, 0.8660254037844387076, 1.000000000000000000, 0.8660254037844387076, 1.000000000000000000, 0.8660254037844387076, 1.000000000000000000, 0.8660254037844387076, 1.000000000000000000, 0.8660254037844387076, 1.000000000000000000, 0.8660254037844387076, 1.000000000000000000, 0.8660254037844387076, 1.000000000000000000, 0.8660254037844387076, 1.000000000000000000, 0.8660254037844387076, 1.000000000000000000, 0.8660254037844387076, 1.000000000000000000, 0.8660254037844387076, 1.000000000000000000, 0.8660254037844387076, 1.000000000000000000, 0.8660254037844387076, 1.000000000000000000, 0.8660254037844387076, 1.000000000000000000, 0.8660254037844387076, 1.000000000000000000, 0.8660254037844387076, 1.000000000000000000, 0.8660254037844387076, 1.000000000000000000, 0.8660254037844387076, 1.000000000000000000, 0.8660254037844387076, 1.000000000000000000, 0.8660254037844387076, 1.000000000000000000, 0.8660254037844387076, 1.000000000000000000, 0.8660254037844387076, 1.000000000000000000, 0.8660254037844387076, 1.000000000000000000, 0.8660254037844387076, 1.000000000000000000, 0.8660254037844387076, 1.000000000000000000, 0.8660254037844387076, 1.000000000000000000, 0.8660254037844387076, 1.000000000000000000, 0.8660254037844387076, 1.000000000000000000, 0.8660254037844387076, 1.000000000000000000, 0.8660254037844387076, 1.000000000000000000, 0.8660254037844387076, 1.000000000000000000, 0.8660254037844387076, 1.000000000000000000, 0.8660254037844387076, 1.000000000000000000, 0.8660254037844387076, 1.000000000000000000, 0.8660254037844387076, 1.000000000000000000, 0.8660254037844387076, 1.000000000000000000, 0.8660254037844387076, 1.000000000000000000, 0.8660254037844387076, 1.000000000000000000, 0.8660254037844387076, 1.000000000000000000, 0.8660254037844387076, 1.000000000000000000, 0.8660254037844387076, 1.000000000000000000, 0.8660254037844387076, 1.000000000000000000, 0.8660254037844387076, 1.000000000000000000, 0.8660254037844387076, 1.000000000000000000, 0.8660254037844387076, 1.000000000000000000, 0.8660254037844387076, 1.000000000000000000) ) ) 
 REPRESENTATION_ITEM ( '' )  SURFACE ( )  );
#9916 = DIRECTION ( 'NONE',  ( 0.000000000000000000, 0.000000000000000000, 1.000000000000000000 ) ) ;
#9917 = CARTESIAN_POINT ( 'NONE',  ( 4.575093719746353038, 1.890691655113156289, 0.8438020912069632562 ) ) ;
#9919 = CARTESIAN_POINT ( 'NONE',  ( -0.6823417656250003738, 2.030208333674753174, -1.181850606188749264 ) ) ;
#9918 = CARTESIAN_POINT ( 'NONE',  ( 7.107960593699191421, 14.55347105030218913, 9.616793498005540286 ) ) ;
#9920 = ORIENTED_EDGE ( 'NONE', *, *, #56811, .F. ) ;
#9921 = CARTESIAN_POINT ( 'NONE',  ( 4.658965222740456547, 1.322560505849355694, 1.879950767321969529 ) ) ;
#9922 = CARTESIAN_POINT ( 'NONE',  ( 6.100805936469477331, 9.101062111647635788, -1.082531754730537088 ) ) ;
#9924 = FACE_OUTER_BOUND ( 'NONE', #89852, .T. ) ;
#9923 = CARTESIAN_POINT ( 'NONE',  ( 6.387299765813869712, 6.624473612970537495, 0.000000000000000000 ) ) ;
#9925 = CARTESIAN_POINT ( 'NONE',  ( 0.2699993869635419208, 1.325028633338236839, 1.870336120953507875 ) ) ;
#9926 = CARTESIAN_POINT ( 'NONE',  ( 6.620655732516683045, 6.038298567659169613, 2.521170675138622475 ) ) ;
#9927 = CARTESIAN_POINT ( 'NONE',  ( -6.505933609711270549, 8.683618192786854095, -1.599625672291271394 ) ) ;
#9928 = CARTESIAN_POINT ( 'NONE',  ( 4.646391893561965247, -1.558859349912258718, 1.157878524630775230 ) ) ;
#9929 = VERTEX_POINT ( 'NONE', #124206 ) ;
#9930 = CARTESIAN_POINT ( 'NONE',  ( 9.869972640624258275, 10.61731562359089587, 0.000000000000000000 ) ) ;
#9931 = ORIENTED_EDGE ( 'NONE', *, *, #73977, .F. ) ;
#9932 = CARTESIAN_POINT ( 'NONE',  ( 4.675980034926481288, 1.890745994642643479, -0.2862527531290667837 ) ) ;
#9933 = CARTESIAN_POINT ( 'NONE',  ( 6.282236785375785892, -0.9178991178065436518, 1.460045492214437246 ) ) ;
#9934 = CARTESIAN_POINT ( 'NONE',  ( 6.087125082597877324, 1.679220375458953862, 1.116214469231976869 ) ) ;
#9936 = CARTESIAN_POINT ( 'NONE',  ( -11.94105721237523099, 12.69999999999999929, 1.187919463087248273 ) ) ;
#9935 = CARTESIAN_POINT ( 'NONE',  ( -7.818248136574758256, 12.27303992597924420, 0.000000000000000000 ) ) ;
#9937 = CARTESIAN_POINT ( 'NONE',  ( 0.000000000000000000, -2.384374999522042238, -3.793834371823813001 ) ) ;
#9939 = CARTESIAN_POINT ( 'NONE',  ( 6.854783864179318620, -1.365764260946045860, 1.125274747944494891 ) ) ;
#9938 = CARTESIAN_POINT ( 'NONE',  ( 2.115285117227220901, -2.027561382914280674, 0.5091250600777631474 ) ) ;
#9940 = CARTESIAN_POINT ( 'NONE',  ( 5.361953999179126740, -0.05229508359532940298, -2.015913028294749942 ) ) ;
#9942 = CARTESIAN_POINT ( 'NONE',  ( 3.029517917392979598, -1.539792254791607862, -1.698243321706040421 ) ) ;
#9941 = CARTESIAN_POINT ( 'NONE',  ( 5.411639590510088027, 6.342609606130419131, -1.199719254218452047 ) ) ;
#9943 = CARTESIAN_POINT ( 'NONE',  ( 2.747703163511563407, 0.5864964929944632699, 1.638654499222062189 ) ) ;
#9944 = CARTESIAN_POINT ( 'NONE',  ( 11.81911962874442068, 11.25710573484113475, -1.591749704452471326 ) ) ;
#9945 = CARTESIAN_POINT ( 'NONE',  ( 2.600625072996507470, 0.8205526226049694172, -1.527383475524378031 ) ) ;
#9946 = CARTESIAN_POINT ( 'NONE',  ( 1.360316468749957597, 1.776041667008106506, 0.7853790794158801436 ) ) ;
#9947 = CARTESIAN_POINT ( 'NONE',  ( 2.189708182147569460, -1.212837473668834098, -1.411683579110091458 ) ) ;
#9948 = CARTESIAN_POINT ( 'NONE',  ( 2.365899470183946640, -0.4773124685180894500, 2.117905883517334775 ) ) ;
#9949 = CARTESIAN_POINT ( 'NONE',  ( 3.116422982138194353, 1.968445132739887748, 0.4370783100892047801 ) ) ;
#9950 = CARTESIAN_POINT ( 'NONE',  ( 3.937500000000001776, 1.451031289060957574, -1.451031289061275320 ) ) ;
#9951 = CARTESIAN_POINT ( 'NONE',  ( -1.402160292154681736E-14, 0.8687500006828192678, -1.732050807568863648 ) ) ;
#9952 = CARTESIAN_POINT ( 'NONE',  ( 6.270143248794765256, 0.9928014866268529692, 1.650855525168734461 ) ) ;
#9953 = CARTESIAN_POINT ( 'NONE',  ( -1.364683531250000748, 14.60937500034140157, 0.000000000000000000 ) ) ;
#9954 = CARTESIAN_POINT ( 'NONE',  ( 3.094184762719538906, 1.412074837861827303, 1.714815191315356868 ) ) ;
#9955 = ORIENTED_EDGE ( 'NONE', *, *, #14467, .T. ) ;
#9956 = CARTESIAN_POINT ( 'NONE',  ( -1.402160292154681736E-14, 0.08750000000001964540, -1.732050807568870754 ) ) ;
#9957 = CARTESIAN_POINT ( 'NONE',  ( 9.074484886248265880, 9.481320543578137361, 0.7998128361456462443 ) ) ;
#9958 = ADVANCED_FACE ( 'NONE', ( #60171 ), #27673, .T. ) ;
#9959 = CARTESIAN_POINT ( 'NONE',  ( 0.6823417656249882723, -0.9072916663252494907, 1.181850606188755259 ) ) ;
#9960 = CARTESIAN_POINT ( 'NONE',  ( -0.03994651564155191764, -1.721383993196375251, -1.403517996469628493 ) ) ;
#9961 = CARTESIAN_POINT ( 'NONE',  ( 4.369553226407375313, -0.3375162941181614751, 1.932460123137308861 ) ) ;
#9963 = CARTESIAN_POINT ( 'NONE',  ( -5.748293942514180799, 7.729428904398431222, -1.443375672974052559 ) ) ;
#9962 = CARTESIAN_POINT ( 'NONE',  ( 2.683624340501134853, 5.218313266304903664, -1.199719254218446718 ) ) ;
#9964 = DIRECTION ( 'NONE',  ( 0.05872483221476467591, -7.952201780260630618E-17, -0.9982742078614211811 ) ) ;
#9965 = CARTESIAN_POINT ( 'NONE',  ( 5.308033872091713512, -2.252217787711635388, 0.2143866227288723780 ) ) ;
#9966 = TOROIDAL_SURFACE ( 'NONE', #154844, 11.92000000000000171, 0.08000000000000000167 ) ;
#9967 = CARTESIAN_POINT ( 'NONE',  ( 2.682143534289625375, -1.185536078076434796, -1.687771684069488076 ) ) ;
#9968 = CARTESIAN_POINT ( 'NONE',  ( -6.718228810771495141, 7.796687353110217877, 1.199719254218450271 ) ) ;
#9969 = VERTEX_POINT ( 'NONE', #191225 ) ;
#9970 = CARTESIAN_POINT ( 'NONE',  ( -1.500000000000013101, 2.702083334016155636, 0.8660254037844403729 ) ) ;
#9971 = CARTESIAN_POINT ( 'NONE',  ( 3.760894150569486616, -1.648321677062795976, -0.8843367818652316803 ) ) ;
#9972 = CARTESIAN_POINT ( 'NONE',  ( 2.619397310362530096, 0.2141275842034353338, 1.720801833696316008 ) ) ;
#9973 = CARTESIAN_POINT ( 'NONE',  ( 6.497619750234602698, -2.191128968173004843, 0.05151875470104508997 ) ) ;
#9974 = CARTESIAN_POINT ( 'NONE',  ( 0.4818276840582723652, 2.058231501447154610, -0.7964225590989246761 ) ) ;
#9975 = CARTESIAN_POINT ( 'NONE',  ( 5.613211309847925712, -1.894178568204254676, 0.4274185452872342195 ) ) ;
#9976 = ADVANCED_FACE ( 'NONE', ( #93768 ), #11412, .T. ) ;
#9978 = ORIENTED_EDGE ( 'NONE', *, *, #82531, .T. ) ;
#9977 = DIRECTION ( 'NONE',  ( -5.551115123125764829E-17, 0.000000000000000000, 1.000000000000000000 ) ) ;
#9979 = CARTESIAN_POINT ( 'NONE',  ( 0.9498425221252141393, -1.824119990893595888, -0.8596288560165299408 ) ) ;
#9980 = CARTESIAN_POINT ( 'NONE',  ( 0.1059362375676886209, 1.575662574916199210, 1.419458935296296520 ) ) ;
#9981 = DIRECTION ( 'NONE',  ( -1.276756478318932191E-15, 1.000000000000000000, -3.330669073875483426E-16 ) ) ;
#9982 = CARTESIAN_POINT ( 'NONE',  ( 6.539686446881147752, -1.556848207870220602, 1.281141925495055123 ) ) ;
#9983 = CARTESIAN_POINT ( 'NONE',  ( -9.450196763925152510, 10.98398329845622001, -1.199719254218441611 ) ) ;
#9984 = CARTESIAN_POINT ( 'NONE',  ( 5.933664784275179294, 10.07435934829639912, -0.7998128361456291469 ) ) ;
#9985 = CARTESIAN_POINT ( 'NONE',  ( 2.680951471028992117, -0.4698187958462032299, -0.1032074697909405592 ) ) ;
#9986 = CARTESIAN_POINT ( 'NONE',  ( 4.090329635444483358, -1.806102819543849769, -0.2658631594732660530 ) ) ;
#9987 = CARTESIAN_POINT ( 'NONE',  ( 1.606762454812577179, -0.7948807482080816333, -2.058825234118460745 ) ) ;
#9988 = ORIENTED_EDGE ( 'NONE', *, *, #175486, .T. ) ;
#9989 = CARTESIAN_POINT ( 'NONE',  ( -3.160459205317013076, 6.701303149596211206, -0.7216878364870458196 ) ) ;
#9990 = UNCERTAINTY_MEASURE_WITH_UNIT (LENGTH_MEASURE( 1.000000000000000082E-05 ), #73905, 'distance_accuracy_value', 'NONE');
#9991 = CARTESIAN_POINT ( 'NONE',  ( 1.642778471875001811, -2.880208332855377584, 2.845375778867859751 ) ) ;
#9992 = CARTESIAN_POINT ( 'NONE',  ( -8.182509401047415309, 9.505014708432145909, 1.199719254218462483 ) ) ;
#9993 = CARTESIAN_POINT ( 'NONE',  ( 0.8440173190735723585, -1.284739210308597723, -1.558479848626155961 ) ) ;
#9994 = CARTESIAN_POINT ( 'NONE',  ( -1.274579945453880425, 3.984756441945468630, 0.4827076737218306546 ) ) ;
#9995 = VERTEX_POINT ( 'NONE', #26601 ) ;
#9996 = CARTESIAN_POINT ( 'NONE',  ( -3.797165540279144214, 6.587721009371067638, 1.199719254218452935 ) ) ;
#9997 = CARTESIAN_POINT ( 'NONE',  ( 2.535811996613965391, 1.140603387277869585, 1.470366759043324478 ) ) ;
#9998 = CARTESIAN_POINT ( 'NONE',  ( 2.679707916995359263, 6.278076336469897711, -0.7998128361456291469 ) ) ;
#9999 = DIRECTION ( 'NONE',  ( -0.000000000000000000, -0.000000000000000000, 1.000000000000000000 ) ) ;
#10000 = EDGE_LOOP ( 'NONE', ( #108378, #59114, #125054, #30437 ) ) ;
#10001 = EDGE_LOOP ( 'NONE', ( #60368, #63576, #62075, #112237 ) ) ;
#10002 =( BOUNDED_CURVE ( )  B_SPLINE_CURVE ( 2, ( #183760, #167517, #32186, #709, #65713, #15909, #67843 ),
 .UNSPECIFIED., .F., .T. ) 
 B_SPLINE_CURVE_WITH_KNOTS ( ( 3, 2, 2, 3 ),
 ( 0.2321428571428570953, 0.2380952380952381098, 0.2440476190476191798, 0.2500000000000002220 ),
 .UNSPECIFIED. ) 
 CURVE ( )  GEOMETRIC_REPRESENTATION_ITEM ( )  RATIONAL_B_SPLINE_CURVE ( ( 1.000000000000001332, 0.8660254037844374864, 1.000000000000000000, 0.8660254037844387076, 1.000000000000000000, 0.8660254037844337116, 1.000000000000005107 ) ) 
 REPRESENTATION_ITEM ( '' )  );
#10003 = CARTESIAN_POINT ( 'NONE',  ( -7.808606406466886973, 11.19745900993164511, 1.199719254218453823 ) ) ;
#10004 = CARTESIAN_POINT ( 'NONE',  ( 3.984828715814022981, -0.1808549858164226476, -1.816707794649790708 ) ) ;
#10006 = CARTESIAN_POINT ( 'NONE',  ( -5.768665591941109838, 6.232869020846472097, -1.039980349891131972 ) ) ;
#10005 = CARTESIAN_POINT ( 'NONE',  ( -4.197131071882288289, 7.054347462908075350, -1.199719254218455378 ) ) ;
#10007 = CARTESIAN_POINT ( 'NONE',  ( 5.413027408713817046, 7.651055653456078076, -1.328921179265474262 ) ) ;
#10008 = CARTESIAN_POINT ( 'NONE',  ( 0.9656601056488465229, 1.412931828189394556, 1.004572000263863840 ) ) ;
#10009 = CARTESIAN_POINT ( 'NONE',  ( 5.454971364017034752, 0.3553261626877933788, -1.806350769464920569 ) ) ;
#10010 = CARTESIAN_POINT ( 'NONE',  ( 3.862222655691281759, 2.290455142492770602, -0.2811034502991411888 ) ) ;
#10011 = CARTESIAN_POINT ( 'NONE',  ( 5.011674058906918638, 5.875983152593414971, 1.199719254218452047 ) ) ;
#10012 = CARTESIAN_POINT ( 'NONE',  ( 0.4388362695032248517, 0.3497011122354178325, 2.030714657000245893 ) ) ;
#10013 = CARTESIAN_POINT ( 'NONE',  ( 7.481401836642521452, 7.622723652371411696, 1.040834085586084257E-14 ) ) ;
#10014 = CARTESIAN_POINT ( 'NONE',  ( 2.120557540808472918, 0.002150750411172245441, 1.942234967187633110 ) ) ;
#10015 = CIRCLE ( 'NONE', #162180, 0.07999999999999990452 ) ;
#10016 = CARTESIAN_POINT ( 'NONE',  ( 5.431170548343748905, 1.126412363255802518, 2.003379520639406497 ) ) ;
#10017 = DIRECTION ( 'NONE',  ( 8.638326563840814399E-31, 0.000000000000000000, 1.000000000000000000 ) ) ;
#10018 = CARTESIAN_POINT ( 'NONE',  ( -5.191846479390389568, 5.021852078902356631, 0.7998128361456281477 ) ) ;
#10019 = CARTESIAN_POINT ( 'NONE',  ( 4.557402362779487959, 0.4096945884842878582, -1.825068887194372991 ) ) ;
#10022 = ADVANCED_FACE ( 'NONE', ( #42888 ), #108997, .T. ) ;
#10021 = CARTESIAN_POINT ( 'NONE',  ( -4.447956913735107598, 7.346977611736363656, 1.199719254218452935 ) ) ;
#10020 = CARTESIAN_POINT ( 'NONE',  ( 2.496234081663367022, -0.9796988711565941532, 1.642222327643327873 ) ) ;
#10023 = CARTESIAN_POINT ( 'NONE',  ( 3.809358915828209735, 1.892446193107431451, 1.135094405146239049 ) ) ;
#10024 = CARTESIAN_POINT ( 'NONE',  ( -1.225000000000038058, 0.08333333401614038960, 0.7072540797572558491 ) ) ;
#10025 = CARTESIAN_POINT ( 'NONE',  ( 6.983263157960404754, -0.005959781318053481922, 2.045923054782183392 ) ) ;
#10026 = CARTESIAN_POINT ( 'NONE',  ( 4.190878879955609371, 7.903459436674603822, -0.7216878364870338292 ) ) ;
#10027 = CARTESIAN_POINT ( 'NONE',  ( -7.065207446052822249, 7.415365906582643163, -0.7216878364870338292 ) ) ;
#10028 = CARTESIAN_POINT ( 'NONE',  ( 1.387891646316425476, -0.8902153388929586741, 1.759007621864362214 ) ) ;
#10029 = EDGE_CURVE ( 'NONE', #84082, #144349, #111127, .T. ) ;
#10030 = CARTESIAN_POINT ( 'NONE',  ( 2.485774399949276070, 2.109797628256422364, -0.9350972159218959856 ) ) ;
#10031 = CARTESIAN_POINT ( 'NONE',  ( 1.996468121258226924, 1.940055844723225009, 0.2909814450420752929 ) ) ;
#10032 = CARTESIAN_POINT ( 'NONE',  ( -1.580000000000001625, -1.099999999999976108, -2.499999999999989342 ) ) ;
#10033 = CARTESIAN_POINT ( 'NONE',  ( 6.139522945012108934, 1.907909241145373525, -0.7841019685283256990 ) ) ;
#10034 = CARTESIAN_POINT ( 'NONE',  ( 3.050221373394638835, 6.502416002361635528, 0.000000000000000000 ) ) ;
#10035 = CARTESIAN_POINT ( 'NONE',  ( 3.731657894805060938, 0.6748485617756972976, -1.900415309456899182 ) ) ;
#10036 = CARTESIAN_POINT ( 'NONE',  ( 3.902768115887398803, 5.646591783325653147, -1.599625672291269396 ) ) ;
#10037 = ORIENTED_EDGE ( 'NONE', *, *, #197437, .F. ) ;
#10038 = CARTESIAN_POINT ( 'NONE',  ( 4.382046175016578005, -2.016188710442788246, -0.04465648322755921829 ) ) ;
#10039 = CARTESIAN_POINT ( 'NONE',  ( -8.646349277213090545, 11.11049346154719508, 1.599625672291269396 ) ) ;
#10040 = LINE ( 'NONE', #109757, #116756 ) ;
#10041 = CARTESIAN_POINT ( 'NONE',  ( 4.163088478618747692E-16, 0.06547992991065912372, 3.399419719642636561 ) ) ;
#10042 = CARTESIAN_POINT ( 'NONE',  ( 9.694243528971124846, 11.26870452434320491, 1.199719254218450271 ) ) ;
#10043 = CARTESIAN_POINT ( 'NONE',  ( 2.237404288245536943, -0.1031769000767470690, -2.168708286310920386 ) ) ;
#10044 = PRESENTATION_STYLE_ASSIGNMENT (( #76118 ) ) ;
#10045 = DIRECTION ( 'NONE',  ( 0.1431542804991169926, 0.000000000000000000, 0.9897003849523248187 ) ) ;
#10046 = CARTESIAN_POINT ( 'NONE',  ( 2.038157526861613889, 1.849479306444936411, 0.2792354855166642724 ) ) ;
#10047 = CIRCLE ( 'NONE', #37733, 0.8299999999999999600 ) ;
#10048 = CARTESIAN_POINT ( 'NONE',  ( 0.4036811037357163623, -0.5522049309486184443, 1.985320814919430132 ) ) ;
#10050 = CARTESIAN_POINT ( 'NONE',  ( 6.827182134110200806, 1.308106637204756728, 1.828351192278207638 ) ) ;
#10049 = CARTESIAN_POINT ( 'NONE',  ( 0.07775346131142638062, 0.2253410668615995205, -2.322482355083537175 ) ) ;
#10051 = CARTESIAN_POINT ( 'NONE',  ( -0.6823417656250246877, 0.05104166700808931978, 1.181850606188755259 ) ) ;
#10052 = CARTESIAN_POINT ( 'NONE',  ( 3.615784255950851289, -0.5524401208748200842, 1.830756043982272097 ) ) ;
#10053 = CARTESIAN_POINT ( 'NONE',  ( 4.557331473417879586, 0.3865553534455662965, -1.726927170965624647 ) ) ;
#10054 = CARTESIAN_POINT ( 'NONE',  ( 1.383307607624170155, 0.1396965592646744470, -1.907218110473147155 ) ) ;
#10055 = CARTESIAN_POINT ( 'NONE',  ( -4.497554271431319250, 6.270232621468402989, -1.599625672291256295 ) ) ;
#10057 = CARTESIAN_POINT ( 'NONE',  ( -0.2411972340276360705, -0.002466136893084554509, -1.900252416837118430 ) ) ;
#10056 = CARTESIAN_POINT ( 'NONE',  ( -2.810282979782591006, 6.500690253046801814, 0.000000000000000000 ) ) ;
#10058 = AXIS2_PLACEMENT_3D ( 'NONE', #199237, #133233, #99634 ) ;
#10059 = CARTESIAN_POINT ( 'NONE',  ( -0.7500000000000006661, 0.3583333333333563187, -1.299038105676652011 ) ) ;
#10060 = CARTESIAN_POINT ( 'NONE',  ( 0.5728211633247158874, 1.428863753495920763, -1.498466819491943269 ) ) ;
#10061 = CARTESIAN_POINT ( 'NONE',  ( -1.364683531250014514, -0.9489583329919112353, -0.7879004041258359514 ) ) ;
#10062 = CARTESIAN_POINT ( 'NONE',  ( 6.104356062600288624, -0.6750377415852754082, -1.744797942764392928 ) ) ;
#10063 = CARTESIAN_POINT ( 'NONE',  ( 1.611646134362737959, -1.812087876328593916, 0.2219229778191167957 ) ) ;
#10065 = CARTESIAN_POINT ( 'NONE',  ( 4.611577566919329740, 8.352668595566711929, -0.2595669225248058432 ) ) ;
#10064 = CARTESIAN_POINT ( 'NONE',  ( 5.813141826352885566, 1.944573597739504889, 1.043518232037063287 ) ) ;
#10066 = CARTESIAN_POINT ( 'NONE',  ( -1.364683531250014514, -0.9697916663252473812, 0.7879004041258379498 ) ) ;
#10067 = CARTESIAN_POINT ( 'NONE',  ( 3.385269252200762580, 0.04793456357342047724, 2.062272590435239028 ) ) ;
#10068 = CARTESIAN_POINT ( 'NONE',  ( -6.042130013184518589, 10.20090211535728031, -0.7998128361456291469 ) ) ;
#10069 = CARTESIAN_POINT ( 'NONE',  ( 7.214910300766615769, 11.56914578420308715, -0.7998128361456291469 ) ) ;
#10070 = CARTESIAN_POINT ( 'NONE',  ( 1.264548378739733581, 3.788599454610471984, -0.5006372017796714147 ) ) ;
#10071 = CARTESIAN_POINT ( 'NONE',  ( 0.1929406647830470833, -0.4748886411078504510, -2.116594070111991410 ) ) ;
#10072 = CARTESIAN_POINT ( 'NONE',  ( 6.530187263637528439, 7.647581891445782709, -1.199719254218452047 ) ) ;
#10073 = VERTEX_POINT ( 'NONE', #160883 ) ;
#10074 = CARTESIAN_POINT ( 'NONE',  ( 5.020015195830264787, 2.048331326439792210, -0.3003445753073652469 ) ) ;
#10075 = CARTESIAN_POINT ( 'NONE',  ( -1.364683531250014514, 0.3010416670080866552, -0.7879004041258359514 ) ) ;
#10076 = CARTESIAN_POINT ( 'NONE',  ( 2.847126979364768218, -1.798887516807456954, 1.198237791991546564 ) ) ;
#10077 = CARTESIAN_POINT ( 'NONE',  ( -4.603881723180708541, 8.384271979250147666, 0.04571010684512218092 ) ) ;
#10079 = CARTESIAN_POINT ( 'NONE',  ( 2.101936620064443151, 0.7537240185569763495, -1.811501260397870405 ) ) ;
#10078 = CARTESIAN_POINT ( 'NONE',  ( 2.701824437540679469, 1.429832853698081108, 1.426684077065028422 ) ) ;
#10080 = B_SPLINE_CURVE_WITH_KNOTS ( 'NONE', 3,
 ( #94114, #8561, #173226, #89846, #77827, #160155, #11753, #206759, #109347, #40015 ),
 .UNSPECIFIED., .F., .F.,
 ( 4, 1, 1, 1, 1, 1, 1, 4 ),
 ( 0.000000000000000000, 0.09123828766142533242, 0.1830323254715014447, 0.2554767746403809325, 0.3605042187413262100, 0.5206858269973231312, 0.7335850107976985557, 1.000000000000000000 ),
 .UNSPECIFIED. ) ;
#10081 = CARTESIAN_POINT ( 'NONE',  ( 6.620655732516607550, 2.431211045237289703, 2.455576803978098521 ) ) ;
#10084 = CARTESIAN_POINT ( 'NONE',  ( 5.775410249741494972, 8.721433810464993996, -1.082531754730537088 ) ) ;
#10083 = CARTESIAN_POINT ( 'NONE',  ( -1.737499999999997824, -0.9916666666666684726, 3.009438278150925683 ) ) ;
#10082 =( LENGTH_UNIT ( ) NAMED_UNIT ( * ) SI_UNIT ( .MILLI., .METRE. ) );
#10085 = CARTESIAN_POINT ( 'NONE',  ( -7.282664789195997912, 8.525472337930658284, 1.199719254218452047 ) ) ;
#10086 = CARTESIAN_POINT ( 'NONE',  ( 1.077361674225948418, 1.530160568918725872, 1.313541346884481209 ) ) ;
#10088 = CARTESIAN_POINT ( 'NONE',  ( 5.987848539424092564, -2.180829346447300310, -0.2163489798085171945 ) ) ;
#10087 = CARTESIAN_POINT ( 'NONE',  ( -6.403528624356093601, 6.365204904703887223, 1.040834085586084257E-14 ) ) ;
#10089 = CARTESIAN_POINT ( 'NONE',  ( 0.7499999999999920064, 5.514583334016151639, 1.299038105676669330 ) ) ;
#10090 = CARTESIAN_POINT ( 'NONE',  ( 4.816621285000030284, -0.6497861859515661198, -1.798733151862880186 ) ) ;
#10091 = CARTESIAN_POINT ( 'NONE',  ( -4.437596350374534815, 4.071617251725375475, -0.7998128361456221525 ) ) ;
#10092 = CARTESIAN_POINT ( 'NONE',  ( 6.114364089638795186, 7.196141528409145671, 1.082531754730558626 ) ) ;
#10094 = CARTESIAN_POINT ( 'NONE',  ( 3.357046149680571023, 0.04665894677104672622, -2.016035383867887276 ) ) ;
#10093 = CARTESIAN_POINT ( 'NONE',  ( -8.419250203962027612, 11.80591375705560608, 1.082531754730549967 ) ) ;
#10095 = CARTESIAN_POINT ( 'NONE',  ( 0.6823417656249969321, 13.83854166700806942, -1.181850606188757036 ) ) ;
#10096 = CARTESIAN_POINT ( 'NONE',  ( 5.754863291335100328, -1.356889945763246841, 1.064653683861387812 ) ) ;
#10097 = CARTESIAN_POINT ( 'NONE',  ( 7.225569521440261767, 7.394528961293920233, -0.7998128361456341429 ) ) ;
#10098 = CARTESIAN_POINT ( 'NONE',  ( 4.369805582306193870, 3.992528022312320957, 1.214306433183764966E-14 ) ) ;
#10099 = CARTESIAN_POINT ( 'NONE',  ( -11.41108574530281494, 11.25836855377625589, -3.405883542057589253 ) ) ;
#10100 = CARTESIAN_POINT ( 'NONE',  ( 4.833189656263336964, -1.710893631887340227, 0.7565425265826587475 ) ) ;
#10101 = CARTESIAN_POINT ( 'NONE',  ( -5.608478439449225306, 5.609308656285654671, -0.4224404339892348093 ) ) ;
#10102 = CARTESIAN_POINT ( 'NONE',  ( 0.5497785174156319954, 1.531638494488884339, 1.392999266381978130 ) ) ;
#10103 = CIRCLE ( 'NONE', #17033, 4.624999999999993783 ) ;
#10104 = CARTESIAN_POINT ( 'NONE',  ( 1.841222038795641122E-16, 2.000000000000001776, 2.750000000000008438 ) ) ;
#10105 = EDGE_LOOP ( 'NONE', ( #185826, #183591, #177194, #70564 ) ) ;
#10106 = CARTESIAN_POINT ( 'NONE',  ( 5.900986446306966116, -0.2725449506757338658, -1.790729509878173475 ) ) ;
#10107 = CARTESIAN_POINT ( 'NONE',  ( 5.174371902270911150, 6.065797303184739420, 1.199719254218452047 ) ) ;
#10108 = DIRECTION ( 'NONE',  ( -1.276756478318932585E-15, 1.000000000000000000, -1.665334536937738262E-16 ) ) ;
#10109 = CARTESIAN_POINT ( 'NONE',  ( 0.1229364404080907497, 1.576183056183463993, 0.8927909362536170512 ) ) ;
#10110 = CARTESIAN_POINT ( 'NONE',  ( 4.678972410047582464, 8.472901888448573615, -0.7216878364870357165 ) ) ;
#10111 = CARTESIAN_POINT ( 'NONE',  ( 11.99427146011852763, 7.649902820345518606, -0.4312808647509002724 ) ) ;
#10112 = VERTEX_POINT ( 'NONE', #123154 ) ;
#10114 = CARTESIAN_POINT ( 'NONE',  ( 7.670162217029129259, 9.971608557999250166, 1.599625672291281386 ) ) ;
#10113 = CARTESIAN_POINT ( 'NONE',  ( 0.6429252097494702056, -0.2364460082661112295, -1.947484529462916836 ) ) ;
#10115 = CARTESIAN_POINT ( 'NONE',  ( 4.692942998425689183, 1.668811738553135804, 0.9403632788237480389 ) ) ;
#10116 = CARTESIAN_POINT ( 'NONE',  ( -4.038971567461725698, 3.986455684509185193, -0.5169845646830102392 ) ) ;
#10117 = FILL_AREA_STYLE ('',( #12248 ) ) ;
#10119 = ORIENTED_EDGE ( 'NONE', *, *, #97268, .F. ) ;
#10118 = CARTESIAN_POINT ( 'NONE',  ( 5.043269954603547767, 4.986162489899998995, -0.7216878364870197293 ) ) ;
#10120 = CARTESIAN_POINT ( 'NONE',  ( -8.731087737520713432, 10.24898578427137963, 1.082531754730558626 ) ) ;
#10121 = CARTESIAN_POINT ( 'NONE',  ( 2.360439101503517101, 0.9236781337260313585, 1.954550705658316678 ) ) ;
#10122 = CARTESIAN_POINT ( 'NONE',  ( -4.390861645979385663, 6.216034235099629157, -1.599625672291271394 ) ) ;
#10123 = CARTESIAN_POINT ( 'NONE',  ( 6.861835142292135536, 9.098836647464588978, 1.443375672974065660 ) ) ;
#10124 = CARTESIAN_POINT ( 'NONE',  ( -0.1401555495076401980, -1.643345231473653190, -1.339971704266910812 ) ) ;
#10125 = CARTESIAN_POINT ( 'NONE',  ( 4.840742024777624053, 0.3130767520662172121, 1.798364180563789327 ) ) ;
#10126 = CARTESIAN_POINT ( 'NONE',  ( 8.811349696246875141, 13.35371418836173696, 7.678511501153402641 ) ) ;
#10127 = CARTESIAN_POINT ( 'NONE',  ( 1.598833994113032730, 1.614015922016404536, -1.131664812120122487 ) ) ;
#10128 = CARTESIAN_POINT ( 'NONE',  ( 3.937688585161042809, -1.828529804631402023, 0.5600222464785462595 ) ) ;
#10129 = VERTEX_POINT ( 'NONE', #40745 ) ;
#10130 = CARTESIAN_POINT ( 'NONE',  ( -5.995491898843540390, 14.48115541367089953, -10.40458799043917359 ) ) ;
#10131 = CARTESIAN_POINT ( 'NONE',  ( 3.420317264040674932, 0.8831254867164675115, 1.760515127234823840 ) ) ;
#10132 = VERTEX_POINT ( 'NONE', #150779 ) ;
#10133 = CARTESIAN_POINT ( 'NONE',  ( 5.706574293107399498, 1.714631337756479912, 0.9119185223999854983 ) ) ;
#10134 = ORIENTED_EDGE ( 'NONE', *, *, #77070, .F. ) ;
#10135 = CARTESIAN_POINT ( 'NONE',  ( -5.261446130555064826, 8.296048364692991228, 1.199719254218452935 ) ) ;
#10137 = CARTESIAN_POINT ( 'NONE',  ( 6.398696098476772676, -2.079943653215409416, -0.4123558718646391785 ) ) ;
#10136 = CARTESIAN_POINT ( 'NONE',  ( -5.147255595043616516, 6.034161611419515125, 1.199719254218452935 ) ) ;
#10138 = CARTESIAN_POINT ( 'NONE',  ( 7.038091138825468107, 8.344099429118761790, -1.082531754730548412 ) ) ;
#10139 = CARTESIAN_POINT ( 'NONE',  ( 4.318947422894989785, 1.476084237994702786, -1.215703867470045774 ) ) ;
#10140 = CARTESIAN_POINT ( 'NONE',  ( -0.9040546642425820734, 15.46908217946011455, -11.99999999974921394 ) ) ;
#10141 = CARTESIAN_POINT ( 'NONE',  ( 0.1302870565101400258, -1.360178740744298675, -1.738515015553928400 ) ) ;
#10142 = VECTOR ( 'NONE', #195719, 1000.000000000000000 ) ;
#10143 = CARTESIAN_POINT ( 'NONE',  ( 7.661067326845555137, -5.325441678136409784, 7.893838479094928751 ) ) ;
#10144 = CARTESIAN_POINT ( 'NONE',  ( 5.549481842319204716, -1.818904971374595503, 0.8629315129762565872 ) ) ;
#10145 = CARTESIAN_POINT ( 'NONE',  ( 0.08058608058607655278, -8.407420853759283830, 10.99970480893082225 ) ) ;
#10146 = CARTESIAN_POINT ( 'NONE',  ( 5.936143289257818978, 0.8957264799932495025, -1.590785280889392528 ) ) ;
#10147 = CARTESIAN_POINT ( 'NONE',  ( 1.469279758060072938, 1.824989553406907383, 0.9776941847434923449 ) ) ;
#10148 = CARTESIAN_POINT ( 'NONE',  ( -6.684333426737305572, 7.757142738403693727, -1.199719254218446718 ) ) ;
#10149 = CARTESIAN_POINT ( 'NONE',  ( -5.779986827147332029, 7.257483166437310729, -1.191988747605486010 ) ) ;
#10150 = B_SPLINE_CURVE_WITH_KNOTS ( 'NONE', 3,
 ( #189465, #58404, #23754, #192645 ),
 .UNSPECIFIED., .F., .F.,
 ( 4, 4 ),
 ( 0.000000000000000000, 0.0002909236271752624683 ),
 .UNSPECIFIED. ) ;
#10151 = CARTESIAN_POINT ( 'NONE',  ( -5.764827401431626974, 7.068052664419927744, -2.440105445505980075 ) ) ;
#10152 = CARTESIAN_POINT ( 'NONE',  ( 6.631728656526095556, -1.223761959379562114, -1.414937998750566361 ) ) ;
#10153 = CARTESIAN_POINT ( 'NONE',  ( 6.471319392424407901, 6.444294134116939077, 0.7998128361456341429 ) ) ;
#10154 = DIRECTION ( 'NONE',  ( -0.000000000000000000, 1.000000000000000000, -0.000000000000000000 ) ) ;
#10155 = EDGE_CURVE ( 'NONE', #31187, #101925, #6748, .T. ) ;
#10156 = CARTESIAN_POINT ( 'NONE',  ( 4.095971805104276164, 7.792734516014745871, 0.7216878364870257245 ) ) ;
#10157 = LINE ( 'NONE', #159624, #161826 ) ;
#10158 = CARTESIAN_POINT ( 'NONE',  ( 0.6823417656249969321, 12.08854166700806765, -1.181850606188757036 ) ) ;
#10159 = CARTESIAN_POINT ( 'NONE',  ( -3.411848212133334446, 7.132240014130862171, 0.7998128361456341429 ) ) ;
#10161 = CARTESIAN_POINT ( 'NONE',  ( -6.957269102468015554, 8.145844036748005834, 1.199719254218452047 ) ) ;
#10160 = CARTESIAN_POINT ( 'NONE',  ( 1.814759087649916003, 3.975067388631702059, -0.4606438099578838985 ) ) ;
#10163 = ADVANCED_FACE ( 'NONE', ( #183253 ), #132422, .F. ) ;
#10162 = PRESENTATION_LAYER_ASSIGNMENT (  '', '', ( #68896 ) ) ;
#10164 = CARTESIAN_POINT ( 'NONE',  ( 4.799290796133064418, 1.190976682166387413, -1.260762715536057899 ) ) ;
#10165 = CARTESIAN_POINT ( 'NONE',  ( -5.928993247877788697, 5.811580298812519807, 0.7998128361456341429 ) ) ;
#10166 = CARTESIAN_POINT ( 'NONE',  ( 2.360293207207576849, -2.069885933316969240, 0.04650197241463926989 ) ) ;
#10167 = CARTESIAN_POINT ( 'NONE',  ( 3.304427501237202414, 1.341129661294770958, -1.638326698864990716 ) ) ;
#10168 = CARTESIAN_POINT ( 'NONE',  ( 8.925345196497941558, 9.307324238869423283, 1.040834085586084257E-14 ) ) ;
#10169 = CARTESIAN_POINT ( 'NONE',  ( -0.6823417656250212460, 3.301041667008085323, 1.181850606188767472 ) ) ;
#10170 = CARTESIAN_POINT ( 'NONE',  ( 1.762491902426995605, -0.7040454445105134296, -1.839503732180563844 ) ) ;
#10171 = CARTESIAN_POINT ( 'NONE',  ( 5.529887635128906354, 6.401445659467410287, 1.229860404580757072 ) ) ;
#10172 = CARTESIAN_POINT ( 'NONE',  ( 4.365362273920250225, 5.155639410070820716, 1.082531754730560403 ) ) ;
#10174 = CARTESIAN_POINT ( 'NONE',  ( -0.4645846211130816306, -7.563986176625375535, -10.12536109763332526 ) ) ;
#10173 = CARTESIAN_POINT ( 'NONE',  ( 3.475000000000000533, -1.604166666666667629, 2.006292185433948827 ) ) ;
#10175 = CARTESIAN_POINT ( 'NONE',  ( 3.767766022312348362, 1.272560033980062455, 1.906398719306565681 ) ) ;
#10176 = CARTESIAN_POINT ( 'NONE',  ( 0.5041868517345666767, -0.6120625888205477594, -1.720162557568189809 ) ) ;
#10177 = CARTESIAN_POINT ( 'NONE',  ( 4.505052181490820651, 8.477920988373101707, -0.7998128361456381397 ) ) ;
#10178 = CARTESIAN_POINT ( 'NONE',  ( 5.463572716182812705, 9.317992568947877530, 0.7216878364870438212 ) ) ;
#10179 = CARTESIAN_POINT ( 'NONE',  ( -8.134002093194872884, 11.57708731111429401, 1.199719254218453823 ) ) ;
#10180 =( BOUNDED_CURVE ( )  B_SPLINE_CURVE ( 2, ( #213393, #68202, #50917, #65017, #165735, #162554, #67133, #33594, #17322 ),
 .UNSPECIFIED., .F., .T. ) 
 B_SPLINE_CURVE_WITH_KNOTS ( ( 3, 2, 2, 2, 3 ),
 ( 0.1093749999999998473, 0.1145833333333333287, 0.1250000000000000000, 0.1354166666666666574, 0.1406250000000001943 ),
 .UNSPECIFIED. ) 
 CURVE ( )  GEOMETRIC_REPRESENTATION_ITEM ( )  RATIONAL_B_SPLINE_CURVE ( ( 0.9330127018922194093, 0.9330127018922174109, 1.000000000000000000, 0.8660254037844387076, 1.000000000000000000, 0.8660254037844387076, 1.000000000000000000, 0.9330127018922168558, 0.9330127018922194093 ) ) 
 REPRESENTATION_ITEM ( '' )  );
#10181 = CARTESIAN_POINT ( 'NONE',  ( 1.406495263175694399, -2.003875642784687994, -0.1933051647188162026 ) ) ;
#10182 = CARTESIAN_POINT ( 'NONE',  ( 2.412880707699780025, -1.519673801815585312, 1.240645658979570909 ) ) ;
#10183 = CARTESIAN_POINT ( 'NONE',  ( -8.830438121202295321, 9.196599317691152464, -0.7998128361456291469 ) ) ;
#10184 = CARTESIAN_POINT ( 'NONE',  ( -5.819474248763749635, 7.812472595022922128, -1.599625672291256295 ) ) ;
#10185 = CARTESIAN_POINT ( 'NONE',  ( 0.07536363704235825300, -0.001874865094115065866, -2.144269471569634433 ) ) ;
#10187 = CARTESIAN_POINT ( 'NONE',  ( 3.555294528146099697, 0.4307136429906773256, -1.716485385381610662 ) ) ;
#10186 = CARTESIAN_POINT ( 'NONE',  ( 5.384749270845579083, 1.844215719714219492, -0.9846981469126301345 ) ) ;
#10188 = CARTESIAN_POINT ( 'NONE',  ( -9.117697077659501659, 15.00000000000574829, 7.299999999990889776 ) ) ;
#10189 = CARTESIAN_POINT ( 'NONE',  ( 6.035170563425642953, -1.656272789430097703, -1.584931405618497990 ) ) ;
#10190 = CARTESIAN_POINT ( 'NONE',  ( 5.279165678654878846, 1.172930834070673889, 1.285866470927458094 ) ) ;
#10191 = CARTESIAN_POINT ( 'NONE',  ( 7.507464373665139412, 9.781794407407920389, 1.599625672291281386 ) ) ;
#10192 = CARTESIAN_POINT ( 'NONE',  ( 5.748750450937779810, 2.265299150918558269, -0.3897391249057541862 ) ) ;
#10193 = CARTESIAN_POINT ( 'NONE',  ( 2.971087601478215934, 6.563059292275168488, 0.4682405089187134384 ) ) ;
#10194 = CARTESIAN_POINT ( 'NONE',  ( 5.061730935934568798, 1.440722419422343803, -0.9642406207952100017 ) ) ;
#10195 = CARTESIAN_POINT ( 'NONE',  ( 5.670445308384678640, -0.9712495897680500923, -1.941886722523916253 ) ) ;
#10196 = CARTESIAN_POINT ( 'NONE',  ( -0.4019237886466871523, 11.19866454968462754, -1.499999999999998668 ) ) ;
#10197 = CARTESIAN_POINT ( 'NONE',  ( 6.509000000000012776, 0.004788705324892602276, 2.000274819378269342 ) ) ;
#10198 = CARTESIAN_POINT ( 'NONE',  ( 4.781250000000003553, 0.7852924748302358982, 1.895863743163977100 ) ) ;
#10199 = CARTESIAN_POINT ( 'NONE',  ( -1.499999999999997780, 5.181250000682820378, 1.214306433183764966E-14 ) ) ;
#10200 = CARTESIAN_POINT ( 'NONE',  ( 3.821244781301834426, -0.1429285350797465659, 1.921155437072092242 ) ) ;
#10201 = CARTESIAN_POINT ( 'NONE',  ( 1.499999999999997113, 11.17708333401612819, -0.8660254037844378194 ) ) ;
#10202 = CARTESIAN_POINT ( 'NONE',  ( 0.1885310067011408963, 1.284270987554763765, 1.812239126532013689 ) ) ;
#10203 = EDGE_LOOP ( 'NONE', ( #213866, #160272, #58142, #76607 ) ) ;
#10204 = CARTESIAN_POINT ( 'NONE',  ( 0.7499999999999920064, 4.733333333333352932, 1.299038105676669330 ) ) ;
#10205 = CARTESIAN_POINT ( 'NONE',  ( 3.988069740714122791, 7.804498464141805592, 0.7998128361456321445 ) ) ;
#10206 = CARTESIAN_POINT ( 'NONE',  ( 5.635385404774530649, 9.726366738878972740, 0.7998128361456462443 ) ) ;
#10207 = CARTESIAN_POINT ( 'NONE',  ( 2.684490341743519082, 1.190536367853095578, 1.875150363231482098 ) ) ;
#10209 = CARTESIAN_POINT ( 'NONE',  ( -9.367496997601190145, 14.57669131240758276, 7.413898975931879853 ) ) ;
#10208 = CIRCLE ( 'NONE', #134720, 10.99999999999999112 ) ;
#10210 = CARTESIAN_POINT ( 'NONE',  ( 6.805829924380108586, 8.963220883242035697, 1.443375672974076540 ) ) ;
#10211 = CARTESIAN_POINT ( 'NONE',  ( -9.205623113554631587, 11.76297960394566466, 1.443375672974076540 ) ) ;
#10212 = CARTESIAN_POINT ( 'NONE',  ( 6.048345925472178308, 9.110135108809304327, 1.082531754730549967 ) ) ;
#10213 = CARTESIAN_POINT ( 'NONE',  ( 0.7389079861009685279, 2.013985778099684154, -0.1017531103126300962 ) ) ;
#10215 = CARTESIAN_POINT ( 'NONE',  ( 5.195784910611107144, -1.456250996468626768, -1.461061404345398440 ) ) ;
#10214 = CARTESIAN_POINT ( 'NONE',  ( 8.565000355531088516, 11.01558638625153286, -1.599625672291257406 ) ) ;
#10216 =( NAMED_UNIT ( * ) SI_UNIT ( $, .STERADIAN. ) SOLID_ANGLE_UNIT ( ) );
#10217 = CARTESIAN_POINT ( 'NONE',  ( -2.442440228756222353, 6.001264033524212671, -0.7998128361456281477 ) ) ;
#10218 = CARTESIAN_POINT ( 'NONE',  ( 5.329763783503544516, 9.232158490813878515, -0.7216878364870458196 ) ) ;
#10219 = LINE ( 'NONE', #155410, #99204 ) ;
#10220 = CARTESIAN_POINT ( 'NONE',  ( -1.364683531250014514, 0.4885416670080875434, -0.7879004041258289570 ) ) ;
#10221 = CARTESIAN_POINT ( 'NONE',  ( 0.4909911900966601461, 1.305473228555413812, 1.195063304280475025 ) ) ;
#10222 = CARTESIAN_POINT ( 'NONE',  ( 6.012339335674446339, -1.629552802491928354, 0.5935831289462877303 ) ) ;
#10223 = CARTESIAN_POINT ( 'NONE',  ( 5.952664183270127474, -1.497414089959566930, -0.8868285315999470120 ) ) ;
#10224 = CARTESIAN_POINT ( 'NONE',  ( 2.718655769491088225, 2.159526321510790492, 0.7694321526581606729 ) ) ;
#10225 = CARTESIAN_POINT ( 'NONE',  ( 0.6823417656249882723, -0.07395833299191079124, -1.181850606188749264 ) ) ;
#10226 = CARTESIAN_POINT ( 'NONE',  ( 2.396224210035051261, 1.478860665732561586, -1.096489538662905217 ) ) ;
#10227 = ADVANCED_FACE ( 'NONE', ( #182175 ), #20146, .F. ) ;
#10228 = CARTESIAN_POINT ( 'NONE',  ( 8.075853055234393452, 12.57357899774884658, 0.7998128361456462443 ) ) ;
#10229 = CARTESIAN_POINT ( 'NONE',  ( 2.748829393344632166, -1.518919317350690967, 1.012417160375630898 ) ) ;
#10230 = CARTESIAN_POINT ( 'NONE',  ( 3.410779880581996437, -1.203353552534730309, -1.617818353255597863 ) ) ;
#10231 = CARTESIAN_POINT ( 'NONE',  ( -9.667127221743832877, 11.23706883257798772, 1.199719254218462483 ) ) ;
#10232 = CARTESIAN_POINT ( 'NONE',  ( -11.55950211276791428, 12.22000000000000064, -3.221476510067114329 ) ) ;
#10233 = CARTESIAN_POINT ( 'NONE',  ( 5.016683434392706253, 1.454383057171860116, -1.523333715015115608 ) ) ;
#10234 = CARTESIAN_POINT ( 'NONE',  ( 7.615526167148707337, 15.99525620954516292, 10.13761593936639294 ) ) ;
#10235 = CARTESIAN_POINT ( 'NONE',  ( 2.313015868914463091, -1.601887806243259771, 1.311650804931147274 ) ) ;
#10236 = CARTESIAN_POINT ( 'NONE',  ( 4.111146893441827821, 5.819424013814004759, 1.599625672291267398 ) ) ;
#10237 = CARTESIAN_POINT ( 'NONE',  ( 0.6801582343749970061, 0.8385416670080649837, -1.178068619123841643 ) ) ;
#10238 = CARTESIAN_POINT ( 'NONE',  ( 4.670628115925999246, 0.8122961462209904449, 1.958930372594757330 ) ) ;
#10239 = ITEM_DEFINED_TRANSFORMATION ( 'NONE', 'NONE', #100697,  #200407 ) ;
#10240 = CARTESIAN_POINT ( 'NONE',  ( 0.4692025345035084061, 0.1902923850431673669, -1.917074784726199965 ) ) ;
#10241 = VERTEX_POINT ( 'NONE', #173433 ) ;
#10242 = CARTESIAN_POINT ( 'NONE',  ( -4.359828915246279024, 7.244161613499399799, -1.199719254218455378 ) ) ;
#10243 = CARTESIAN_POINT ( 'NONE',  ( 9.433775957010412938, 9.900493459467314850, 0.000000000000000000 ) ) ;
#10244 = CARTESIAN_POINT ( 'NONE',  ( 4.950135482320912494, 6.868520377498098739, -1.443375672974068769 ) ) ;
#10245 = CARTESIAN_POINT ( 'NONE',  ( 3.475000000000000533, -1.181249999044085897, 0.000000000000000000 ) ) ;
#10246 = CARTESIAN_POINT ( 'NONE',  ( -4.717347382551060342, 7.590990148696470818, 1.199719254218464037 ) ) ;
#10247 = CARTESIAN_POINT ( 'NONE',  ( -0.1399463097118925359, -1.722747986054250058, -1.402038615606171046 ) ) ;
#10248 = CARTESIAN_POINT ( 'NONE',  ( 2.520660759794272732, 1.376564137786383091, -1.593852158419235332 ) ) ;
#10249 = CARTESIAN_POINT ( 'NONE',  ( -4.197131071882288289, 7.054347462908075350, -1.199719254218455378 ) ) ;
#10250 = CARTESIAN_POINT ( 'NONE',  ( 6.968000882419564945, 10.21675256520979858, 1.199719254218460707 ) ) ;
#10251 = CARTESIAN_POINT ( 'NONE',  ( 6.086726144739807332, 1.793049480792831440, 0.4976782122840143763 ) ) ;
#10252 = CARTESIAN_POINT ( 'NONE',  ( 6.089583550832340819, 10.25626457594641749, 1.040834085586084257E-14 ) ) ;
#10253 = EDGE_CURVE ( 'NONE', #34262, #758, #122624, .T. ) ;
#10254 = CARTESIAN_POINT ( 'NONE',  ( -11.97929049433705373, 9.719999999999998863, 0.7046979865771783036 ) ) ;
#10255 = ORIENTED_EDGE ( 'NONE', *, *, #183912, .F. ) ;
#10256 = CARTESIAN_POINT ( 'NONE',  ( -5.483346782084204563, 5.361935765378481378, 0.000000000000000000 ) ) ;
#10257 = CARTESIAN_POINT ( 'NONE',  ( -9.002250809793991948, 12.48608113052627289, -1.082531754730543971 ) ) ;
#10258 = CARTESIAN_POINT ( 'NONE',  ( 0.1410940620840978044, 2.031152781523197337, 0.6094965309384676733 ) ) ;
#10260 = CARTESIAN_POINT ( 'NONE',  ( 2.224987305166142626, -1.792472147789250236, -0.7979012372742313453 ) ) ;
#10259 = CARTESIAN_POINT ( 'NONE',  ( -3.355169270512988773E-14, -0.8124999999999558131, -1.414508159514601626 ) ) ;
#10261 = CARTESIAN_POINT ( 'NONE',  ( 0.8312129145573650124, 0.1600495679085281175, 2.155820468135719814 ) ) ;
#10263 = CARTESIAN_POINT ( 'NONE',  ( -6.123425537405413621, 6.005001634332811200, 0.2246051741978810634 ) ) ;
#10262 = CARTESIAN_POINT ( 'NONE',  ( -4.098307573080856692, 8.003385611894792362, 0.7998128361456352531 ) ) ;
#10264 = CARTESIAN_POINT ( 'NONE',  ( -0.6823417656250003738, 1.217708333674752286, -1.181850606188749264 ) ) ;
#10265 = CARTESIAN_POINT ( 'NONE',  ( 2.817972641794503019, 1.638747005868109285, 0.5862587914967545277 ) ) ;
#10266 = CARTESIAN_POINT ( 'NONE',  ( 5.829642864196157070, 8.784705193995428374, 1.082531754730558626 ) ) ;
#10267 = CARTESIAN_POINT ( 'NONE',  ( -11.33523815116046229, 5.279172990141937305, 5.677742996778201601 ) ) ;
#10268 = CARTESIAN_POINT ( 'NONE',  ( 2.776720060080526853, -1.994564479802892087, 0.2930246351905210211 ) ) ;
#10269 = CARTESIAN_POINT ( 'NONE',  ( 6.825078400183548943, 1.222324429417048330, 2.356141576552318817 ) ) ;
#10270 = CARTESIAN_POINT ( 'NONE',  ( -3.149236820124241110, 6.896136400112061970, -0.7998128361456481317 ) ) ;
#10271 = CARTESIAN_POINT ( 'NONE',  ( 1.815242386724497337, -0.2434097785052463103, 1.956328700473447979 ) ) ;
#10274 = EDGE_CURVE ( 'NONE', #26370, #93781, #171269, .T. ) ;
#10273 = CARTESIAN_POINT ( 'NONE',  ( -6.048345925472225382, 8.149765894507963182, 1.443375672974058777 ) ) ;
#10272 = CARTESIAN_POINT ( 'NONE',  ( 5.976807594091997800, -1.347613670528555740, 1.357171208065083512 ) ) ;
#10275 = CARTESIAN_POINT ( 'NONE',  ( -5.600926855776888758, 7.627776979863398310, -1.443375672974066548 ) ) ;
#10276 = CARTESIAN_POINT ( 'NONE',  ( 4.715203562502613188, 8.723097599553565118, 0.7998128361456341429 ) ) ;
#10277 = CARTESIAN_POINT ( 'NONE',  ( -4.847922445338252118, 7.813604065273374921, -1.199719254218453823 ) ) ;
#10278 = CARTESIAN_POINT ( 'NONE',  ( 1.207682226051248753, 1.530763495831432452, 1.317637323925124671 ) ) ;
#10279 = FACE_OUTER_BOUND ( 'NONE', #198975, .T. ) ;
#10280 = EDGE_CURVE ( 'NONE', #187973, #85130, #834, .T. ) ;
#10281 = CARTESIAN_POINT ( 'NONE',  ( 5.315557996638371918, -0.3450676865139382099, 2.281540517825955128 ) ) ;
#10282 = CARTESIAN_POINT ( 'NONE',  ( 5.406682003534418079, 0.5678430586343993225, 1.877905798087247335 ) ) ;
#10283 = CARTESIAN_POINT ( 'NONE',  ( 2.658977320520792276, 1.578554556127611308, -1.164590279592196298 ) ) ;
#10284 = CARTESIAN_POINT ( 'NONE',  ( 9.433775957010412938, 9.900493459467314850, 0.000000000000000000 ) ) ;
#10285 = CARTESIAN_POINT ( 'NONE',  ( 1.108046318188542489, -0.04667474159409169127, 2.016033875899234662 ) ) ;
#10286 = ORIENTED_EDGE ( 'NONE', *, *, #171577, .T. ) ;
#10287 = CARTESIAN_POINT ( 'NONE',  ( 0.9896463964080002285, -0.5083134511523321741, 2.055333615346987663 ) ) ;
#10289 = CARTESIAN_POINT ( 'NONE',  ( -6.124532705071231931, 8.168374127381657246, -1.599625672291263179 ) ) ;
#10288 = CARTESIAN_POINT ( 'NONE',  ( -3.436101866059630527, 6.096203712789787232, 1.199719254218462483 ) ) ;
#10290 = CARTESIAN_POINT ( 'NONE',  ( 1.640310086786896049, -1.556016536173940645, 0.9838780322720328542 ) ) ;
#10291 = ORIENTED_EDGE ( 'NONE', *, *, #105774, .F. ) ;
#10292 = CARTESIAN_POINT ( 'NONE',  ( 11.14442593998487219, 9.074645745019246590, -4.464617754680513251 ) ) ;
#10293 = CARTESIAN_POINT ( 'NONE',  ( 2.689816194747224110, 2.012238202079220439, -0.6693303307304664385 ) ) ;
#10294 = CARTESIAN_POINT ( 'NONE',  ( -0.7500000000000215383, 4.722916667349482012, 1.299038105676671107 ) ) ;
#10295 = CARTESIAN_POINT ( 'NONE',  ( 8.938903350111612411, 9.323142084752035430, -0.7998128361456221525 ) ) ;
#10296 = CARTESIAN_POINT ( 'NONE',  ( 5.338878628731272613, 9.450718510153643948, -0.7998128361456481317 ) ) ;
#10297 = CARTESIAN_POINT ( 'NONE',  ( 3.638010413220875705, 0.9297346566990055683, -1.839232330223056433 ) ) ;
#10298 = VECTOR ( 'NONE', #111373, 1000.000000000000000 ) ;
#10300 = CARTESIAN_POINT ( 'NONE',  ( 1.294213439101927321, 1.504999338701202394, -1.060447551955064016 ) ) ;
#10299 = CARTESIAN_POINT ( 'NONE',  ( -6.679363233026820446, 10.94434087183997129, 0.000000000000000000 ) ) ;
#10301 = CARTESIAN_POINT ( 'NONE',  ( 0.6823417656249899377, 5.176041667008086655, -1.181850606188754593 ) ) ;
#10302 = CARTESIAN_POINT ( 'NONE',  ( 1.500236433942635950, 4.350729682706125701, -0.06629318219673785428 ) ) ;
#10303 = CARTESIAN_POINT ( 'NONE',  ( -11.89942855770814134, 13.79999999999999893, 0.6999999999999992895 ) ) ;
#10304 = CARTESIAN_POINT ( 'NONE',  ( 0.9267433102794273569, 1.311770220233858586, -1.774563083084364834 ) ) ;
#10305 = CARTESIAN_POINT ( 'NONE',  ( 2.935161367736533133, 0.2740405928264351143, 2.245665650516134093 ) ) ;
#10306 = CARTESIAN_POINT ( 'NONE',  ( -7.700668062882072284, 10.00719871149432549, -1.443375672974059665 ) ) ;
#10307 = CARTESIAN_POINT ( 'NONE',  ( 2.162115752888054576, 1.811270999727595976, 0.04120172278379052866 ) ) ;
#10308 = CARTESIAN_POINT ( 'NONE',  ( 2.659291035590090058, 1.817528298045675061, -0.6055613653334031010 ) ) ;
#10309 = CARTESIAN_POINT ( 'NONE',  ( 4.369627354678314646, -0.3570511267821044332, 2.039192500141631115 ) ) ;
#10310 = CARTESIAN_POINT ( 'NONE',  ( 0.6823417656249882723, 2.738541667008084879, -1.181850606188749264 ) ) ;
#10311 = CARTESIAN_POINT ( 'NONE',  ( 2.694160965578366262, -1.966063403948969057, -0.1468289651068572232 ) ) ;
#10312 = CARTESIAN_POINT ( 'NONE',  ( 0.1121488755844394364, -0.8197171475488943537, -1.741376145853351431 ) ) ;
#10313 = CARTESIAN_POINT ( 'NONE',  ( 3.906994808788874174, 1.604092888448312326, 0.9621832354540849064 ) ) ;
#10314 = CIRCLE ( 'NONE', #107335, 0.08000000000000020983 ) ;
#10316 = CARTESIAN_POINT ( 'NONE',  ( 4.609415035364720303, 8.472105597856021575, 0.2450749143364742144 ) ) ;
#10315 = CARTESIAN_POINT ( 'NONE',  ( 2.491230068042503465, -0.3961224009183231809, -2.273300736686647117 ) ) ;
#10317 = CARTESIAN_POINT ( 'NONE',  ( 3.402650393365719506, 0.4499446578831092780, 1.805719076957598368 ) ) ;
#10318 = CARTESIAN_POINT ( 'NONE',  ( 1.364683531249990311, 3.884375000341417028, 1.214306433183764966E-14 ) ) ;
#10319 = CARTESIAN_POINT ( 'NONE',  ( -4.111146893441842920, 5.819424013814012753, 1.599625672291267398 ) ) ;
#10320 = CARTESIAN_POINT ( 'NONE',  ( 7.311924916471702396, 7.425000578838787391, -0.7998128361456281477 ) ) ;
#10321 = CARTESIAN_POINT ( 'NONE',  ( -1.265299903344048404, 3.920951693072811661, 0.4993168358707228971 ) ) ;
#10322 = CARTESIAN_POINT ( 'NONE',  ( 0.3113324583694621617, 1.833617258854224552, 1.035894449818143270 ) ) ;
#10323 = CARTESIAN_POINT ( 'NONE',  ( -1.201851678989727383E-14, 3.884375000341423689, 1.575800808251672791 ) ) ;
#10324 = CARTESIAN_POINT ( 'NONE',  ( 6.204392391313840349, -0.7715976231806519481, -2.019385000091134419 ) ) ;
#10325 = CARTESIAN_POINT ( 'NONE',  ( -0.2048590494372501680, -0.1558505989666530422, -1.986559690435693026 ) ) ;
#10326 = CARTESIAN_POINT ( 'NONE',  ( -1.402160292154681736E-14, -0.05312499965857903073, -1.575800808251665908 ) ) ;
#10327 = CARTESIAN_POINT ( 'NONE',  ( -4.229780737783618072, 6.918199379847403740, 1.082531754730560403 ) ) ;
#10330 = CARTESIAN_POINT ( 'NONE',  ( 4.717874267875568961, 4.606534188717351874, -0.7216878364870188411 ) ) ;
#10329 = CARTESIAN_POINT ( 'NONE',  ( 6.925078400183545035, 0.003529629153843985134, 1.755452343125718073 ) ) ;
#10328 = CARTESIAN_POINT ( 'NONE',  ( 5.956828388357757298, 8.042995434541133193, 1.599625672291269396 ) ) ;
#10331 = CARTESIAN_POINT ( 'NONE',  ( -0.2104748580754183807, 4.084054299358617079, -2.658391380015924010 ) ) ;
#10332 = CARTESIAN_POINT ( 'NONE',  ( 5.243375144629232487, 0.3886363430659239837, -1.978554426619572926 ) ) ;
#10334 = CARTESIAN_POINT ( 'NONE',  ( -5.600926855776877211, 9.548515408466085930, -0.7216878364870338292 ) ) ;
#10333 = CARTESIAN_POINT ( 'NONE',  ( -9.544576954340667996, 11.19805653722800365, 1.082531754730558626 ) ) ;
#10336 = CARTESIAN_POINT ( 'NONE',  ( -8.012344526598182026E-15, 11.29687500034139980, -1.575800808251669460 ) ) ;
#10335 = CARTESIAN_POINT ( 'NONE',  ( 6.438358464623771482, 2.137424745569570295, 0.3223339197731683869 ) ) ;
#10337 = CARTESIAN_POINT ( 'NONE',  ( -10.32183501870554387, 10.93656236477829502, 0.7998128361456462443 ) ) ;
#10339 = CARTESIAN_POINT ( 'NONE',  ( 6.151970292378349470, 1.039009440890667824, 1.727993850779283802 ) ) ;
#10338 = CARTESIAN_POINT ( 'NONE',  ( -5.219525951136837705, 9.033271343060892633, -0.7216878364870207285 ) ) ;
#10340 = CARTESIAN_POINT ( 'NONE',  ( 0.6823417656249882723, 1.238541667008083547, -1.181850606188749264 ) ) ;
#10341 = B_SPLINE_CURVE_WITH_KNOTS ( 'NONE', 3,
 ( #36646, #69128, #123342, #103804, #121197, #169853 ),
 .UNSPECIFIED., .F., .F.,
 ( 4, 2, 4 ),
 ( 0.000000000000000000, 0.0003767011250903910184, 0.0007534022501807820368 ),
 .UNSPECIFIED. ) ;
#10342 = CARTESIAN_POINT ( 'NONE',  ( 6.883263157960362477, 3.690127339433949327, 2.567897385111846731 ) ) ;
#10343 = CARTESIAN_POINT ( 'NONE',  ( 1.499999999999993117, 8.854166666666667851, 0.8660254037844409281 ) ) ;
#10344 = CARTESIAN_POINT ( 'NONE',  ( 1.470901328764297800, 0.1297424413324743397, -1.720050270840302487 ) ) ;
#10345 = CARTESIAN_POINT ( 'NONE',  ( 4.947799714344386146, 4.737130853015369958, -0.7998128361456481317 ) ) ;
#10346 = CARTESIAN_POINT ( 'NONE',  ( 6.150558962454855561, 7.204682206732687000, 1.199719254218452047 ) ) ;
#10347 = CARTESIAN_POINT ( 'NONE',  ( -1.402160292154681736E-14, -0.7406249996585823059, -1.575800808251665908 ) ) ;
#10348 = CARTESIAN_POINT ( 'NONE',  ( 0.6668358675281795822, 0.1816249057532189626, -1.760414781625377234 ) ) ;
#10349 = CARTESIAN_POINT ( 'NONE',  ( 1.840491241682026047, 1.157229580565920513, -1.647056139248611384 ) ) ;
#10350 = ADVANCED_FACE ( 'NONE', ( #105229 ), #71614, .T. ) ;
#10351 = CARTESIAN_POINT ( 'NONE',  ( 2.372313692266983853, 5.711523707712699682, 0.7216878364870438212 ) ) ;
#10352 = CARTESIAN_POINT ( 'NONE',  ( 4.471826267013489620, 2.141383520707430321, -0.5327586567505787629 ) ) ;
#10353 = CARTESIAN_POINT ( 'NONE',  ( 5.418865745523654631, -1.577555059383651814, 1.491859142196997334 ) ) ;
#10354 = ORIENTED_EDGE ( 'NONE', *, *, #144993, .T. ) ;
#10355 = CARTESIAN_POINT ( 'NONE',  ( 2.911969131885072670, 6.619324097166378706, 0.000000000000000000 ) ) ;
#10356 = CARTESIAN_POINT ( 'NONE',  ( 8.473482818416664841, 10.90881592628469932, -1.443375672974063439 ) ) ;
#10358 = CARTESIAN_POINT ( 'NONE',  ( 3.146111402376899235, 0.9091623069825971459, 1.799915193831227889 ) ) ;
#10357 = CARTESIAN_POINT ( 'NONE',  ( 3.211701520346501582, 1.672844727185973657, 1.303009041611735030 ) ) ;
#10360 = ORIENTED_EDGE ( 'NONE', *, *, #101405, .T. ) ;
#10359 = CARTESIAN_POINT ( 'NONE',  ( 3.920002888225936566, -1.806327840557620412, 0.1390898763422818984 ) ) ;
#10361 = CARTESIAN_POINT ( 'NONE',  ( 5.200434439293556643, 8.224868058221247225, -1.199719254218452047 ) ) ;
#10362 = ORIENTED_EDGE ( 'NONE', *, *, #196360, .F. ) ;
#10363 = TOROIDAL_SURFACE ( 'NONE', #159107, 10.89999999999920455, 0.2000000000000000111 ) ;
#10364 = CARTESIAN_POINT ( 'NONE',  ( 0.5318453760667535279, 0.9654296485097980662, -1.602142582367314549 ) ) ;
#10365 = CARTESIAN_POINT ( 'NONE',  ( 5.777927443424748510, 1.091106472389313131, 1.463626628978510702 ) ) ;
#10367 = CARTESIAN_POINT ( 'NONE',  ( 1.147507391605587568, 1.886754179610318438, -0.3309440326291489542 ) ) ;
#10366 = CARTESIAN_POINT ( 'NONE',  ( -3.684065054611367351, 5.321161868511784299, -1.599625672291256295 ) ) ;
#10368 = FACE_OUTER_BOUND ( 'NONE', #10203, .T. ) ;
#10369 = CARTESIAN_POINT ( 'NONE',  ( 1.364683531249988535, 1.676041667008085101, 0.7879004041258500513 ) ) ;
#10370 = CARTESIAN_POINT ( 'NONE',  ( 2.088542702721609690, 3.956598013261175772, -11.35310118413587510 ) ) ;
#10371 = VERTEX_POINT ( 'NONE', #20731 ) ;
#10372 = CARTESIAN_POINT ( 'NONE',  ( 6.617788377246179188, 8.814115421577600529, -1.443375672974078761 ) ) ;
#10373 = CARTESIAN_POINT ( 'NONE',  ( -6.143253000767895600, 6.339752387083549934, 0.000000000000000000 ) ) ;
#10374 = CARTESIAN_POINT ( 'NONE',  ( -7.425025402139490360, 8.691559719698066289, 1.199719254218452047 ) ) ;
#10375 = CARTESIAN_POINT ( 'NONE',  ( 3.410498715577559015, -2.118327196165440185, -0.1003008382433126094 ) ) ;
#10376 = ADVANCED_FACE ( 'NONE', ( #137727, #86826, #55391, #4468, #22863, #70540, #136659, #54333 ), #120472, .F. ) ;
#10378 = CARTESIAN_POINT ( 'NONE',  ( -10.83925572545688176, 5.627432043407306850, 6.488667418600651438 ) ) ;
#10377 = CARTESIAN_POINT ( 'NONE',  ( -1.499999999999997780, 5.650000000000023448, 1.214306433183764966E-14 ) ) ;
#10379 = CARTESIAN_POINT ( 'NONE',  ( 4.393795938483449071, -0.7573388051436024115, 1.820269059793070410 ) ) ;
#10380 = CARTESIAN_POINT ( 'NONE',  ( 6.082274476537278041, 0.9889857280602430967, 1.636697341158253272 ) ) ;
#10381 = ORIENTED_EDGE ( 'NONE', *, *, #158942, .F. ) ;
#10382 = CARTESIAN_POINT ( 'NONE',  ( 0.2986504545328653726, 1.456477371935499088, -1.536899124724122601 ) ) ;
#10383 = CARTESIAN_POINT ( 'NONE',  ( 7.127657509075540965, 14.48195938056236898, 9.656923498056537269 ) ) ;
#10384 = CARTESIAN_POINT ( 'NONE',  ( 1.768117254402020277, -2.054967671486531255, 0.2513356459030794410 ) ) ;
#10385 = CARTESIAN_POINT ( 'NONE',  ( 2.660020691486902233, -1.338829530657672073, 1.406886975181226296 ) ) ;
#10386 = ORIENTED_EDGE ( 'NONE', *, *, #83202, .T. ) ;
#10387 = CARTESIAN_POINT ( 'NONE',  ( 4.908934136599710563, 7.884784371745123366, 1.199719254218451159 ) ) ;
#10388 = CARTESIAN_POINT ( 'NONE',  ( 5.742760583840166966, 8.857581893525663830, 1.199719254218452047 ) ) ;
#10390 = CARTESIAN_POINT ( 'NONE',  ( 5.819474248763732760, 7.812472595022922128, -1.599625672291262513 ) ) ;
#10389 = CARTESIAN_POINT ( 'NONE',  ( 3.205106881211945868, -0.4073652088906943858, 2.050380944992454602 ) ) ;
#10391 = CARTESIAN_POINT ( 'NONE',  ( 3.729901657090948230, 6.405283462364505631, 1.082531754730549078 ) ) ;
#10393 = ORIENTED_EDGE ( 'NONE', *, *, #121074, .F. ) ;
#10392 = CARTESIAN_POINT ( 'NONE',  ( 0.4514444101613367955, -1.279852094280601760, -1.282217761895942720 ) ) ;
#10394 = CARTESIAN_POINT ( 'NONE',  ( 5.127635347277352373, -2.096377701570474539, 0.6897739467496829535 ) ) ;
#10395 = CARTESIAN_POINT ( 'NONE',  ( 0.08058608058607032165, -6.134628647623513231, -10.99970480893079916 ) ) ;
#10396 = EDGE_CURVE ( 'NONE', #184431, #168636, #192837, .T. ) ;
#10397 = CARTESIAN_POINT ( 'NONE',  ( 3.135963548190400019, -1.480894843444351849, -1.636267651353009445 ) ) ;
#10398 = CARTESIAN_POINT ( 'NONE',  ( 7.072549687823125097, 11.40305840243567381, -0.7998128361456291469 ) ) ;
#10399 = CARTESIAN_POINT ( 'NONE',  ( 1.734935157289751562, 1.374772708486753370, 1.500000000000001332 ) ) ;
#10400 = CARTESIAN_POINT ( 'NONE',  ( 1.594246750649646494, -1.022002606473694675, 1.616071880676916317 ) ) ;
#10401 = CARTESIAN_POINT ( 'NONE',  ( 9.935427640716063991, 10.48575375712389679, -0.7998128361456281477 ) ) ;
#10402 = CARTESIAN_POINT ( 'NONE',  ( 5.459458695672200435, 1.690470114046587646, 1.195012289465044564 ) ) ;
#10404 = CARTESIAN_POINT ( 'NONE',  ( 2.799875798528407511, -0.6792266858460673795, 2.052276964324008635 ) ) ;
#10403 = CARTESIAN_POINT ( 'NONE',  ( -3.045082456892887812, 6.452177443058107364, 0.6540759397886571902 ) ) ;
#10405 = CARTESIAN_POINT ( 'NONE',  ( 4.687173145698103838, 1.624054394666199830, 1.471728111018810070 ) ) ;
#10406 = ORIENTED_EDGE ( 'NONE', *, *, #104659, .T. ) ;
#10407 = LINE ( 'NONE', #28811, #27850 ) ;
#10408 = EDGE_CURVE ( 'NONE', #191915, #200036, #10885, .T. ) ;
#10409 = CARTESIAN_POINT ( 'NONE',  ( 3.475000000000000533, -1.924999999999999600, 0.000000000000000000 ) ) ;
#10410 = CARTESIAN_POINT ( 'NONE',  ( -0.5511734105799743766, 7.507429961897361892, 1.922562588595814415 ) ) ;
#10411 = CARTESIAN_POINT ( 'NONE',  ( 5.246079093845007257, 5.085123462432798114, 0.7998128361456352531 ) ) ;
#10412 = CARTESIAN_POINT ( 'NONE',  ( -1.642778471874998480, -2.938541666188707602, 2.845375778867863303 ) ) ;
#10413 = ADVANCED_FACE ( 'NONE', ( #111677 ), #79098, .F. ) ;
#10414 = CARTESIAN_POINT ( 'NONE',  ( -7.212574532790087645, 11.35849468832304154, -0.7216878364870267237 ) ) ;
#10415 = CARTESIAN_POINT ( 'NONE',  ( 4.386945222473598527, 7.275797305264619652, -1.199719254218452047 ) ) ;
#10416 = CARTESIAN_POINT ( 'NONE',  ( 5.453992358814952368, -0.7503507308065425763, 1.929658000011783336 ) ) ;
#10417 = CARTESIAN_POINT ( 'NONE',  ( 3.932187577746598883, 1.029727551008235320, -1.628035494724868970 ) ) ;
#10418 = CARTESIAN_POINT ( 'NONE',  ( 6.609000000000050612, -6.653734691735092887E-05, 2.100160721423645960 ) ) ;
#10419 = CARTESIAN_POINT ( 'NONE',  ( -8.448702279610222021, 13.00856975952063088, 1.040834085586084257E-14 ) ) ;
#10420 = CARTESIAN_POINT ( 'NONE',  ( 5.497994985541524215, 6.373081223675282736, -1.199719254218445830 ) ) ;
#10421 = DIRECTION ( 'NONE',  ( 0.000000000000000000, 0.000000000000000000, 1.000000000000000000 ) ) ;
#10422 = CARTESIAN_POINT ( 'NONE',  ( 5.278159644759479185, -1.050164822159710853, -1.665878549478349013 ) ) ;
#10423 = CARTESIAN_POINT ( 'NONE',  ( 6.544901331262317434, -1.836973039681317088, -1.370978055005685370 ) ) ;
#10424 = CARTESIAN_POINT ( 'NONE',  ( 4.969292227364340953, 0.1756445257206709631, -1.817221496977147854 ) ) ;
#10425 = CARTESIAN_POINT ( 'NONE',  ( 5.695833931516881776, 9.659240330162777610, -0.7216878364870458196 ) ) ;
#10426 = CARTESIAN_POINT ( 'NONE',  ( 2.358755538653318773, 5.695705861830088423, 1.040834085586084257E-14 ) ) ;
#10427 = ADVANCED_FACE ( 'NONE', ( #60716 ), #3176, .F. ) ;
#10428 = CARTESIAN_POINT ( 'NONE',  ( -5.281783360975562225, 8.319775133516907673, 1.199719254218452935 ) ) ;
#10429 = CARTESIAN_POINT ( 'NONE',  ( 5.123001941117305336, 7.070197912760590064, 1.599625672291268286 ) ) ;
#10430 = ORIENTED_EDGE ( 'NONE', *, *, #30893, .F. ) ;
#10432 = CARTESIAN_POINT ( 'NONE',  ( 6.240495565780414644, 1.155569484861172391, -1.648366056897664800 ) ) ;
#10431 = CARTESIAN_POINT ( 'NONE',  ( 2.138008341990283778, 0.4048980806483238326, 1.796005048712509655 ) ) ;
#10433 = CARTESIAN_POINT ( 'NONE',  ( 1.142455020822298106, -0.05817821010643645790, -2.297781139197229372 ) ) ;
#10434 = CARTESIAN_POINT ( 'NONE',  ( 5.067221110791254368, 1.704927679941736329, 0.9703409489375602881 ) ) ;
#10435 = CARTESIAN_POINT ( 'NONE',  ( -6.715366157470410435, 6.729015360003925750, -0.7998128361456291469 ) ) ;
#10436 = CARTESIAN_POINT ( 'NONE',  ( 0.3978093821460239599, 3.011896635411783318, -0.3978093821461178292 ) ) ;
#10437 = CARTESIAN_POINT ( 'NONE',  ( -4.243865776277440993, 4.909930479533815451, -1.199719254218446718 ) ) ;
#10438 = CARTESIAN_POINT ( 'NONE',  ( 0.6079806153083644471, 0.6509857562557037625, -1.965403638620793147 ) ) ;
#10439 = CARTESIAN_POINT ( 'NONE',  ( -4.176793841461789114, 7.030620694084159794, -1.199719254218455378 ) ) ;
#10441 = CARTESIAN_POINT ( 'NONE',  ( 0.2857447052702493662, -0.8859512962964136706, 1.647562673099879138 ) ) ;
#10440 = CARTESIAN_POINT ( 'NONE',  ( 1.646151360528936625, 0.6591259108063004524, 1.984184313626126350 ) ) ;
#10442 = CARTESIAN_POINT ( 'NONE',  ( 1.419999999999990603, 6.280000000000042881, 2.500000000000000444 ) ) ;
#10443 = CARTESIAN_POINT ( 'NONE',  ( -0.2104748580754183529, 0.2283854016844401591, -2.137091067173245929 ) ) ;
#10444 = CARTESIAN_POINT ( 'NONE',  ( 1.575334329707895664, -0.9311816076861539893, 1.470162731330543426 ) ) ;
#10445 = CARTESIAN_POINT ( 'NONE',  ( 6.010342169559767633, 5.906487374108181143, -0.7998128361456281477 ) ) ;
#10447 = CARTESIAN_POINT ( 'NONE',  ( 1.567286081490169902, 8.684911043814580012, 2.501016734198271418 ) ) ;
#10446 = FACE_OUTER_BOUND ( 'NONE', #165738, .T. ) ;
#10448 = CARTESIAN_POINT ( 'NONE',  ( 2.332253321102405685, 1.672780984221501122, 0.4201815020834080427 ) ) ;
#10449 = CARTESIAN_POINT ( 'NONE',  ( 3.280998142716429200, 1.980384277226649559, -0.9389412094223739125 ) ) ;
#10450 = CARTESIAN_POINT ( 'NONE',  ( 0.1407077508718111714, 0.6607813331330723017, 1.603534759577706303 ) ) ;
#10451 = CARTESIAN_POINT ( 'NONE',  ( 5.092482806099829062, -2.189899077852827780, -0.2726905915074183673 ) ) ;
#10452 = CARTESIAN_POINT ( 'NONE',  ( -9.970593631352514308, 5.552127128363319564, -5.997086463700067149 ) ) ;
#10453 = CARTESIAN_POINT ( 'NONE',  ( 2.764704757504053756, -0.8271204958998740198, -2.007528505447711886 ) ) ;
#10454 = CARTESIAN_POINT ( 'NONE',  ( 1.418276456094772708, 1.227529518603141190, -1.351586893430449576 ) ) ;
#10455 = CARTESIAN_POINT ( 'NONE',  ( 3.257133915093980203, 0.04755548373316278304, -2.116953498886654295 ) ) ;
#10456 = CARTESIAN_POINT ( 'NONE',  ( 6.539320575229254473, 0.5926322452488984593, 1.950287522085321301 ) ) ;
#10457 = VERTEX_POINT ( 'NONE', #177684 ) ;
#10459 = CARTESIAN_POINT ( 'NONE',  ( -1.201851678989727383E-14, 1.884375000341422135, 1.575800808251672791 ) ) ;
#10458 = CARTESIAN_POINT ( 'NONE',  ( 3.245926457026059531, 2.292545471606484142, -0.001860936589836299044 ) ) ;
#10460 = CARTESIAN_POINT ( 'NONE',  ( -5.229199737892074420E-15, 0.06250000000001598721, 1.224999999999961009 ) ) ;
#10461 = CARTESIAN_POINT ( 'NONE',  ( 3.083589872104280705, 5.684939719841914929, 1.199719254218450271 ) ) ;
#10462 = CARTESIAN_POINT ( 'NONE',  ( 5.918639493159310483, -0.7970842504121906646, -2.073522590485813666 ) ) ;
#10463 = CARTESIAN_POINT ( 'NONE',  ( -7.049876689426121779, 7.327203680526343632, -0.7216878364870278340 ) ) ;
#10464 = CARTESIAN_POINT ( 'NONE',  ( 4.121315508874254796, 5.831287398485176077, -1.443375672974051449 ) ) ;
#10465 = CARTESIAN_POINT ( 'NONE',  ( -5.382223794500827552, 9.223085493652217082, -0.7216878364870207285 ) ) ;
#10466 = CARTESIAN_POINT ( 'NONE',  ( 0.06712591543027901508, -9.995102890834049347, 10.91960056525075906 ) ) ;
#10467 = ORIENTED_EDGE ( 'NONE', *, *, #129354, .T. ) ;
#10468 = CARTESIAN_POINT ( 'NONE',  ( 4.008435526009396455, -1.928752077057366732, 0.5880193435906443389 ) ) ;
#10470 = CARTESIAN_POINT ( 'NONE',  ( 1.745062578162811073, -0.2986309630071918853, -2.040702096407704058 ) ) ;
#10469 = CARTESIAN_POINT ( 'NONE',  ( 6.419949431270806528, 7.448694743692793274, 1.199719254218462483 ) ) ;
#10471 = CARTESIAN_POINT ( 'NONE',  ( -10.85277107007939001, 3.956598013261175772, 3.932872935640539414 ) ) ;
#10472 = CARTESIAN_POINT ( 'NONE',  ( 4.923019175093585886, 5.876515471431535076, -1.082531754730548412 ) ) ;
#10473 = CARTESIAN_POINT ( 'NONE',  ( -1.642778471874998480, -3.551041666188709645, 2.845375778867863303 ) ) ;
#10474 = CARTESIAN_POINT ( 'NONE',  ( 1.364683531249990311, 5.134375000341417916, 1.214306433183764966E-14 ) ) ;
#10475 = CARTESIAN_POINT ( 'NONE',  ( 4.927760762764835434, 1.128268568998530563, -1.878541326455762661 ) ) ;
#10476 = CARTESIAN_POINT ( 'NONE',  ( 3.815077410725797424, 1.076317812134291119, -1.704938119663282903 ) ) ;
#10477 = CARTESIAN_POINT ( 'NONE',  ( 2.102840161960460197, -0.4018910908503615653, 1.796694178532439956 ) ) ;
#10478 = ADVANCED_FACE ( 'NONE', ( #95389 ), #96455, .F. ) ;
#10479 = CARTESIAN_POINT ( 'NONE',  ( 6.283314124929436417, 9.417951348137970413, -1.199719254218440723 ) ) ;
#10480 = SHAPE_REPRESENTATION_RELATIONSHIP ( 'NONE' , 'NONE' ,  #113740, #127801 ) ;
#10481 = CARTESIAN_POINT ( 'NONE',  ( 5.842758758449526191, 0.3585452818064547853, 1.789846783968067845 ) ) ;
#10482 = CARTESIAN_POINT ( 'NONE',  ( -7.386494761346872551, 7.511998731193139989, -0.7998128361456291469 ) ) ;
#10484 = CARTESIAN_POINT ( 'NONE',  ( -5.991777542596674166, 5.955104985976372944, 0.000000000000000000 ) ) ;
#10483 = CARTESIAN_POINT ( 'NONE',  ( 5.981380223923965289, 2.093118249296622491, -0.8594570314751952544 ) ) ;
#10485 = CARTESIAN_POINT ( 'NONE',  ( 2.069099208297279002, -1.926018337604347597, -0.8524663740339888385 ) ) ;
#10486 = CARTESIAN_POINT ( 'NONE',  ( -4.450819567036169211, 8.414649604842665553, -0.7998128361456362523 ) ) ;
#10487 =( REPRESENTATION_RELATIONSHIP ('NONE','NONE', #84563, #121983 ) REPRESENTATION_RELATIONSHIP_WITH_TRANSFORMATION ( #191114 )SHAPE_REPRESENTATION_RELATIONSHIP( ) );
#10488 = CARTESIAN_POINT ( 'NONE',  ( 7.391166297744269365, 11.77477778067701664, 1.040834085586084257E-14 ) ) ;
#10489 = CARTESIAN_POINT ( 'NONE',  ( 6.116136693096175136, 9.189224337703940648, -1.082531754730548412 ) ) ;
#10490 = DIRECTION ( 'NONE',  ( 1.000000000000000000, 6.590148024362812955E-17, -2.081668171172168513E-16 ) ) ;
#10491 = CARTESIAN_POINT ( 'NONE',  ( -8.552495972122143186, 8.872333477097637200, 0.7998128361456462443 ) ) ;
#10492 = CARTESIAN_POINT ( 'NONE',  ( 6.640718169121218928, -6.363025497629811511, 7.257245574616259631 ) ) ;
#10493 = CARTESIAN_POINT ( 'NONE',  ( 7.253248993186724114, 9.485209796849769504, 1.443375672974076540 ) ) ;
#10494 = CARTESIAN_POINT ( 'NONE',  ( 4.166517013042797757, 7.612504677086913141, -0.8493068020909979587 ) ) ;
#10495 = CARTESIAN_POINT ( 'NONE',  ( -8.514157279702020631, 11.91663867875229776, -1.082531754730543971 ) ) ;
#10497 = CARTESIAN_POINT ( 'NONE',  ( 2.496574912728947382, -1.137965521849234607, 1.907653428263719864 ) ) ;
#10496 = CARTESIAN_POINT ( 'NONE',  ( 2.355864820516640812, -1.574449018071517825, -1.420800595792824028 ) ) ;
#10498 = CARTESIAN_POINT ( 'NONE',  ( 0.5400322017136415242, -1.563516176313231920, -1.557742479837947558 ) ) ;
#10499 = CARTESIAN_POINT ( 'NONE',  ( -5.936491157937300756, 8.019268665717216749, 1.599625672291263179 ) ) ;
#10500 = CARTESIAN_POINT ( 'NONE',  ( 3.811813743736467419, 7.598866467667865443, 1.040834085586084257E-14 ) ) ;
#10501 = CARTESIAN_POINT ( 'NONE',  ( 4.000408739481801312, 1.952204270133122810, 0.1946113827649766925 ) ) ;
#10502 = CARTESIAN_POINT ( 'NONE',  ( 8.378048858240820351, 11.86180853700128601, -1.199719254218446718 ) ) ;
#10503 = CARTESIAN_POINT ( 'NONE',  ( -5.724176140219916498, 6.114206214821067853, 0.7043541215260868960 ) ) ;
#10504 = CYLINDRICAL_SURFACE ( 'NONE', #199519, 1.250000000000000000 ) ;
#10505 = CARTESIAN_POINT ( 'NONE',  ( 1.364683531249988757, 0.6343750003414208027, 0.000000000000000000 ) ) ;
#10506 = CARTESIAN_POINT ( 'NONE',  ( -4.611181642423629157, 7.433443445252599702, 1.082531754730549967 ) ) ;
#10508 = ORIENTED_EDGE ( 'NONE', *, *, #21226, .T. ) ;
#10507 = CARTESIAN_POINT ( 'NONE',  ( -7.076992996653451939, 7.358839372291564374, 0.7216878364870317197 ) ) ;
#10509 = CARTESIAN_POINT ( 'NONE',  ( 3.252298345715322281, 0.9499829135306799843, -1.895951488860507128 ) ) ;
#10510 = CARTESIAN_POINT ( 'NONE',  ( -4.797606254389363833, 6.690569611577942943, 1.599625672291263179 ) ) ;
#10511 = CARTESIAN_POINT ( 'NONE',  ( 4.311504812833309330, -0.3723461477018601973, 2.129241309423899775 ) ) ;
#10512 = CARTESIAN_POINT ( 'NONE',  ( 3.702549152423353807, 1.581054339307564449, 0.9433870219286569769 ) ) ;
#10513 = CARTESIAN_POINT ( 'NONE',  ( -4.409122955247444686, 7.142713865425108111, 1.076920909521961622 ) ) ;
#10514 = CARTESIAN_POINT ( 'NONE',  ( 1.364683531249988757, -0.5531249996585801965, 0.000000000000000000 ) ) ;
#10515 = CARTESIAN_POINT ( 'NONE',  ( 5.753775850233431299, 0.7111499035084413167, 1.588595604753391122 ) ) ;
#10516 = CARTESIAN_POINT ( 'NONE',  ( 6.827182134110188372, 3.700652156503980716, 2.425390344263624431 ) ) ;
#10517 = CARTESIAN_POINT ( 'NONE',  ( 3.145128448690309053, 4.692402494937224056, -1.443375672974057666 ) ) ;
#10518 = CARTESIAN_POINT ( 'NONE',  ( 11.84668730067608600, 13.40000000000000036, -1.400000000000001910 ) ) ;
#10519 = AXIS2_PLACEMENT_3D ( 'NONE', #166262, #133803, #81817 ) ;
#10520 = CARTESIAN_POINT ( 'NONE',  ( 2.483474991488154870, 1.976725341044349271, -0.8753317036461552014 ) ) ;
#10521 = CARTESIAN_POINT ( 'NONE',  ( 5.184922634274871989, -1.076153828860962225, -1.704676470440001701 ) ) ;
#10522 = CARTESIAN_POINT ( 'NONE',  ( -7.497295758232720431, 10.73030023703809555, -1.082531754730543083 ) ) ;
#10523 = CARTESIAN_POINT ( 'NONE',  ( 1.868271315571629509, 1.111147431007172726, 1.854118885846419262 ) ) ;
#10524 = CARTESIAN_POINT ( 'NONE',  ( 3.532457849674102590, 1.922574350601889082, 0.4351428330651128662 ) ) ;
#10525 = SURFACE_SIDE_STYLE ('',( #43070 ) ) ;
#10526 = CARTESIAN_POINT ( 'NONE',  ( 0.6929124517485165669, -2.290651033777380441, -0.2787006195923043550 ) ) ;
#10527 = CARTESIAN_POINT ( 'NONE',  ( 4.985854738014197984, -1.927824157794202353, -0.2341192097771953584 ) ) ;
#10530 = ORIENTED_EDGE ( 'NONE', *, *, #128394, .T. ) ;
#10529 = ADVANCED_FACE ( 'NONE', ( #92194 ), #212283, .F. ) ;
#10528 = CARTESIAN_POINT ( 'NONE',  ( -8.961576348508641487, 11.47825837805867799, -1.443375672974058777 ) ) ;
#10531 = CARTESIAN_POINT ( 'NONE',  ( -5.932574734431526942, 9.079031735882207244, 1.199719254218454489 ) ) ;
#10532 = CARTESIAN_POINT ( 'NONE',  ( -0.02224634325198420262, -0.007204097619508141419, -2.289079630542791399 ) ) ;
#10534 = ORIENTED_EDGE ( 'NONE', *, *, #86344, .F. ) ;
#10533 = CARTESIAN_POINT ( 'NONE',  ( -5.601453741101424022, 6.564059448486966986, -1.199719254218453823 ) ) ;
#10535 = CARTESIAN_POINT ( 'NONE',  ( -7.009202228140739344, 11.12122699956546334, -0.7216878364870267237 ) ) ;
#10536 = CARTESIAN_POINT ( 'NONE',  ( 2.274722540679521288, -1.357913018379176995, 1.739418515187239223 ) ) ;
#10537 = CARTESIAN_POINT ( 'NONE',  ( 3.285556943750000070, -0.6343749995220415716, 0.000000000000000000 ) ) ;
#10538 = CARTESIAN_POINT ( 'NONE',  ( 6.403176761927252159, -1.659045864033869666, 1.046607237317781269 ) ) ;
#10539 = CARTESIAN_POINT ( 'NONE',  ( 1.364683531249990311, 5.676041667008088432, 0.7879004041258500513 ) ) ;
#10540 = CARTESIAN_POINT ( 'NONE',  ( -0.7500000000000215383, 3.972916667349481123, 1.299038105676671107 ) ) ;
#10541 = CARTESIAN_POINT ( 'NONE',  ( 5.889294496748854968, 6.159041356224602026, -0.8323295365256941913 ) ) ;
#10542 = CARTESIAN_POINT ( 'NONE',  ( 0.1749903794560592751, 2.884130749173496877, -2.444045186936738112 ) ) ;
#10543 = CARTESIAN_POINT ( 'NONE',  ( 5.613187951484799321, -1.795345830453990654, 0.4073638586896133340 ) ) ;
#10544 = ORIENTED_EDGE ( 'NONE', *, *, #147046, .T. ) ;
#10545 = CARTESIAN_POINT ( 'NONE',  ( -1.225000000000024736, 2.562500000682817358, -1.908195823574487804E-14 ) ) ;
#10546 = ADVANCED_FACE ( 'NONE', ( #50868 ), #173918, .T. ) ;
#10547 = CARTESIAN_POINT ( 'NONE',  ( -5.533699252672048985, 9.607732894759390518, -0.7998128361456231517 ) ) ;
#10548 = CARTESIAN_POINT ( 'NONE',  ( -3.009396220815599321, 6.452359640394901952, 0.6004564335717228474 ) ) ;
#10549 = CARTESIAN_POINT ( 'NONE',  ( 6.539320575229233157, 0.001224430076711413356, 2.103502572931112091 ) ) ;
#10550 = CARTESIAN_POINT ( 'NONE',  ( 9.976179289984715481, 9.863349661746255492, -6.608275209389087301 ) ) ;
#10551 = CARTESIAN_POINT ( 'NONE',  ( 5.229694566569264680, 7.124396299129368337, 1.599625672291267398 ) ) ;
#10552 = CARTESIAN_POINT ( 'NONE',  ( 0.3388364525104338165, 0.3516977924403408284, 2.030485180972623205 ) ) ;
#10555 = CARTESIAN_POINT ( 'NONE',  ( 4.282634502089007533, 1.642705626968201216, -0.8318752211165170163 ) ) ;
#10554 = CARTESIAN_POINT ( 'NONE',  ( 2.101794631558097315, 0.7159089574285321111, -1.718054499674229074 ) ) ;
#10553 = CARTESIAN_POINT ( 'NONE',  ( -9.770225302207578011, 4.446947604919802011, 6.899101747692366615 ) ) ;
#10556 = CARTESIAN_POINT ( 'NONE',  ( 7.796102023057898123, 9.054206100777749455, -1.199719254218441611 ) ) ;
#10557 = CARTESIAN_POINT ( 'NONE',  ( -9.380315451526849202, 14.53091799469200396, -7.483989755400268784 ) ) ;
#10558 = COLOUR_RGB ( '', 0.40784314, 0.44705882, 0.49803922) ;
#10559 = CARTESIAN_POINT ( 'NONE',  ( -4.281342646865346602, 8.216926531310035031, 0.7998128361456352531 ) ) ;
#10560 = ORIENTED_EDGE ( 'NONE', *, *, #10274, .F. ) ;
#10561 = CARTESIAN_POINT ( 'NONE',  ( 4.494872972331320327, -0.4818267175418550208, -2.153482813429814069 ) ) ;
#10562 = CARTESIAN_POINT ( 'NONE',  ( 5.888003241735360938, -1.025016604251761221, 2.016990234832950701 ) ) ;
#10563 = CARTESIAN_POINT ( 'NONE',  ( -5.260200412422200600, 8.120355666925794580, -1.082531754730544860 ) ) ;
#10564 = CARTESIAN_POINT ( 'NONE',  ( 5.800986464141828058, -0.2745434460682676936, -1.790553645544520345 ) ) ;
#10565 = CARTESIAN_POINT ( 'NONE',  ( -0.01248194115436446205, -0.5331630387654020531, 1.944732228473695868 ) ) ;
#10566 = EDGE_CURVE ( 'NONE', #105092, #73686, #214205, .T. ) ;
#10567 = CARTESIAN_POINT ( 'NONE',  ( 3.947104627881618200, 8.980740528188865923, 0.7749999999999996891 ) ) ;
#10568 = CARTESIAN_POINT ( 'NONE',  ( 6.890000000000050306, -0.002781820520068867264, 1.999840353888074240 ) ) ;
#10569 = CARTESIAN_POINT ( 'NONE',  ( 5.514289750425454883, -1.912461473380810961, 0.004301308668797076962 ) ) ;
#10570 = CARTESIAN_POINT ( 'NONE',  ( -11.01135777277262129, 13.40000000000000036, -1.400000000000001910 ) ) ;
#10571 = EDGE_CURVE ( 'NONE', #26620, #83476, #10314, .T. ) ;
#10572 = CARTESIAN_POINT ( 'NONE',  ( 0.4087956859853311142, 1.625333209436867321, 0.9259686016569528277 ) ) ;
#10573 = CARTESIAN_POINT ( 'NONE',  ( 2.852750215419812108, -1.865046845876184189, -0.7672916333427428626 ) ) ;
#10575 = CARTESIAN_POINT ( 'NONE',  ( 4.406922956430887162, 1.628233754946675882, -1.335794222675233511 ) ) ;
#10574 = CARTESIAN_POINT ( 'NONE',  ( -9.826962411806732689, 10.35921099006301382, -0.7998128361456291469 ) ) ;
#10576 = CARTESIAN_POINT ( 'NONE',  ( 9.257519960032755790, 9.694861462993381807, 0.7998128361456462443 ) ) ;
#10578 = CARTESIAN_POINT ( 'NONE',  ( -9.176171038350775078, 9.599954387697719582, -0.7998128361456291469 ) ) ;
#10577 = CARTESIAN_POINT ( 'NONE',  ( -0.7500000000000215383, 0.1916666666666871910, 1.299038105676659116 ) ) ;
#10579 =( NAMED_UNIT ( * ) SI_UNIT ( $, .STERADIAN. ) SOLID_ANGLE_UNIT ( ) );
#10580 = CARTESIAN_POINT ( 'NONE',  ( 3.129170305635332383, 1.827809467758968243, 0.8596994449004448091 ) ) ;
#10581 = CARTESIAN_POINT ( 'NONE',  ( -0.6823417656249969321, 3.217708333674754062, -1.181850606188749264 ) ) ;
#10582 = CARTESIAN_POINT ( 'NONE',  ( 2.900554798319789906, 5.471398800426671372, 1.199719254218452047 ) ) ;
#10583 = CARTESIAN_POINT ( 'NONE',  ( 4.921240491056324551, -0.1114908479964340365, 2.158860929761210912 ) ) ;
#10584 = CARTESIAN_POINT ( 'NONE',  ( 7.635176783151273128, 8.936736330878529699, 1.199719254218452935 ) ) ;
#10585 = CARTESIAN_POINT ( 'NONE',  ( -1.001543065824772872E-14, 5.462500000000020783, 1.732050807568877637 ) ) ;
#10587 = CARTESIAN_POINT ( 'NONE',  ( -9.486534023829914730, -9.006863021369436950, 0.5123739589067574096 ) ) ;
#10586 = CARTESIAN_POINT ( 'NONE',  ( 8.154303043976348420, 8.478051404252736845, 0.7998128361456281477 ) ) ;
#10588 = CARTESIAN_POINT ( 'NONE',  ( 8.066738210006674237, 11.39464976410773467, 1.082531754730558626 ) ) ;
#10589 = CARTESIAN_POINT ( 'NONE',  ( 1.680376142759659075, -1.205403815041187210, -1.805639882349929781 ) ) ;
#10591 = CARTESIAN_POINT ( 'NONE',  ( 0.5558949066124979632, -1.334021266253348381, 1.269314063962425854 ) ) ;
#10590 = CARTESIAN_POINT ( 'NONE',  ( -7.212574532790102744, 8.477387045419011002, -1.082531754730550855 ) ) ;
#10592 = CARTESIAN_POINT ( 'NONE',  ( -1.364683531250012516, 2.488541667008088876, -0.7879004041258289570 ) ) ;
#10593 = CARTESIAN_POINT ( 'NONE',  ( 1.786939262935317130, 1.904797134731281538, -1.083727916527020607 ) ) ;
#10594 = CARTESIAN_POINT ( 'NONE',  ( 6.142902043169038429, 7.013529245237516641, 0.9864344219776898237 ) ) ;
#10595 = CARTESIAN_POINT ( 'NONE',  ( 3.133911187764222728, -1.518274094020392706, -1.677614996870570918 ) ) ;
#10596 = CARTESIAN_POINT ( 'NONE',  ( -8.342344591110322227, 8.627156865917170236, -0.7998128361456291469 ) ) ;
#10597 = CARTESIAN_POINT ( 'NONE',  ( -1.364683531249997417, 5.321875000341417916, 1.214306433183764966E-14 ) ) ;
#10598 = CARTESIAN_POINT ( 'NONE',  ( 5.654245663017247736, 7.339362581565530341, 1.229167601055790815 ) ) ;
#10599 = CARTESIAN_POINT ( 'NONE',  ( -6.009258394948636914E-15, 11.93750000000000000, -1.732050807568875195 ) ) ;
#10600 = CARTESIAN_POINT ( 'NONE',  ( 5.058600711674583472, 8.915801573680086634, 0.000000000000000000 ) ) ;
#10601 =( BOUNDED_SURFACE ( )  B_SPLINE_SURFACE ( 1, 2, ( 
 ( #75386, #139333, #8239, #24473, #125285, #60191, #126351, #73226, #6083, #122087, #138263, #74322, #56997, #191245, #140419, #109018, #206437, #104693, #106872, #172899, #175037, #55932, #90587, #154505, #192311, #124227, #190186, #41842, #207508, #107954, #170744, #157715, #173981, #25553, #42909, #9312, #141500, #26623, #158771, #10366, #22329, #72154, #188049, #39680, #105789, #171815, #78573, #15691, #45040, #159833, #47175, #176097, #93794, #195538, #212829, #12501, #196597, #31974, #110085, #129553, #30918, #98053, #11433, #178229, #127424, #77509, #14625, #96994, #144693, #43970, #27697, #211762, #143629, #130609, #80720, #48240, #210706, #128493, #114353, #163046, #209624, #81777, #164107, #62334, #147859, #213875, #193396, #146811, #161981, #180349, #61265, #194461, #111153, #113288, #112222, #13572, #63400, #28771, #177153, #94853, #160904, #29844, #65497, #46104, #179295, #95926, #131645, #79645, #145761, #64467, #67618, #84968, #53536, #19953, #52473, #101211, #70822, #99106, #199770, #82835, #118599, #165157, #4747, #50344, #184587, #116465, #103359, #36205, #167297, #100157, #16750, #117536, #66551, #148910, #168358, #102281, #83894, #197647, #115410, #151060, #484, #69761, #86037, #135867, #166220, #133762, #201886, #152113, #132693, #169422, #37286, #149984, #185655, #21005, #198700, #3684, #18883, #119668, #33028, #17810, #182457, #134817, #51415, #2623, #68694, #34085, #1557, #183531, #35137, #200822, #87102, #153172, #49294, #181403, #29318, #136938, #155311, #6894, #72972, #24215, #210176, #176636, #209102, #40508, #13044, #38354, #139077, #172639, #205101, #90317, #110634, #56742, #10908, #39422, #202965, #105516, #122910, #159311, #120753, #193937, #188868, #45584, #187794, #28248, #94341, #61816, #106612, #5820, #76984, #143110, #111701, #60740, #138003, #186731, #71895, #104432, #88177, #95413, #204020, #126902, #44518, #171550, #170480, #78060, #160383, #22065, #55668, #11983, #23145, #177708, #54605, #89261, #192860, #144185, #127984, #161464, #154248, #121824, #214404, #183013, #63942, #164644, #113840, #212307, #14100, #197133, #99639, #97534, #162527, #163591, #147340, #50891, #16227, #80190, #62869, #146295, #195012, #30392, #34630, #130097, #82310, #198188, #179836, #112768, #17296, #181938, #46645, #196091, #49823, #47723, #117014, #145239, #31457, #64989, #81261, #213368, #165707, #1040, #79123, #66034, #100700, #15174, #148405, #131144, #48771, #114886, #180885, #83373, #178780, #132182, #96480, #166777, #32507, #115948, #98582, #199244, #33568, #149457, #67103, #133239, #211244, #129036, #51965, #203504, #71374, #119149, #18373, #150538, #186203, #134306, #104989, #55156, #171030, #201374, #102842, #22626, #137489, #118088, #204573, #72450, #185131, #6379, #138550, #101769, #121303, #136422, #88736, #68176, #53015, #184074, #169959, #86586, #202438, #37838, #3169, #200314, #69240, #35693, #152652, #154792, #167837, #87657, #84450, #122385, #2102, #36757, #168898, #20501, #120230, #56222, #187277, #153726, #54093, #106090, #19435, #4236, #103914, #70306, #21546, #38905, #5295, #188342, #135357, #85515, #39981, #151601, #207784, #155860, #11716, #9593, #77790, #8524, #208842, #126629, #94073, #160114, #73527, #26902, #172112, #61542, #23705, #190466, #42125, #108238, #59411, #27980, #60472, #93006, #75669, #45312, #139629, #174262, #125568, #25834, #191529, #142836, #91943, #43193, #74605, #89815, #140709, #158005, #109306, #7447, #143911, #141777, #209904, #206724, #192593, #44247, #127708, #175316, #41056, #159051, #10643, #193669, #76719, #173190, #205652, #107165, #57289, #123452, #189414, #24770, #110368, #176374, #58351, #90873, #156935, #124507, #12771, #112492, #82047, #79915, #83110, #177435, #162252, #97262, #113565, #179568, #131915, #33299, #111430, #32243, #765, #96203, #196870, #146023, #30113, #46373, #14898, #197924, #210971, #98314, #78845, #132975, #178503, #164378, #13839, #17032, #15963, #80992, #212034, #144965, #31189, #194735, #62599, #148140, #214142, #63676, #29052, #95135, #64733, #128761, #49552, #65768, #115678, #129830, #195813, #181672, #99384 ),
 ( #165436, #47450, #163316, #198977, #161185, #149190, #147080, #213102, #130877, #48508, #66832, #114628, #180618, #68981, #53835, #118889, #71117, #3977, #85252, #36500, #185943, #102578, #86326, #151340, #152398, #20241, #202178, #19177, #52754, #70045, #54898, #184874, #35431, #5041, #67904, #100439, #136160, #116748, #34365, #168639, #119966, #101508, #37576, #21297, #182747, #103656, #169707, #153468, #167578, #2909, #137233, #87402, #134049, #203255, #50622, #51708, #200058, #166510, #18100, #84188, #150275, #135100, #1845, #201114, #117829, #183820, #92677, #157664, #76393, #10319, #11383, #143579, #106820, #142502, #141451, #110038, #73174, #58011, #123122, #174988, #91614, #207457, #42861, #8189, #139282, #74274, #56950, #9262, #159782, #205312, #158722, #23358, #127374, #89468, #41793, #107906, #173933, #125236, #93743, #60144, #208510, #59076, #111099, #189081, #25505, #191195, #75333, #108969, #126302, #26573, #192261, #140367, #155521, #206385, #43923, #176050, #7102, #77461, #27643, #209572, #124176, #61217, #193346, #44990, #40714, #172849, #24420, #90533, #156597, #190139, #178180, #160856, #46055, #78526, #128446, #66507, #113241, #130562, #147812, #30869, #48195, #79597, #177105, #145716, #96947, #212782, #12448, #16704, #14578, #82790, #13525, #213831, #131599, #99057, #195490, #112175, #47125, #162997, #148863, #114307, #29795, #144643, #95879, #210659, #194412, #132648, #161934, #180305, #81730, #211714, #62286, #115366, #65449, #63351, #129509, #197601, #179245, #437, #28721, #80674, #146764, #64418, #196552, #49244, #165112, #94807, #98008, #198652, #31927, #164063, #15642, #181355, #32981, #50301, #136891, #1508, #37243, #83850, #137959, #183484, #103314, #35093, #22023, #169376, #19910, #18837, #149940, #36162, #199724, #67574, #87058, #20960, #2579, #116419, #34039, #69718, #17762, #202918, #153130, #54562, #84922, #200780, #120708, #4703, #185612, #102241, #70777, #186683, #104388, #88132, #51370, #38311, #85995, #170435, #166173, #151010, #133719, #53490, #184542, #152069, #135821, #101164, #117493, #167251, #68649, #168313, #154203, #134772, #5772, #182410, #71851, #100112, #52432, #118558, #3639, #201846, #203979, #119627, #124983, #173678, #143323, #171508, #57764, #91354, #157415, #93488, #42607, #206134, #9006, #142247, #75081, #190943, #140107, #108715, #58829, #158468, #123925, #25253, #174742, #55626, #141194, #90275, #27388, #56700, #23101, #26316, #187750, #105475, #207205, #10068, #24172, #208260, #43670, #121783, #92428, #76144, #175796, #156344, #189893, #159527, #59893, #122867, #126043, #39379, #6850, #155269, #192005, #109788, #41535, #11126, #188828, #77204, #89217, #72928, #139034, #205058, #107646, #40463, #106566, #172594, #7929, #74017, #95633, #213582, #112988, #80415, #14323, #211462, #96702, #180055, #128196, #63097, #82534, #60963, #97755, #16453, #210399, #31677, #64171, #147560, #131357, #115112, #163813, #48994, #32726, #197352, #178998, #146513, #161682, #212531, #12202, #209316, #129266, #79350, #62043, #65205, #194157, #46874, #45805, #15390, #127120, #130314, #81483, #181110, #29541, #30613, #195237, #98807, #164860, #193088, #111926, #110844, #78272, #28464, #162750, #177927, #44738, #196302, #176850, #47948, #94557, #114063, #160597, #144398, #13276, #145467, #198406, #186427, #118305, #150762, #68400, #36982, #99866, #38066, #1264, #151824, #53243, #183237, #182157, #86809, #103065, #50050, #149683, #119373, #117237, #120452, #188, #199470, #134528, #2325, #200534, #169121, #70523, #148620, #69466, #104135, #133467, #19663, #34841, #67323, #83601, #52180, #20716, #33787, #135571, #116171, #170181, #51112, #201595, #100916, #54314, #185360, #184292, #167004, #165929, #35917, #17514, #18595, #152875, #4453, #84674, #66256, #132404, #101993, #168061, #136640, #202664, #21769, #85739, #3397, #174484, #140932, #157160, #7670, #206946, #74833, #75890, #208011, #171250, #58576, #205880, #26061, #137707, #122605, #187499, #24996, #156084, #57514, #107393, #72679, #203728, #138775, #121530, #73756, #9814, #55375, #8751, #87877, #191755, #153950, #106311 ) ),
 .UNSPECIFIED., .F., .F., .F. ) 
 B_SPLINE_SURFACE_WITH_KNOTS ( ( 2, 2 ),
 ( 3, 2, 2, 2, 2, 2, 2, 2, 2, 2, 2, 2, 2, 2, 2, 2, 2, 2, 2, 2, 2, 2, 2, 2, 2, 2, 2, 2, 2, 2, 2, 2, 2, 2, 2, 2, 2, 2, 2, 2, 2, 2, 2, 2, 2, 2, 2, 2, 2, 2, 2, 2, 2, 2, 2, 2, 2, 2, 2, 2, 2, 2, 2, 2, 2, 2, 2, 2, 2, 2, 2, 2, 2, 2, 2, 2, 2, 2, 2, 2, 2, 2, 2, 2, 2, 2, 2, 2, 2, 2, 2, 2, 2, 2, 2, 2, 2, 2, 2, 2, 2, 2, 2, 2, 2, 2, 2, 2, 2, 2, 2, 2, 2, 2, 2, 2, 2, 2, 2, 2, 2, 2, 2, 2, 2, 2, 2, 2, 2, 2, 2, 2, 2, 2, 2, 2, 2, 2, 2, 2, 2, 2, 2, 2, 2, 2, 2, 2, 2, 2, 2, 2, 2, 2, 2, 2, 2, 2, 2, 2, 2, 2, 2, 2, 2, 2, 2, 2, 2, 2, 2, 2, 2, 2, 2, 2, 2, 2, 2, 2, 2, 2, 2, 2, 2, 2, 2, 2, 2, 2, 2, 2, 2, 2, 2, 2, 2, 2, 2, 2, 2, 2, 2, 2, 2, 2, 2, 2, 2, 2, 2, 2, 2, 2, 2, 2, 2, 2, 2, 2, 2, 2, 2, 2, 2, 2, 2, 2, 2, 2, 2, 2, 2, 2, 2, 2, 2, 2, 2, 2, 3 ),
 ( 0.000000000000000000, 1.000000000000000000 ),
 ( 0.000000000000000000, 0.004166666666666666609, 0.008333333333333333218, 0.01250000000000000069, 0.01666666666666666644, 0.02083333333333333218, 0.02500000000000000139, 0.02916666666666666713, 0.03333333333333333287, 0.03749999999999999861, 0.04166666666666666435, 0.04583333333333333010, 0.05000000000000000278, 0.05416666666666666852, 0.05833333333333333426, 0.06250000000000000000, 0.06666666666666666574, 0.07083333333333333148, 0.07499999999999999722, 0.07916666666666666297, 0.08333333333333332871, 0.08749999999999999445, 0.09166666666666666019, 0.09583333333333333981, 0.1000000000000000056, 0.1041666666666666713, 0.1083333333333333370, 0.1125000000000000028, 0.1166666666666666685, 0.1208333333333333343, 0.1250000000000000000, 0.1291666666666666796, 0.1333333333333333315, 0.1375000000000000111, 0.1416666666666666630, 0.1458333333333333426, 0.1499999999999999944, 0.1541666666666666741, 0.1583333333333333259, 0.1625000000000000056, 0.1666666666666666574, 0.1708333333333333370, 0.1749999999999999889, 0.1791666666666666685, 0.1833333333333333204, 0.1875000000000000000, 0.1916666666666666796, 0.1958333333333333315, 0.2000000000000000111, 0.2041666666666666630, 0.2083333333333333426, 0.2124999999999999944, 0.2166666666666666741, 0.2208333333333333259, 0.2250000000000000056, 0.2291666666666666574, 0.2333333333333333370, 0.2374999999999999889, 0.2416666666666666685, 0.2458333333333333204, 0.2500000000000000000, 0.2541666666666666519, 0.2583333333333333592, 0.2625000000000000111, 0.2666666666666666630, 0.2708333333333333148, 0.2750000000000000222, 0.2791666666666666741, 0.2833333333333333259, 0.2874999999999999778, 0.2916666666666666852, 0.2958333333333333370, 0.2999999999999999889, 0.3041666666666666408, 0.3083333333333333481, 0.3125000000000000000, 0.3166666666666666519, 0.3208333333333333592, 0.3250000000000000111, 0.3291666666666666630, 0.3333333333333333148, 0.3375000000000000222, 0.3416666666666666741, 0.3458333333333333259, 0.3499999999999999778, 0.3541666666666666852, 0.3583333333333333370, 0.3624999999999999889, 0.3666666666666666408, 0.3708333333333333481, 0.3750000000000000000, 0.3791666666666666519, 0.3833333333333333592, 0.3875000000000000111, 0.3916666666666666630, 0.3958333333333333148, 0.4000000000000000222, 0.4041666666666666741, 0.4083333333333333259, 0.4124999999999999778, 0.4166666666666666852, 0.4208333333333333370, 0.4249999999999999889, 0.4291666666666666408, 0.4333333333333333481, 0.4375000000000000000, 0.4416666666666666519, 0.4458333333333333592, 0.4500000000000000111, 0.4541666666666666630, 0.4583333333333333148, 0.4625000000000000222, 0.4666666666666666741, 0.4708333333333333259, 0.4749999999999999778, 0.4791666666666666852, 0.4833333333333333370, 0.4874999999999999889, 0.4916666666666666408, 0.4958333333333333481, 0.5000000000000000000, 0.5041666666666666519, 0.5083333333333333037, 0.5124999999999999556, 0.5166666666666667185, 0.5208333333333333703, 0.5250000000000000222, 0.5291666666666666741, 0.5333333333333333259, 0.5374999999999999778, 0.5416666666666666297, 0.5458333333333332815, 0.5500000000000000444, 0.5541666666666666963, 0.5583333333333333481, 0.5625000000000000000, 0.5666666666666666519, 0.5708333333333333037, 0.5749999999999999556, 0.5791666666666667185, 0.5833333333333333703, 0.5875000000000000222, 0.5916666666666666741, 0.5958333333333333259, 0.5999999999999999778, 0.6041666666666666297, 0.6083333333333332815, 0.6125000000000000444, 0.6166666666666666963, 0.6208333333333333481, 0.6250000000000000000, 0.6291666666666666519, 0.6333333333333333037, 0.6374999999999999556, 0.6416666666666667185, 0.6458333333333333703, 0.6500000000000000222, 0.6541666666666666741, 0.6583333333333333259, 0.6624999999999999778, 0.6666666666666666297, 0.6708333333333332815, 0.6750000000000000444, 0.6791666666666666963, 0.6833333333333333481, 0.6875000000000000000, 0.6916666666666666519, 0.6958333333333333037, 0.6999999999999999556, 0.7041666666666667185, 0.7083333333333333703, 0.7125000000000000222, 0.7166666666666666741, 0.7208333333333333259, 0.7249999999999999778, 0.7291666666666666297, 0.7333333333333332815, 0.7375000000000000444, 0.7416666666666666963, 0.7458333333333333481, 0.7500000000000000000, 0.7541666666666666519, 0.7583333333333333037, 0.7624999999999999556, 0.7666666666666667185, 0.7708333333333333703, 0.7750000000000000222, 0.7791666666666666741, 0.7833333333333333259, 0.7874999999999999778, 0.7916666666666666297, 0.7958333333333332815, 0.8000000000000000444, 0.8041666666666666963, 0.8083333333333333481, 0.8125000000000000000, 0.8166666666666666519, 0.8208333333333333037, 0.8249999999999999556, 0.8291666666666667185, 0.8333333333333333703, 0.8375000000000000222, 0.8416666666666666741, 0.8458333333333333259, 0.8499999999999999778, 0.8541666666666666297, 0.8583333333333332815, 0.8625000000000000444, 0.8666666666666666963, 0.8708333333333333481, 0.8750000000000000000, 0.8791666666666666519, 0.8833333333333333037, 0.8874999999999999556, 0.8916666666666667185, 0.8958333333333333703, 0.9000000000000000222, 0.9041666666666666741, 0.9083333333333333259, 0.9124999999999999778, 0.9166666666666666297, 0.9208333333333332815, 0.9250000000000000444, 0.9291666666666666963, 0.9333333333333333481, 0.9375000000000000000, 0.9416666666666666519, 0.9458333333333333037, 0.9499999999999999556, 0.9541666666666667185, 0.9583333333333333703, 0.9625000000000000222, 0.9666666666666666741, 0.9708333333333333259, 0.9749999999999999778, 0.9791666666666666297, 0.9833333333333332815, 0.9875000000000000444, 0.9916666666666666963, 0.9958333333333333481, 1.000000000000000000 ),
 .UNSPECIFIED. ) 
 GEOMETRIC_REPRESENTATION_ITEM ( )  RATIONAL_B_SPLINE_SURFACE ( (
 ( 1.000000000000000000, 0.8660254037844387076, 1.000000000000000000, 0.8660254037844387076, 1.000000000000000000, 0.8660254037844387076, 1.000000000000000000, 0.8660254037844387076, 1.000000000000000000, 0.8660254037844387076, 1.000000000000000000, 0.8660254037844387076, 1.000000000000000000, 0.8660254037844387076, 1.000000000000000000, 0.8660254037844387076, 1.000000000000000000, 0.8660254037844387076, 1.000000000000000000, 0.8660254037844387076, 1.000000000000000000, 0.8660254037844387076, 1.000000000000000000, 0.8660254037844387076, 1.000000000000000000, 0.8660254037844387076, 1.000000000000000000, 0.8660254037844387076, 1.000000000000000000, 0.8660254037844387076, 1.000000000000000000, 0.8660254037844387076, 1.000000000000000000, 0.8660254037844387076, 1.000000000000000000, 0.8660254037844387076, 1.000000000000000000, 0.8660254037844387076, 1.000000000000000000, 0.8660254037844387076, 1.000000000000000000, 0.8660254037844387076, 1.000000000000000000, 0.8660254037844387076, 1.000000000000000000, 0.8660254037844387076, 1.000000000000000000, 0.8660254037844387076, 1.000000000000000000, 0.8660254037844387076, 1.000000000000000000, 0.8660254037844387076, 1.000000000000000000, 0.8660254037844387076, 1.000000000000000000, 0.8660254037844387076, 1.000000000000000000, 0.8660254037844387076, 1.000000000000000000, 0.8660254037844387076, 1.000000000000000000, 0.8660254037844387076, 1.000000000000000000, 0.8660254037844387076, 1.000000000000000000, 0.8660254037844387076, 1.000000000000000000, 0.8660254037844387076, 1.000000000000000000, 0.8660254037844387076, 1.000000000000000000, 0.8660254037844387076, 1.000000000000000000, 0.8660254037844387076, 1.000000000000000000, 0.8660254037844387076, 1.000000000000000000, 0.8660254037844387076, 1.000000000000000000, 0.8660254037844387076, 1.000000000000000000, 0.8660254037844387076, 1.000000000000000000, 0.8660254037844387076, 1.000000000000000000, 0.8660254037844387076, 1.000000000000000000, 0.8660254037844387076, 1.000000000000000000, 0.8660254037844387076, 1.000000000000000000, 0.8660254037844387076, 1.000000000000000000, 0.8660254037844387076, 1.000000000000000000, 0.8660254037844387076, 1.000000000000000000, 0.8660254037844387076, 1.000000000000000000, 0.8660254037844387076, 1.000000000000000000, 0.8660254037844387076, 1.000000000000000000, 0.8660254037844387076, 1.000000000000000000, 0.8660254037844387076, 1.000000000000000000, 0.8660254037844387076, 1.000000000000000000, 0.8660254037844387076, 1.000000000000000000, 0.8660254037844387076, 1.000000000000000000, 0.8660254037844387076, 1.000000000000000000, 0.8660254037844387076, 1.000000000000000000, 0.8660254037844387076, 1.000000000000000000, 0.8660254037844387076, 1.000000000000000000, 0.8660254037844387076, 1.000000000000000000, 0.8660254037844387076, 1.000000000000000000, 0.8660254037844387076, 1.000000000000000000, 0.8660254037844387076, 1.000000000000000000, 0.8660254037844387076, 1.000000000000000000, 0.8660254037844387076, 1.000000000000000000, 0.8660254037844387076, 1.000000000000000000, 0.8660254037844387076, 1.000000000000000000, 0.8660254037844387076, 1.000000000000000000, 0.8660254037844387076, 1.000000000000000000, 0.8660254037844387076, 1.000000000000000000, 0.8660254037844387076, 1.000000000000000000, 0.8660254037844387076, 1.000000000000000000, 0.8660254037844387076, 1.000000000000000000, 0.8660254037844387076, 1.000000000000000000, 0.8660254037844387076, 1.000000000000000000, 0.8660254037844387076, 1.000000000000000000, 0.8660254037844387076, 1.000000000000000000, 0.8660254037844387076, 1.000000000000000000, 0.8660254037844387076, 1.000000000000000000, 0.8660254037844387076, 1.000000000000000000, 0.8660254037844387076, 1.000000000000000000, 0.8660254037844387076, 1.000000000000000000, 0.8660254037844387076, 1.000000000000000000, 0.8660254037844387076, 1.000000000000000000, 0.8660254037844387076, 1.000000000000000000, 0.8660254037844387076, 1.000000000000000000, 0.8660254037844387076, 1.000000000000000000, 0.8660254037844387076, 1.000000000000000000, 0.8660254037844387076, 1.000000000000000000, 0.8660254037844387076, 1.000000000000000000, 0.8660254037844387076, 1.000000000000000000, 0.8660254037844387076, 1.000000000000000000, 0.8660254037844387076, 1.000000000000000000, 0.8660254037844387076, 1.000000000000000000, 0.8660254037844387076, 1.000000000000000000, 0.8660254037844387076, 1.000000000000000000, 0.8660254037844387076, 1.000000000000000000, 0.8660254037844387076, 1.000000000000000000, 0.8660254037844387076, 1.000000000000000000, 0.8660254037844387076, 1.000000000000000000, 0.8660254037844387076, 1.000000000000000000, 0.8660254037844387076, 1.000000000000000000, 0.8660254037844387076, 1.000000000000000000, 0.8660254037844387076, 1.000000000000000000, 0.8660254037844387076, 1.000000000000000000, 0.8660254037844387076, 1.000000000000000000, 0.8660254037844387076, 1.000000000000000000, 0.8660254037844387076, 1.000000000000000000, 0.8660254037844387076, 1.000000000000000000, 0.8660254037844387076, 1.000000000000000000, 0.8660254037844387076, 1.000000000000000000, 0.8660254037844387076, 1.000000000000000000, 0.8660254037844387076, 1.000000000000000000, 0.8660254037844387076, 1.000000000000000000, 0.8660254037844387076, 1.000000000000000000, 0.8660254037844387076, 1.000000000000000000, 0.8660254037844387076, 1.000000000000000000, 0.8660254037844387076, 1.000000000000000000, 0.8660254037844387076, 1.000000000000000000, 0.8660254037844387076, 1.000000000000000000, 0.8660254037844387076, 1.000000000000000000, 0.8660254037844387076, 1.000000000000000000, 0.8660254037844387076, 1.000000000000000000, 0.8660254037844387076, 1.000000000000000000, 0.8660254037844387076, 1.000000000000000000, 0.8660254037844387076, 1.000000000000000000, 0.8660254037844387076, 1.000000000000000000, 0.8660254037844387076, 1.000000000000000000, 0.8660254037844387076, 1.000000000000000000, 0.8660254037844387076, 1.000000000000000000, 0.8660254037844387076, 1.000000000000000000, 0.8660254037844387076, 1.000000000000000000, 0.8660254037844387076, 1.000000000000000000, 0.8660254037844387076, 1.000000000000000000, 0.8660254037844387076, 1.000000000000000000, 0.8660254037844387076, 1.000000000000000000, 0.8660254037844387076, 1.000000000000000000, 0.8660254037844387076, 1.000000000000000000, 0.8660254037844387076, 1.000000000000000000, 0.8660254037844387076, 1.000000000000000000, 0.8660254037844387076, 1.000000000000000000, 0.8660254037844387076, 1.000000000000000000, 0.8660254037844387076, 1.000000000000000000, 0.8660254037844387076, 1.000000000000000000, 0.8660254037844387076, 1.000000000000000000, 0.8660254037844387076, 1.000000000000000000, 0.8660254037844387076, 1.000000000000000000, 0.8660254037844387076, 1.000000000000000000, 0.8660254037844387076, 1.000000000000000000, 0.8660254037844387076, 1.000000000000000000, 0.8660254037844387076, 1.000000000000000000, 0.8660254037844387076, 1.000000000000000000, 0.8660254037844387076, 1.000000000000000000, 0.8660254037844387076, 1.000000000000000000, 0.8660254037844387076, 1.000000000000000000, 0.8660254037844387076, 1.000000000000000000, 0.8660254037844387076, 1.000000000000000000, 0.8660254037844387076, 1.000000000000000000, 0.8660254037844387076, 1.000000000000000000, 0.8660254037844387076, 1.000000000000000000, 0.8660254037844387076, 1.000000000000000000, 0.8660254037844387076, 1.000000000000000000, 0.8660254037844387076, 1.000000000000000000, 0.8660254037844387076, 1.000000000000000000, 0.8660254037844387076, 1.000000000000000000, 0.8660254037844387076, 1.000000000000000000, 0.8660254037844387076, 1.000000000000000000, 0.8660254037844387076, 1.000000000000000000, 0.8660254037844387076, 1.000000000000000000, 0.8660254037844387076, 1.000000000000000000, 0.8660254037844387076, 1.000000000000000000, 0.8660254037844387076, 1.000000000000000000, 0.8660254037844387076, 1.000000000000000000, 0.8660254037844387076, 1.000000000000000000, 0.8660254037844387076, 1.000000000000000000, 0.8660254037844387076, 1.000000000000000000, 0.8660254037844387076, 1.000000000000000000, 0.8660254037844387076, 1.000000000000000000, 0.8660254037844387076, 1.000000000000000000, 0.8660254037844387076, 1.000000000000000000, 0.8660254037844387076, 1.000000000000000000, 0.8660254037844387076, 1.000000000000000000, 0.8660254037844387076, 1.000000000000000000, 0.8660254037844387076, 1.000000000000000000, 0.8660254037844387076, 1.000000000000000000, 0.8660254037844387076, 1.000000000000000000, 0.8660254037844387076, 1.000000000000000000, 0.8660254037844387076, 1.000000000000000000, 0.8660254037844387076, 1.000000000000000000, 0.8660254037844387076, 1.000000000000000000, 0.8660254037844387076, 1.000000000000000000, 0.8660254037844387076, 1.000000000000000000, 0.8660254037844387076, 1.000000000000000000, 0.8660254037844387076, 1.000000000000000000, 0.8660254037844387076, 1.000000000000000000, 0.8660254037844387076, 1.000000000000000000, 0.8660254037844387076, 1.000000000000000000, 0.8660254037844387076, 1.000000000000000000, 0.8660254037844387076, 1.000000000000000000, 0.8660254037844387076, 1.000000000000000000, 0.8660254037844387076, 1.000000000000000000, 0.8660254037844387076, 1.000000000000000000, 0.8660254037844387076, 1.000000000000000000, 0.8660254037844387076, 1.000000000000000000, 0.8660254037844387076, 1.000000000000000000, 0.8660254037844387076, 1.000000000000000000, 0.8660254037844387076, 1.000000000000000000, 0.8660254037844387076, 1.000000000000000000, 0.8660254037844387076, 1.000000000000000000, 0.8660254037844387076, 1.000000000000000000, 0.8660254037844387076, 1.000000000000000000, 0.8660254037844387076, 1.000000000000000000, 0.8660254037844387076, 1.000000000000000000, 0.8660254037844387076, 1.000000000000000000, 0.8660254037844387076, 1.000000000000000000, 0.8660254037844387076, 1.000000000000000000, 0.8660254037844387076, 1.000000000000000000, 0.8660254037844387076, 1.000000000000000000, 0.8660254037844387076, 1.000000000000000000, 0.8660254037844387076, 1.000000000000000000, 0.8660254037844387076, 1.000000000000000000, 0.8660254037844387076, 1.000000000000000000, 0.8660254037844387076, 1.000000000000000000, 0.8660254037844387076, 1.000000000000000000, 0.8660254037844387076, 1.000000000000000000, 0.8660254037844387076, 1.000000000000000000, 0.8660254037844387076, 1.000000000000000000, 0.8660254037844387076, 1.000000000000000000, 0.8660254037844387076, 1.000000000000000000, 0.8660254037844387076, 1.000000000000000000, 0.8660254037844387076, 1.000000000000000000, 0.8660254037844387076, 1.000000000000000000, 0.8660254037844387076, 1.000000000000000000, 0.8660254037844387076, 1.000000000000000000, 0.8660254037844387076, 1.000000000000000000, 0.8660254037844387076, 1.000000000000000000, 0.8660254037844387076, 1.000000000000000000, 0.8660254037844387076, 1.000000000000000000, 0.8660254037844387076, 1.000000000000000000),
 ( 1.000000000000000000, 0.8660254037844387076, 1.000000000000000000, 0.8660254037844387076, 1.000000000000000000, 0.8660254037844387076, 1.000000000000000000, 0.8660254037844387076, 1.000000000000000000, 0.8660254037844387076, 1.000000000000000000, 0.8660254037844387076, 1.000000000000000000, 0.8660254037844387076, 1.000000000000000000, 0.8660254037844387076, 1.000000000000000000, 0.8660254037844387076, 1.000000000000000000, 0.8660254037844387076, 1.000000000000000000, 0.8660254037844387076, 1.000000000000000000, 0.8660254037844387076, 1.000000000000000000, 0.8660254037844387076, 1.000000000000000000, 0.8660254037844387076, 1.000000000000000000, 0.8660254037844387076, 1.000000000000000000, 0.8660254037844387076, 1.000000000000000000, 0.8660254037844387076, 1.000000000000000000, 0.8660254037844387076, 1.000000000000000000, 0.8660254037844387076, 1.000000000000000000, 0.8660254037844387076, 1.000000000000000000, 0.8660254037844387076, 1.000000000000000000, 0.8660254037844387076, 1.000000000000000000, 0.8660254037844387076, 1.000000000000000000, 0.8660254037844387076, 1.000000000000000000, 0.8660254037844387076, 1.000000000000000000, 0.8660254037844387076, 1.000000000000000000, 0.8660254037844387076, 1.000000000000000000, 0.8660254037844387076, 1.000000000000000000, 0.8660254037844387076, 1.000000000000000000, 0.8660254037844387076, 1.000000000000000000, 0.8660254037844387076, 1.000000000000000000, 0.8660254037844387076, 1.000000000000000000, 0.8660254037844387076, 1.000000000000000000, 0.8660254037844387076, 1.000000000000000000, 0.8660254037844387076, 1.000000000000000000, 0.8660254037844387076, 1.000000000000000000, 0.8660254037844387076, 1.000000000000000000, 0.8660254037844387076, 1.000000000000000000, 0.8660254037844387076, 1.000000000000000000, 0.8660254037844387076, 1.000000000000000000, 0.8660254037844387076, 1.000000000000000000, 0.8660254037844387076, 1.000000000000000000, 0.8660254037844387076, 1.000000000000000000, 0.8660254037844387076, 1.000000000000000000, 0.8660254037844387076, 1.000000000000000000, 0.8660254037844387076, 1.000000000000000000, 0.8660254037844387076, 1.000000000000000000, 0.8660254037844387076, 1.000000000000000000, 0.8660254037844387076, 1.000000000000000000, 0.8660254037844387076, 1.000000000000000000, 0.8660254037844387076, 1.000000000000000000, 0.8660254037844387076, 1.000000000000000000, 0.8660254037844387076, 1.000000000000000000, 0.8660254037844387076, 1.000000000000000000, 0.8660254037844387076, 1.000000000000000000, 0.8660254037844387076, 1.000000000000000000, 0.8660254037844387076, 1.000000000000000000, 0.8660254037844387076, 1.000000000000000000, 0.8660254037844387076, 1.000000000000000000, 0.8660254037844387076, 1.000000000000000000, 0.8660254037844387076, 1.000000000000000000, 0.8660254037844387076, 1.000000000000000000, 0.8660254037844387076, 1.000000000000000000, 0.8660254037844387076, 1.000000000000000000, 0.8660254037844387076, 1.000000000000000000, 0.8660254037844387076, 1.000000000000000000, 0.8660254037844387076, 1.000000000000000000, 0.8660254037844387076, 1.000000000000000000, 0.8660254037844387076, 1.000000000000000000, 0.8660254037844387076, 1.000000000000000000, 0.8660254037844387076, 1.000000000000000000, 0.8660254037844387076, 1.000000000000000000, 0.8660254037844387076, 1.000000000000000000, 0.8660254037844387076, 1.000000000000000000, 0.8660254037844387076, 1.000000000000000000, 0.8660254037844387076, 1.000000000000000000, 0.8660254037844387076, 1.000000000000000000, 0.8660254037844387076, 1.000000000000000000, 0.8660254037844387076, 1.000000000000000000, 0.8660254037844387076, 1.000000000000000000, 0.8660254037844387076, 1.000000000000000000, 0.8660254037844387076, 1.000000000000000000, 0.8660254037844387076, 1.000000000000000000, 0.8660254037844387076, 1.000000000000000000, 0.8660254037844387076, 1.000000000000000000, 0.8660254037844387076, 1.000000000000000000, 0.8660254037844387076, 1.000000000000000000, 0.8660254037844387076, 1.000000000000000000, 0.8660254037844387076, 1.000000000000000000, 0.8660254037844387076, 1.000000000000000000, 0.8660254037844387076, 1.000000000000000000, 0.8660254037844387076, 1.000000000000000000, 0.8660254037844387076, 1.000000000000000000, 0.8660254037844387076, 1.000000000000000000, 0.8660254037844387076, 1.000000000000000000, 0.8660254037844387076, 1.000000000000000000, 0.8660254037844387076, 1.000000000000000000, 0.8660254037844387076, 1.000000000000000000, 0.8660254037844387076, 1.000000000000000000, 0.8660254037844387076, 1.000000000000000000, 0.8660254037844387076, 1.000000000000000000, 0.8660254037844387076, 1.000000000000000000, 0.8660254037844387076, 1.000000000000000000, 0.8660254037844387076, 1.000000000000000000, 0.8660254037844387076, 1.000000000000000000, 0.8660254037844387076, 1.000000000000000000, 0.8660254037844387076, 1.000000000000000000, 0.8660254037844387076, 1.000000000000000000, 0.8660254037844387076, 1.000000000000000000, 0.8660254037844387076, 1.000000000000000000, 0.8660254037844387076, 1.000000000000000000, 0.8660254037844387076, 1.000000000000000000, 0.8660254037844387076, 1.000000000000000000, 0.8660254037844387076, 1.000000000000000000, 0.8660254037844387076, 1.000000000000000000, 0.8660254037844387076, 1.000000000000000000, 0.8660254037844387076, 1.000000000000000000, 0.8660254037844387076, 1.000000000000000000, 0.8660254037844387076, 1.000000000000000000, 0.8660254037844387076, 1.000000000000000000, 0.8660254037844387076, 1.000000000000000000, 0.8660254037844387076, 1.000000000000000000, 0.8660254037844387076, 1.000000000000000000, 0.8660254037844387076, 1.000000000000000000, 0.8660254037844387076, 1.000000000000000000, 0.8660254037844387076, 1.000000000000000000, 0.8660254037844387076, 1.000000000000000000, 0.8660254037844387076, 1.000000000000000000, 0.8660254037844387076, 1.000000000000000000, 0.8660254037844387076, 1.000000000000000000, 0.8660254037844387076, 1.000000000000000000, 0.8660254037844387076, 1.000000000000000000, 0.8660254037844387076, 1.000000000000000000, 0.8660254037844387076, 1.000000000000000000, 0.8660254037844387076, 1.000000000000000000, 0.8660254037844387076, 1.000000000000000000, 0.8660254037844387076, 1.000000000000000000, 0.8660254037844387076, 1.000000000000000000, 0.8660254037844387076, 1.000000000000000000, 0.8660254037844387076, 1.000000000000000000, 0.8660254037844387076, 1.000000000000000000, 0.8660254037844387076, 1.000000000000000000, 0.8660254037844387076, 1.000000000000000000, 0.8660254037844387076, 1.000000000000000000, 0.8660254037844387076, 1.000000000000000000, 0.8660254037844387076, 1.000000000000000000, 0.8660254037844387076, 1.000000000000000000, 0.8660254037844387076, 1.000000000000000000, 0.8660254037844387076, 1.000000000000000000, 0.8660254037844387076, 1.000000000000000000, 0.8660254037844387076, 1.000000000000000000, 0.8660254037844387076, 1.000000000000000000, 0.8660254037844387076, 1.000000000000000000, 0.8660254037844387076, 1.000000000000000000, 0.8660254037844387076, 1.000000000000000000, 0.8660254037844387076, 1.000000000000000000, 0.8660254037844387076, 1.000000000000000000, 0.8660254037844387076, 1.000000000000000000, 0.8660254037844387076, 1.000000000000000000, 0.8660254037844387076, 1.000000000000000000, 0.8660254037844387076, 1.000000000000000000, 0.8660254037844387076, 1.000000000000000000, 0.8660254037844387076, 1.000000000000000000, 0.8660254037844387076, 1.000000000000000000, 0.8660254037844387076, 1.000000000000000000, 0.8660254037844387076, 1.000000000000000000, 0.8660254037844387076, 1.000000000000000000, 0.8660254037844387076, 1.000000000000000000, 0.8660254037844387076, 1.000000000000000000, 0.8660254037844387076, 1.000000000000000000, 0.8660254037844387076, 1.000000000000000000, 0.8660254037844387076, 1.000000000000000000, 0.8660254037844387076, 1.000000000000000000, 0.8660254037844387076, 1.000000000000000000, 0.8660254037844387076, 1.000000000000000000, 0.8660254037844387076, 1.000000000000000000, 0.8660254037844387076, 1.000000000000000000, 0.8660254037844387076, 1.000000000000000000, 0.8660254037844387076, 1.000000000000000000, 0.8660254037844387076, 1.000000000000000000, 0.8660254037844387076, 1.000000000000000000, 0.8660254037844387076, 1.000000000000000000, 0.8660254037844387076, 1.000000000000000000, 0.8660254037844387076, 1.000000000000000000, 0.8660254037844387076, 1.000000000000000000, 0.8660254037844387076, 1.000000000000000000, 0.8660254037844387076, 1.000000000000000000, 0.8660254037844387076, 1.000000000000000000, 0.8660254037844387076, 1.000000000000000000, 0.8660254037844387076, 1.000000000000000000, 0.8660254037844387076, 1.000000000000000000, 0.8660254037844387076, 1.000000000000000000, 0.8660254037844387076, 1.000000000000000000, 0.8660254037844387076, 1.000000000000000000, 0.8660254037844387076, 1.000000000000000000, 0.8660254037844387076, 1.000000000000000000, 0.8660254037844387076, 1.000000000000000000, 0.8660254037844387076, 1.000000000000000000, 0.8660254037844387076, 1.000000000000000000, 0.8660254037844387076, 1.000000000000000000, 0.8660254037844387076, 1.000000000000000000, 0.8660254037844387076, 1.000000000000000000, 0.8660254037844387076, 1.000000000000000000, 0.8660254037844387076, 1.000000000000000000, 0.8660254037844387076, 1.000000000000000000, 0.8660254037844387076, 1.000000000000000000, 0.8660254037844387076, 1.000000000000000000, 0.8660254037844387076, 1.000000000000000000, 0.8660254037844387076, 1.000000000000000000, 0.8660254037844387076, 1.000000000000000000, 0.8660254037844387076, 1.000000000000000000, 0.8660254037844387076, 1.000000000000000000, 0.8660254037844387076, 1.000000000000000000, 0.8660254037844387076, 1.000000000000000000, 0.8660254037844387076, 1.000000000000000000, 0.8660254037844387076, 1.000000000000000000, 0.8660254037844387076, 1.000000000000000000, 0.8660254037844387076, 1.000000000000000000, 0.8660254037844387076, 1.000000000000000000, 0.8660254037844387076, 1.000000000000000000, 0.8660254037844387076, 1.000000000000000000, 0.8660254037844387076, 1.000000000000000000, 0.8660254037844387076, 1.000000000000000000, 0.8660254037844387076, 1.000000000000000000, 0.8660254037844387076, 1.000000000000000000, 0.8660254037844387076, 1.000000000000000000, 0.8660254037844387076, 1.000000000000000000, 0.8660254037844387076, 1.000000000000000000, 0.8660254037844387076, 1.000000000000000000, 0.8660254037844387076, 1.000000000000000000, 0.8660254037844387076, 1.000000000000000000, 0.8660254037844387076, 1.000000000000000000, 0.8660254037844387076, 1.000000000000000000, 0.8660254037844387076, 1.000000000000000000, 0.8660254037844387076, 1.000000000000000000, 0.8660254037844387076, 1.000000000000000000, 0.8660254037844387076, 1.000000000000000000, 0.8660254037844387076, 1.000000000000000000, 0.8660254037844387076, 1.000000000000000000, 0.8660254037844387076, 1.000000000000000000) ) ) 
 REPRESENTATION_ITEM ( '' )  SURFACE ( )  );
#10602 = CARTESIAN_POINT ( 'NONE',  ( 4.200303217096891473, -0.5537481437246688509, -1.680960689856024537 ) ) ;
#10603 = CARTESIAN_POINT ( 'NONE',  ( 7.560643217915098191, 11.97250085420964716, -0.7998128361456291469 ) ) ;
#10604 = CARTESIAN_POINT ( 'NONE',  ( 1.044129769988952683, 0.8535497088724073311, -1.925424821390888663 ) ) ;
#10606 = CARTESIAN_POINT ( 'NONE',  ( 1.499999999999989120, 1.025000000000019007, 0.000000000000000000 ) ) ;
#10605 = CARTESIAN_POINT ( 'NONE',  ( -8.012344526598182026E-15, 10.04687500034140335, -1.575800808251669460 ) ) ;
#10607 = CARTESIAN_POINT ( 'NONE',  ( -4.716257332707368910, 6.595662536282280719, -1.599625672291271394 ) ) ;
#10608 = CARTESIAN_POINT ( 'NONE',  ( 6.345327396762703742, 0.3419173589993273477, -1.987050850726256979 ) ) ;
#10610 = EDGE_LOOP ( 'NONE', ( #177507, #184502, #89963, #50062 ) ) ;
#10609 = CARTESIAN_POINT ( 'NONE',  ( 5.115404481452859642, 1.485474843905653985, 1.036646722175238011 ) ) ;
#10611 = CARTESIAN_POINT ( 'NONE',  ( 8.062294901620731480, 12.55776115186623620, 1.040834085586084257E-14 ) ) ;
#10612 = CARTESIAN_POINT ( 'NONE',  ( 3.678450976403758066, -1.802590750232490491, -0.4997190347926713794 ) ) ;
#10613 = CARTESIAN_POINT ( 'NONE',  ( 3.871986384844767315, -2.040452582458017083, 0.3490408808229996662 ) ) ;
#10614 = MECHANICAL_DESIGN_GEOMETRIC_PRESENTATION_REPRESENTATION (  '', ( #239 ), #138667 ) ;
#10615 = CARTESIAN_POINT ( 'NONE',  ( -7.241463443030476732, 7.620997903056574430, 0.000000000000000000 ) ) ;
#10616 = CARTESIAN_POINT ( 'NONE',  ( -0.4019237886466871523, 10.72991455036742892, -1.499999999999998668 ) ) ;
#10617 = CARTESIAN_POINT ( 'NONE',  ( -5.070386261386537363, 5.017798181146802428, 1.214306433183764966E-14 ) ) ;
#10618 = CARTESIAN_POINT ( 'NONE',  ( 7.517069824134078537, 7.734612647770044092, 0.000000000000000000 ) ) ;
#10619 = CARTESIAN_POINT ( 'NONE',  ( -5.317849202849146195, 6.330384893147431136, -1.092305163593216388 ) ) ;
#10620 = CARTESIAN_POINT ( 'NONE',  ( 0.6823417656249864960, -1.073958332991911568, -1.181850606188749264 ) ) ;
#10621 = CARTESIAN_POINT ( 'NONE',  ( 4.105873170248697690, 0.6631157982108953908, -1.846516426336957784 ) ) ;
#10622 = CARTESIAN_POINT ( 'NONE',  ( 0.7552322466577044979, -2.000550463317086525, -0.2495714061315074117 ) ) ;
#10623 = CARTESIAN_POINT ( 'NONE',  ( -5.307090785106547415, 5.156303768904543894, -0.7998128361456362523 ) ) ;
#10624 = PRESENTATION_STYLE_ASSIGNMENT (( #74585 ) ) ;
#10625 = CARTESIAN_POINT ( 'NONE',  ( 1.545950201917587696, 1.868165254341861647, 0.09716206808172561660 ) ) ;
#10626 = CARTESIAN_POINT ( 'NONE',  ( 1.364683531249988535, 4.363541667008090208, 0.7879004041258500513 ) ) ;
#10627 = CARTESIAN_POINT ( 'NONE',  ( 3.164317521226766239, 2.013376229028215558, -0.004237188189804701709 ) ) ;
#10629 = CARTESIAN_POINT ( 'NONE',  ( 2.952857568058687043, -1.957288919824872186, -0.8077276291160383481 ) ) ;
#10628 = CARTESIAN_POINT ( 'NONE',  ( -6.317736394288148816, 8.393778431468064127, 1.443375672974078761 ) ) ;
#10630 = CARTESIAN_POINT ( 'NONE',  ( 0.08000000000000020983, 7.849261790823902629, -9.579665964948882007 ) ) ;
#10631 = CARTESIAN_POINT ( 'NONE',  ( 5.353992430378140099, -0.7485205528568983357, 1.930488744064068785 ) ) ;
#10632 = CARTESIAN_POINT ( 'NONE',  ( 2.898410978271408922, 6.603506251283770112, -0.7998128361456362523 ) ) ;
#10634 = CARTESIAN_POINT ( 'NONE',  ( 11.81907076198591966, 13.75731224596471769, 1.592066415281218505 ) ) ;
#10633 = CARTESIAN_POINT ( 'NONE',  ( 0.01142647129402651375, -2.049560973810752085, 0.4120210816158270117 ) ) ;
#10636 = ORIENTED_EDGE ( 'NONE', *, *, #5066, .T. ) ;
#10635 = CARTESIAN_POINT ( 'NONE',  ( 5.385714059857480862, 1.227405483141888132, 1.351559456777707835 ) ) ;
#10637 = CARTESIAN_POINT ( 'NONE',  ( 7.914208982075123799, 10.25632978388623684, -1.599625672291262513 ) ) ;
#10638 = CARTESIAN_POINT ( 'NONE',  ( 6.520158902582594784, 5.290451655907107309, -2.438235897557449405 ) ) ;
#10639 = CARTESIAN_POINT ( 'NONE',  ( 11.48888942944796021, 8.940748223555385010, 3.094007481724269315 ) ) ;
#10640 = CARTESIAN_POINT ( 'NONE',  ( 6.370183515248876382, 1.128980158350336049, 1.895982279999992359 ) ) ;
#10641 = CARTESIAN_POINT ( 'NONE',  ( 1.364683531250000748, 11.56770833367472839, -0.7879004041258355073 ) ) ;
#10642 = CARTESIAN_POINT ( 'NONE',  ( 6.252599623108594074, 1.892168639490459325, 0.2757424028280440753 ) ) ;
#10643 = CARTESIAN_POINT ( 'NONE',  ( -9.820183334999905256, 10.35130206712171130, 1.040834085586084257E-14 ) ) ;
#10644 =( BOUNDED_SURFACE ( )  B_SPLINE_SURFACE ( 3, 1, ( 
 ( #149942, #116421 ),
 ( #439, #65451 ),
 ( #66508, #100114 ),
 ( #148865, #49245 ),
 ( #132649, #50303 ),
 ( #81732, #198654 ),
 ( #85997, #147814 ) ),
 .UNSPECIFIED., .T., .F., .T. ) 
 B_SPLINE_SURFACE_WITH_KNOTS ( ( 4, 3, 4 ),
 ( 2, 2 ),
 ( 0.000000000000000000, 0.5000000000000000000, 1.000000000000000000 ),
 ( 0.000000000000000000, 1.000000000000000000 ),
 .UNSPECIFIED. ) 
 GEOMETRIC_REPRESENTATION_ITEM ( )  RATIONAL_B_SPLINE_SURFACE ( (
 ( 1.000000000000000000, 1.000000000000000000),
 ( 0.3333333333333333703, 0.3333333333333333703),
 ( 0.3333333333333333703, 0.3333333333333333703),
 ( 1.000000000000000000, 1.000000000000000000),
 ( 0.3333333333333333703, 0.3333333333333333703),
 ( 0.3333333333333333703, 0.3333333333333333703),
 ( 1.000000000000000000, 1.000000000000000000) ) ) 
 REPRESENTATION_ITEM ( '' )  SURFACE ( )  );
#10645 = CARTESIAN_POINT ( 'NONE',  ( 5.686755365928134687, 8.721966129303114101, 1.199719254218462483 ) ) ;
#10646 = CARTESIAN_POINT ( 'NONE',  ( -0.6801582343750403048, 2.463541667008038782, 1.178068619123829430 ) ) ;
#10647 = CARTESIAN_POINT ( 'NONE',  ( 3.755245360860917536, 5.404205559136275205, -1.443375672974051449 ) ) ;
#10648 = CARTESIAN_POINT ( 'NONE',  ( 0.4019237886466778820, 9.823664549684629321, 1.500000000000001554 ) ) ;
#10649 = CARTESIAN_POINT ( 'NONE',  ( 3.822509244049070887, 6.547012320444182798, -1.199719254218452047 ) ) ;
#10650 = ORIENTED_EDGE ( 'NONE', *, *, #170575, .T. ) ;
#10652 = EDGE_CURVE ( 'NONE', #108753, #32719, #85310, .T. ) ;
#10651 = AXIS2_PLACEMENT_3D ( 'NONE', #60312, #126471, #44089 ) ;
#10653 = CARTESIAN_POINT ( 'NONE',  ( -7.584860592202423035, 7.813701877183096833, -0.7998128361456362523 ) ) ;
#10654 = CARTESIAN_POINT ( 'NONE',  ( 0.07700591528354228110, 6.948790505698306141, -2.505847838500625979 ) ) ;
#10656 = CARTESIAN_POINT ( 'NONE',  ( 7.015418140428412386, 7.149352350113456822, 0.7998128361456331437 ) ) ;
#10655 = CARTESIAN_POINT ( 'NONE',  ( 0.2959466228873472438, -9.091099919222584091, -9.630212118911142483 ) ) ;
#10657 = CARTESIAN_POINT ( 'NONE',  ( -6.937452841262697234, -7.242250812743805000, 6.937452841262715886 ) ) ;
#10658 = CARTESIAN_POINT ( 'NONE',  ( -0.1405533004718703405, 5.725074605807632722, -2.314389626777931586 ) ) ;
#10659 = CARTESIAN_POINT ( 'NONE',  ( -4.921246572080546500, 8.685278734161874681, 1.214306433183764966E-14 ) ) ;
#10660 = CARTESIAN_POINT ( 'NONE',  ( 3.928111819657337911, 5.605883094398769195, 1.599625672291267398 ) ) ;
#10661 = CARTESIAN_POINT ( 'NONE',  ( 2.676555125969529048, 1.290216341703333436, -1.488019019629209572 ) ) ;
#10662 = CARTESIAN_POINT ( 'NONE',  ( 3.849232595480827079, 0.2440098934328518987, -2.001514877671112025 ) ) ;
#10663 = CARTESIAN_POINT ( 'NONE',  ( -7.157815033010924921, 10.43820240756634199, 1.199719254218453823 ) ) ;
#10664 = CARTESIAN_POINT ( 'NONE',  ( 6.827182134110199918, 0.5620517916639695688, 2.240906645742099190 ) ) ;
#10665 = CARTESIAN_POINT ( 'NONE',  ( 3.802820697025221630, 1.879323313303274734, 1.126966401794778250 ) ) ;
#10666 = DIRECTION ( 'NONE',  ( 0.000000000000000000, -1.000000000000000000, 0.000000000000000000 ) ) ;
#10667 = CARTESIAN_POINT ( 'NONE',  ( 1.711812753757115502, -1.912122584522325086, 0.2334695860961126246 ) ) ;
#10668 = CARTESIAN_POINT ( 'NONE',  ( -8.507905087775398556, 9.884643009614800135, 1.199719254218462483 ) ) ;
#10669 = CARTESIAN_POINT ( 'NONE',  ( -0.6311622855796981124, 3.299999999999983391, 0.3999999999999715450 ) ) ;
#10670 = CARTESIAN_POINT ( 'NONE',  ( 0.1329588055935214397, 0.7520877941899367647, -1.931583167801545819 ) ) ;
#10671 = CARTESIAN_POINT ( 'NONE',  ( 3.851925040058331806, 5.587274861525073355, -1.443375672974066548 ) ) ;
#10672 = CARTESIAN_POINT ( 'NONE',  ( 6.123478934866503742, 10.29580919065294431, 0.7998128361456462443 ) ) ;
#10673 = ADVANCED_FACE ( 'NONE', ( #148380 ), #99618, .T. ) ;
#10674 = CARTESIAN_POINT ( 'NONE',  ( 4.985647801523278133, 6.839675073242382553, -1.599625672291256295 ) ) ;
#10675 = CARTESIAN_POINT ( 'NONE',  ( -0.6125000000000262457, 1.208333333333311277, -1.060881119635962211 ) ) ;
#10676 = CARTESIAN_POINT ( 'NONE',  ( 6.048345925472191631, 7.189396680206621149, 1.082531754730549967 ) ) ;
#10677 = EDGE_LOOP ( 'NONE', ( #9586, #187528, #32539, #130158 ) ) ;
#10679 = CARTESIAN_POINT ( 'NONE',  ( 3.387361027847039185, 0.04724124570358113201, -2.012690625139363032 ) ) ;
#10678 = CARTESIAN_POINT ( 'NONE',  ( 5.935073298327618652, -1.338256116417003927, -1.264887592264056559 ) ) ;
#10680 = CARTESIAN_POINT ( 'NONE',  ( 4.358954191739877082, -0.8846011062542002978, 2.121510506163324372 ) ) ;
#10682 = CARTESIAN_POINT ( 'NONE',  ( 2.149040161283378936, 1.622117262959487549, -0.9118680782764712056 ) ) ;
#10681 = CARTESIAN_POINT ( 'NONE',  ( -0.1290005225502433017, 0.6921039065478848951, -2.255494067288220439 ) ) ;
#10683 = CARTESIAN_POINT ( 'NONE',  ( 7.635176783151273128, 8.936736330878529699, 1.199719254218452935 ) ) ;
#10684 = CARTESIAN_POINT ( 'NONE',  ( 11.97181042169641962, 11.37999999999999901, -0.8318531151397201562 ) ) ;
#10685 = FILL_AREA_STYLE ('',( #126670 ) ) ;
#10686 = CARTESIAN_POINT ( 'NONE',  ( -7.640183256500752584, 8.872300873127729304, -1.199719254218446718 ) ) ;
#10687 = CARTESIAN_POINT ( 'NONE',  ( -6.183927461608886844, 7.347575139032721303, 1.082531754730548412 ) ) ;
#10689 = CARTESIAN_POINT ( 'NONE',  ( 4.908994958506140982, 1.627828031611065152, 0.9215782234750914403 ) ) ;
#10688 = CARTESIAN_POINT ( 'NONE',  ( 4.599217410553211316, -0.5561919879800735211, 2.015351296096360656 ) ) ;
#10690 = CARTESIAN_POINT ( 'NONE',  ( 6.534666852106798096, 7.686494751288491578, -1.082531754730543083 ) ) ;
#10691 = VERTEX_POINT ( 'NONE', #198165 ) ;
#10692 = CARTESIAN_POINT ( 'NONE',  ( 2.973470450930305820, 6.532579092154530365, -0.5245438083391358308 ) ) ;
#10693 = DIRECTION ( 'NONE',  ( 0.000000000000000000, 0.000000000000000000, 1.000000000000000000 ) ) ;
#10694 = CARTESIAN_POINT ( 'NONE',  ( 6.445920802586958764, 0.6525945181424031016, -1.596887126696917791 ) ) ;
#10695 = CARTESIAN_POINT ( 'NONE',  ( -6.762819695118240659, 6.784377820593065600, 0.7998128361456341429 ) ) ;
#10696 = PRODUCT_DEFINITION_FORMATION_WITH_SPECIFIED_SOURCE ( 'ANY', '', #60975, .NOT_KNOWN. ) ;
#10697 = CARTESIAN_POINT ( 'NONE',  ( 1.160356219728400307, 1.032376606561947741, 1.393149478428891364 ) ) ;
#10698 = CARTESIAN_POINT ( 'NONE',  ( -4.779331034874314099, 14.55303417034376423, 10.96804219640860012 ) ) ;
#10699 = CARTESIAN_POINT ( 'NONE',  ( 8.002408263930250953, -6.836568542494980250, -7.346809171966436125 ) ) ;
#10700 = TOROIDAL_SURFACE ( 'NONE', #211399, 11.92000000000000348, 0.08000000000000000167 ) ;
#10701 = LINE ( 'NONE', #209958, #145088 ) ;
#10702 = CARTESIAN_POINT ( 'NONE',  ( 6.016515519638066856, 0.8726334679417474538, 1.988148615226674298 ) ) ;
#10703 = CARTESIAN_POINT ( 'NONE',  ( 4.371595934376539816, 1.770262903079304451, -0.4459408992859363319 ) ) ;
#10704 = CARTESIAN_POINT ( 'NONE',  ( 1.885527806591394961, -1.848987351811198998, 0.6559936482007988623 ) ) ;
#10705 = CARTESIAN_POINT ( 'NONE',  ( 6.503150284217945831, -0.1439854277452867481, 2.084527530714448407 ) ) ;
#10706 = CIRCLE ( 'NONE', #183731, 0.5000000000000015543 ) ;
#10707 = LINE ( 'NONE', #189472, #61281 ) ;
#10708 = DIRECTION ( 'NONE',  ( 0.000000000000000000, 0.000000000000000000, -1.000000000000000000 ) ) ;
#10709 = CARTESIAN_POINT ( 'NONE',  ( 6.913768267964901071, 10.15348118167935709, -1.199719254218441611 ) ) ;
#10710 = CARTESIAN_POINT ( 'NONE',  ( 2.877707679121459083, 0.3088738507561124558, -2.097740099398600400 ) ) ;
#10711 = DIRECTION ( 'NONE',  ( -0.9998476951563912696, 0.000000000000000000, 0.01745240643728004568 ) ) ;
#10712 = DIRECTION ( 'NONE',  ( 0.000000000000000000, 1.000000000000000000, 0.000000000000000000 ) ) ;
#10713 = CARTESIAN_POINT ( 'NONE',  ( -4.869203491162207520, 6.719169366249152731, -1.250126817991310757 ) ) ;
#10714 = CARTESIAN_POINT ( 'NONE',  ( 0.3036855567021545244, -1.598042064648269811, -1.315789336611736138 ) ) ;
#10716 = CARTESIAN_POINT ( 'NONE',  ( -1.500000000000008216, 13.28125000068279604, 3.469446951953614189E-15 ) ) ;
#10715 = DIRECTION ( 'NONE',  ( 0.000000000000000000, 1.000000000000000000, 0.000000000000000000 ) ) ;
#10718 = ORIENTED_EDGE ( 'NONE', *, *, #203693, .T. ) ;
#10717 = CARTESIAN_POINT ( 'NONE',  ( 3.756649600333416217, 2.210663847611141986, 0.2169408864148083815 ) ) ;
#10719 = CARTESIAN_POINT ( 'NONE',  ( 0.4054594355042361875, -1.236789717346518769, -1.937488090237641014 ) ) ;
#10721 = CARTESIAN_POINT ( 'NONE',  ( 6.702015009205530838, 0.7948373677021604022, -1.903462506645931640 ) ) ;
#10720 = CARTESIAN_POINT ( 'NONE',  ( 3.765413976293345844, 5.416068943807445635, 1.599625672291267398 ) ) ;
#10723 = CARTESIAN_POINT ( 'NONE',  ( 3.475000000000000533, -2.654166666666666785, 2.006292185433948827 ) ) ;
#10722 = CARTESIAN_POINT ( 'NONE',  ( 4.577813143269636065, 5.369812084349879555, -1.199719254218450271 ) ) ;
#10724 = CARTESIAN_POINT ( 'NONE',  ( 0.1331565106231571705, 2.881392620029461504, -2.434650611646618223 ) ) ;
#10725 = CARTESIAN_POINT ( 'NONE',  ( 5.231922985772964552, 1.814955821992572993, 0.3091130605668013231 ) ) ;
#10726 = CARTESIAN_POINT ( 'NONE',  ( -5.697837992078444991, 6.130623284354489222, -0.7472135431472062272 ) ) ;
#10727 = CARTESIAN_POINT ( 'NONE',  ( -0.2102771530458459603, 6.947233595868168798, -2.798738817348767949 ) ) ;
#10728 = CARTESIAN_POINT ( 'NONE',  ( 2.608071471510875039, -0.6576475463303601554, -1.594674760072743114 ) ) ;
#10729 = CARTESIAN_POINT ( 'NONE',  ( 1.727750297885573882, 0.7672897036171549834, -1.865047645237365215 ) ) ;
#10730 = CARTESIAN_POINT ( 'NONE',  ( 3.252836000005991046, 2.242300829042419785, -0.5054477054214584486 ) ) ;
#10731 = CARTESIAN_POINT ( 'NONE',  ( 2.530887537405112298, 2.193952394701288000, 0.5517939747049571686 ) ) ;
#10732 = CARTESIAN_POINT ( 'NONE',  ( 4.758481774355417748, 0.8053329972168337125, 1.946216683261194236 ) ) ;
#10733 = CARTESIAN_POINT ( 'NONE',  ( -6.048345925472225382, 8.149765894507963182, 1.443375672974058777 ) ) ;
#10735 = B_SPLINE_CURVE_WITH_KNOTS ( 'NONE', 3,
 ( #114074, #1276, #195249, #49005 ),
 .UNSPECIFIED., .F., .F.,
 ( 4, 4 ),
 ( 0.000000000000000000, 0.0001207671576358290770 ),
 .UNSPECIFIED. ) ;
#10734 = CARTESIAN_POINT ( 'NONE',  ( 3.286155083303475166, -1.742946490318267205, -0.3057894240724549628 ) ) ;
#10737 = CARTESIAN_POINT ( 'NONE',  ( 6.286719507307084065, 1.996765193862446885, -1.125943789698529818 ) ) ;
#10736 = CARTESIAN_POINT ( 'NONE',  ( 3.553645660113312399, 7.160020680191912845, -1.734723475976807094E-15 ) ) ;
#10738 = CARTESIAN_POINT ( 'NONE',  ( 4.435397664686764330, 0.7849604969769330420, -1.665558179074405620 ) ) ;
#10739 = CARTESIAN_POINT ( 'NONE',  ( -3.411848212133334446, 7.132240014130862171, 0.7998128361456341429 ) ) ;
#10740 = CARTESIAN_POINT ( 'NONE',  ( 4.487385655998873624, 7.218738451098584363, 1.082531754730558626 ) ) ;
#10741 = CARTESIAN_POINT ( 'NONE',  ( -1.500000000000013101, 3.379166666666691299, -0.8660254037844313801 ) ) ;
#10742 = CARTESIAN_POINT ( 'NONE',  ( 4.716832014018703667, -0.1092502567305031480, 2.188841582221649595 ) ) ;
#10743 = CARTESIAN_POINT ( 'NONE',  ( -3.653032323878261600, 6.349289246911547835, -1.199719254218452047 ) ) ;
#10744 = DIRECTION ( 'NONE',  ( 0.7592566023653005702, 0.6507913734559639396, 0.000000000000000000 ) ) ;
#10745 = CARTESIAN_POINT ( 'NONE',  ( 4.967269779104159788, 1.799668380515653920, 1.023422521214325309 ) ) ;
#10746 = CARTESIAN_POINT ( 'NONE',  ( 0.4093891192313535710, -1.913260280790154866, 0.6371585790938688598 ) ) ;
#10747 = CARTESIAN_POINT ( 'NONE',  ( -1.364683531250010295, 4.780208333674755394, 0.7879004041258379498 ) ) ;
#10748 = CARTESIAN_POINT ( 'NONE',  ( 3.475144788579834110, 0.04656949993332368254, -1.926097043150078791 ) ) ;
#10749 = CARTESIAN_POINT ( 'NONE',  ( -8.012344526598182026E-15, 9.046875000341405126, -1.575800808251669460 ) ) ;
#10750 = CARTESIAN_POINT ( 'NONE',  ( -3.145128448690317935, 5.652771709238564313, -1.082531754730549967 ) ) ;
#10751 = CARTESIAN_POINT ( 'NONE',  ( 0.01825978460381037782, -0.5840345307000054387, 2.143236301556954881 ) ) ;
#10752 = ORIENTED_EDGE ( 'NONE', *, *, #6489, .F. ) ;
#10753 = CARTESIAN_POINT ( 'NONE',  ( 1.499999999999821032, 7.388542872122531691, -4.154462424328212222 ) ) ;
#10754 = CARTESIAN_POINT ( 'NONE',  ( 4.436542580169809291, 6.199052314996659874, 1.599625672291267398 ) ) ;
#10755 = CARTESIAN_POINT ( 'NONE',  ( 8.013579835756319270, -5.223163706540481677, -7.501945787865609283 ) ) ;
#10756 = CARTESIAN_POINT ( 'NONE',  ( 11.22152876905117402, 8.821419385122529988, 4.110082514564867395 ) ) ;
#10757 = CARTESIAN_POINT ( 'NONE',  ( 3.544905708052195514, 7.357750102694700978, 0.1464419079581855410 ) ) ;
#10758 = CARTESIAN_POINT ( 'NONE',  ( 1.732786548908150648, -1.861864252656076912, -0.6185235971247132758 ) ) ;
#10759 = CARTESIAN_POINT ( 'NONE',  ( -1.364683531250012516, 1.592708333674756727, 0.7879004041258379498 ) ) ;
#10760 = LINE ( 'NONE', #76834, #202916 ) ;
#10761 = CARTESIAN_POINT ( 'NONE',  ( 5.037533845850875380, 1.831247050742194515, -0.7043679133837479345 ) ) ;
#10762 = CARTESIAN_POINT ( 'NONE',  ( -8.286004436246233951, 12.81875560892930466, 1.040834085586084257E-14 ) ) ;
#10763 = CARTESIAN_POINT ( 'NONE',  ( -5.707619481228822345, 7.681975366232176583, -1.443375672974051449 ) ) ;
#10764 = CARTESIAN_POINT ( 'NONE',  ( 6.666866396406604167, -1.974176978123330040, -0.8811043787171415342 ) ) ;
#10766 = VERTEX_POINT ( 'NONE', #163566 ) ;
#10765 = CARTESIAN_POINT ( 'NONE',  ( -0.2104748580754409182, 6.947232144882289795, -2.698723162346649662 ) ) ;
#10767 = CARTESIAN_POINT ( 'NONE',  ( 0.6823417656249917140, 4.342708333674755394, 1.181850606188765695 ) ) ;
#10768 = EDGE_CURVE ( 'NONE', #125996, #182627, #104485, .T. ) ;
#10769 = CARTESIAN_POINT ( 'NONE',  ( 6.925078400183515726, -0.002206826874838820583, 1.955452213090567160 ) ) ;
#10770 = CARTESIAN_POINT ( 'NONE',  ( 6.485661447747480324, 1.619333758318822536, 0.6201139256068515238 ) ) ;
#10772 = CARTESIAN_POINT ( 'NONE',  ( 2.595491417077447238, -0.6846416945752286098, 2.081959150545972914 ) ) ;
#10771 = CARTESIAN_POINT ( 'NONE',  ( -1.360316468750013108, 1.140625000341413564, -2.081668171172168513E-14 ) ) ;
#10773 = CARTESIAN_POINT ( 'NONE',  ( 4.383989010750934945, 1.503879422573949132, 1.750323999079455684 ) ) ;
#10774 = CARTESIAN_POINT ( 'NONE',  ( 6.309851081105539272, -2.045767358615140807, 0.2475669877257078710 ) ) ;
#10775 = CARTESIAN_POINT ( 'NONE',  ( 2.202979905913711178, -0.4252542987780962291, 1.894666818490578164 ) ) ;
#10776 = CARTESIAN_POINT ( 'NONE',  ( -5.165293336682207581, 8.009630745229104676, 1.082531754730548412 ) ) ;
#10777 = CARTESIAN_POINT ( 'NONE',  ( 11.81900460097218186, 11.25757134874136334, 1.592493057836596115 ) ) ;
#10778 = CARTESIAN_POINT ( 'NONE',  ( 4.816704082729271086, -0.7169179515637627009, -1.995842421597990413 ) ) ;
#10779 = CARTESIAN_POINT ( 'NONE',  ( 2.602185585689294367, -0.1948409242511044692, 2.006959980107574371 ) ) ;
#10780 = CARTESIAN_POINT ( 'NONE',  ( -6.060131475184148186, 6.172500930577367484, 0.7216878364870317197 ) ) ;
#10781 = CARTESIAN_POINT ( 'NONE',  ( 5.772568991252683190, -1.404203161598962968, 1.702366421003978392 ) ) ;
#10782 = CARTESIAN_POINT ( 'NONE',  ( -8.120407659942227241, 8.438506789546210030, 0.7998128361456341429 ) ) ;
#10783 = CARTESIAN_POINT ( 'NONE',  ( 8.992082194361556091, 11.51384853155376220, 1.599625672291279388 ) ) ;
#10784 = CARTESIAN_POINT ( 'NONE',  ( 0.1526014871912773629, -1.468541917219987836, 1.084465738218153064 ) ) ;
#10785 = CARTESIAN_POINT ( 'NONE',  ( -6.611536185319534908, 7.742488966741438716, 1.199719254218452047 ) ) ;
#10787 = CARTESIAN_POINT ( 'NONE',  ( -5.037045483985590266, 7.982112132234349566, -1.219308355916954412 ) ) ;
#10786 = CARTESIAN_POINT ( 'NONE',  ( -5.025714415505916577, 8.007183762769660262, 1.161964715574652196 ) ) ;
#10788 = FACE_OUTER_BOUND ( 'NONE', #93961, .T. ) ;
#10789 = ORIENTED_EDGE ( 'NONE', *, *, #36106, .F. ) ;
#10790 = CARTESIAN_POINT ( 'NONE',  ( 5.313377624208335703, -0.3045090135303843981, 2.038146128872863283 ) ) ;
#10791 = EDGE_CURVE ( 'NONE', #160452, #37010, #210978, .T. ) ;
#10792 = CARTESIAN_POINT ( 'NONE',  ( -0.2108831679771167866, 1.375689764684871808, -2.152500126786048185 ) ) ;
#10793 = CARTESIAN_POINT ( 'NONE',  ( -3.418627288940168096, 7.140148937072163804, -0.7998128361456281477 ) ) ;
#10794 = DIRECTION ( 'NONE',  ( 0.000000000000000000, 1.000000000000000000, 0.000000000000000000 ) ) ;
#10795 = CARTESIAN_POINT ( 'NONE',  ( 4.125652552961744490, -0.3430436748357457710, 1.990152796604119034 ) ) ;
#10797 = ORIENTED_EDGE ( 'NONE', *, *, #174895, .F. ) ;
#10796 = CARTESIAN_POINT ( 'NONE',  ( 1.499999999999985123, 0.2958333333333566517, -0.8660254037844323793 ) ) ;
#10799 = CARTESIAN_POINT ( 'NONE',  ( 9.408995418203971894, 11.03987807840189816, 1.082531754730549967 ) ) ;
#10798 = CARTESIAN_POINT ( 'NONE',  ( -5.991777542596674166, 5.955104985976372944, 0.000000000000000000 ) ) ;
#10800 = CARTESIAN_POINT ( 'NONE',  ( 7.741869408603235136, 8.990934717247309749, 1.199719254218462483 ) ) ;
#10801 = CARTESIAN_POINT ( 'NONE',  ( 3.819256682291353400, -0.1532216265913727837, 2.055260608361098473 ) ) ;
#10802 = CARTESIAN_POINT ( 'NONE',  ( 2.549454116737331244, -1.388485404012842261, 1.462446031800922253 ) ) ;
#10803 = VERTEX_POINT ( 'NONE', #7423 ) ;
#10804 = CARTESIAN_POINT ( 'NONE',  ( 1.896367326442722989, 3.293421909012314686, -0.4056650308922483128 ) ) ;
#10805 = CARTESIAN_POINT ( 'NONE',  ( 2.869522067586683711, 6.499526178826442013, 0.7998128361456362523 ) ) ;
#10807 = VERTEX_POINT ( 'NONE', #90850 ) ;
#10806 = CARTESIAN_POINT ( 'NONE',  ( -9.797921721691023933, 3.956598013261175772, -6.103348209225892163 ) ) ;
#10808 = CARTESIAN_POINT ( 'NONE',  ( 3.321638586175166719, -1.528507173905558014, 1.314795459203411676 ) ) ;
#10809 = CARTESIAN_POINT ( 'NONE',  ( 2.695044507329581673, -0.5773736025265225891, 1.748335772842606106 ) ) ;
#10810 = CARTESIAN_POINT ( 'NONE',  ( 1.366329765314050482, 2.272867617333930390, -0.3986118548820920537 ) ) ;
#10811 = CARTESIAN_POINT ( 'NONE',  ( 4.115782150200256950, 6.959440387612411349, 1.199719254218452047 ) ) ;
#10812 = CARTESIAN_POINT ( 'NONE',  ( 2.548304106926166490, 2.161049004374314464, 0.05582717182670697553 ) ) ;
#10813 = CARTESIAN_POINT ( 'NONE',  ( -6.144869935491728441, 8.192100896205577243, -1.599625672291263179 ) ) ;
#10814 = ORIENTED_EDGE ( 'NONE', *, *, #43321, .F. ) ;
#10815 = CARTESIAN_POINT ( 'NONE',  ( 0.6124999999999862776, 2.333333333333325932, 1.060881119635898040 ) ) ;
#10816 = CARTESIAN_POINT ( 'NONE',  ( 1.639302681421180852, -1.352760811461351187, -1.292285834730775074 ) ) ;
#10817 = ADVANCED_FACE ( 'NONE', ( #8503 ), #110742, .T. ) ;
#10818 = CARTESIAN_POINT ( 'NONE',  ( 5.858272006539261056, 0.7985356142178706707, 1.802671990260945156 ) ) ;
#10820 = CARTESIAN_POINT ( 'NONE',  ( 9.056483423804305488, 9.668244870634271848, 1.040834085586084257E-14 ) ) ;
#10819 = CARTESIAN_POINT ( 'NONE',  ( -1.201851678989727383E-14, 2.946875000341419248, -1.575800808251660134 ) ) ;
#10822 = CARTESIAN_POINT ( 'NONE',  ( 0.5048604690408053930, -0.7474223562033958101, -2.076596198196341003 ) ) ;
#10821 = CARTESIAN_POINT ( 'NONE',  ( -4.415151579544611238, 8.302760609444034046, -0.7998128361456281477 ) ) ;
#10823 = CARTESIAN_POINT ( 'NONE',  ( 6.725056259267968350, -1.891221747171191403, -0.8428681758992571105 ) ) ;
#10824 = CARTESIAN_POINT ( 'NONE',  ( 4.761938266897790761, 6.578680616179308771, 1.599625672291267398 ) ) ;
#10825 = CARTESIAN_POINT ( 'NONE',  ( -6.437424008390261854, 6.404749519410410485, 0.7998128361456341429 ) ) ;
#10826 = CARTESIAN_POINT ( 'NONE',  ( 6.539320575229233157, 0.001224430076711413356, 2.103502572931112091 ) ) ;
#10827 = CARTESIAN_POINT ( 'NONE',  ( 5.225445458360559847, -1.872321802520343414, 0.6175577138636638708 ) ) ;
#10828 = CARTESIAN_POINT ( 'NONE',  ( 6.205333298273250975, 1.755376394247827987, -0.9990029765977179732 ) ) ;
#10829 = CARTESIAN_POINT ( 'NONE',  ( 3.985262446249608903, -0.2245550567474114134, -2.296750103337093396 ) ) ;
#10830 = CARTESIAN_POINT ( 'NONE',  ( 2.676693276584718895, 1.350517573672470606, -1.558986216346124776 ) ) ;
#10831 = CARTESIAN_POINT ( 'NONE',  ( 5.666945020832167224, 8.594891043404107478, 1.082531754730558626 ) ) ;
#10832 = CARTESIAN_POINT ( 'NONE',  ( 4.518610335104485287, 8.493738834255713854, 0.000000000000000000 ) ) ;
#10833 = CARTESIAN_POINT ( 'NONE',  ( 4.386945222473598527, 7.275797305264619652, -1.199719254218452047 ) ) ;
#10834 = CARTESIAN_POINT ( 'NONE',  ( 1.364683531249986537, 1.717708333674749399, -0.7879004041258239610 ) ) ;
#10835 = CARTESIAN_POINT ( 'NONE',  ( -3.007788591379378040, 14.48002907089885483, 11.62584875609310231 ) ) ;
#10836 = CARTESIAN_POINT ( 'NONE',  ( 5.138177029454836564, 7.977995053463880382, 1.082531754730558626 ) ) ;
#10837 = CARTESIAN_POINT ( 'NONE',  ( 5.424361751532248199, 1.065549429306617446, 1.891644033573415040 ) ) ;
#10839 = CARTESIAN_POINT ( 'NONE',  ( 4.563899478665734755, -1.199029595066217313, 1.397436126395680267 ) ) ;
#10838 = CARTESIAN_POINT ( 'NONE',  ( -2.494337075234348777, 5.853884321174607663, -0.7216878364870267237 ) ) ;
#10841 = PLANE ( 'NONE',  #30498 ) ;
#10840 = CARTESIAN_POINT ( 'NONE',  ( -11.86239285000045740, 11.37999999999998302, 1.812080536912751283 ) ) ;
#10842 = CARTESIAN_POINT ( 'NONE',  ( 5.091441847573507928, -0.7891374179831472935, 2.044738775321436997 ) ) ;
#10843 = CARTESIAN_POINT ( 'NONE',  ( 1.249999999999964695, 8.500000000000000000, -9.921567416492218072 ) ) ;
#10844 = CARTESIAN_POINT ( 'NONE',  ( 6.649321564832020748, -1.812311508879884459, -1.354277771019767762 ) ) ;
#10845 = CARTESIAN_POINT ( 'NONE',  ( -3.992976280936286759, 7.825322551632388546, 0.2949607357299148802 ) ) ;
#10846 = CARTESIAN_POINT ( 'NONE',  ( 0.000000000000000000, 13.49999999999999822, 0.000000000000000000 ) ) ;
#10847 = CARTESIAN_POINT ( 'NONE',  ( 5.602183562003149042, 7.492195738860313092, 1.335281325244306982 ) ) ;
#10848 = CARTESIAN_POINT ( 'NONE',  ( -4.462041952228954500, 6.299077925724123617, -1.443375672974066548 ) ) ;
#10849 = CARTESIAN_POINT ( 'NONE',  ( 3.106226591306694651, 6.638031766584184368, 0.000000000000000000 ) ) ;
#10850 = CARTESIAN_POINT ( 'NONE',  ( 0.6195364366361589825, -0.9414703481081601044, -1.498462015107356882 ) ) ;
#10851 = CIRCLE ( 'NONE', #104268, 0.08000000000000020983 ) ;
#10852 = CARTESIAN_POINT ( 'NONE',  ( 5.654944829759325664, 0.3949471196958070918, 1.973809479704929704 ) ) ;
#10853 = CARTESIAN_POINT ( 'NONE',  ( 5.524057522564145728, 8.532151978711786100, 1.199719254218462483 ) ) ;
#10854 = CARTESIAN_POINT ( 'NONE',  ( 3.663195928028176063, -1.856456087625086182, -0.9943140874985546551 ) ) ;
#10855 = CARTESIAN_POINT ( 'NONE',  ( 3.198755040744692302, 1.733147561012362559, 0.8161988141396243623 ) ) ;
#10856 = CARTESIAN_POINT ( 'NONE',  ( -3.337985173046072340, 6.383183490859034137, 0.8077998227833966816 ) ) ;
#10857 = CARTESIAN_POINT ( 'NONE',  ( 4.176189586714727398, -1.010410353755032409, -1.690456409470885824 ) ) ;
#10858 = CARTESIAN_POINT ( 'NONE',  ( 5.396742217995451618, -1.971451684502657287, -0.4385051361721309937 ) ) ;
#10859 = CARTESIAN_POINT ( 'NONE',  ( 1.498681428038322050, 1.531199225506232553, -1.074333469806128427 ) ) ;
#10862 = ORIENTED_EDGE ( 'NONE', *, *, #211148, .T. ) ;
#10861 = CARTESIAN_POINT ( 'NONE',  ( 1.388764059443419407, -1.816923020173771830, -0.5969786173363604842 ) ) ;
#10860 = CARTESIAN_POINT ( 'NONE',  ( 5.092313435308955860, -1.712476623254995278, -0.2059198849207622417 ) ) ;
#10864 = CARTESIAN_POINT ( 'NONE',  ( 4.202664430556254160, 5.926194473780837413, 1.443375672974062551 ) ) ;
#10863 = CARTESIAN_POINT ( 'NONE',  ( 1.823171247573553311, 2.059948494222668014, 0.7922594597074559264 ) ) ;
#10865 = CARTESIAN_POINT ( 'NONE',  ( 1.364683531249988757, 2.196875000341415252, 1.214306433183764966E-14 ) ) ;
#10866 = CARTESIAN_POINT ( 'NONE',  ( 6.250445965835445428, -1.952298026214387194, -0.1936728439068043650 ) ) ;
#10867 = CARTESIAN_POINT ( 'NONE',  ( 7.076466111328892694, 10.34329533227067799, -1.199719254218441611 ) ) ;
#10868 = CARTESIAN_POINT ( 'NONE',  ( 11.45846087878779329, 12.50688399218553748, -3.566076377698155664 ) ) ;
#10869 = CARTESIAN_POINT ( 'NONE',  ( 0.6823417656249899377, 3.176041667008085323, -1.181850606188754593 ) ) ;
#10870 = CARTESIAN_POINT ( 'NONE',  ( -3.879604511804807032, 7.677955697080921738, 0.7998128361456341429 ) ) ;
#10871 = DIRECTION ( 'NONE',  ( 0.000000000000000000, 0.000000000000000000, 1.000000000000000000 ) ) ;
#10872 = EDGE_LOOP ( 'NONE', ( #73651, #77938 ) ) ;
#10873 = CARTESIAN_POINT ( 'NONE',  ( 1.768117254402020277, -2.054967671486531255, 0.2513356459030794410 ) ) ;
#10874 = CARTESIAN_POINT ( 'NONE',  ( -0.7499999999999972244, 3.358333333333359150, -1.299038105676652011 ) ) ;
#10875 = CARTESIAN_POINT ( 'NONE',  ( 4.638861114170084399, 8.563755066507100722, 0.7998128361456462443 ) ) ;
#10876 = CARTESIAN_POINT ( 'NONE',  ( -7.202405917357668663, 9.425892875049191488, 1.599625672291295375 ) ) ;
#10877 = CARTESIAN_POINT ( 'NONE',  ( 5.713835393516482952, 5.630839145382857680, 0.7998128361456352531 ) ) ;
#10878 = CARTESIAN_POINT ( 'NONE',  ( 6.217454246653871586, 1.762742247767977055, 1.178343227268910054 ) ) ;
#10879 = CARTESIAN_POINT ( 'NONE',  ( -3.084802633888621859, 6.542760806271256335, 0.3243353321068309092 ) ) ;
#10880 = CARTESIAN_POINT ( 'NONE',  ( -1.201851678989727383E-14, 3.071875000341420137, 1.575800808251672791 ) ) ;
#10882 = CARTESIAN_POINT ( 'NONE',  ( 10.05978679165993483, 11.79913468076720306, 1.082531754730548412 ) ) ;
#10881 = CARTESIAN_POINT ( 'NONE',  ( 1.500000000000035971, 7.750000000000000000, 10.64483442802187696 ) ) ;
#10883 = CARTESIAN_POINT ( 'NONE',  ( 5.307970166423544356, -1.730600239375930549, 1.034008556546859969 ) ) ;
#10884 = CARTESIAN_POINT ( 'NONE',  ( 4.874201634824506080, -1.902012294098894829, -0.2279625308443770371 ) ) ;
#10885 = LINE ( 'NONE', #75908, #107172 ) ;
#10886 = CARTESIAN_POINT ( 'NONE',  ( 2.823975127348026248, 1.215230906543849354, -1.823574674616668556 ) ) ;
#10887 = CARTESIAN_POINT ( 'NONE',  ( 0.1335669894368890498, 2.867242032283002562, -2.641834823421157719 ) ) ;
#10888 = CARTESIAN_POINT ( 'NONE',  ( -0.7500000000000215383, 0.4729166673494850093, 1.299038105676659116 ) ) ;
#10889 = CARTESIAN_POINT ( 'NONE',  ( 5.396744779746093457, -1.965104602953187563, -0.4368240711251635822 ) ) ;
#10890 = CARTESIAN_POINT ( 'NONE',  ( 1.652457426684301955, 1.892030339952909035, 0.2773405859870237133 ) ) ;
#10891 = CARTESIAN_POINT ( 'NONE',  ( -7.393273838153706201, 7.519907654134449615, 0.7998128361456341429 ) ) ;
#10893 = CARTESIAN_POINT ( 'NONE',  ( -0.1409997244346088141, -0.002808977843308038680, -2.000147647483838220 ) ) ;
#10892 = CARTESIAN_POINT ( 'NONE',  ( -4.473827502829599290, 4.321812962830357208, 0.7216878364870317197 ) ) ;
#10894 = CARTESIAN_POINT ( 'NONE',  ( 1.364683531249997417, 9.546875000341396245, 2.602085213965210642E-15 ) ) ;
#10896 = CARTESIAN_POINT ( 'NONE',  ( -7.605197822622922210, 7.837428646007010613, -0.7998128361456362523 ) ) ;
#10895 = CARTESIAN_POINT ( 'NONE',  ( 3.474242889556743652, -2.015522812629696237, -0.5555695364270489822 ) ) ;
#10898 = EDGE_LOOP ( 'NONE', ( #50583, #111180 ) ) ;
#10897 = CARTESIAN_POINT ( 'NONE',  ( 1.588428401085600461, -0.2480725091915989278, -1.706701089166535512 ) ) ;
#10899 = CARTESIAN_POINT ( 'NONE',  ( -1.607015867998808023, -0.9165151389911689872, 1.199999999999999734 ) ) ;
#10900 = CARTESIAN_POINT ( 'NONE',  ( 6.661133543015731462, 6.665743976473484267, -0.7998128361456281477 ) ) ;
#10901 = CARTESIAN_POINT ( 'NONE',  ( 0.009341296487024523809, -9.943660733012633202, 9.579650209538311145 ) ) ;
#10902 = CARTESIAN_POINT ( 'NONE',  ( 6.958662999125706961, -8.148356111791676071, -6.505896022970784287 ) ) ;
#10903 = CARTESIAN_POINT ( 'NONE',  ( 6.342516933094585418, 6.294024598232139667, 1.040834085586084257E-14 ) ) ;
#10904 = ORIENTED_EDGE ( 'NONE', *, *, #205115, .F. ) ;
#10905 = DIRECTION ( 'NONE',  ( 0.000000000000000000, 0.000000000000000000, 1.000000000000000000 ) ) ;
#10906 = ORIENTED_EDGE ( 'NONE', *, *, #83416, .F. ) ;
#10907 = CARTESIAN_POINT ( 'NONE',  ( 2.350024359177401490, 0.8526225883829393615, -1.598239438867412820 ) ) ;
#10908 = CARTESIAN_POINT ( 'NONE',  ( -4.706651882238427120, 8.642844295920152575, 1.040834085586084257E-14 ) ) ;
#10909 = ORIENTED_EDGE ( 'NONE', *, *, #46958, .F. ) ;
#10910 = CARTESIAN_POINT ( 'NONE',  ( 4.891794496432329886, 4.601515088792824670, -0.7998128361456211532 ) ) ;
#10911 = ORIENTED_EDGE ( 'NONE', *, *, #6116, .T. ) ;
#10912 = CARTESIAN_POINT ( 'NONE',  ( 4.050854035433010480, 7.948023151305657841, 0.000000000000000000 ) ) ;
#10913 = CARTESIAN_POINT ( 'NONE',  ( 3.633306742369224462, -0.1297899475344466980, 1.806866856981071967 ) ) ;
#10914 = CARTESIAN_POINT ( 'NONE',  ( -4.650083499807243115, 5.295740330745369207, -1.052294140492322283 ) ) ;
#10915 = CARTESIAN_POINT ( 'NONE',  ( 4.632932323280743780, 6.889805956345480986, 1.213532624337316124 ) ) ;
#10916 = EDGE_CURVE ( 'NONE', #14542, #45069, #56199, .T. ) ;
#10917 = CARTESIAN_POINT ( 'NONE',  ( 4.334314691326750513, -1.072585289120084440, 1.520660633866082634 ) ) ;
#10918 = CARTESIAN_POINT ( 'NONE',  ( 1.915515091613760656, -1.252924113133683237, -1.449102840280371618 ) ) ;
#10919 = CARTESIAN_POINT ( 'NONE',  ( 1.008509592878764183, 1.385430265305506170, -1.188947219173806413 ) ) ;
#10920 = CARTESIAN_POINT ( 'NONE',  ( -1.416652131158683492, 8.000043606524068096, -10.86080395187256187 ) ) ;
#10921 = CARTESIAN_POINT ( 'NONE',  ( -6.089020385868876062, 6.276481003034692030, -0.7216878364870337181 ) ) ;
#10922 = CIRCLE ( 'NONE', #52517, 11.92000000000000171 ) ;
#10923 = CARTESIAN_POINT ( 'NONE',  ( 5.148720134264945791, 7.772403765597828418, 1.171659602702241676 ) ) ;
#10924 = CARTESIAN_POINT ( 'NONE',  ( 5.707977696796493916, 7.405608897698303217, 1.328948192410238649 ) ) ;
#10925 = CARTESIAN_POINT ( 'NONE',  ( -4.559605246071217088, 3.300000000000025135, 0.7750000000000135669 ) ) ;
#10926 = CARTESIAN_POINT ( 'NONE',  ( 9.083599731475992201, 9.699880562917908122, 0.7216878364870438212 ) ) ;
#10927 = CARTESIAN_POINT ( 'NONE',  ( 6.157084851585769236, 1.612115889470520314, -1.131004145815546424 ) ) ;
#10928 = CARTESIAN_POINT ( 'NONE',  ( -5.525111292768871252, 6.404716915440499037, -1.199719254218446718 ) ) ;
#10929 = DIRECTION ( 'NONE',  ( 1.000000000000000000, 0.000000000000000000, 0.000000000000000000 ) ) ;
#10930 = CARTESIAN_POINT ( 'NONE',  ( 0.6563342376118604937, -1.512884991606887386, 1.443139479479842668 ) ) ;
#10931 = CARTESIAN_POINT ( 'NONE',  ( 8.959240580532112475, 9.346868853575953651, -0.7998128361456221525 ) ) ;
#10932 = CARTESIAN_POINT ( 'NONE',  ( 5.737312389570451643, -1.741366515823379757, 0.8240431586447917178 ) ) ;
#10933 = CARTESIAN_POINT ( 'NONE',  ( -5.205440912643032547, 8.160432600470439723, 1.199719254218452047 ) ) ;
#10934 = CARTESIAN_POINT ( 'NONE',  ( 1.289775909805501719, -0.8246113042270180049, 1.628811597173693393 ) ) ;
#10935 = CARTESIAN_POINT ( 'NONE',  ( 1.647397727484143592, -1.863059487452220386, 1.182652941231487453 ) ) ;
#10936 = CARTESIAN_POINT ( 'NONE',  ( 0.4019237886466778820, 10.32366454968463110, 1.500000000000001554 ) ) ;
#10937 = CARTESIAN_POINT ( 'NONE',  ( 1.212987991671743204, 1.561712320281399835, -1.103468303573502673 ) ) ;
#10938 = ORIENTED_EDGE ( 'NONE', *, *, #88956, .T. ) ;
#10939 = CARTESIAN_POINT ( 'NONE',  ( 6.825064197248748243, -1.799304382776808930, -0.8012231885662893793 ) ) ;
#10940 = CARTESIAN_POINT ( 'NONE',  ( 2.894010800797857108, -0.5660635412718226789, -1.857715926975093135 ) ) ;
#10941 = ORIENTED_EDGE ( 'NONE', *, *, #183326, .T. ) ;
#10942 = CARTESIAN_POINT ( 'NONE',  ( 0.4212496859960760953, 0.7689994822442263178, 1.863884711849304487 ) ) ;
#10944 = CARTESIAN_POINT ( 'NONE',  ( 6.455886261557550299, -0.6278800607443285609, 1.751925260802848827 ) ) ;
#10943 = CARTESIAN_POINT ( 'NONE',  ( -5.387385936583832802, 7.378645907471495846, -1.599625672291271394 ) ) ;
#10945 = CARTESIAN_POINT ( 'NONE',  ( 3.790386463472274148, 6.579812086429759788, 1.199719254218452047 ) ) ;
#10946 = DIRECTION ( 'NONE',  ( 0.000000000000000000, -2.168404344971008079E-15, 1.000000000000000000 ) ) ;
#10947 = CARTESIAN_POINT ( 'NONE',  ( 8.238550898598388628, 12.76339314834017102, 0.7998128361456462443 ) ) ;
#10948 = CARTESIAN_POINT ( 'NONE',  ( -4.120788623549732854, 6.895004929861607401, -1.199719254218452047 ) ) ;
#10949 = CARTESIAN_POINT ( 'NONE',  ( -7.045397100956844127, 8.248660034984974132, -1.199719254218452047 ) ) ;
#10950 = CARTESIAN_POINT ( 'NONE',  ( 2.033021410476544943, -1.955939774129427988, 0.9887309579383956049 ) ) ;
#10951 = CARTESIAN_POINT ( 'NONE',  ( 4.690757960648234359, 4.574898496952131133, 0.7216878364870317197 ) ) ;
#10952 =( GEOMETRIC_REPRESENTATION_CONTEXT ( 3 ) GLOBAL_UNCERTAINTY_ASSIGNED_CONTEXT ( ( #17993 ) ) GLOBAL_UNIT_ASSIGNED_CONTEXT ( ( #71744, #172486, #58725 ) ) REPRESENTATION_CONTEXT ( 'NONE', 'WORKASPACE' ) );
#10953 = CARTESIAN_POINT ( 'NONE',  ( 7.849244587668864348, 8.122149871893999062, 0.7998128361456291469 ) ) ;
#10954 = CARTESIAN_POINT ( 'NONE',  ( -15.75000000000000000, 9.799999999999982947, 1.799999999999999600 ) ) ;
#10955 = CARTESIAN_POINT ( 'NONE',  ( 2.297230901563730665, 1.410920830412419003, 1.158640757216542028 ) ) ;
#10956 = CARTESIAN_POINT ( 'NONE',  ( 4.867013957181530515, 5.740899707208986236, -1.082531754730548412 ) ) ;
#10957 = CARTESIAN_POINT ( 'NONE',  ( -3.602716132929368875, 5.226254793216122074, 1.599625672291267398 ) ) ;
#10958 = CARTESIAN_POINT ( 'NONE',  ( -5.897079639132071449, 7.258985838325384243, -1.264812401031592204 ) ) ;
#10959 = LINE ( 'NONE', #77034, #67322 ) ;
#10960 = CARTESIAN_POINT ( 'NONE',  ( 7.730120138085914583, 12.17022392774227768, 0.7998128361456462443 ) ) ;
#10962 = EDGE_CURVE ( 'NONE', #38441, #175466, #186729, .T. ) ;
#10961 = CARTESIAN_POINT ( 'NONE',  ( 1.014139625077722595, -0.8655271193952519537, -1.721200913303379654 ) ) ;
#10963 = CARTESIAN_POINT ( 'NONE',  ( 5.348475771816907809, -1.946495798708135938, -0.2439133590248846462 ) ) ;
#10964 = VECTOR ( 'NONE', #31462, 1000.000000000000000 ) ;
#10965 = CARTESIAN_POINT ( 'NONE',  ( -6.009258394948636914E-15, 14.68749999999999822, -1.732050807568875195 ) ) ;
#10966 = CARTESIAN_POINT ( 'NONE',  ( -7.497822643557261024, 8.706213491360317747, -1.199719254218446718 ) ) ;
#10967 = CARTESIAN_POINT ( 'NONE',  ( 5.823390672269506574, 6.752709524857930745, -1.199719254218446718 ) ) ;
#10968 = CARTESIAN_POINT ( 'NONE',  ( 5.267185993530860699, 2.112242253262315739, -0.5839428218426812034 ) ) ;
#10969 = CARTESIAN_POINT ( 'NONE',  ( 4.955668840994886359, 5.740367388370866131, 1.199719254218462483 ) ) ;
#10970 = ADVANCED_FACE ( 'NONE', ( #74584 ), #140687, .T. ) ;
#10971 = CARTESIAN_POINT ( 'NONE',  ( 4.522371119077151391, 0.9712943915625820157, 1.828230030883712498 ) ) ;
#10973 = CARTESIAN_POINT ( 'NONE',  ( 1.364683531249986537, 1.217708333674754950, -0.7879004041258239610 ) ) ;
#10972 = CARTESIAN_POINT ( 'NONE',  ( 8.790098660144264997, 13.29414747594432455, 8.101455065885630802 ) ) ;
#10974 = ORIENTED_EDGE ( 'NONE', *, *, #26823, .F. ) ;
#10975 = CARTESIAN_POINT ( 'NONE',  ( 4.342621253679892490, 0.5038326875656545800, -2.242679570940506739 ) ) ;
#10976 = CARTESIAN_POINT ( 'NONE',  ( 8.283668668269706714, 8.766627655843892697, 1.040834085586084257E-14 ) ) ;
#10978 = CARTESIAN_POINT ( 'NONE',  ( 1.001543065824772753E-15, -1.421874999522042327, 3.793834371823811669 ) ) ;
#10977 = CARTESIAN_POINT ( 'NONE',  ( 5.939880696562888751, 7.062853913145737295, -1.082531754730548412 ) ) ;
#10979 = CARTESIAN_POINT ( 'NONE',  ( 6.620655732516647518, 7.053381450551401421, 2.424417106520880161 ) ) ;
#10980 = CARTESIAN_POINT ( 'NONE',  ( -6.912678218121246942, 9.158153569265168770, 1.599625672291269396 ) ) ;
#10981 = CARTESIAN_POINT ( 'NONE',  ( 4.242085645372923430, 0.5190250516928176516, 1.871238508296804604 ) ) ;
#10982 = ORIENTED_EDGE ( 'NONE', *, *, #205622, .T. ) ;
#10983 = CARTESIAN_POINT ( 'NONE',  ( 8.392133896734652154, 12.73464727959172293, 0.7216878364870438212 ) ) ;
#10984 = ORIENTED_EDGE ( 'NONE', *, *, #7050, .F. ) ;
#10985 = CARTESIAN_POINT ( 'NONE',  ( 5.713130151434068438, 1.559639147136464343, -1.106415316399149473 ) ) ;
#10986 = CARTESIAN_POINT ( 'NONE',  ( 5.965779495465724835, 1.698367018877691370, -0.2996015908335278310 ) ) ;
#10987 = CARTESIAN_POINT ( 'NONE',  ( 4.926970384345759513, -1.727065721694167832, 1.040790168839386798 ) ) ;
#10988 = LINE ( 'NONE', #28323, #73718 ) ;
#10990 = FACE_OUTER_BOUND ( 'NONE', #173079, .T. ) ;
#10989 = CARTESIAN_POINT ( 'NONE',  ( -8.962103233833181193, 10.41454084668224489, -1.199719254218446718 ) ) ;
#10991 = CARTESIAN_POINT ( 'NONE',  ( -1.642778471874998480, -2.938541666188707602, 2.845375778867863303 ) ) ;
#10993 = CARTESIAN_POINT ( 'NONE',  ( 6.872329512321287304, -1.085958120241878877, 1.397742320866280252 ) ) ;
#10992 = CARTESIAN_POINT ( 'NONE',  ( 1.359446872921949101, 2.059443214669457234, -0.3588360909314599612 ) ) ;
#10994 = CARTESIAN_POINT ( 'NONE',  ( 5.871720251644387822, -0.2986239867289949834, -1.994071864161291119 ) ) ;
#10996 = CARTESIAN_POINT ( 'NONE',  ( 3.627152717534872561, -2.118219197452147373, 0.8765883884584676489 ) ) ;
#10995 = CARTESIAN_POINT ( 'NONE',  ( 3.898851692381625877, 6.706354853490643642, -1.199719254218452047 ) ) ;
#10997 = CARTESIAN_POINT ( 'NONE',  ( 1.640152974701726496, -1.471428658003028911, 0.9289965205148569272 ) ) ;
#10998 = CARTESIAN_POINT ( 'NONE',  ( 2.724977724663907530, 1.532976055022855499, -1.465462182430438798 ) ) ;
#10999 = CARTESIAN_POINT ( 'NONE',  ( 11.89844258446855818, 11.32852689329961215, -1.560502987793222163 ) ) ;
#11000 = CARTESIAN_POINT ( 'NONE',  ( 0.5086469178660666390, 1.728604602589098205, 0.1357594709466679594 ) ) ;
#11001 = CARTESIAN_POINT ( 'NONE',  ( 1.360316468749941610, 2.276041667008116942, 0.7853790794158921340 ) ) ;
#11002 = CARTESIAN_POINT ( 'NONE',  ( 1.258004785490075994, -1.861241886096485221, -0.004951839839751126689 ) ) ;
#11003 = CARTESIAN_POINT ( 'NONE',  ( 1.838563082212365085, -1.162459688571298111, 1.833603174184100792 ) ) ;
#11004 = CARTESIAN_POINT ( 'NONE',  ( 3.134000194803722383, 2.016708403948695771, -0.004836970814638129855 ) ) ;
#11005 = CARTESIAN_POINT ( 'NONE',  ( 4.437500000000002665, 1.451031289060936480, -1.451031289061293528 ) ) ;
#11006 = MECHANICAL_DESIGN_GEOMETRIC_PRESENTATION_REPRESENTATION (  '', ( #121815 ), #118389 ) ;
#11007 = CARTESIAN_POINT ( 'NONE',  ( 0.7499999999999902300, 1.264583334016147642, 1.299038105676657340 ) ) ;
#11008 = CARTESIAN_POINT ( 'NONE',  ( 6.445928676245076261, 0.7346846062235148356, -1.781103304711729729 ) ) ;
#11009 = CARTESIAN_POINT ( 'NONE',  ( -1.402160292154681736E-14, 13.92187500034139624, 1.575800808251682339 ) ) ;
#11010 = CARTESIAN_POINT ( 'NONE',  ( 3.445754134864047025, -2.051236611594880799, 0.8531546545873994747 ) ) ;
#11011 = ORIENTED_EDGE ( 'NONE', *, *, #204911, .F. ) ;
#11013 = AXIS2_PLACEMENT_3D ( 'NONE', #208059, #142044, #22898 ) ;
#11012 = CARTESIAN_POINT ( 'NONE',  ( -15.75000000000000000, 12.30000000000000071, 0.6999999999999992895 ) ) ;
#11014 = CARTESIAN_POINT ( 'NONE',  ( -0.7500000000000006661, -0.6416666666666446250, -1.299038105676652011 ) ) ;
#11015 = CARTESIAN_POINT ( 'NONE',  ( 8.320953590485093088, 10.73086516036454618, 1.599625672291281386 ) ) ;
#11016 = CARTESIAN_POINT ( 'NONE',  ( -1.402160292154681736E-14, -0.4281249996585808071, 1.575800808251672791 ) ) ;
#11017 = CARTESIAN_POINT ( 'NONE',  ( -0.05755013669183139946, -1.372491973113322050, -1.747462644287574030 ) ) ;
#11018 = CARTESIAN_POINT ( 'NONE',  ( 4.492601031306558745, 1.923586649950057792, 0.3847822903023030428 ) ) ;
#11020 = CARTESIAN_POINT ( 'NONE',  ( -5.585596099150182958, 8.499983968108443477, -1.082531754730544860 ) ) ;
#11019 = CARTESIAN_POINT ( 'NONE',  ( 4.695201269034174452, 4.372156323494968966, 1.214306433183764966E-14 ) ) ;
#11021 = LINE ( 'NONE', #175688, #104367 ) ;
#11022 = CARTESIAN_POINT ( 'NONE',  ( 5.905634875922824989, -0.5580066813290808225, 2.192401876011939699 ) ) ;
#11023 = CARTESIAN_POINT ( 'NONE',  ( 2.225118093709726352, -1.884898904786440177, -0.8381453960227978062 ) ) ;
#11024 = CARTESIAN_POINT ( 'NONE',  ( -7.718669524881690336, 7.899535955317097624, 0.7998128361456462443 ) ) ;
#11025 = EDGE_LOOP ( 'NONE', ( #127296, #55478, #5029, #135031, #55241 ) ) ;
#11026 = CARTESIAN_POINT ( 'NONE',  ( -1.500000000000013101, 1.452083334016150085, 0.8660254037844403729 ) ) ;
#11027 = CARTESIAN_POINT ( 'NONE',  ( 3.532352470753961082, 1.824241569866682289, 0.4128566369710484629 ) ) ;
#11028 = CARTESIAN_POINT ( 'NONE',  ( 2.988574679986736093, -1.732066829584472556, 0.08781845822969887305 ) ) ;
#11029 = CARTESIAN_POINT ( 'NONE',  ( -0.07607780150072247782, -1.417851297177070258, -1.802264747598992800 ) ) ;
#11030 = CARTESIAN_POINT ( 'NONE',  ( 1.518904762042364354, 1.481482853740143657, -1.635709697223409531 ) ) ;
#11031 = CARTESIAN_POINT ( 'NONE',  ( 4.293933718354110418, -0.8299404887524584051, 1.996233173270183681 ) ) ;
#11032 = CARTESIAN_POINT ( 'NONE',  ( 5.279219580190475547, 1.305526251850267272, 1.437786642569781614 ) ) ;
#11033 = CARTESIAN_POINT ( 'NONE',  ( 7.219650724572225897, 15.51887837940885895, 9.591874471555675186 ) ) ;
#11034 = CARTESIAN_POINT ( 'NONE',  ( 0.09375222243388467436, -1.895918425137008034, -0.7852924748299833224 ) ) ;
#11035 = CARTESIAN_POINT ( 'NONE',  ( 1.499999999999961364, 8.500000000000000000, -10.64483442802188939 ) ) ;
#11036 = FACE_OUTER_BOUND ( 'NONE', #129823, .T. ) ;
#11037 = CARTESIAN_POINT ( 'NONE',  ( -0.6801582343750316451, 2.098958333674738608, -1.178068619123862515 ) ) ;
#11038 = CARTESIAN_POINT ( 'NONE',  ( -2.931280137532493946, 6.571577260429871892, 0.3558765841190729140 ) ) ;
#11039 = CARTESIAN_POINT ( 'NONE',  ( -9.365985188942097750, 9.821404230054264772, 0.7998128361456462443 ) ) ;
#11040 = CARTESIAN_POINT ( 'NONE',  ( 7.467843683028853263, 7.606905806488803101, 0.7998128361456341429 ) ) ;
#11041 = CARTESIAN_POINT ( 'NONE',  ( 11.94655611907589154, 12.44799055453095527, 1.134828163062136852 ) ) ;
#11042 = CARTESIAN_POINT ( 'NONE',  ( 3.721172816245840842, -0.1328194893376876962, 1.820914920514608459 ) ) ;
#11043 = CARTESIAN_POINT ( 'NONE',  ( 2.450463542074859724, 2.206263077450395738, 0.05474276496272853509 ) ) ;
#11044 = ORIENTED_EDGE ( 'NONE', *, *, #114672, .F. ) ;
#11045 = CARTESIAN_POINT ( 'NONE',  ( -4.950135482320939140, 4.947781948895412008, -0.7216878364870338292 ) ) ;
#11046 = EDGE_CURVE ( 'NONE', #93819, #29771, #166021, .T. ) ;
#11047 = CARTESIAN_POINT ( 'NONE',  ( 3.285556943750000070, -3.171874999522043215, 0.000000000000000000 ) ) ;
#11048 = CARTESIAN_POINT ( 'NONE',  ( -9.155833807930273238, 9.576227618873799585, -0.7998128361456291469 ) ) ;
#11049 = CARTESIAN_POINT ( 'NONE',  ( 1.054951293920348698, 0.3981946776167448188, 1.979963216457211850 ) ) ;
#11050 = CARTESIAN_POINT ( 'NONE',  ( 1.664851754375612058, 0.6682523891239250391, 2.012492909199379731 ) ) ;
#11051 = CARTESIAN_POINT ( 'NONE',  ( -3.796053574490474869, 15.00000000000207656, -12.24940615670125510 ) ) ;
#11052 = CARTESIAN_POINT ( 'NONE',  ( -5.285699784481336927, 7.260012063351913625, 1.599625672291263179 ) ) ;
#11053 = CARTESIAN_POINT ( 'NONE',  ( 2.992830011424299830, 0.2227009285440742226, 1.847472864794322156 ) ) ;
#11054 = AXIS2_PLACEMENT_3D ( 'NONE', #125554, #122371, #73513 ) ;
#11055 = CARTESIAN_POINT ( 'NONE',  ( 4.701980345841006326, 4.380065246436280368, 0.7998128361456341429 ) ) ;
#11056 = CARTESIAN_POINT ( 'NONE',  ( 1.147603855448702248, -1.704515299458901012, -1.329379018566230641 ) ) ;
#11057 = DIRECTION ( 'NONE',  ( 0.000000000000000000, 1.000000000000000000, 0.000000000000000000 ) ) ;
#11058 = ORIENTED_EDGE ( 'NONE', *, *, #149314, .F. ) ;
#11059 = ORIENTED_EDGE ( 'NONE', *, *, #119894, .F. ) ;
#11060 = CARTESIAN_POINT ( 'NONE',  ( -5.687809136132860210, 6.594531066031826150, -1.199719254218446718 ) ) ;
#11061 = CARTESIAN_POINT ( 'NONE',  ( -10.62011439820619429, 11.28455497419572318, -0.7998128361456221525 ) ) ;
#11062 = CARTESIAN_POINT ( 'NONE',  ( 4.459475772512963232, 0.3974328844052883447, -1.781742007231662983 ) ) ;
#11064 = CARTESIAN_POINT ( 'NONE',  ( -5.789674969154799733, 6.218922551941099108, -1.014761583188450000 ) ) ;
#11063 = CARTESIAN_POINT ( 'NONE',  ( -5.764151584465413869, 6.753873599078290546, -1.199719254218453823 ) ) ;
#11065 = CARTESIAN_POINT ( 'NONE',  ( 6.083581728852979431, 7.123651168416324175, -1.137916992902558100 ) ) ;
#11066 = CARTESIAN_POINT ( 'NONE',  ( 6.397814513887354337, 0.1948139983735352188, 2.006652364629394114 ) ) ;
#11067 = CARTESIAN_POINT ( 'NONE',  ( 5.542853976212075651, -1.453887124689148935, -1.129494548679485844 ) ) ;
#11068 = CARTESIAN_POINT ( 'NONE',  ( -0.02319159430947542386, 1.394398620246390275, -2.068318759734718792 ) ) ;
#11069 = CARTESIAN_POINT ( 'NONE',  ( 4.864078691051298975, 2.283152030527708209, -0.3349727840419229330 ) ) ;
#11070 = CARTESIAN_POINT ( 'NONE',  ( 5.855142236255289845, 7.924361590421551860, -1.599625672291281386 ) ) ;
#11071 = CARTESIAN_POINT ( 'NONE',  ( 6.919229410208834530, -0.1638780278429008419, 2.126154539342207883 ) ) ;
#11072 = CARTESIAN_POINT ( 'NONE',  ( 7.253775878511261155, 8.421492265473332850, 1.199719254218462483 ) ) ;
#11073 = CARTESIAN_POINT ( 'NONE',  ( 1.839301188190944902, 0.7414227542083090539, -1.795152619562689233 ) ) ;
#11074 = CARTESIAN_POINT ( 'NONE',  ( 5.606872354539667036, 0.9390355927846851802, -2.097984029676060125 ) ) ;
#11075 = DIRECTION ( 'NONE',  ( 1.000000000000000000, 0.000000000000000000, 0.000000000000000000 ) ) ;
#11076 = CARTESIAN_POINT ( 'NONE',  ( -2.993318053567081360, 6.714231172462041819, 0.000000000000000000 ) ) ;
#11077 = VECTOR ( 'NONE', #8695, 1000.000000000000000 ) ;
#11078 = CARTESIAN_POINT ( 'NONE',  ( 4.821099876132087125, -0.09137817997613774390, 1.868553921495450965 ) ) ;
#11079 = ORIENTED_EDGE ( 'NONE', *, *, #66779, .T. ) ;
#11080 = B_SPLINE_CURVE_WITH_KNOTS ( 'NONE', 3,
 ( #11085, #24132, #188780, #76100, #205011, #158425, #106521, #208218, #57723, #206088, #91312, #155225 ),
 .UNSPECIFIED., .F., .F.,
 ( 4, 2, 2, 2, 2, 4 ),
 ( -5.999999997212162571E-08, 0.0007498576660960367670, 0.001124816499144041257, 0.001499775332192045639, 0.002249692998288053102, 0.002999610664384060564 ),
 .UNSPECIFIED. ) ;
#11083 = CARTESIAN_POINT ( 'NONE',  ( -4.960304097753355457, 6.880383762169266504, 1.599625672291263179 ) ) ;
#11082 = CARTESIAN_POINT ( 'NONE',  ( -1.201851678989727383E-14, 1.743750000682815493, 1.732050807568877637 ) ) ;
#11081 = CARTESIAN_POINT ( 'NONE',  ( 2.039183100597967258, 0.003605121848727563250, 1.912571728241836633 ) ) ;
#11084 = CARTESIAN_POINT ( 'NONE',  ( 3.475398437264758833, 0.05438942809191970457, -2.206374867412825402 ) ) ;
#11085 = CARTESIAN_POINT ( 'NONE',  ( -10.84254087577847869, 4.919568073182958301, 5.035408296252059657 ) ) ;
#11086 = CARTESIAN_POINT ( 'NONE',  ( 5.682275777458846377, 7.722684055159064975, 1.443375672974064550 ) ) ;
#11087 = CARTESIAN_POINT ( 'NONE',  ( -6.251718229232857915, 7.426664367927358512, -1.082531754730549967 ) ) ;
#11088 = CARTESIAN_POINT ( 'NONE',  ( 2.108605603913331183, 1.463472826393363624, -1.321001006224751917 ) ) ;
#11089 = CARTESIAN_POINT ( 'NONE',  ( 1.413547897872836856, 2.036140070965312354, 1.085889434398391584 ) ) ;
#11090 = CARTESIAN_POINT ( 'NONE',  ( 2.928120951529111338, 1.047165451586975049, 1.658829547137883775 ) ) ;
#11091 = CARTESIAN_POINT ( 'NONE',  ( -5.367048706163331850, 7.354919138647580290, -1.599625672291271394 ) ) ;
#11092 = CARTESIAN_POINT ( 'NONE',  ( 5.963753124799120897, -0.5065058054696270906, 1.999279329544477513 ) ) ;
#11093 = CARTESIAN_POINT ( 'NONE',  ( 3.877268743828276243, 4.586196958296845594, 1.082531754730560403 ) ) ;
#11094 = CARTESIAN_POINT ( 'NONE',  ( 4.065638850954083061, 1.320825628876612479, 1.523796413913918846 ) ) ;
#11095 = CARTESIAN_POINT ( 'NONE',  ( 6.229045230835819069, 6.231917288922055320, -0.7998128361456481317 ) ) ;
#11096 = ORIENTED_EDGE ( 'NONE', *, *, #111969, .T. ) ;
#11097 = CARTESIAN_POINT ( 'NONE',  ( -9.972185678051314284, 11.59297036493672017, 1.199719254218462483 ) ) ;
#11098 = DIRECTION ( 'NONE',  ( 1.000000000000000000, 0.000000000000000000, -1.224646799147353207E-16 ) ) ;
#11099 = CARTESIAN_POINT ( 'NONE',  ( 9.480175724453529185, 12.08329098332774265, 1.599625672291279388 ) ) ;
#11100 = CARTESIAN_POINT ( 'NONE',  ( 2.483468006519026439, -0.003752633953101049049, 2.171239807183155790 ) ) ;
#11101 = SURFACE_SIDE_STYLE ('',( #143299 ) ) ;
#11102 = CARTESIAN_POINT ( 'NONE',  ( -3.111427816635929045, 14.48006665644674484, -11.59831529056025801 ) ) ;
#11103 = CARTESIAN_POINT ( 'NONE',  ( -10.99962150373186809, -9.919999999999998153, 0.09125116240079125807 ) ) ;
#11104 = CARTESIAN_POINT ( 'NONE',  ( 3.022558680773678397, 1.760047114015901526, 0.6337009143728977723 ) ) ;
#11105 = CARTESIAN_POINT ( 'NONE',  ( 6.309879873373573922, -2.146112031266556919, 0.2576265230809087758 ) ) ;
#11106 = CIRCLE ( 'NONE', #17884, 0.08000000000000020983 ) ;
#11108 = CARTESIAN_POINT ( 'NONE',  ( 6.727182134110241130, 2.994815527893503138, 2.165292399158074588 ) ) ;
#11107 = CARTESIAN_POINT ( 'NONE',  ( 0.07755575628183573877, -0.002876890934064984650, -2.188974970840869005 ) ) ;
#11109 = CARTESIAN_POINT ( 'NONE',  ( -1.364683531250014514, -1.219791666325248602, 0.7879004041258379498 ) ) ;
#11110 = CARTESIAN_POINT ( 'NONE',  ( -1.364643601765285208, 3.684187268283338312, 0.6238217115099010668 ) ) ;
#11111 = CARTESIAN_POINT ( 'NONE',  ( 1.998553653897700011, -1.875654816251038248, -0.3715787057524469472 ) ) ;
#11112 = CARTESIAN_POINT ( 'NONE',  ( 3.994789325776046507, 1.495029845459275863, -0.9468837749658890468 ) ) ;
#11113 = CARTESIAN_POINT ( 'NONE',  ( 2.051281676579026492, -1.707476168062868060, 0.8611843332394366612 ) ) ;
#11114 = CARTESIAN_POINT ( 'NONE',  ( -5.915435094264120508, 5.795762452929912101, 0.000000000000000000 ) ) ;
#11116 = CARTESIAN_POINT ( 'NONE',  ( -0.1005721928965920831, -1.878210221491773524, 0.3762452260359094303 ) ) ;
#11115 = DIRECTION ( 'NONE',  ( 8.638326563840814399E-31, 0.000000000000000000, 1.000000000000000000 ) ) ;
#11117 = CARTESIAN_POINT ( 'NONE',  ( 0.7499999999999885647, -0.5166666666666444030, 1.299038105676657340 ) ) ;
#11118 = CARTESIAN_POINT ( 'NONE',  ( 0.4673438449808891004, 1.800595422158430825, 1.021790579661909781 ) ) ;
#11119 = CARTESIAN_POINT ( 'NONE',  ( -1.402160292154681736E-14, -0.4906249996585810846, -1.575800808251665908 ) ) ;
#11120 = CARTESIAN_POINT ( 'NONE',  ( 5.524238439434661530, 1.113281918156138639, -1.503147240406087271 ) ) ;
#11121 = CARTESIAN_POINT ( 'NONE',  ( 1.418276456094772708, 1.227529518603141190, -1.351586893430449576 ) ) ;
#11123 = CARTESIAN_POINT ( 'NONE',  ( 4.876420697298537554, 8.045338245374718866, 0.9427337716215690167 ) ) ;
#11122 = CARTESIAN_POINT ( 'NONE',  ( 5.444034239667132624, 0.8972360612293399651, -2.016436982482258333 ) ) ;
#11124 = CARTESIAN_POINT ( 'NONE',  ( -0.6823417656250246877, -0.4489583329919111243, 1.181850606188755259 ) ) ;
#11125 = CARTESIAN_POINT ( 'NONE',  ( 2.857939457652844073, -0.6493452292726099584, 1.957851178230881395 ) ) ;
#11126 = CARTESIAN_POINT ( 'NONE',  ( -7.365103760721662951, 9.615707025640515937, 1.599625672291295375 ) ) ;
#11127 = CARTESIAN_POINT ( 'NONE',  ( 6.610000000000003872, 7.053606217926155608, 2.318153411789238838 ) ) ;
#11128 = CARTESIAN_POINT ( 'NONE',  ( 9.915090410295563927, 10.46202698829998567, -0.7998128361456281477 ) ) ;
#11129 = CARTESIAN_POINT ( 'NONE',  ( 1.273593037967014618, 3.987039452347238999, -0.4852599168373658567 ) ) ;
#11130 = FACE_OUTER_BOUND ( 'NONE', #207955, .T. ) ;
#11131 = CARTESIAN_POINT ( 'NONE',  ( 5.155843554946782703, 9.237177590738404831, -0.7998128361456481317 ) ) ;
#11132 = ORIENTED_EDGE ( 'NONE', *, *, #47186, .F. ) ;
#11133 = CARTESIAN_POINT ( 'NONE',  ( 5.951642636407409093, 1.565221049572671719, 1.355249363302114318 ) ) ;
#11134 = CARTESIAN_POINT ( 'NONE',  ( 1.364683531249986537, -0.2822916663252520997, -0.7879004041258309554 ) ) ;
#11135 = CARTESIAN_POINT ( 'NONE',  ( 2.284651837757902371, -2.119410549416993916, -0.4241055355862289877 ) ) ;
#11136 = CARTESIAN_POINT ( 'NONE',  ( -4.662190612263335865, 8.310640895677696705, -0.4745246276153299858 ) ) ;
#11137 = CARTESIAN_POINT ( 'NONE',  ( 3.422525317731230032, -0.8204878289409988090, -1.845699721510121183 ) ) ;
#11138 = CARTESIAN_POINT ( 'NONE',  ( 6.720655732516648051, 2.039834428248034293, 2.379457109286802208 ) ) ;
#11141 = CARTESIAN_POINT ( 'NONE',  ( 6.805829924380105034, 9.923590097543378619, 1.082531754730558626 ) ) ;
#11140 = CARTESIAN_POINT ( 'NONE',  ( -1.737500000000000266, -0.7583333333333330817, -3.009438278150923907 ) ) ;
#11139 = CARTESIAN_POINT ( 'NONE',  ( 10.33323920393400286, 4.021557182957047338, 5.965898435991960902 ) ) ;
#11142 = CARTESIAN_POINT ( 'NONE',  ( -7.553827861469316396, 8.841829255582865699, -1.199719254218452047 ) ) ;
#11143 = CARTESIAN_POINT ( 'NONE',  ( 1.587125413319636635, 1.679225032509903404, 1.116207499648947943 ) ) ;
#11145 = CARTESIAN_POINT ( 'NONE',  ( 6.286699343557896391, 1.907799665397520883, -1.078441415684105120 ) ) ;
#11144 = CARTESIAN_POINT ( 'NONE',  ( -4.069418662396130593, 7.899405539437467816, -0.7998128361456281477 ) ) ;
#11146 = CARTESIAN_POINT ( 'NONE',  ( -0.7500000000000215383, 4.472916667349482012, 1.299038105676671107 ) ) ;
#11147 = CARTESIAN_POINT ( 'NONE',  ( 4.201352949932454450, 1.705870964349815333, -0.8646410313453978258 ) ) ;
#11148 = CARTESIAN_POINT ( 'NONE',  ( -11.94105722165067363, 12.57417237917041142, 1.187919369849792295 ) ) ;
#11149 = CARTESIAN_POINT ( 'NONE',  ( 6.358410854684775515, 8.441231968597481483, -1.443375672974058777 ) ) ;
#11151 = CARTESIAN_POINT ( 'NONE',  ( 3.321888824615967906, 0.9040932542298124597, -1.802426844439278142 ) ) ;
#11150 = CARTESIAN_POINT ( 'NONE',  ( -7.971831134711019118, 12.24429405723079967, 0.000000000000000000 ) ) ;
#11152 = CARTESIAN_POINT ( 'NONE',  ( -1.364683531250014514, 14.15104166700806765, -0.7879004041258335089 ) ) ;
#11153 = CARTESIAN_POINT ( 'NONE',  ( -6.291865805193673111, 9.498204651771386509, -1.199719254218452047 ) ) ;
#11154 = CARTESIAN_POINT ( 'NONE',  ( 5.420820933352582749, 1.595050213381223214, 0.6567411224575621098 ) ) ;
#11155 = CARTESIAN_POINT ( 'NONE',  ( 5.742760583840166966, 8.857581893525663830, 1.199719254218452047 ) ) ;
#11156 = CARTESIAN_POINT ( 'NONE',  ( 4.383363735919856730, 4.008345868194933104, -0.7998128361456211532 ) ) ;
#11157 = DIRECTION ( 'NONE',  ( 1.224646799147353207E-16, 0.000000000000000000, -1.000000000000000000 ) ) ;
#11158 = CARTESIAN_POINT ( 'NONE',  ( 4.885944009213345929, -0.8832235454491498272, 1.648918812636574804 ) ) ;
#11159 = LINE ( 'NONE', #128229, #92249 ) ;
#11161 = CIRCLE ( 'NONE', #159920, 3.971937515251341644 ) ;
#11160 = CARTESIAN_POINT ( 'NONE',  ( 1.498975721005956441, 0.3999860688887920679, 2.031077231357696355 ) ) ;
#11162 = CARTESIAN_POINT ( 'NONE',  ( 6.764690511086886823E-16, -5.511313137147262786, 11.00000000000000178 ) ) ;
#11163 = EDGE_LOOP ( 'NONE', ( #117885, #9988 ) ) ;
#11164 = CARTESIAN_POINT ( 'NONE',  ( -0.2051949539778260834, -0.1395167590549877823, -1.781371329038708096 ) ) ;
#11165 = CARTESIAN_POINT ( 'NONE',  ( 3.705121118284530279, 7.544668081299086282, -1.734723475976807094E-15 ) ) ;
#11166 =( NAMED_UNIT ( * ) SI_UNIT ( $, .STERADIAN. ) SOLID_ANGLE_UNIT ( ) );
#11167 = CARTESIAN_POINT ( 'NONE',  ( 0.2283786121510515688, 1.249231189971045319, -1.312217732533569103 ) ) ;
#11168 = ADVANCED_FACE ( 'NONE', ( #21522 ), #37814, .F. ) ;
#11169 = CARTESIAN_POINT ( 'NONE',  ( 5.031484404002879884, 6.963427452793765404, 1.443375672974065660 ) ) ;
#11170 = CARTESIAN_POINT ( 'NONE',  ( 11.80937116653883123, 7.958520514542954949, 2.169913335582353664 ) ) ;
#11171 = ORIENTED_EDGE ( 'NONE', *, *, #206662, .F. ) ;
#11172 = EDGE_CURVE ( 'NONE', #205805, #2289, #107528, .T. ) ;
#11174 = CARTESIAN_POINT ( 'NONE',  ( 7.426115451983150706, 9.686887332112256388, -1.599625672291262513 ) ) ;
#11173 = CARTESIAN_POINT ( 'NONE',  ( 0.5726126529861442771, 1.355618539282506640, -1.418395753018865113 ) ) ;
#11175 = CARTESIAN_POINT ( 'NONE',  ( 5.431221565750523617, -1.512988070448300970, -1.174818341023081913 ) ) ;
#11176 = DIRECTION ( 'NONE',  ( -0.1510067114093955887, 0.000000000000000000, -0.9885327375000383388 ) ) ;
#11177 = CARTESIAN_POINT ( 'NONE',  ( -5.472807559815892731, 7.501441282320147508, 1.250076539767187578 ) ) ;
#11178 = SHAPE_REPRESENTATION ( 'negative coil', ( #200407 ), #193485 ) ;
#11179 = LINE ( 'NONE', #188872, #139754 ) ;
#11181 = ORIENTED_EDGE ( 'NONE', *, *, #81383, .T. ) ;
#11180 = CARTESIAN_POINT ( 'NONE',  ( 6.493992391265805075, 6.678671999339316656, 1.040834085586084257E-14 ) ) ;
#11182 = CARTESIAN_POINT ( 'NONE',  ( -7.375272376154077492, 11.54830883891436422, -0.7216878364870267237 ) ) ;
#11183 = CARTESIAN_POINT ( 'NONE',  ( 1.551884642779034262, 0.6273040060550126862, -2.068667048528524344 ) ) ;
#11184 = CARTESIAN_POINT ( 'NONE',  ( -3.311934663488232733, 7.085950550703385531, -0.7998128361456481317 ) ) ;
#11185 = ADVANCED_FACE ( 'NONE', ( #136399 ), #168874, .T. ) ;
#11186 = CARTESIAN_POINT ( 'NONE',  ( 7.702440666339465558, 8.158804663583751449, -0.7216878364870317197 ) ) ;
#11187 = CARTESIAN_POINT ( 'NONE',  ( 0.1234922912959918878, 1.848187084301698757, 1.039613981531524400 ) ) ;
#11188 = CARTESIAN_POINT ( 'NONE',  ( 4.629811725094972630, -1.123643258228578024, -1.438734611599351565 ) ) ;
#11189 = CARTESIAN_POINT ( 'NONE',  ( 11.38909496574627056, 7.479950087089620503, -5.016624281428613941 ) ) ;
#11190 = CARTESIAN_POINT ( 'NONE',  ( 1.423050710548888542, -0.05258038247234024520, 1.970828066091591557 ) ) ;
#11191 = CARTESIAN_POINT ( 'NONE',  ( 3.164218664783400747, 1.912571728330178855, -0.004505864839042527346 ) ) ;
#11192 = EDGE_LOOP ( 'NONE', ( #61149, #16527, #181946, #91125, #63396, #130380, #156162, #137227, #149617, #195284 ) ) ;
#11193 = CARTESIAN_POINT ( 'NONE',  ( 4.105875410593727182, 0.6658617523271005423, -1.853701319000864656 ) ) ;
#11194 = ORIENTED_EDGE ( 'NONE', *, *, #152817, .T. ) ;
#11195 = CARTESIAN_POINT ( 'NONE',  ( 5.495633776345048460, -1.942234966517431660, 0.004081557570839721392 ) ) ;
#11196 = VERTEX_POINT ( 'NONE', #86565 ) ;
#11197 = CARTESIAN_POINT ( 'NONE',  ( -7.449279056065764237, 7.655523418356991350, 0.7998128361456341429 ) ) ;
#11199 = CARTESIAN_POINT ( 'NONE',  ( 5.888958097455845753, -2.014202512972632420, -0.6635655960139997811 ) ) ;
#11198 = CARTESIAN_POINT ( 'NONE',  ( -6.296835998904160014, 6.311006518335105397, 0.000000000000000000 ) ) ;
#11200 = CARTESIAN_POINT ( 'NONE',  ( 5.668717623845194176, 9.627604637879139560, 0.000000000000000000 ) ) ;
#11202 = ORIENTED_EDGE ( 'NONE', *, *, #86135, .F. ) ;
#11201 = CARTESIAN_POINT ( 'NONE',  ( 3.791585636498477463, 1.799617611794877670, -0.6470144256675299799 ) ) ;
#11203 = CARTESIAN_POINT ( 'NONE',  ( 4.499531974119707733, 7.248992493261455117, -1.273121237324711386 ) ) ;
#11204 = DIRECTION ( 'NONE',  ( 1.000000000000000000, -0.000000000000000000, -0.000000000000000000 ) ) ;
#11205 = FACE_OUTER_BOUND ( 'NONE', #153685, .T. ) ;
#11206 = VECTOR ( 'NONE', #134834, 1000.000000000000114 ) ;
#11207 = CARTESIAN_POINT ( 'NONE',  ( 5.725249205227378013, 1.776381904961796154, 0.9470739834369249488 ) ) ;
#11208 = DIRECTION ( 'NONE',  ( 0.000000000000000000, 0.000000000000000000, -1.000000000000000000 ) ) ;
#11210 = CARTESIAN_POINT ( 'NONE',  ( 5.805875103277515770, -1.124240986939632592, -1.673857227857282082 ) ) ;
#11209 = CARTESIAN_POINT ( 'NONE',  ( 6.024025069106937913, -1.018266858664597763, -1.515143308444939274 ) ) ;
#11211 = CARTESIAN_POINT ( 'NONE',  ( 2.348173244826061268, -0.8873571809006628452, 1.870714752860686447 ) ) ;
#11212 = CARTESIAN_POINT ( 'NONE',  ( -8.853111120043687166, 9.430977182913531820, 1.040834085586084257E-14 ) ) ;
#11213 = CARTESIAN_POINT ( 'NONE',  ( -6.190206388764837975, 6.963036634120459922, -0.8879648754220506035 ) ) ;
#11214 = CARTESIAN_POINT ( 'NONE',  ( -1.045839947578414805E-15, 1.812499999999992673, 1.224999999999988987 ) ) ;
#11215 = CARTESIAN_POINT ( 'NONE',  ( 6.702024585102262400, -1.870183347854617040, 0.04844413084104796929 ) ) ;
#11216 = CARTESIAN_POINT ( 'NONE',  ( 6.634017235788401301, 6.634108284708264414, 0.7998128361456341429 ) ) ;
#11217 = CARTESIAN_POINT ( 'NONE',  ( 5.153507786970260796, 7.105788066255672497, -1.443375672974078761 ) ) ;
#11218 = CARTESIAN_POINT ( 'NONE',  ( 2.218730694130720771, 5.740269576461138890, 0.7998128361456462443 ) ) ;
#11219 = CARTESIAN_POINT ( 'NONE',  ( -1.364683531250010295, 11.19270833367473550, 0.7879004041258445001 ) ) ;
#11220 = CARTESIAN_POINT ( 'NONE',  ( -3.249150368769345043, 6.942425863539538611, 0.7998128361456341429 ) ) ;
#11222 = CARTESIAN_POINT ( 'NONE',  ( -7.632314129850253259, 7.869064337772231355, 0.7998128361456341429 ) ) ;
#11221 = CARTESIAN_POINT ( 'NONE',  ( 1.772826578343079884, 3.999999999999976019, 0.4499999999999729772 ) ) ;
#11223 = CARTESIAN_POINT ( 'NONE',  ( 4.131323472851686773, 0.4681366286901997853, 1.669664985128198831 ) ) ;
#11224 = VECTOR ( 'NONE', #73435, 1000.000000000000000 ) ;
#11225 = CARTESIAN_POINT ( 'NONE',  ( -5.037017762676898158, 5.835274463666530131, -1.199719254218446718 ) ) ;
#11226 = VECTOR ( 'NONE', #131183, 1000.000000000000000 ) ;
#11227 = CARTESIAN_POINT ( 'NONE',  ( 1.411079811451225074, -1.634442866182721277, 1.270590680402396311 ) ) ;
#11228 = CARTESIAN_POINT ( 'NONE',  ( 2.988026824963069927, -2.114671507216555391, 0.1067447620008883935 ) ) ;
#11229 = CARTESIAN_POINT ( 'NONE',  ( 8.749089199520284410, 9.101692242395490240, 0.7998128361456481317 ) ) ;
#11231 = EDGE_CURVE ( 'NONE', #175232, #33823, #171598, .T. ) ;
#11230 = CARTESIAN_POINT ( 'NONE',  ( 0.02270195696656561457, 6.343288419976386372, 3.091051226635131322 ) ) ;
#11232 = CARTESIAN_POINT ( 'NONE',  ( 0.2859135117265668158, -1.207096249910791563, -1.556650298907244823 ) ) ;
#11233 = CARTESIAN_POINT ( 'NONE',  ( 4.556571072163061231, 7.192851904033680910, 1.311937382574361877 ) ) ;
#11234 = CARTESIAN_POINT ( 'NONE',  ( 5.395781948558860286, 6.357795697149212444, -1.082531754730542195 ) ) ;
#11236 = CARTESIAN_POINT ( 'NONE',  ( -0.1405747822309927342, -1.479430311965252542, -1.211566217618691210 ) ) ;
#11235 = CARTESIAN_POINT ( 'NONE',  ( 1.001543065824772753E-15, -2.362500000000001155, 4.012584370867899430 ) ) ;
#11237 = CARTESIAN_POINT ( 'NONE',  ( 3.275583346405244622, 1.454120551940318418, 1.771997285204220507 ) ) ;
#11238 = CARTESIAN_POINT ( 'NONE',  ( 1.013953575274041619, -0.8186894766500467657, -1.631917417583013341 ) ) ;
#11239 = CARTESIAN_POINT ( 'NONE',  ( 3.832203377193269755, -0.9874410831685247469, -1.637625244210038300 ) ) ;
#11240 = EDGE_CURVE ( 'NONE', #33454, #1299, #188318, .T. ) ;
#11241 = CARTESIAN_POINT ( 'NONE',  ( 4.830447868218803897, 8.857549289555754157, -0.7998128361456481317 ) ) ;
#11242 = CARTESIAN_POINT ( 'NONE',  ( 7.429504990164394584, 7.770103364721017591, 1.040834085586084257E-14 ) ) ;
#11243 = CARTESIAN_POINT ( 'NONE',  ( -7.995557903757128493, 10.35123685918189729, 1.599625672291295375 ) ) ;
#11244 = CARTESIAN_POINT ( 'NONE',  ( 1.863541034856039502, -1.619513613076409397, -1.195741390080407918 ) ) ;
#11245 = CARTESIAN_POINT ( 'NONE',  ( 1.867943658074404434, -1.947550630801861526, 0.2349073745619503772 ) ) ;
#11246 = CARTESIAN_POINT ( 'NONE',  ( -10.30827686509187835, 10.92074451889568643, 1.040834085586084257E-14 ) ) ;
#11247 = CARTESIAN_POINT ( 'NONE',  ( -6.684333426737305572, 7.757142738403693727, -1.199719254218446718 ) ) ;
#11248 = FACE_OUTER_BOUND ( 'NONE', #80750, .T. ) ;
#11250 = CARTESIAN_POINT ( 'NONE',  ( 3.572906242625200068, 0.04398576871290219709, -1.769473305487194281 ) ) ;
#11249 = CARTESIAN_POINT ( 'NONE',  ( 5.244118971382810912, 0.6063552182394044143, 2.000762070341703502 ) ) ;
#11251 = CARTESIAN_POINT ( 'NONE',  ( -11.44789321844504215, 13.79999999999998295, 3.303298730975396946 ) ) ;
#11252 = CARTESIAN_POINT ( 'NONE',  ( -0.02321191073820921824, -0.1601477211686137825, -2.156400265872604471 ) ) ;
#11253 = CARTESIAN_POINT ( 'NONE',  ( 5.050617384047394687, -1.472844127453584839, -0.9267575401476387809 ) ) ;
#11254 = AXIS2_PLACEMENT_3D ( 'NONE', #22281, #2834, #169632 ) ;
#11255 = CARTESIAN_POINT ( 'NONE',  ( 7.130698725783555680, 10.40656671580112658, 1.199719254218460707 ) ) ;
#11256 = CARTESIAN_POINT ( 'NONE',  ( -0.1104750535120268828, 4.084583917300321332, -2.658209514912849514 ) ) ;
#11257 = CARTESIAN_POINT ( 'NONE',  ( 4.516742233720687949, 1.733484511791906879, -0.04249706786149141935 ) ) ;
#11258 =( BOUNDED_CURVE ( )  B_SPLINE_CURVE ( 2, ( #117538, #83897, #184589, #186733, #101214, #103361, #38356 ),
 .UNSPECIFIED., .F., .T. ) 
 B_SPLINE_CURVE_WITH_KNOTS ( ( 3, 2, 2, 3 ),
 ( 0.1071428571428572341, 0.1130952380952381098, 0.1190476190476189855, 0.1249999999999998612 ),
 .UNSPECIFIED. ) 
 CURVE ( )  GEOMETRIC_REPRESENTATION_ITEM ( )  RATIONAL_B_SPLINE_CURVE ( ( 0.9999999999999977796, 0.8660254037844409281, 1.000000000000000000, 0.8660254037844387076, 1.000000000000000000, 0.8660254037844418162, 0.9999999999999968914 ) ) 
 REPRESENTATION_ITEM ( '' )  );
#11259 = CARTESIAN_POINT ( 'NONE',  ( 6.162576015390932582, -0.7755629475397389783, -2.028117739495437277 ) ) ;
#11260 = CARTESIAN_POINT ( 'NONE',  ( -1.500000000000001110, 11.27083333333333393, 0.8660254037844418162 ) ) ;
#11261 = CARTESIAN_POINT ( 'NONE',  ( -0.2056253921914633354, -0.9106808701126485328, -1.909331193683319050 ) ) ;
#11262 = CARTESIAN_POINT ( 'NONE',  ( 5.312500000000002665, 1.451031289061327501, 1.451031289060900065 ) ) ;
#11263 = CARTESIAN_POINT ( 'NONE',  ( -1.500000000000011324, 5.452083334016153415, 0.8660254037844403729 ) ) ;
#11264 = CARTESIAN_POINT ( 'NONE',  ( 3.381779240904962069, 1.220913077095790111, 1.490098802054098837 ) ) ;
#11265 = CARTESIAN_POINT ( 'NONE',  ( -1.402160292154681736E-14, 10.84375000068279782, 1.732050807568881190 ) ) ;
#11266 = CARTESIAN_POINT ( 'NONE',  ( 6.293255338728928727, -0.1078348580665164369, -2.218937141123643375 ) ) ;
#11267 = ORIENTED_EDGE ( 'NONE', *, *, #148738, .T. ) ;
#11268 = CARTESIAN_POINT ( 'NONE',  ( -0.1411974294641681893, 1.383765339824583052, -2.157932961605046440 ) ) ;
#11269 = CARTESIAN_POINT ( 'NONE',  ( -1.500000000000011324, 2.920833333333352932, 0.8660254037844403729 ) ) ;
#11270 = CARTESIAN_POINT ( 'NONE',  ( 5.931855901178834323, 6.879252291918818152, 1.199719254218462483 ) ) ;
#11271 = CARTESIAN_POINT ( 'NONE',  ( 2.456000923045877027, -1.648014358291004733, -1.489564561520567487 ) ) ;
#11272 = LINE ( 'NONE', #176992, #139528 ) ;
#11273 = CARTESIAN_POINT ( 'NONE',  ( 7.619319141200063150, 9.912291636198670375, 1.443375672974076540 ) ) ;
#11274 = CARTESIAN_POINT ( 'NONE',  ( 1.500000000000001332, 10.15625000068279249, 0.000000000000000000 ) ) ;
#11275 = CARTESIAN_POINT ( 'NONE',  ( 4.228163802615382494, 6.026220084508304708, -1.599625672291269396 ) ) ;
#11276 = CARTESIAN_POINT ( 'NONE',  ( 0.2467204944939948574, 1.994070950632735428, -0.2986300710981006357 ) ) ;
#11278 = CARTESIAN_POINT ( 'NONE',  ( 5.318824396150737321, -1.496427615725079097, 1.419873077484270496 ) ) ;
#11277 = CARTESIAN_POINT ( 'NONE',  ( 10.05067194643221207, 10.62020544712608938, 0.7998128361456462443 ) ) ;
#11279 = CARTESIAN_POINT ( 'NONE',  ( -15.75000000000000000, 13.39999999999998259, 3.599999999999999201 ) ) ;
#11280 = DIRECTION ( 'NONE',  ( 0.000000000000000000, 8.546850786086437571E-32, 1.000000000000000000 ) ) ;
#11281 =( NAMED_UNIT ( * ) SI_UNIT ( $, .STERADIAN. ) SOLID_ANGLE_UNIT ( ) );
#11282 = CARTESIAN_POINT ( 'NONE',  ( -0.6823417656250212460, 1.301041667008083547, 1.181850606188755259 ) ) ;
#11283 = CARTESIAN_POINT ( 'NONE',  ( 0.2096995604969940641, -0.7494040810181783474, -1.602093636072899008 ) ) ;
#11284 = CARTESIAN_POINT ( 'NONE',  ( 5.731065183167076249, 1.732634240323025043, 0.07581458514279926231 ) ) ;
#11285 = CARTESIAN_POINT ( 'NONE',  ( 5.354937190278808323, 0.3318421670873850648, -1.708331137930273913 ) ) ;
#11286 = CARTESIAN_POINT ( 'NONE',  ( 3.158078472442786833, 1.032628797542353816, 2.046708512074166819 ) ) ;
#11287 = CARTESIAN_POINT ( 'NONE',  ( 1.364683531249986537, -0.6364583329919177856, 0.7879004041258500513 ) ) ;
#11288 = CARTESIAN_POINT ( 'NONE',  ( 2.782953997937851920, 1.302219384484751830, 1.301801165952347628 ) ) ;
#11289 = CARTESIAN_POINT ( 'NONE',  ( 9.423080456697809026, 10.95234760669099749, -1.199719254218446718 ) ) ;
#11290 = CARTESIAN_POINT ( 'NONE',  ( 2.977373796215293300, 1.734057503958493118, -0.5710112477543202170 ) ) ;
#11291 = CARTESIAN_POINT ( 'NONE',  ( 4.149064681782777875, 0.9530105817698063531, 1.777011888912001014 ) ) ;
#11292 = CARTESIAN_POINT ( 'NONE',  ( -2.941756144040970522, 5.415504020480993219, -1.082531754730543083 ) ) ;
#11293 = CARTESIAN_POINT ( 'NONE',  ( 0.2999999999999877764, 3.322650755865456773, -0.5865692111442898371 ) ) ;
#11294 = CARTESIAN_POINT ( 'NONE',  ( 4.805753954608172229, -0.5644290981201576241, 2.028831172856554677 ) ) ;
#11295 = CARTESIAN_POINT ( 'NONE',  ( -6.911959384868566758, 6.958374125301778790, 1.040834085586084257E-14 ) ) ;
#11296 = CARTESIAN_POINT ( 'NONE',  ( 6.742108083425078391, 15.99925261518604636, 9.534780690565009209 ) ) ;
#11297 = CARTESIAN_POINT ( 'NONE',  ( 2.418496320782090869, 0.8830982243829659240, 1.872697815963566992 ) ) ;
#11298 = CARTESIAN_POINT ( 'NONE',  ( 4.355193658487811703, 6.104145239700998538, -1.599625672291255185 ) ) ;
#11299 = CARTESIAN_POINT ( 'NONE',  ( 1.360316468749989793, 0.8177083336747339448, -0.7853790794159001276 ) ) ;
#11300 = CARTESIAN_POINT ( 'NONE',  ( 4.283913115580790354, 2.056533504189705930, -0.5163123687341104606 ) ) ;
#11301 = CONTEXT_DEPENDENT_SHAPE_REPRESENTATION ( #165472, #16098 ) ;
#11302 = CARTESIAN_POINT ( 'NONE',  ( 0.2231027806867662000, -0.09612335957175778545, 1.924217376148322334 ) ) ;
#11303 = ORIENTED_EDGE ( 'NONE', *, *, #162598, .F. ) ;
#11304 = CARTESIAN_POINT ( 'NONE',  ( -5.991777542596674166, 5.955104985976372944, 0.000000000000000000 ) ) ;
#11305 = CARTESIAN_POINT ( 'NONE',  ( 9.759171643738394408, 10.28012176064996197, 0.000000000000000000 ) ) ;
#11306 = CARTESIAN_POINT ( 'NONE',  ( 6.672020991256494504, 6.956648375986938859, 0.000000000000000000 ) ) ;
#11307 = CARTESIAN_POINT ( 'NONE',  ( -1.737499999999997824, -1.297916665710750150, 3.009438278150925683 ) ) ;
#11308 = CARTESIAN_POINT ( 'NONE',  ( -4.283486466913726254, 7.084819080452935403, -1.199719254218452047 ) ) ;
#11309 = CARTESIAN_POINT ( 'NONE',  ( 6.533471381225442798, -0.1521382079053348602, 2.086446650026114735 ) ) ;
#11310 = CARTESIAN_POINT ( 'NONE',  ( 1.079290920250153496, -0.05147710300976635067, -2.105495365820194920 ) ) ;
#11311 = CARTESIAN_POINT ( 'NONE',  ( -5.926849427829407269, 6.943687749669614995, -1.199719254218453823 ) ) ;
#11312 = CARTESIAN_POINT ( 'NONE',  ( 9.887974103068218668, 10.43039129653476493, 0.7998128361456462443 ) ) ;
#11313 = CARTESIAN_POINT ( 'NONE',  ( 5.858217239054963166, -1.861131630269092341, -0.001575894832107904492 ) ) ;
#11314 = CARTESIAN_POINT ( 'NONE',  ( 6.968000882419564945, 10.21675256520979858, 1.199719254218460707 ) ) ;
#11315 = CARTESIAN_POINT ( 'NONE',  ( 4.879410147971470657, 4.944948943068641967, -0.7687999843507594688 ) ) ;
#11316 = CARTESIAN_POINT ( 'NONE',  ( -5.632486471834530661, 5.535932070087196344, -0.7998128361456362523 ) ) ;
#11317 = CARTESIAN_POINT ( 'NONE',  ( -4.288456660624211381, 3.897620947016656956, 1.214306433183764966E-14 ) ) ;
#11318 = AXIS2_PLACEMENT_3D ( 'NONE', #60726, #163577, #47709 ) ;
#11319 = CARTESIAN_POINT ( 'NONE',  ( -5.764883781430355292, 7.068005876895869122, 2.440105357730325331 ) ) ;
#11321 = CARTESIAN_POINT ( 'NONE',  ( 2.260140581184489239, -1.961506502764579052, 0.04509734162668613960 ) ) ;
#11320 = CARTESIAN_POINT ( 'NONE',  ( -1.225000000000004086, -0.2708333333333212689, -0.7072540797572958171 ) ) ;
#11322 = CARTESIAN_POINT ( 'NONE',  ( 1.200320640528436789, -2.161883444890321915, 0.0006282887012112879947 ) ) ;
#11323 = CIRCLE ( 'NONE', #59729, 12.00000000000000178 ) ;
#11325 = CARTESIAN_POINT ( 'NONE',  ( -6.131443063645894753, 6.000026256920684808, -0.1528826387674747100 ) ) ;
#11324 = CARTESIAN_POINT ( 'NONE',  ( -4.450819567036169211, 8.414649604842665553, -0.7998128361456362523 ) ) ;
#11326 = CARTESIAN_POINT ( 'NONE',  ( -1.364683531250014514, 1.738541667008085545, -0.7879004041258289570 ) ) ;
#11327 = CARTESIAN_POINT ( 'NONE',  ( 3.251044507966997177, -1.707695807076513805, -0.2988343314351063484 ) ) ;
#11328 = CARTESIAN_POINT ( 'NONE',  ( 2.062088869592033635, -1.590637294955974390, -0.7065417998822677292 ) ) ;
#11329 = CARTESIAN_POINT ( 'NONE',  ( 6.832946231607457399, 7.074118146404578589, -0.7216878364870257245 ) ) ;
#11330 = CARTESIAN_POINT ( 'NONE',  ( -11.83627402213341107, 4.942735150756283780, -4.855302456647772935 ) ) ;
#11331 = CARTESIAN_POINT ( 'NONE',  ( 1.739611019359630584, -1.913509794028777522, -0.6351045200190530426 ) ) ;
#11332 = CARTESIAN_POINT ( 'NONE',  ( 6.825078400183551608, 0.5660753733540256905, 2.196387875007102419 ) ) ;
#11333 = CARTESIAN_POINT ( 'NONE',  ( -5.646044625448194410, 5.551749915969804938, 0.000000000000000000 ) ) ;
#11334 = CARTESIAN_POINT ( 'NONE',  ( 1.375784083019690351, 1.172551417808114893, 1.584734682399450145 ) ) ;
#11336 = CARTESIAN_POINT ( 'NONE',  ( -5.316205630334255972, 8.255971431148344308, -1.082531754730549967 ) ) ;
#11335 = CARTESIAN_POINT ( 'NONE',  ( 6.310809538426106258, -0.5167911955388967415, -1.841158844219364044 ) ) ;
#11337 = CARTESIAN_POINT ( 'NONE',  ( -5.926322542504877333, 7.047036066744706950, -1.082531754730549967 ) ) ;
#11338 = CARTESIAN_POINT ( 'NONE',  ( 5.956828388357757298, 8.042995434541133193, 1.599625672291269396 ) ) ;
#11339 = CARTESIAN_POINT ( 'NONE',  ( -5.769876891067536206, 8.889217585290882795, 1.199719254218454489 ) ) ;
#11340 = CARTESIAN_POINT ( 'NONE',  ( 1.699873857359509799, 1.394438142870989772, 1.461265194366095033 ) ) ;
#11341 = DIRECTION ( 'NONE',  ( 0.000000000000000000, 0.000000000000000000, 1.000000000000000000 ) ) ;
#11342 = CARTESIAN_POINT ( 'NONE',  ( 5.596783072813162896, -0.5536939349623200002, -2.240073236831362280 ) ) ;
#11343 = CARTESIAN_POINT ( 'NONE',  ( 5.353941776413853937, -0.7077614321437855072, 1.829919609802006741 ) ) ;
#11344 = CARTESIAN_POINT ( 'NONE',  ( 3.045700443693433179, 1.383923128670875746, 1.390673908496591782 ) ) ;
#11345 = CARTESIAN_POINT ( 'NONE',  ( 9.610031953988080744, 10.10612545594124967, -0.7998128361456281477 ) ) ;
#11346 = CARTESIAN_POINT ( 'NONE',  ( 0.2642963535325442148, 1.880433764241522088, -0.7283817610406126963 ) ) ;
#11347 = VERTEX_POINT ( 'NONE', #171008 ) ;
#11348 = CARTESIAN_POINT ( 'NONE',  ( 1.657563801924813784, 2.024516536105415820, -0.6199660602846206459 ) ) ;
#11350 = CARTESIAN_POINT ( 'NONE',  ( -6.509886312855995172, 10.74661779830734254, -0.7998128361456291469 ) ) ;
#11349 = CARTESIAN_POINT ( 'NONE',  ( -2.598358995313378550, 6.183169261174235487, 0.7998128361456341429 ) ) ;
#11351 = CARTESIAN_POINT ( 'NONE',  ( 1.693040327840355408, -0.6214066371539993527, 1.733238834403828754 ) ) ;
#11352 = ORIENTED_EDGE ( 'NONE', *, *, #160804, .F. ) ;
#11353 = CARTESIAN_POINT ( 'NONE',  ( 11.97020876039858628, 7.690570200886937435, -0.8734403169683351287 ) ) ;
#11354 = CARTESIAN_POINT ( 'NONE',  ( 2.496466685713152334, -1.086271176545396067, 1.821091972856798913 ) ) ;
#11355 = CARTESIAN_POINT ( 'NONE',  ( -1.500000000000011324, 4.702083334016148974, 0.8660254037844403729 ) ) ;
#11356 = CARTESIAN_POINT ( 'NONE',  ( 7.239163954692881653, 10.53310948286200599, -1.199719254218441611 ) ) ;
#11357 = CARTESIAN_POINT ( 'NONE',  ( 6.068156270568149324, 9.237210194708310951, 1.199719254218452047 ) ) ;
#11358 = ORIENTED_EDGE ( 'NONE', *, *, #33313, .T. ) ;
#11359 = CARTESIAN_POINT ( 'NONE',  ( 2.723961130741957781, -1.183836802208296568, -1.686624133856133412 ) ) ;
#11360 = AXIS2_PLACEMENT_3D ( 'NONE', #61323, #206490, #59176 ) ;
#11362 = CARTESIAN_POINT ( 'NONE',  ( 0.4288785890452541105, 3.049942316455306113, 0.4196807566830256797 ) ) ;
#11361 = CARTESIAN_POINT ( 'NONE',  ( -6.340409392685171674, 10.54889472477470846, 0.7998128361456481317 ) ) ;
#11363 = CARTESIAN_POINT ( 'NONE',  ( -1.364683531250010295, 4.030208333674751842, 0.7879004041258379498 ) ) ;
#11364 = FACE_OUTER_BOUND ( 'NONE', #112380, .T. ) ;
#11365 = CARTESIAN_POINT ( 'NONE',  ( 1.423138288543973617, 3.789741015373900623, 0.4995221786828039634 ) ) ;
#11366 = DIRECTION ( 'NONE',  ( -0.000000000000000000, -1.000000000000000000, -0.000000000000000000 ) ) ;
#11367 = CARTESIAN_POINT ( 'NONE',  ( 2.741812758617673040, -1.674694146245614412, -1.521292302590461665 ) ) ;
#11368 = CARTESIAN_POINT ( 'NONE',  ( -8.188761592974040937, 11.53701037756964887, -1.082531754730543971 ) ) ;
#11369 = CARTESIAN_POINT ( 'NONE',  ( 2.777393361597128685, 0.2615887081860277519, -1.792441719956331170 ) ) ;
#11370 = CARTESIAN_POINT ( 'NONE',  ( 3.608511690770484837, 1.820787697044351505, 0.5958877267112758780 ) ) ;
#11371 = CARTESIAN_POINT ( 'NONE',  ( 3.771986465066007099, -2.040223509676724500, 0.3510349978646867264 ) ) ;
#11372 = CARTESIAN_POINT ( 'NONE',  ( -1.364683531250012516, 2.592708333674753174, 0.7879004041258379498 ) ) ;
#11373 = CARTESIAN_POINT ( 'NONE',  ( 2.500799400523348037, 1.584503739761052188, -1.172863459551294341 ) ) ;
#11374 = CARTESIAN_POINT ( 'NONE',  ( 6.410771793481705672, 1.425725087049932505, -1.295833391663123724 ) ) ;
#11375 = CARTESIAN_POINT ( 'NONE',  ( 3.028041890241763401, 1.040506211802554981, -1.554362669439563360 ) ) ;
#11376 = EDGE_CURVE ( 'NONE', #2318, #33454, #142846, .T. ) ;
#11378 = CARTESIAN_POINT ( 'NONE',  ( 4.595358334023878832, 8.489709390108890474, -0.01759220550971198060 ) ) ;
#11377 = CARTESIAN_POINT ( 'NONE',  ( 2.719673384174253972, -0.2251885735481904405, 2.296679687964820360 ) ) ;
#11379 = CARTESIAN_POINT ( 'NONE',  ( 2.945584473374110779, 1.314022426170344815, 1.318171089286435560 ) ) ;
#11380 = CARTESIAN_POINT ( 'NONE',  ( -0.6823417656250212460, 3.051041667008084879, 1.181850606188767472 ) ) ;
#11381 = CARTESIAN_POINT ( 'NONE',  ( 6.777782349474076540, -2.001779569883685106, 0.4972090909861492936 ) ) ;
#11383 = CARTESIAN_POINT ( 'NONE',  ( -3.598799709423620374, 6.286017863381107240, 1.199719254218464037 ) ) ;
#11382 = AXIS2_PLACEMENT_3D ( 'NONE', #137681, #202638, #122579 ) ;
#11384 = CARTESIAN_POINT ( 'NONE',  ( 6.449928391799196525, 8.548002428564306143, -1.599625672291262513 ) ) ;
#11385 = CARTESIAN_POINT ( 'NONE',  ( -1.443823057115803055, 3.571423696980855489, 0.4219843264275927597 ) ) ;
#11386 = CARTESIAN_POINT ( 'NONE',  ( 0.1355649208573142805, -1.924581242375450030, 0.8557158107796616342 ) ) ;
#11387 = CARTESIAN_POINT ( 'NONE',  ( -0.6823417656250212460, 3.613541667008085767, 1.181850606188767472 ) ) ;
#11388 = CARTESIAN_POINT ( 'NONE',  ( 6.098930168602409552, 1.771044849343451633, -1.239067683784184748 ) ) ;
#11389 = CARTESIAN_POINT ( 'NONE',  ( 6.428379779529339366, -0.9538188281377130151, -1.780268319267635846 ) ) ;
#11390 = CARTESIAN_POINT ( 'NONE',  ( -0.6823417656250246877, 0.05104166700808931978, 1.181850606188755259 ) ) ;
#11391 = CARTESIAN_POINT ( 'NONE',  ( -5.273758566035884776, 5.255065869904374409, 0.000000000000000000 ) ) ;
#11392 = VECTOR ( 'NONE', #196537, 1000.000000000000000 ) ;
#11395 = CARTESIAN_POINT ( 'NONE',  ( 5.694061328059515148, 5.745419092265303007, -0.7216878364870207285 ) ) ;
#11394 = CARTESIAN_POINT ( 'NONE',  ( -3.285556943750000070, -0.4593749995220435256, 0.000000000000000000 ) ) ;
#11393 = CARTESIAN_POINT ( 'NONE',  ( 4.715203562502613188, 8.723097599553565118, 0.7998128361456341429 ) ) ;
#11396 = CARTESIAN_POINT ( 'NONE',  ( -4.625266680917477835, 5.425174544939014964, -1.199719254218453823 ) ) ;
#11397 = CARTESIAN_POINT ( 'NONE',  ( 4.276577519141481432, -0.4465006364167342645, -1.966305148836451577 ) ) ;
#11398 = CARTESIAN_POINT ( 'NONE',  ( -6.690058733339450114, 9.892486724616283311, 1.199719254218452047 ) ) ;
#11400 = CARTESIAN_POINT ( 'NONE',  ( -6.251718229232846369, 9.347402796530044355, -1.082531754730549967 ) ) ;
#11399 = CARTESIAN_POINT ( 'NONE',  ( -8.026063749610047537, 11.34719622697832264, -1.082531754730543971 ) ) ;
#11401 = DIRECTION ( 'NONE',  ( -0.000000000000000000, -1.000000000000000000, -0.000000000000000000 ) ) ;
#11403 = CARTESIAN_POINT ( 'NONE',  ( -1.364683531250010740, 9.380208333674735499, 0.7879004041258445001 ) ) ;
#11402 = CARTESIAN_POINT ( 'NONE',  ( 5.981359018292748075, 1.999130597612966742, -0.8229454869796914984 ) ) ;
#11404 = CARTESIAN_POINT ( 'NONE',  ( 10.38894090356631139, 1.970899860167849127, -5.551243578533891387 ) ) ;
#11406 = CARTESIAN_POINT ( 'NONE',  ( -9.001723924469462901, 12.58942944760136484, -1.199719254218446718 ) ) ;
#11405 = B_SPLINE_CURVE_WITH_KNOTS ( 'NONE', 3,
 ( #7967, #139073, #56739, #123964 ),
 .UNSPECIFIED., .F., .F.,
 ( 4, 4 ),
 ( 0.002059939351769829192, 0.002341702326271049867 ),
 .UNSPECIFIED. ) ;
#11408 = CARTESIAN_POINT ( 'NONE',  ( 6.573846656420020196, -0.8593871168269312522, 1.822298249534954673 ) ) ;
#11407 = CARTESIAN_POINT ( 'NONE',  ( -7.063434842595444962, 8.303390740191881392, 1.082531754730549967 ) ) ;
#11409 = CARTESIAN_POINT ( 'NONE',  ( 1.364683531249986537, 0.9260416670080896528, 0.7879004041258500513 ) ) ;
#11410 = EDGE_CURVE ( 'NONE', #127623, #2109, #69198, .T. ) ;
#11411 = CIRCLE ( 'NONE', #122067, 2.000000000000000000 ) ;
#11412 = PLANE ( 'NONE',  #193551 ) ;
#11413 = CARTESIAN_POINT ( 'NONE',  ( 2.086159243269372521, -1.691233086580298695, -0.3380474007560717031 ) ) ;
#11414 = CARTESIAN_POINT ( 'NONE',  ( 7.856023664475727308, 8.130058794835305136, -0.7998128361456341429 ) ) ;
#11415 = CARTESIAN_POINT ( 'NONE',  ( 4.844006021832467646, 8.873367135438366304, 0.000000000000000000 ) ) ;
#11416 = CARTESIAN_POINT ( 'NONE',  ( -11.08262820474602250, 7.067544101916862331, -4.606611893229879406 ) ) ;
#11417 = CARTESIAN_POINT ( 'NONE',  ( 1.053533388295304629, 1.768092659605845052, -0.07913920300933743879 ) ) ;
#11418 = CARTESIAN_POINT ( 'NONE',  ( 1.699859389132576837, 1.389752512480733060, 1.456620396263593520 ) ) ;
#11419 = CARTESIAN_POINT ( 'NONE',  ( 4.331241739176756589, 0.1049304944579672605, 2.204394592675275710 ) ) ;
#11420 = CARTESIAN_POINT ( 'NONE',  ( 5.612245307067635025, 2.168910047263863827, -0.09915484274719725544 ) ) ;
#11421 = EDGE_LOOP ( 'NONE', ( #161579, #41739, #186545, #14360, #111637, #203733, #125969, #131833 ) ) ;
#11422 = FACE_OUTER_BOUND ( 'NONE', #155978, .T. ) ;
#11423 = CARTESIAN_POINT ( 'NONE',  ( 8.880227426826646564, 9.462612874160329923, 0.7216878364870458196 ) ) ;
#11425 = CARTESIAN_POINT ( 'NONE',  ( 3.040638836679772528, -1.525031945187466098, 1.319243992433154267 ) ) ;
#11424 = CARTESIAN_POINT ( 'NONE',  ( 2.930460433956377564, -1.047063434655249647, -1.843881786051679850 ) ) ;
#11427 = EDGE_LOOP ( 'NONE', ( #37506, #127124, #157490, #49976 ) ) ;
#11426 = CARTESIAN_POINT ( 'NONE',  ( 3.252039308394638173, 0.8100161731663655384, -1.620448113725055483 ) ) ;
#11428 = CARTESIAN_POINT ( 'NONE',  ( 4.850785098639300408, 8.881276058379668825, -0.7998128361456481317 ) ) ;
#11429 = ORIENTED_EDGE ( 'NONE', *, *, #18201, .F. ) ;
#11430 = CARTESIAN_POINT ( 'NONE',  ( 0.000000000000000000, 2.099999999999997868, 0.000000000000000000 ) ) ;
#11431 = CARTESIAN_POINT ( 'NONE',  ( 4.310602774141044868, 7.116454772218158809, -1.199719254218452047 ) ) ;
#11432 = CARTESIAN_POINT ( 'NONE',  ( 6.024025069106937913, -1.018266858664597763, -1.515143308444939274 ) ) ;
#11434 = CARTESIAN_POINT ( 'NONE',  ( 1.516650397601801759, 0.1914660871255029484, 1.906153142492900132 ) ) ;
#11433 = CARTESIAN_POINT ( 'NONE',  ( -3.469997250093771246, 6.135748327496311383, -1.199719254218452935 ) ) ;
#11435 = PRESENTATION_STYLE_ASSIGNMENT (( #26625 ) ) ;
#11436 = CARTESIAN_POINT ( 'NONE',  ( 1.403499169903295263, 7.376709478543810761, -4.304123474983216902 ) ) ;
#11437 = CARTESIAN_POINT ( 'NONE',  ( 1.364683531249986537, 1.217708333674754950, -0.7879004041258239610 ) ) ;
#11438 = DIRECTION ( 'NONE',  ( 0.000000000000000000, 1.000000000000000000, 0.000000000000000000 ) ) ;
#11439 = CARTESIAN_POINT ( 'NONE',  ( -8.239604668803112375, 10.63595808506888396, -1.599625672291263179 ) ) ;
#11440 = ORIENTED_EDGE ( 'NONE', *, *, #147573, .F. ) ;
#11441 = CARTESIAN_POINT ( 'NONE',  ( 5.155217493315787713, -1.824165352752779246, -1.159627250419709155 ) ) ;
#11442 = CARTESIAN_POINT ( 'NONE',  ( -5.994113311017573054, 6.165756082374834079, 0.7216878364870257245 ) ) ;
#11443 = EDGE_CURVE ( 'NONE', #166897, #157452, #130929, .T. ) ;
#11444 = CARTESIAN_POINT ( 'NONE',  ( -5.912237504011027767, 9.055304967058290799, 1.199719254218454489 ) ) ;
#11445 = CARTESIAN_POINT ( 'NONE',  ( 2.865608904542978674, -1.736054085904148669, -1.217558864107195937 ) ) ;
#11447 = CARTESIAN_POINT ( 'NONE',  ( -10.44369633504468631, 5.112959841837462882, -5.232137017608344820 ) ) ;
#11446 = CARTESIAN_POINT ( 'NONE',  ( -4.873355750086138194, 4.879908661787099255, 0.5084451132007505869 ) ) ;
#11448 =( BOUNDED_CURVE ( )  B_SPLINE_CURVE ( 3, ( #45548, #44480, #144145, #190693 ),
 .UNSPECIFIED., .F., .T. ) 
 B_SPLINE_CURVE_WITH_KNOTS ( ( 4, 4 ),
 ( 4.837716811552755125, 4.862957253161376059 ),
 .UNSPECIFIED. ) 
 CURVE ( )  GEOMETRIC_REPRESENTATION_ITEM ( )  RATIONAL_B_SPLINE_CURVE ( ( 1.000000000000000000, 0.9999469107135832147, 0.9999469107135832147, 1.000000000000000000 ) ) 
 REPRESENTATION_ITEM ( '' )  );
#11449 = CARTESIAN_POINT ( 'NONE',  ( 4.288322324034578692, -1.949444798393678013, -0.2924651067536877536 ) ) ;
#11450 = CARTESIAN_POINT ( 'NONE',  ( -0.1228044941411730595, -1.800067586368118588, -0.9016598371343366169 ) ) ;
#11451 = VERTEX_POINT ( 'NONE', #141756 ) ;
#11452 = CARTESIAN_POINT ( 'NONE',  ( 6.051990796818580876, 1.090527953092842894, 1.814802726937503330 ) ) ;
#11453 = SURFACE_SIDE_STYLE ('',( #147877 ) ) ;
#11454 = CARTESIAN_POINT ( 'NONE',  ( 0.2739938332866619364, -2.030697503880642518, 0.4024348779970430834 ) ) ;
#11455 = CARTESIAN_POINT ( 'NONE',  ( 2.607286591753724014, -1.920749920159558810, 0.2854125566163211447 ) ) ;
#11456 = ORIENTED_EDGE ( 'NONE', *, *, #48444, .T. ) ;
#11457 = CARTESIAN_POINT ( 'NONE',  ( 2.276512373593124305, 5.629777788065645439, 0.5132344841170741745 ) ) ;
#11458 = CARTESIAN_POINT ( 'NONE',  ( 4.850785098639300408, 8.881276058379668825, -0.7998128361456481317 ) ) ;
#11460 = CARTESIAN_POINT ( 'NONE',  ( 5.120175567455225618, 9.125288595339771547, -0.7998128361456281477 ) ) ;
#11459 = CARTESIAN_POINT ( 'NONE',  ( 3.310569631373377231, 1.890246369116010960, 0.8934441069041214600 ) ) ;
#11461 = CARTESIAN_POINT ( 'NONE',  ( 3.512971199272317602, 6.152197928242737923, -1.082531754730549967 ) ) ;
#11463 = ORIENTED_EDGE ( 'NONE', *, *, #107473, .F. ) ;
#11462 = CARTESIAN_POINT ( 'NONE',  ( 0.1525891599635448848, 0.3075033511844190159, 1.785008687375288172 ) ) ;
#11464 = CARTESIAN_POINT ( 'NONE',  ( 5.373716497573798101, 2.127666891504222502, -0.5857064233696291922 ) ) ;
#11465 = CARTESIAN_POINT ( 'NONE',  ( -0.2118258318330372425, -6.614835951978776940, -10.99866081003794527 ) ) ;
#11466 = CARTESIAN_POINT ( 'NONE',  ( 3.417197246517459597, 1.994164043739574232, 0.9453733912969732867 ) ) ;
#11467 = CARTESIAN_POINT ( 'NONE',  ( 9.094822116668764167, 9.505047312402055582, 0.7998128361456462443 ) ) ;
#11468 = CYLINDRICAL_SURFACE ( 'NONE', #175789, 1.000000000000000222 ) ;
#11469 = EDGE_CURVE ( 'NONE', #121012, #213712, #206703, .T. ) ;
#11470 = CARTESIAN_POINT ( 'NONE',  ( 1.277824965264368728, 1.883817941867833134, -0.3277997056638781714 ) ) ;
#11471 = COLOUR_RGB ( '', 0.31764706, 0.68627451, 0.89019608) ;
#11472 = CARTESIAN_POINT ( 'NONE',  ( 7.886038904643079661, 12.35212915539230139, -0.7998128361456352531 ) ) ;
#11473 = CARTESIAN_POINT ( 'NONE',  ( 5.617656447048144486, 0.4075009240860454907, -2.029694874052537568 ) ) ;
#11474 = AXIS2_PLACEMENT_3D ( 'NONE', #84087, #150175, #1743 ) ;
#11475 = CARTESIAN_POINT ( 'NONE',  ( 2.571340117545738657, 0.1069729528509130723, -2.159185227005658181 ) ) ;
#11476 = CARTESIAN_POINT ( 'NONE',  ( 4.353197867323560288, 0.4795420089713005041, -2.138300074133951068 ) ) ;
#11477 = VERTEX_POINT ( 'NONE', #175296 ) ;
#11478 = CARTESIAN_POINT ( 'NONE',  ( 9.480175724453529185, 12.08329098332774265, 1.599625672291279388 ) ) ;
#11479 = FACE_OUTER_BOUND ( 'NONE', #135491, .T. ) ;
#11480 = CARTESIAN_POINT ( 'NONE',  ( -0.4491468415841158301, 7.944909564338812125, 1.993991491228178869 ) ) ;
#11481 = CARTESIAN_POINT ( 'NONE',  ( 3.898851692381625877, 6.706354853490643642, -1.199719254218452047 ) ) ;
#11482 = FACE_OUTER_BOUND ( 'NONE', #131641, .T. ) ;
#11483 = CARTESIAN_POINT ( 'NONE',  ( -4.625266680917477835, 5.425174544939014964, -1.199719254218453823 ) ) ;
#11484 = CARTESIAN_POINT ( 'NONE',  ( 0.4400775573648734174, -1.704940109561555950, -1.076314675215600314 ) ) ;
#11485 = CARTESIAN_POINT ( 'NONE',  ( -9.666600336863641729, 10.38004793587015584, 1.040834085586084257E-14 ) ) ;
#11486 = CARTESIAN_POINT ( 'NONE',  ( 5.224688093219824303, 7.188831756880171397, -1.599625672291283607 ) ) ;
#11487 = CARTESIAN_POINT ( 'NONE',  ( 5.383670357325340383, -1.967593191946028996, 0.6441560278484458335 ) ) ;
#11488 = CARTESIAN_POINT ( 'NONE',  ( 4.846275584324886587, 1.921458954407113451, 0.1401587531122197583 ) ) ;
#11489 = CARTESIAN_POINT ( 'NONE',  ( 0.1929827526203631294, 1.755782054984224683, 0.9913788669043410717 ) ) ;
#11490 = CARTESIAN_POINT ( 'NONE',  ( -1.040834085586084257E-14, -7.126685749120009739, 9.926723642588090257 ) ) ;
#11491 = CARTESIAN_POINT ( 'NONE',  ( 3.960953433486789521, 7.772862772376584850, -0.7998128361456221525 ) ) ;
#11493 = EDGE_CURVE ( 'NONE', #16624, #13808, #3343, .T. ) ;
#11492 = DIRECTION ( 'NONE',  ( 0.000000000000000000, 0.000000000000000000, -1.000000000000000000 ) ) ;
#11494 = CARTESIAN_POINT ( 'NONE',  ( 3.608217298448283206, 1.969629311412910866, 0.004557946788486669405 ) ) ;
#11495 = CARTESIAN_POINT ( 'NONE',  ( 0.4631483011842302266, 0.2107759881739781904, -2.181290363801504650 ) ) ;
#11496 = CARTESIAN_POINT ( 'NONE',  ( 3.686012862905340803, -0.8985999850123352894, 1.589152278004740237 ) ) ;
#11497 = EDGE_CURVE ( 'NONE', #109299, #83910, #150502, .T. ) ;
#11498 = CARTESIAN_POINT ( 'NONE',  ( 6.373741612200162443, 8.529394195690610303, 1.443375672974065660 ) ) ;
#11499 = CARTESIAN_POINT ( 'NONE',  ( 5.002595493318194642, 4.938708951733754127, -0.7216878364870197293 ) ) ;
#11500 = CARTESIAN_POINT ( 'NONE',  ( -6.469175572376043348, 7.576401584974034265, 1.199719254218452047 ) ) ;
#11501 = CARTESIAN_POINT ( 'NONE',  ( 5.903649544107831382, 5.852288987739402870, -0.7998128361456481317 ) ) ;
#11502 = VERTEX_POINT ( 'NONE', #191508 ) ;
#11504 = CARTESIAN_POINT ( 'NONE',  ( 4.676043659170272093, 1.990676093108449951, -0.2997180003130732739 ) ) ;
#11503 = CARTESIAN_POINT ( 'NONE',  ( 1.346931166825489967, 0.5339940059071214273, -1.762130705996706181 ) ) ;
#11505 = CARTESIAN_POINT ( 'NONE',  ( 1.177631936369994303, -1.035077938576201451, -2.052156377449709357 ) ) ;
#11506 = CARTESIAN_POINT ( 'NONE',  ( 5.383633123045536983, -1.864019207510819953, 0.6117972396969260096 ) ) ;
#11507 = CARTESIAN_POINT ( 'NONE',  ( -4.205000198532790279, 8.057583998263570635, 0.7998128361456341429 ) ) ;
#11508 = CARTESIAN_POINT ( 'NONE',  ( 0.000000000000000000, 9.799999999999982947, 0.000000000000000000 ) ) ;
#11509 = CARTESIAN_POINT ( 'NONE',  ( -3.948449050077848632, 5.629609863222681199, 1.599625672291267398 ) ) ;
#11510 = CARTESIAN_POINT ( 'NONE',  ( 0.9243811426856913815, 1.018911950503737174, 1.802186752163869699 ) ) ;
#11511 = CARTESIAN_POINT ( 'NONE',  ( -4.960304097753355457, 6.880383762169266504, 1.599625672291263179 ) ) ;
#11513 = CARTESIAN_POINT ( 'NONE',  ( 6.596581986989779267, -0.4770763175313968429, -1.704276504685025673 ) ) ;
#11512 = CARTESIAN_POINT ( 'NONE',  ( 0.9782033901477287241, -2.040585271250746846, -0.4545043172074214599 ) ) ;
#11514 = CARTESIAN_POINT ( 'NONE',  ( 2.359223927328457648E-13, 7.078193277237625480, 2.121339347286388843 ) ) ;
#11515 = CARTESIAN_POINT ( 'NONE',  ( -0.1102773484824119410, 4.081664357266182819, -2.758211214536327116 ) ) ;
#11516 = CARTESIAN_POINT ( 'NONE',  ( 2.085156077859366519, -0.7432962182043149069, 1.573855765194108081 ) ) ;
#11517 = AXIS2_PLACEMENT_3D ( 'NONE', #25231, #45785, #141173 ) ;
#11518 = CARTESIAN_POINT ( 'NONE',  ( 6.322179702674084467, 6.270297829408224111, 1.040834085586084257E-14 ) ) ;
#11520 = FACE_OUTER_BOUND ( 'NONE', #148034, .T. ) ;
#11519 = DIRECTION ( 'NONE',  ( 0.000000000000000000, 0.000000000000000000, -1.000000000000000000 ) ) ;
#11521 = CARTESIAN_POINT ( 'NONE',  ( 1.822448697576475540, 1.608646582964175176, 0.6229558172686412432 ) ) ;
#11522 = CARTESIAN_POINT ( 'NONE',  ( 2.173600921376659834, 1.351110561487681716, 1.725424542402646422 ) ) ;
#11523 = CARTESIAN_POINT ( 'NONE',  ( 3.914836437932368796, 1.561248537261412883, -1.560010120355350471 ) ) ;
#11524 = CARTESIAN_POINT ( 'NONE',  ( -11.38600250725030172, 3.712543481068769857, -5.706073308245968256 ) ) ;
#11525 = CARTESIAN_POINT ( 'NONE',  ( 2.782273231148081116, -1.246650745954593464, -1.777310168556520464 ) ) ;
#11526 = CARTESIAN_POINT ( 'NONE',  ( 0.8030139110496161692, 1.490934425176414502, 1.053415343471690857 ) ) ;
#11527 = CARTESIAN_POINT ( 'NONE',  ( 3.538375268227810011, 0.7659831068804138221, 1.974087397274668643 ) ) ;
#11528 = CARTESIAN_POINT ( 'NONE',  ( 6.539320575229257138, 2.987941927008979537, 2.250856951216452906 ) ) ;
#11529 = EDGE_LOOP ( 'NONE', ( #127053, #177665, #111076, #68710 ) ) ;
#11531 = CARTESIAN_POINT ( 'NONE',  ( 1.364683531249986537, 1.967708333674750731, -0.7879004041258239610 ) ) ;
#11530 = CARTESIAN_POINT ( 'NONE',  ( 4.107168962890386688, -0.3918867163640211704, 2.258474592593032959 ) ) ;
#11532 = CARTESIAN_POINT ( 'NONE',  ( 3.871016551901614200, 4.474939717762034697, -1.199719254218446718 ) ) ;
#11533 = CARTESIAN_POINT ( 'NONE',  ( 5.203632029546647608, 4.965325544092860532, 1.040834085586084257E-14 ) ) ;
#11534 = CARTESIAN_POINT ( 'NONE',  ( 6.235052692738393354, 2.071546745583602522, 0.8022605484305275203 ) ) ;
#11535 = CARTESIAN_POINT ( 'NONE',  ( -6.561783159334137139, 8.678499657355050800, -1.443375672974059665 ) ) ;
#11536 = CARTESIAN_POINT ( 'NONE',  ( 4.039966587192257208, 6.696749537490852333, 1.082531754730558626 ) ) ;
#11537 = AXIS2_PLACEMENT_3D ( 'NONE', #9463, #141646, #207655 ) ;
#11538 = CARTESIAN_POINT ( 'NONE',  ( -6.683806541412768532, 8.820860269780128604, -1.443375672974058777 ) ) ;
#11539 = CIRCLE ( 'NONE', #136023, 0.4000000000000001887 ) ;
#11540 = CARTESIAN_POINT ( 'NONE',  ( 6.825078400183556049, 1.282741234726337165, 1.971047034039686174 ) ) ;
#11541 = ORIENTED_EDGE ( 'NONE', *, *, #81633, .F. ) ;
#11542 = CARTESIAN_POINT ( 'NONE',  ( 4.149064681782777875, 0.9530105817698063531, 1.777011888912001014 ) ) ;
#11544 = CARTESIAN_POINT ( 'NONE',  ( 2.676693276584718895, 1.350517573672470606, -1.558986216346124776 ) ) ;
#11543 = CARTESIAN_POINT ( 'NONE',  ( 5.774883364416965037, 8.824782127540085952, -1.199719254218440723 ) ) ;
#11545 = CARTESIAN_POINT ( 'NONE',  ( 6.471393748265540147, 5.229711127717882491, 2.420000000000010587 ) ) ;
#11546 = CARTESIAN_POINT ( 'NONE',  ( 3.079110283634975964, 6.606396074300548982, 0.7216878364870257245 ) ) ;
#11547 = CARTESIAN_POINT ( 'NONE',  ( -1.642778471875000035, -3.667708332855373676, -2.845375778867859751 ) ) ;
#11548 = CARTESIAN_POINT ( 'NONE',  ( 0.6823417656249917140, 4.842708333674755394, 1.181850606188765695 ) ) ;
#11549 = CARTESIAN_POINT ( 'NONE',  ( 4.875033280109006384, 2.045454206080063120, -0.7869404205859964474 ) ) ;
#11550 = CARTESIAN_POINT ( 'NONE',  ( 2.988907892087853568, -2.013985899409028946, 0.1017507309580278629 ) ) ;
#11551 = CARTESIAN_POINT ( 'NONE',  ( 2.190726087351921425, 1.424366561657765207, 1.166803476217087576 ) ) ;
#11552 = CARTESIAN_POINT ( 'NONE',  ( 7.983053520348166288, 8.207983950027992748, -0.7998128361456281477 ) ) ;
#11553 =( NAMED_UNIT ( * ) PLANE_ANGLE_UNIT ( ) SI_UNIT ( $, .RADIAN. ) );
#11554 = CARTESIAN_POINT ( 'NONE',  ( 5.965807262869926575, 1.798080572464531679, -0.3147057940002598864 ) ) ;
#11555 = AXIS2_PLACEMENT_3D ( 'NONE', #54180, #33655, #2192 ) ;
#11556 = CARTESIAN_POINT ( 'NONE',  ( -8.525379664894808585, 8.840697785332414682, -0.7998128361456291469 ) ) ;
#11558 = CARTESIAN_POINT ( 'NONE',  ( -5.330290668828105538, 6.247702530834755130, 1.199719254218452935 ) ) ;
#11557 = CARTESIAN_POINT ( 'NONE',  ( 5.506774338047922157, 1.717276559928378132, -1.473185486808053835 ) ) ;
#11559 = CARTESIAN_POINT ( 'NONE',  ( 1.418734189139436275, 1.413363300903627717, -1.561561204404242842 ) ) ;
#11560 = CARTESIAN_POINT ( 'NONE',  ( -5.803772275101700906, 8.928762199997411386, -1.199719254218452047 ) ) ;
#11561 = CARTESIAN_POINT ( 'NONE',  ( 8.483651433849084711, 10.92067931095586886, 1.599625672291281386 ) ) ;
#11562 = CARTESIAN_POINT ( 'NONE',  ( 5.817857313595521163, 9.801600942587855414, -0.7216878364870458196 ) ) ;
#11563 = DIRECTION ( 'NONE',  ( 0.4522552831782836735, -0.8434774318626376832, 0.2898464779426172533 ) ) ;
#11564 = CARTESIAN_POINT ( 'NONE',  ( -6.177711549321182716, 10.35908057418338402, 0.7998128361456481317 ) ) ;
#11565 = DIRECTION ( 'NONE',  ( 1.000000000000000000, 0.000000000000000000, 0.000000000000000000 ) ) ;
#11566 = CARTESIAN_POINT ( 'NONE',  ( 8.568389893712330618, 9.098802418860289620, 1.040834085586084257E-14 ) ) ;
#11567 = CARTESIAN_POINT ( 'NONE',  ( 4.250508905105749413, 7.277302409985156650, -0.9232175757047023090 ) ) ;
#11568 = CARTESIAN_POINT ( 'NONE',  ( -8.758204044748012507, 11.24099069033793974, 1.443375672974064550 ) ) ;
#11570 = CARTESIAN_POINT ( 'NONE',  ( 2.391161334010579509, -2.127237363102509882, -0.6400520371602820280 ) ) ;
#11569 = CARTESIAN_POINT ( 'NONE',  ( 1.652743449602233072, 2.098267697663995790, 0.3060111223712052020 ) ) ;
#11571 = CARTESIAN_POINT ( 'NONE',  ( 6.883263157960364254, 6.036844454314826081, 2.541088405340941492 ) ) ;
#11572 = CARTESIAN_POINT ( 'NONE',  ( -7.123883369337781879, 7.275895117174344229, 0.7998128361456341429 ) ) ;
#11573 = CARTESIAN_POINT ( 'NONE',  ( 4.473300617505036492, 7.306268922809479704, -1.199719254218452047 ) ) ;
#11574 = CARTESIAN_POINT ( 'NONE',  ( 4.615648854252428102, 0.4318217149890530848, -1.913582009320368371 ) ) ;
#11575 = CARTESIAN_POINT ( 'NONE',  ( 8.594979316059474073, 12.11489407112305372, 1.199719254218450271 ) ) ;
#11576 = CARTESIAN_POINT ( 'NONE',  ( -5.638288519115033814, 6.168138913823901781, 0.8326226707794943671 ) ) ;
#11577 = CARTESIAN_POINT ( 'NONE',  ( -1.364683531250014514, 0.2385416670080863499, -0.7879004041258359514 ) ) ;
#11578 = CARTESIAN_POINT ( 'NONE',  ( -3.512971199716682591, 7.112567143062499930, 0.000000000000000000 ) ) ;
#11579 = CARTESIAN_POINT ( 'NONE',  ( -6.670248388243482651, 9.765411638717282017, 1.082531754730548412 ) ) ;
#11580 = CARTESIAN_POINT ( 'NONE',  ( 3.814780496183818315, -0.6684712460508880350, -2.012520831323429515 ) ) ;
#11581 = CARTESIAN_POINT ( 'NONE',  ( -5.581116510680924847, 6.540332679663050541, -1.199719254218453823 ) ) ;
#11582 = CARTESIAN_POINT ( 'NONE',  ( 4.838837662799537753, 0.3661284547709364734, 2.130314178654398205 ) ) ;
#11583 = CARTESIAN_POINT ( 'NONE',  ( 3.860763913883006992, 0.2215400755124704024, -1.827792592973469743 ) ) ;
#11584 = CARTESIAN_POINT ( 'NONE',  ( -4.653572958549120564, 6.905085616583060748, 1.214936962016188726 ) ) ;
#11585 = CARTESIAN_POINT ( 'NONE',  ( -1.364683531250014514, -0.1572916663252435232, 0.7879004041258379498 ) ) ;
#11586 = CARTESIAN_POINT ( 'NONE',  ( 5.367066450689647716, 1.675684007255513475, -0.4696764748959629809 ) ) ;
#11587 = CARTESIAN_POINT ( 'NONE',  ( 6.727182134110203826, 2.985950691969770254, 2.264927069331075238 ) ) ;
#11588 = CARTESIAN_POINT ( 'NONE',  ( 2.684151225825664788, 5.114964949229812596, -1.082531754730543083 ) ) ;
#11589 = CARTESIAN_POINT ( 'NONE',  ( -6.368956045697454549, 6.779621784316542055, -0.6049335659975106916 ) ) ;
#11590 = CARTESIAN_POINT ( 'NONE',  ( 2.553791647773369089, 0.5774160426356907960, -2.083079400968433248 ) ) ;
#11591 = CARTESIAN_POINT ( 'NONE',  ( 5.395861176733054876, 0.1455124041884261754, 2.010896217931843921 ) ) ;
#11592 = CARTESIAN_POINT ( 'NONE',  ( -8.527715432871366019, 10.01171809551380143, 1.082531754730558626 ) ) ;
#11593 = CARTESIAN_POINT ( 'NONE',  ( 2.641676655999642076, -1.601130012699041982, -1.452526871000489495 ) ) ;
#11594 = CARTESIAN_POINT ( 'NONE',  ( 3.831288253049653481, -1.822718488796180925, 0.7514253593702052703 ) ) ;
#11595 = CARTESIAN_POINT ( 'NONE',  ( 2.000000000000000000, 2.453105802350469389E-14, -1.733336949948507013E-30 ) ) ;
#11596 = CARTESIAN_POINT ( 'NONE',  ( 4.265135581495039574, 1.882949608596860669, -0.4750026310351186387 ) ) ;
#11599 = VERTEX_POINT ( 'NONE', #162232 ) ;
#11598 = CARTESIAN_POINT ( 'NONE',  ( 7.967649405165779797, -5.251137252134810751, -7.547231044119373067 ) ) ;
#11597 = CARTESIAN_POINT ( 'NONE',  ( -9.178506806327330736, 10.77097469787910455, 1.082531754730558626 ) ) ;
#11600 = CARTESIAN_POINT ( 'NONE',  ( -6.954406449166956605, 7.078172043641714595, -0.7998128361456362523 ) ) ;
#11601 = CARTESIAN_POINT ( 'NONE',  ( 11.92619525870748021, 10.07377703206318031, 1.328859154005125554 ) ) ;
#11603 = ORIENTED_EDGE ( 'NONE', *, *, #137720, .T. ) ;
#11602 = CARTESIAN_POINT ( 'NONE',  ( -3.630551273409382329, 7.457669928944732796, 0.7998128361456352531 ) ) ;
#11604 = CARTESIAN_POINT ( 'NONE',  ( -8.148087131688683371, 11.48955683940339867, -1.082531754730543083 ) ) ;
#11605 = CARTESIAN_POINT ( 'NONE',  ( 2.309865001130634976, -0.4838574416936823885, 2.152911442350906146 ) ) ;
#11606 = CARTESIAN_POINT ( 'NONE',  ( -1.642778471874998480, -0.7510416661887092671, 2.845375778867863303 ) ) ;
#11607 = CARTESIAN_POINT ( 'NONE',  ( 6.121922100595678096, 1.933298025717408608, -0.3319332437697538607 ) ) ;
#11608 = CARTESIAN_POINT ( 'NONE',  ( 1.364683531249988535, 5.717708333674752730, -0.7879004041258300672 ) ) ;
#11609 = CARTESIAN_POINT ( 'NONE',  ( -0.7499999999999972244, 3.639583334016149863, -1.299038105676652011 ) ) ;
#11610 = CARTESIAN_POINT ( 'NONE',  ( 5.997902985473373860, 6.089292839903872157, -0.6134941253506603909 ) ) ;
#11612 = CARTESIAN_POINT ( 'NONE',  ( 1.499999999999993117, 12.63541666734946389, 0.8660254037844408170 ) ) ;
#11611 = FACE_OUTER_BOUND ( 'NONE', #114076, .T. ) ;
#11613 = CARTESIAN_POINT ( 'NONE',  ( 5.349485151062910226, 1.838858031828109141, -0.09410559872920225277 ) ) ;
#11614 = VERTEX_POINT ( 'NONE', #207764 ) ;
#11615 = CARTESIAN_POINT ( 'NONE',  ( -1.225000000000048050, 2.791666667349440800, -0.7072540797572958171 ) ) ;
#11616 = CARTESIAN_POINT ( 'NONE',  ( -7.507464373665155399, 9.781794407407920389, 1.599625672291295375 ) ) ;
#11617 = CARTESIAN_POINT ( 'NONE',  ( -5.229199737892074420E-15, 0.06250000000001598721, 1.224999999999961009 ) ) ;
#11618 = CARTESIAN_POINT ( 'NONE',  ( 11.35396574786309998, 7.538279440392132713, 3.751616533526511699 ) ) ;
#11619 = CARTESIAN_POINT ( 'NONE',  ( 3.798255590122797898, 7.583048621785260401, -0.7998128361456221525 ) ) ;
#11620 = ADVANCED_FACE ( 'NONE', ( #29031 ), #3673, .T. ) ;
#11621 = CARTESIAN_POINT ( 'NONE',  ( 6.678986887005352813, -0.09631167155637165855, -2.058642716137318640 ) ) ;
#11624 = CARTESIAN_POINT ( 'NONE',  ( 3.772867777003403589, 1.732451475078290448, -0.6238847238279123797 ) ) ;
#11623 = CARTESIAN_POINT ( 'NONE',  ( 2.084208510888691190, 1.074786400414856624, -1.519112143004421434 ) ) ;
#11622 = FILL_AREA_STYLE_COLOUR ( '', #100701 ) ;
#11625 = CARTESIAN_POINT ( 'NONE',  ( 7.145310649601935182, 8.294949498412453437, -1.199719254218446718 ) ) ;
#11626 = CARTESIAN_POINT ( 'NONE',  ( -4.911920813620073822, 4.715216669348689216, 0.3991582675463816177 ) ) ;
#11627 = AXIS2_PLACEMENT_3D ( 'NONE', #57571, #123729, #41342 ) ;
#11628 = CARTESIAN_POINT ( 'NONE',  ( -5.932574734431526942, 9.079031735882207244, 1.199719254218454489 ) ) ;
#11630 = ORIENTED_EDGE ( 'NONE', *, *, #5161, .T. ) ;
#11629 = FACE_OUTER_BOUND ( 'NONE', #2552, .T. ) ;
#11631 = STYLED_ITEM ( 'NONE', ( #120690 ), #56751 ) ;
#11632 = CARTESIAN_POINT ( 'NONE',  ( 3.616033620774202983, -2.174319932014677548, 0.3768175846284789743 ) ) ;
#11633 = CARTESIAN_POINT ( 'NONE',  ( 6.292268727954291485, -2.250598158220047385, -0.2311834041341890578 ) ) ;
#11634 = CARTESIAN_POINT ( 'NONE',  ( -6.290620087060847965, 7.401773525401500464, 1.082531754730549967 ) ) ;
#11635 = CARTESIAN_POINT ( 'NONE',  ( 6.152603492317154199, 1.793228361101945056, 0.2563216274220745938 ) ) ;
#11636 = CARTESIAN_POINT ( 'NONE',  ( 0.02267320670834571672, 0.3494893071277604402, 1.985867805234131644 ) ) ;
#11637 = EDGE_CURVE ( 'NONE', #69998, #31219, #69047, .T. ) ;
#11638 = CARTESIAN_POINT ( 'NONE',  ( -4.498292041426138255, 5.425847295072050436, 1.271850428444160963 ) ) ;
#11639 = CARTESIAN_POINT ( 'NONE',  ( 6.438356904408193415, 1.850619875698428674, 0.2722718653145329015 ) ) ;
#11640 = EDGE_CURVE ( 'NONE', #105851, #112521, #34587, .T. ) ;
#11641 = CARTESIAN_POINT ( 'NONE',  ( 5.109976026518994630, -0.6845719981980763480, 1.785733525123212928 ) ) ;
#11642 = CARTESIAN_POINT ( 'NONE',  ( 11.41267819554179042, 3.499999999999989342, -3.708203932499494648 ) ) ;
#11643 = CARTESIAN_POINT ( 'NONE',  ( 0.8306673739700667358, 0.1335802410974036292, 1.865940672528036304 ) ) ;
#11644 = CARTESIAN_POINT ( 'NONE',  ( 1.235564962061060257, 0.5807501988173838781, -1.931125984888550473 ) ) ;
#11646 = CARTESIAN_POINT ( 'NONE',  ( 4.547555978022395529, -1.627529793438415417, -1.336665591334128100 ) ) ;
#11645 = CARTESIAN_POINT ( 'NONE',  ( -9.504429378379839477, 11.04725468198666150, 1.199719254218462483 ) ) ;
#11647 = CARTESIAN_POINT ( 'NONE',  ( 9.271078113646423091, 9.710679308875986848, 1.040834085586084257E-14 ) ) ;
#11649 = CARTESIAN_POINT ( 'NONE',  ( -7.343712760096452463, 11.71941532008788833, -0.7998128361456291469 ) ) ;
#11648 = CARTESIAN_POINT ( 'NONE',  ( 0.7499999999999867883, -0.4333333333333133641, -1.299038105676652899 ) ) ;
#11650 = CARTESIAN_POINT ( 'NONE',  ( 11.41381676900476805, 10.06958039977608088, 3.704697931490188889 ) ) ;
#11651 = CARTESIAN_POINT ( 'NONE',  ( 2.900653795123844692, -1.990604234199357281, -0.3410580241900613707 ) ) ;
#11652 = CARTESIAN_POINT ( 'NONE',  ( -1.364683531250012516, 3.280208333674756727, 0.7879004041258379498 ) ) ;
#11653 = CARTESIAN_POINT ( 'NONE',  ( 4.304877467538922531, 4.981110786005563007, 1.199719254218464037 ) ) ;
#11654 = CARTESIAN_POINT ( 'NONE',  ( 3.620547430246877862, 1.374377816306590727, -1.668374205817772182 ) ) ;
#11655 = CARTESIAN_POINT ( 'NONE',  ( 11.28709712336965332, 1.000000000000000888, -3.871943585350003048 ) ) ;
#11656 = CARTESIAN_POINT ( 'NONE',  ( 0.7499999999999920064, 5.233333333333353821, 1.299038105676669330 ) ) ;
#11658 = CARTESIAN_POINT ( 'NONE',  ( -9.490381562237910629, -9.037089468803426229, 0.4325416218483088548 ) ) ;
#11657 = CARTESIAN_POINT ( 'NONE',  ( 7.991605200612358573, 8.288237253661408843, 0.7998128361456281477 ) ) ;
#11659 = CARTESIAN_POINT ( 'NONE',  ( 9.042925270190632858, 10.61279623905300085, 1.082531754730549967 ) ) ;
#11661 = CARTESIAN_POINT ( 'NONE',  ( 8.386878554176760758, 15.11743023405602848, -8.584041405059041452 ) ) ;
#11660 = CARTESIAN_POINT ( 'NONE',  ( 0.4323793472312524311, 1.250547990301904111, 1.774695861279996567 ) ) ;
#11662 = CARTESIAN_POINT ( 'NONE',  ( -5.409340102172518705, 9.254721185935849803, 0.000000000000000000 ) ) ;
#11663 = CARTESIAN_POINT ( 'NONE',  ( -0.6823417656250003738, 1.967708333674753174, -1.181850606188749264 ) ) ;
#11664 = CARTESIAN_POINT ( 'NONE',  ( 1.593588134247824639, -0.7342643958434189599, 2.065040727587868830 ) ) ;
#11665 = DIRECTION ( 'NONE',  ( 0.000000000000000000, 1.000000000000000000, 0.000000000000000000 ) ) ;
#11666 = CARTESIAN_POINT ( 'NONE',  ( 2.360583983009652442, 0.9673915393220763326, 2.045390427905840358 ) ) ;
#11667 = CARTESIAN_POINT ( 'NONE',  ( -6.989391883044787868, 8.113044270762433285, -1.199719254218446718 ) ) ;
#11668 = CARTESIAN_POINT ( 'NONE',  ( -1.201851678989727383E-14, 4.134375000341417028, 1.575800808251672791 ) ) ;
#11669 = CARTESIAN_POINT ( 'NONE',  ( 4.978641999450219124, 7.938775605734648799, 1.052364473307040305 ) ) ;
#11670 = CARTESIAN_POINT ( 'NONE',  ( -1.500000000000008216, 12.49999999999999645, 3.469446951953614189E-15 ) ) ;
#11671 = CARTESIAN_POINT ( 'NONE',  ( 6.048345925472183637, 8.149765894507963182, 1.443375672974065660 ) ) ;
#11672 = CARTESIAN_POINT ( 'NONE',  ( 4.622157715239192832, 1.089468934077148399, -1.394508319181851697 ) ) ;
#11673 = CARTESIAN_POINT ( 'NONE',  ( 8.880754312151170282, 10.31963377138658089, 1.199719254218453823 ) ) ;
#11674 = CARTESIAN_POINT ( 'NONE',  ( 0.9386647947689167326, 2.074798300807283447, 0.3599966696490787266 ) ) ;
#11676 = CARTESIAN_POINT ( 'NONE',  ( 1.499999999999985123, 0.5458333333333577064, -0.8660254037844253849 ) ) ;
#11675 = CARTESIAN_POINT ( 'NONE',  ( -1.402160292154681736E-14, 9.421875000341398021, 1.575800808251682339 ) ) ;
#11677 = CARTESIAN_POINT ( 'NONE',  ( -5.632486471834530661, 5.535932070087196344, -0.7998128361456362523 ) ) ;
#11678 = CARTESIAN_POINT ( 'NONE',  ( 6.450795914701256351, -1.844717532910484570, -0.8146137538835170888 ) ) ;
#11680 = ORIENTED_EDGE ( 'NONE', *, *, #196609, .F. ) ;
#11679 = CARTESIAN_POINT ( 'NONE',  ( 4.992358684838777982, -0.9999893916136384231, 1.510367140083505699 ) ) ;
#11681 = CARTESIAN_POINT ( 'NONE',  ( 9.911173986789782120, 11.52179005846497972, -1.199719254218440723 ) ) ;
#11682 = CARTESIAN_POINT ( 'NONE',  ( 3.555401268124198655, 0.4554524271490404952, -1.814226883376020671 ) ) ;
#11683 = CARTESIAN_POINT ( 'NONE',  ( 4.346580092118113470, -2.046995731385771400, -0.3088174131898810959 ) ) ;
#11684 = AXIS2_PLACEMENT_3D ( 'NONE', #22954, #191862, #43523 ) ;
#11685 = CARTESIAN_POINT ( 'NONE',  ( -6.143253000323532831, 7.300121600866474658, 1.082531754730548412 ) ) ;
#11686 = CARTESIAN_POINT ( 'NONE',  ( 7.727257484784855635, 11.10255193463598111, -1.199719254218446718 ) ) ;
#11687 = CARTESIAN_POINT ( 'NONE',  ( -1.538487831126141625, 8.695753106490483830, 2.511613306591230721 ) ) ;
#11688 = CARTESIAN_POINT ( 'NONE',  ( 7.856023664475727308, 8.130058794835305136, -0.7998128361456341429 ) ) ;
#11689 = MECHANICAL_DESIGN_GEOMETRIC_PRESENTATION_REPRESENTATION (  '', ( #60243 ), #42963 ) ;
#11690 = CARTESIAN_POINT ( 'NONE',  ( 5.063152511717405879, 4.908155404373435005, -0.2552525419090029835 ) ) ;
#11691 = CARTESIAN_POINT ( 'NONE',  ( -1.001543065824772872E-14, 5.384375000341415252, 1.575800808251672791 ) ) ;
#11692 = CARTESIAN_POINT ( 'NONE',  ( 3.543363863352413823, 1.774678991803163575, -0.8365776047038612218 ) ) ;
#11693 = CARTESIAN_POINT ( 'NONE',  ( 0.6497672626537411844, -0.2439889887937417567, -2.001205234435726066 ) ) ;
#11694 = EDGE_CURVE ( 'NONE', #146105, #41517, #124877, .T. ) ;
#11695 = CARTESIAN_POINT ( 'NONE',  ( -3.688700311369816909, 6.461178242310183784, -1.199719254218450271 ) ) ;
#11697 = CARTESIAN_POINT ( 'NONE',  ( 7.800371912476624203, -5.581885079358428925, 7.755938900619411491 ) ) ;
#11696 = CARTESIAN_POINT ( 'NONE',  ( 8.503988664269582998, 10.94440607977979063, 1.599625672291281386 ) ) ;
#11698 = CARTESIAN_POINT ( 'NONE',  ( 1.176777557245082262, -0.04011917365428705612, -1.870279424122413658 ) ) ;
#11699 = CARTESIAN_POINT ( 'NONE',  ( -1.364683531250012516, 3.530208333674758059, 0.7879004041258379498 ) ) ;
#11700 = CARTESIAN_POINT ( 'NONE',  ( 2.812746579430201788, -0.5882912493809470122, -1.925304731621484633 ) ) ;
#11702 = CARTESIAN_POINT ( 'NONE',  ( 2.495853057047519030, -2.093741659442478920, 0.3138373457529738397 ) ) ;
#11701 = CARTESIAN_POINT ( 'NONE',  ( -5.246642258808529746, 9.064907035344523578, 0.000000000000000000 ) ) ;
#11703 = FACE_OUTER_BOUND ( 'NONE', #195943, .T. ) ;
#11704 = CARTESIAN_POINT ( 'NONE',  ( 3.754400092289136737, -2.067862582909282487, -0.1045053291982081939 ) ) ;
#11705 = CARTESIAN_POINT ( 'NONE',  ( 4.934241560730721510, 4.721313007132757811, 0.000000000000000000 ) ) ;
#11707 = CARTESIAN_POINT ( 'NONE',  ( 3.460355519985863548, 5.060167411448709629, 1.599625672291267398 ) ) ;
#11706 = CARTESIAN_POINT ( 'NONE',  ( 0.3805629577237649719, -0.2597898305938106112, -2.074488238918821725 ) ) ;
#11709 = ORIENTED_EDGE ( 'NONE', *, *, #108573, .T. ) ;
#11708 = CARTESIAN_POINT ( 'NONE',  ( 5.666980381186065507, -1.651371415153819688, -0.7785968546244539379 ) ) ;
#11710 = CARTESIAN_POINT ( 'NONE',  ( 9.185812768458653466, 10.67553530374532045, 1.199719254218453823 ) ) ;
#11711 = CARTESIAN_POINT ( 'NONE',  ( 6.511106444361000278, 5.279176164185798825, -2.499999999999995559 ) ) ;
#11712 = CARTESIAN_POINT ( 'NONE',  ( 9.962237412473150755, 12.35880645891234408, 7.801823201411741238 ) ) ;
#11713 = CARTESIAN_POINT ( 'NONE',  ( 6.422910180798067969, 2.056742032306459578, 0.8002587082300142152 ) ) ;
#11714 = CARTESIAN_POINT ( 'NONE',  ( -1.364683531250010740, 11.69270833367473017, 0.7879004041258445001 ) ) ;
#11715 = CARTESIAN_POINT ( 'NONE',  ( 4.899028947338643469, -0.2378672112019977747, -1.897373119303269018 ) ) ;
#11716 = CARTESIAN_POINT ( 'NONE',  ( -8.670602931139386627, 10.07445716020612103, 1.199719254218462483 ) ) ;
#11717 = CARTESIAN_POINT ( 'NONE',  ( 6.657217119509961201, 7.725507046638470321, -1.199719254218446718 ) ) ;
#11718 = CARTESIAN_POINT ( 'NONE',  ( 0.6801582343749883464, 2.588541667008101399, -1.178068619123865846 ) ) ;
#11719 = CARTESIAN_POINT ( 'NONE',  ( -3.752568318859959007, 7.355240624044412812, 0.6449737300090957470 ) ) ;
#11720 = CARTESIAN_POINT ( 'NONE',  ( 3.659811400685081040, 6.357198169852855685, -1.199719254218446718 ) ) ;
#11721 = ORIENTED_EDGE ( 'NONE', *, *, #154961, .T. ) ;
#11722 = DIRECTION ( 'NONE',  ( 0.000000000000000000, -1.000000000000000000, 0.000000000000000000 ) ) ;
#11723 = CARTESIAN_POINT ( 'NONE',  ( -0.02299388927988389730, 0.001624902753813092359, -1.910968047046639251 ) ) ;
#11724 = CARTESIAN_POINT ( 'NONE',  ( 5.508355548902068577, 9.648441583686274470, 0.7998128361456331437 ) ) ;
#11725 = CARTESIAN_POINT ( 'NONE',  ( -7.019253602638862333, -7.126685749119995528, 7.019253602638880984 ) ) ;
#11726 = CARTESIAN_POINT ( 'NONE',  ( -5.584154938098890852, 7.410262610144577877, 1.243513269814926492 ) ) ;
#11727 = CARTESIAN_POINT ( 'NONE',  ( -5.083944415444539899, 8.875092884753202682, 0.000000000000000000 ) ) ;
#11728 = CARTESIAN_POINT ( 'NONE',  ( 2.822068529938852155, 6.444163718237301275, -0.7998128361456291469 ) ) ;
#11729 = CARTESIAN_POINT ( 'NONE',  ( 2.746873616242023086, -0.3318220265390697254, -1.941108330032844664 ) ) ;
#11730 = CARTESIAN_POINT ( 'NONE',  ( 3.058220425488000327, -1.198843740453523266, 1.621196181159669347 ) ) ;
#11731 = CARTESIAN_POINT ( 'NONE',  ( -8.369460898337653276, 8.658792557682392754, 0.7998128361456462443 ) ) ;
#11732 = CARTESIAN_POINT ( 'NONE',  ( 5.611095471209277541, 7.639640364534566075, 1.599625672291268286 ) ) ;
#11734 = EDGE_CURVE ( 'NONE', #18521, #148587, #190134, .T. ) ;
#11733 = CARTESIAN_POINT ( 'NONE',  ( 6.827182134110192813, 7.051736335826703339, 2.787205296604370108 ) ) ;
#11735 = CARTESIAN_POINT ( 'NONE',  ( 3.978626637211603700, -0.2140425413966473567, -2.180973779111646138 ) ) ;
#11736 = DIRECTION ( 'NONE',  ( 1.000000000000000000, 0.000000000000000000, 0.000000000000000000 ) ) ;
#11737 = CARTESIAN_POINT ( 'NONE',  ( 1.641497204607924809, -1.393575563620005786, -1.330239063421148948 ) ) ;
#11738 = CARTESIAN_POINT ( 'NONE',  ( -9.809487834687324437, 11.40315621434539395, 1.199719254218462483 ) ) ;
#11739 = CARTESIAN_POINT ( 'NONE',  ( 0.1331565106231328566, 1.371277436080810208, -2.201942895618694607 ) ) ;
#11740 = EDGE_CURVE ( 'NONE', #76194, #55540, #76041, .T. ) ;
#11741 = CARTESIAN_POINT ( 'NONE',  ( 5.234856708652235291, 5.279956712948652431, 0.7216878364870338292 ) ) ;
#11742 = CARTESIAN_POINT ( 'NONE',  ( 8.959240580532112475, 9.346868853575953651, -0.7998128361456221525 ) ) ;
#11743 = CARTESIAN_POINT ( 'NONE',  ( -6.980013479859874082, -8.233136965322266576, 6.444907381559366932 ) ) ;
#11744 = CARTESIAN_POINT ( 'NONE',  ( 4.245111494854632461, 7.966730820723463502, 0.000000000000000000 ) ) ;
#11745 = VERTEX_POINT ( 'NONE', #158635 ) ;
#11747 = CARTESIAN_POINT ( 'NONE',  ( 1.541653539051958122, -1.894817064119158401, 0.6801782934461576557 ) ) ;
#11746 = CARTESIAN_POINT ( 'NONE',  ( 6.075717905342373548, -0.9791751913862613010, 1.559117742379905858 ) ) ;
#11748 = CARTESIAN_POINT ( 'NONE',  ( 4.780793123113402210, -2.255322609370190357, 0.4421783396322577775 ) ) ;
#11750 = CARTESIAN_POINT ( 'NONE',  ( 2.061162768541408230, 1.543764177570670970, 1.038864413082870142 ) ) ;
#11749 = CARTESIAN_POINT ( 'NONE',  ( -0.02919842301644676522, 2.866066704180502800, -2.562138095921069780 ) ) ;
#11752 = CARTESIAN_POINT ( 'NONE',  ( -3.285556943750000070, -1.509374999522042238, 0.000000000000000000 ) ) ;
#11751 = APPLICATION_CONTEXT ( 'automotive_design' ) ;
#11753 = CARTESIAN_POINT ( 'NONE',  ( -0.1290005225502432740, 4.081813041011835175, -2.728655865233818201 ) ) ;
#11754 = CARTESIAN_POINT ( 'NONE',  ( 5.150612376422202487, 1.885107930906554152, 0.3209214958604587054 ) ) ;
#11755 = CARTESIAN_POINT ( 'NONE',  ( -8.843996274815957293, 9.212417163573759282, 1.040834085586084257E-14 ) ) ;
#11756 = CARTESIAN_POINT ( 'NONE',  ( -5.153507786970275006, 7.105788066255672497, -1.443375672974066548 ) ) ;
#11758 = CARTESIAN_POINT ( 'NONE',  ( 3.485083742438867649, 1.691615344724434200, -0.7988839237506044633 ) ) ;
#11757 = CARTESIAN_POINT ( 'NONE',  ( 4.476172314981810452, -2.028359691925533781, -0.5064535023821553628 ) ) ;
#11759 = CARTESIAN_POINT ( 'NONE',  ( 5.938108093105483931, 8.911247961056314892, -1.082531754730537088 ) ) ;
#11760 = VERTEX_POINT ( 'NONE', #123031 ) ;
#11761 = CARTESIAN_POINT ( 'NONE',  ( -1.451998047846444262, 7.315968950355187239, 4.301760722574934803 ) ) ;
#11762 = CARTESIAN_POINT ( 'NONE',  ( 4.572363442555127833, 8.499999999999996447, 0.3169179603640607246 ) ) ;
#11763 = CARTESIAN_POINT ( 'NONE',  ( 6.639270748794153576, -1.536914537172892725, 0.7831451356504478545 ) ) ;
#11764 = CARTESIAN_POINT ( 'NONE',  ( -5.656776405399756236, 7.622658444431597680, -1.599625672291256295 ) ) ;
#11765 = CARTESIAN_POINT ( 'NONE',  ( 1.476802972400652170, -1.725769044224190196, -0.1698483453264828802 ) ) ;
#11766 = CARTESIAN_POINT ( 'NONE',  ( -5.972841284750454172, 14.55272318667275933, 10.36653721697756936 ) ) ;
#11767 =( LENGTH_UNIT ( ) NAMED_UNIT ( * ) SI_UNIT ( .MILLI., .METRE. ) );
#11768 = CARTESIAN_POINT ( 'NONE',  ( 0.000000000000000000, 8.500000000000000000, 0.000000000000000000 ) ) ;
#11769 = CARTESIAN_POINT ( 'NONE',  ( 6.332918745153389928, -2.058942774313234025, -0.6888473222384088324 ) ) ;
#11770 = CARTESIAN_POINT ( 'NONE',  ( 4.723181480036696023, -0.08661695748878039947, 1.823760500460340550 ) ) ;
#11771 = CARTESIAN_POINT ( 'NONE',  ( 1.867943658074404434, -1.947550630801861526, 0.2349073745619503772 ) ) ;
#11772 = CARTESIAN_POINT ( 'NONE',  ( 6.403513597085680686, -2.053302684608013795, 0.5162988180226235624 ) ) ;
#11773 = FILL_AREA_STYLE ('',( #124564 ) ) ;
#11774 = CARTESIAN_POINT ( 'NONE',  ( 0.7499999999999902300, 5.566666666666685082, -1.299038105676658228 ) ) ;
#11775 = CARTESIAN_POINT ( 'NONE',  ( 9.101601193475611140, 9.512956235343358102, -0.7998128361456221525 ) ) ;
#11776 = CARTESIAN_POINT ( 'NONE',  ( 2.930460433956377564, -1.047063434655249647, -1.843881786051679850 ) ) ;
#11777 = CARTESIAN_POINT ( 'NONE',  ( -4.284013352238262407, 6.021101549076499637, -1.443375672974053447 ) ) ;
#11778 = CARTESIAN_POINT ( 'NONE',  ( -11.18654035131441127, 1.000000000000000888, 4.041720556560751021 ) ) ;
#11779 = ADVANCED_FACE ( 'NONE', ( #43834 ), #76307, .T. ) ;
#11780 = CARTESIAN_POINT ( 'NONE',  ( -5.157125652413038885, 6.495829312680758250, -1.199528311315662510 ) ) ;
#11781 = CARTESIAN_POINT ( 'NONE',  ( 0.3212534483023680165, -1.847719145540312358, -0.9339786784923131968 ) ) ;
#11783 = CARTESIAN_POINT ( 'NONE',  ( 0.7500000000000006661, 13.94791666734946567, -1.299038105676657340 ) ) ;
#11782 = CARTESIAN_POINT ( 'NONE',  ( -10.98241130803290488, 3.975933801733734896, 3.568401746110938966 ) ) ;
#11785 = VERTEX_POINT ( 'NONE', #9171 ) ;
#11784 = CARTESIAN_POINT ( 'NONE',  ( 3.826986476844072005, 1.570263387305373737, -1.571374446222243204 ) ) ;
#11786 = CARTESIAN_POINT ( 'NONE',  ( 0.5460333347737976739, -1.659586600764794584, 1.590741637488497062 ) ) ;
#11788 = CARTESIAN_POINT ( 'NONE',  ( 5.928601196466630086, -1.312702821215183002, 1.590880328853358394 ) ) ;
#11787 = CARTESIAN_POINT ( 'NONE',  ( 3.358669367883368118, 4.941533567329135401, -1.599625672291262513 ) ) ;
#11790 = CARTESIAN_POINT ( 'NONE',  ( -3.475000000000000533, -2.479166666666667851, -2.006292185433948827 ) ) ;
#11789 = CARTESIAN_POINT ( 'NONE',  ( 6.215487077222150880, 6.216099443039444949, 0.000000000000000000 ) ) ;
#11791 = CARTESIAN_POINT ( 'NONE',  ( 0.1329588055935396196, 0.2493489391296536684, -1.880683181770840262 ) ) ;
#11792 = CARTESIAN_POINT ( 'NONE',  ( 5.179192671508887180, 1.240781939916297372, 1.360553736468192554 ) ) ;
#11793 = DIRECTION ( 'NONE',  ( -0.6507913734559641616, -0.7592566023653004592, 0.000000000000000000 ) ) ;
#11794 = CARTESIAN_POINT ( 'NONE',  ( 5.054492339796319733, 4.791329239384148231, -0.7998128361456211532 ) ) ;
#11795 = CARTESIAN_POINT ( 'NONE',  ( 2.156250000000001776, -1.895863743164040160, 0.7852924748301010061 ) ) ;
#11796 = CARTESIAN_POINT ( 'NONE',  ( 2.906937612971383089, 1.455985047528246090, 0.9243032718214757582 ) ) ;
#11797 = CARTESIAN_POINT ( 'NONE',  ( 1.024625454658374624, 0.3981145430279106057, 1.976669095394629982 ) ) ;
#11798 = CARTESIAN_POINT ( 'NONE',  ( 2.866213343745026343, -0.1723225051825111875, -2.292302961975992037 ) ) ;
#11799 = CARTESIAN_POINT ( 'NONE',  ( -1.364683531250012516, 3.551041667008086211, -0.7879004041258300672 ) ) ;
#11800 = CARTESIAN_POINT ( 'NONE',  ( 2.249658590878771847, -1.816102774931172448, -1.348951556275684194 ) ) ;
#11801 = CARTESIAN_POINT ( 'NONE',  ( 4.899102953068730670, 1.751457851224359041, -1.169261236274852012 ) ) ;
#11802 = CARTESIAN_POINT ( 'NONE',  ( -7.295696057929500711, 7.684269287105433222, 0.7216878364870317197 ) ) ;
#11803 = CARTESIAN_POINT ( 'NONE',  ( 3.338855477594515175, -1.562335520734370320, 0.8312421073871211208 ) ) ;
#11804 = CARTESIAN_POINT ( 'NONE',  ( 4.449046963578762615, 8.342305224150557308, -0.7998128361456231517 ) ) ;
#11806 = CARTESIAN_POINT ( 'NONE',  ( 6.163675082799745297, 1.174783243402954591, 1.968361872208840069 ) ) ;
#11805 = CARTESIAN_POINT ( 'NONE',  ( 4.163762572728282763, 6.911454530608037494, -1.082531754730548412 ) ) ;
#11807 = CARTESIAN_POINT ( 'NONE',  ( 4.663899394030392997, -1.200468288914667614, 1.396033019000951336 ) ) ;
#11808 = CARTESIAN_POINT ( 'NONE',  ( -5.111587607552082524, 5.922272616020886282, 1.199719254218450271 ) ) ;
#11809 = CARTESIAN_POINT ( 'NONE',  ( 6.114364089638798738, 6.235772314107808079, 0.7216878364870317197 ) ) ;
#11810 = CARTESIAN_POINT ( 'NONE',  ( 0.7499999999999902300, 4.066666666666690411, -1.299038105676658228 ) ) ;
#11811 = CARTESIAN_POINT ( 'NONE',  ( 4.189532503254236318, -0.8396404696654431454, 2.024412170900617092 ) ) ;
#11812 = CARTESIAN_POINT ( 'NONE',  ( -3.815730167242251003, 6.539103397502874948, -1.199719254218452047 ) ) ;
#11813 = CARTESIAN_POINT ( 'NONE',  ( -0.007473969438131279966, 8.279395425053861501, -1.999986034896452436 ) ) ;
#11814 = CARTESIAN_POINT ( 'NONE',  ( 0.000000000000000000, 4.000007913748540922, 1.105031132475055157E-32 ) ) ;
#11815 = CARTESIAN_POINT ( 'NONE',  ( -1.201851678989727383E-14, 4.946875000341420581, -1.575800808251660134 ) ) ;
#11816 = CARTESIAN_POINT ( 'NONE',  ( 2.982943389344643759, -0.1423259158175680661, -1.921303036959535415 ) ) ;
#11817 = CARTESIAN_POINT ( 'NONE',  ( -1.364683531250000748, 8.859375000341396245, 0.000000000000000000 ) ) ;
#11818 = CARTESIAN_POINT ( 'NONE',  ( -2.982430605326321427, 6.423326772948587227, -0.7216878364870267237 ) ) ;
#11819 = CARTESIAN_POINT ( 'NONE',  ( -0.1927127643980519056, -0.4999767001874329542, -2.172835435166208473 ) ) ;
#11820 = EDGE_LOOP ( 'NONE', ( #18910, #197386, #111993, #73215 ) ) ;
#11821 = FACE_OUTER_BOUND ( 'NONE', #53816, .T. ) ;
#11822 = CARTESIAN_POINT ( 'NONE',  ( 5.203632029546647608, 4.965325544092860532, 1.040834085586084257E-14 ) ) ;
#11823 = SURFACE_SIDE_STYLE ('',( #142948 ) ) ;
#11824 = FACE_OUTER_BOUND ( 'NONE', #161814, .T. ) ;
#11825 = CARTESIAN_POINT ( 'NONE',  ( 4.911089278408375947, 4.764320510802636299, 0.1685941148131786249 ) ) ;
#11826 = LINE ( 'NONE', #162373, #194839 ) ;
#11827 = CARTESIAN_POINT ( 'NONE',  ( -1.201851678989727383E-14, 1.884375000341422135, 1.575800808251672791 ) ) ;
#11828 = CARTESIAN_POINT ( 'NONE',  ( 6.403215362905616992, 1.794359850238020693, 1.205212418099836480 ) ) ;
#11829 =( GEOMETRIC_REPRESENTATION_CONTEXT ( 3 ) GLOBAL_UNCERTAINTY_ASSIGNED_CONTEXT ( ( #204976 ) ) GLOBAL_UNIT_ASSIGNED_CONTEXT ( ( #111538, #61654, #146131 ) ) REPRESENTATION_CONTEXT ( 'NONE', 'WORKASPACE' ) );
#11830 = CARTESIAN_POINT ( 'NONE',  ( 5.934033239752055877, 1.167398200610193282, 1.576599764842034457 ) ) ;
#11831 = CARTESIAN_POINT ( 'NONE',  ( -8.136864746495904299, 12.64475930422059768, -0.7998128361456281477 ) ) ;
#11832 = CARTESIAN_POINT ( 'NONE',  ( -4.053524740361572398, 7.672936597156388316, 0.7216878364870317197 ) ) ;
#11833 = CARTESIAN_POINT ( 'NONE',  ( 5.805597153138060129, -0.5296426447994294628, 2.095691122003799478 ) ) ;
#11835 = VERTEX_POINT ( 'NONE', #209484 ) ;
#11834 = DIRECTION ( 'NONE',  ( 0.000000000000000000, 1.000000000000000000, 0.000000000000000000 ) ) ;
#11836 = CARTESIAN_POINT ( 'NONE',  ( 0.6823417656249917140, 3.842708333674754506, 1.181850606188765695 ) ) ;
#11837 = CARTESIAN_POINT ( 'NONE',  ( 0.5263522483448194178, 1.788089326329355577, 0.5492086291003297482 ) ) ;
#11838 = CARTESIAN_POINT ( 'NONE',  ( 5.975915019019427454, 1.530855338724030457, 0.8140783706773281336 ) ) ;
#11839 = AXIS2_PLACEMENT_3D ( 'NONE', #150815, #54373, #120511 ) ;
#11841 = CARTESIAN_POINT ( 'NONE',  ( 3.140350738262797314, 0.5347024899306859202, 2.125194831261326911 ) ) ;
#11840 = CARTESIAN_POINT ( 'NONE',  ( 0.6801582343750038895, 0.3072916670080680368, -1.178068619123848526 ) ) ;
#11842 = CARTESIAN_POINT ( 'NONE',  ( 2.942713080207468579, 2.290027058972336604, 0.2837140972290051466 ) ) ;
#11843 = CARTESIAN_POINT ( 'NONE',  ( 5.395800779767854216, -0.7457615368846971515, 1.921284171288279996 ) ) ;
#11844 = CARTESIAN_POINT ( 'NONE',  ( 1.271315641948435493, 1.156325127695263744, 1.560008962195078563 ) ) ;
#11845 = CARTESIAN_POINT ( 'NONE',  ( -6.710922848640111127, 6.931757532942661726, 0.7216878364870317197 ) ) ;
#11846 = CARTESIAN_POINT ( 'NONE',  ( -3.492107083971660586, 6.231819477012331632, 1.199719254218452935 ) ) ;
#11847 = CARTESIAN_POINT ( 'NONE',  ( -2.193105066167322370, 5.702484939155337607, -2.500000000000000444 ) ) ;
#11848 = CARTESIAN_POINT ( 'NONE',  ( 4.957343421279006179, -1.817532610912236724, 1.092287347377165485 ) ) ;
#11849 = DIRECTION ( 'NONE',  ( 0.000000000000000000, -1.000000000000000000, 0.000000000000000000 ) ) ;
#11850 = CARTESIAN_POINT ( 'NONE',  ( 2.443982611291168450, -1.755769474653746665, -0.9913988478210812305 ) ) ;
#11851 = CARTESIAN_POINT ( 'NONE',  ( -6.222829318548141586, 6.362315081168691044, 0.7216878364870317197 ) ) ;
#11852 = CARTESIAN_POINT ( 'NONE',  ( 6.018643902988223715, 1.486383190695803158, -1.631276885294789203 ) ) ;
#11853 = CARTESIAN_POINT ( 'NONE',  ( -5.643072231634639557, 5.548282123187322945, -0.1753453157342581004 ) ) ;
#11854 = CARTESIAN_POINT ( 'NONE',  ( 0.4041367621137400001, 3.038026290190015022, -0.4210133165200654615 ) ) ;
#11855 = PLANE ( 'NONE',  #28189 ) ;
#11856 = CARTESIAN_POINT ( 'NONE',  ( -6.912678218121246942, 9.158153569265168770, 1.599625672291269396 ) ) ;
#11858 = CARTESIAN_POINT ( 'NONE',  ( -5.608633734226008194, 5.643391804966442216, 0.4859901473732997079 ) ) ;
#11857 = CARTESIAN_POINT ( 'NONE',  ( -4.866517195131829787, 8.171732932056599452, 0.9908671576431731243 ) ) ;
#11859 = CARTESIAN_POINT ( 'NONE',  ( -10.19097401674926395, 4.476076320095182304, 5.708917106338025960 ) ) ;
#11860 = ORIENTED_EDGE ( 'NONE', *, *, #78658, .T. ) ;
#11861 = CARTESIAN_POINT ( 'NONE',  ( 3.907146709503729110, 1.766719954806586612, 1.060879741047163316 ) ) ;
#11862 = CARTESIAN_POINT ( 'NONE',  ( -8.041394506236766659, 8.554250810130591631, -0.7216878364870338292 ) ) ;
#11863 = UNCERTAINTY_MEASURE_WITH_UNIT (LENGTH_MEASURE( 1.000000000000000082E-05 ), #8814, 'distance_accuracy_value', 'NONE');
#11864 = CARTESIAN_POINT ( 'NONE',  ( 0.03436587256740384483, -7.792803924024841677, 9.554207839743742881 ) ) ;
#11865 = CARTESIAN_POINT ( 'NONE',  ( -5.148345644887285744, 7.029489223833707001, -1.599625672291256295 ) ) ;
#11866 = CARTESIAN_POINT ( 'NONE',  ( -5.958368452836739770, 6.108636665014236300, 0.7718718275001738016 ) ) ;
#11867 = CARTESIAN_POINT ( 'NONE',  ( 4.406902263202909786, -0.4446603063312704607, -1.969940172527106625 ) ) ;
#11868 = CARTESIAN_POINT ( 'NONE',  ( 1.499999999999987121, 0.7958333333333510451, -0.8660254037844253849 ) ) ;
#11870 = CARTESIAN_POINT ( 'NONE',  ( 9.761507412159302177, 10.49077285704843199, -0.7216878364870257245 ) ) ;
#11869 = CARTESIAN_POINT ( 'NONE',  ( -4.950662367645459305, 5.804802846121667415, -1.199719254218453823 ) ) ;
#11871 = CARTESIAN_POINT ( 'NONE',  ( 5.960781091502512119, 10.10599504006161986, 0.7998128361456462443 ) ) ;
#11872 = CARTESIAN_POINT ( 'NONE',  ( 2.764585236803930979, -1.422233405468891210, 1.491712647946776826 ) ) ;
#11873 = CARTESIAN_POINT ( 'NONE',  ( 2.848279904836711118, 0.2930702634792031747, -1.994869876753922799 ) ) ;
#11874 = ORIENTED_EDGE ( 'NONE', *, *, #110186, .F. ) ;
#11875 =( BOUNDED_SURFACE ( )  B_SPLINE_SURFACE ( 3, 2, ( 
 ( #892, #180740, #181790 ),
 ( #194858, #16082, #64852 ),
 ( #95256, #148259, #66959 ),
 ( #130999, #114742, #48626 ) ),
 .UNSPECIFIED., .F., .F., .F. ) 
 B_SPLINE_SURFACE_WITH_KNOTS ( ( 4, 4 ),
 ( 3, 3 ),
 ( 1.570796326794896558, 2.636531018672050752 ),
 ( 0.000000000000000000, 1.000000000000000000 ),
 .UNSPECIFIED. ) 
 GEOMETRIC_REPRESENTATION_ITEM ( )  RATIONAL_B_SPLINE_SURFACE ( (
 ( 1.000000000000000000, 0.7071067811865960895, 1.000000000000000000),
 ( 1.000000000000000000, 0.8161930835858371980, 1.000000000000000000),
 ( 1.000000000000000000, 0.8980788380693774942, 1.000000000000000000),
 ( 1.000000000000000000, 0.9374448844494288613, 1.000000000000000000) ) ) 
 REPRESENTATION_ITEM ( '' )  SURFACE ( )  );
#11876 = FACE_OUTER_BOUND ( 'NONE', #59289, .T. ) ;
#11877 = CARTESIAN_POINT ( 'NONE',  ( 5.705283713252285338, 5.550585841749444249, -0.7998128361456211532 ) ) ;
#11879 = VERTEX_POINT ( 'NONE', #172756 ) ;
#11878 = CARTESIAN_POINT ( 'NONE',  ( -0.5528008270655216938, 7.812676398891195362, -1.922238454054859824 ) ) ;
#11880 = CARTESIAN_POINT ( 'NONE',  ( 2.987657498945671897, 1.897406709466815444, 0.6818930838706839248 ) ) ;
#11881 = CARTESIAN_POINT ( 'NONE',  ( 2.993917163610838816, -0.5349900852187582379, -1.761688665035024304 ) ) ;
#11882 = CARTESIAN_POINT ( 'NONE',  ( 0.6984242042700332664, -0.8252692633385866339, 2.155259511649917137 ) ) ;
#11883 = CARTESIAN_POINT ( 'NONE',  ( 5.923986774528332333, 5.876015756563318426, -0.7998128361456481317 ) ) ;
#11884 = CARTESIAN_POINT ( 'NONE',  ( 2.917419293707240069, -0.2150262876145451196, 2.150894318904146729 ) ) ;
#11885 = CARTESIAN_POINT ( 'NONE',  ( -4.889686956022917919, 8.856385215335397021, 1.214306433183764966E-14 ) ) ;
#11886 = EDGE_CURVE ( 'NONE', #122450, #88429, #25414, .T. ) ;
#11887 = CARTESIAN_POINT ( 'NONE',  ( 2.671599042396528123, -0.8780164823973014565, -2.124237947079451683 ) ) ;
#11888 = ORIENTED_EDGE ( 'NONE', *, *, #167055, .T. ) ;
#11889 = CARTESIAN_POINT ( 'NONE',  ( -9.000007961041697868, 1.000000000000000888, -7.937244906211844864 ) ) ;
#11890 = CARTESIAN_POINT ( 'NONE',  ( 1.779943879855113709, -1.003247456797161652, 1.578688272967261996 ) ) ;
#11891 = CARTESIAN_POINT ( 'NONE',  ( 5.506699291815658093, 1.493407355681115378, -1.287129089984188290 ) ) ;
#11892 = AXIS2_PLACEMENT_3D ( 'NONE', #211954, #199964, #198888 ) ;
#11894 = CARTESIAN_POINT ( 'NONE',  ( 8.934460041281305109, 10.48625347199211966, -1.082531754730543083 ) ) ;
#11893 = CARTESIAN_POINT ( 'NONE',  ( 1.364683531249988535, 3.863541667008087543, 0.7879004041258500513 ) ) ;
#11896 = CARTESIAN_POINT ( 'NONE',  ( 0.2412292383832773390, 0.3817025157030576321, 2.173470055567463088 ) ) ;
#11895 = CARTESIAN_POINT ( 'NONE',  ( -5.551173829791513192, 8.563787670477010394, 1.199719254218452047 ) ) ;
#11897 = CARTESIAN_POINT ( 'NONE',  ( 6.865700769154306826, -0.4580177224273937475, 2.026514595051785772 ) ) ;
#11898 = CARTESIAN_POINT ( 'NONE',  ( 6.307567778855705853, 8.381915046796901692, -1.599625672291262513 ) ) ;
#11899 = CARTESIAN_POINT ( 'NONE',  ( -4.466521540698216164, 7.298359999868178960, -1.199719254218452047 ) ) ;
#11900 = CARTESIAN_POINT ( 'NONE',  ( 6.639320575229294086, 2.013432609116216021, 2.506292271646192393 ) ) ;
#11901 = CARTESIAN_POINT ( 'NONE',  ( 4.522318884118472049, 1.213545612936163032, -1.553610194691892765 ) ) ;
#11902 = CARTESIAN_POINT ( 'NONE',  ( -0.06985027309261250539, -2.078401542846250116, 0.4200961532789050379 ) ) ;
#11903 = CARTESIAN_POINT ( 'NONE',  ( 1.499999999999987121, 0.2854166673494805684, 0.8660254037844524744 ) ) ;
#11904 = CARTESIAN_POINT ( 'NONE',  ( 4.776155900897590456, 1.325808183606682622, 1.888659687595494407 ) ) ;
#11905 = TOROIDAL_SURFACE ( 'NONE', #129666, 11.92000000000000171, 0.08000000000000000167 ) ;
#11906 = CARTESIAN_POINT ( 'NONE',  ( 1.692308231870808921, 1.020316376917740575, -1.792489025137546044 ) ) ;
#11907 = CARTESIAN_POINT ( 'NONE',  ( 7.375272376154084597, 9.627570410311676596, -1.443375672974057666 ) ) ;
#11908 = EDGE_CURVE ( 'NONE', #48473, #131174, #111815, .T. ) ;
#11909 = CARTESIAN_POINT ( 'NONE',  ( 5.499767588998890844, 6.445425604367387429, 1.199719254218451159 ) ) ;
#11910 = CARTESIAN_POINT ( 'NONE',  ( 4.760848217054122422, 5.583353003765119560, -1.199719254218452047 ) ) ;
#11911 = CARTESIAN_POINT ( 'NONE',  ( 1.364683531249988535, 2.426041667008088432, 0.7879004041258500513 ) ) ;
#11912 = CARTESIAN_POINT ( 'NONE',  ( 5.239300017038202917, 5.077214539491492928, 0.000000000000000000 ) ) ;
#11913 = CARTESIAN_POINT ( 'NONE',  ( 5.138177029454829459, 8.938364267765221527, 0.7216878364870438212 ) ) ;
#11914 = CARTESIAN_POINT ( 'NONE',  ( 4.018178019744323315, 2.155211776303669335, -0.2622048733134130782 ) ) ;
#11915 = DIRECTION ( 'NONE',  ( 0.000000000000000000, 1.000000000000000000, 0.000000000000000000 ) ) ;
#11917 = CARTESIAN_POINT ( 'NONE',  ( 3.895923546780861724, -0.5813109859279729230, -1.747131793041277970 ) ) ;
#11916 = CARTESIAN_POINT ( 'NONE',  ( -2.982430605326328532, 5.462957558647244305, -1.082531754730543971 ) ) ;
#11919 = CARTESIAN_POINT ( 'NONE',  ( 6.720655732516650716, 2.467238681591706673, 2.210725262702870175 ) ) ;
#11918 = CARTESIAN_POINT ( 'NONE',  ( -1.364683531250010295, 5.530208333674751842, 0.7879004041258379498 ) ) ;
#11920 = CARTESIAN_POINT ( 'NONE',  ( 5.794512526436308875, 1.792401445336734733, -1.260760892635464980 ) ) ;
#11921 = DIRECTION ( 'NONE',  ( -0.9999980456341537316, 0.000000000000000000, -0.001977050295958626257 ) ) ;
#11922 = CARTESIAN_POINT ( 'NONE',  ( 6.350461102289020054, 0.7023508724467423248, 2.150821023316491498 ) ) ;
#11923 = VERTEX_POINT ( 'NONE', #126211 ) ;
#11924 = CARTESIAN_POINT ( 'NONE',  ( -4.338732707277040745, 7.407397761066524922, -1.160996969951762159 ) ) ;
#11925 = CARTESIAN_POINT ( 'NONE',  ( -0.6311622855796981124, 3.199999999999959766, 0.3999999999999542255 ) ) ;
#11926 = CARTESIAN_POINT ( 'NONE',  ( 4.655672573246532941, 8.415299432525721102, 0.4976263304441782553 ) ) ;
#11927 = CARTESIAN_POINT ( 'NONE',  ( -3.960390268523300339, 7.634556056670224855, 1.214306433183764966E-14 ) ) ;
#11928 = CARTESIAN_POINT ( 'NONE',  ( -3.035422819611498735, 6.295728927258597452, 0.6346236910419257304 ) ) ;
#11929 = CARTESIAN_POINT ( 'NONE',  ( 0.7777615046654516862, -0.9880915000441170548, 1.468120464595161989 ) ) ;
#11930 =( BOUNDED_CURVE ( )  B_SPLINE_CURVE ( 2, ( #138777, #188571, #106313, #55377, #172336, #185362, #136642, #23925, #202666, #20718, #54316, #121532, #21770, #39131, #90030, #7672, #139852, #205882, #105214, #173417, #24998, #120454, #87879, #186429, #69468, #53245, #137709, #104137, #170183, #36984, #135573, #71600, #152877, #155015, #171252, #57516, #22847, #123674, #189636, #41287, #107395, #201597, #11947, #209063, #46607, #124733, #194970, #58578, #190692, #59637, #61779, #143069, #96437, #210136, #125795, #94303, #176598, #76944, #108466, #191757, #159270, #174486, #127946, #10870, #126864, #30352, #13006 ),
 .UNSPECIFIED., .F., .T. ) 
 B_SPLINE_CURVE_WITH_KNOTS ( ( 3, 2, 2, 2, 2, 2, 2, 2, 2, 2, 2, 2, 2, 2, 2, 2, 2, 2, 2, 2, 2, 2, 2, 2, 2, 2, 2, 2, 2, 2, 2, 2, 2, 3 ),
 ( 0.1422369605164285622, 0.1458333333333333426, 0.1499999999999999944, 0.1541666666666666741, 0.1583333333333333259, 0.1625000000000000056, 0.1666666666666666574, 0.1708333333333333370, 0.1749999999999999889, 0.1791666666666666685, 0.1833333333333333204, 0.1875000000000000000, 0.1916666666666666796, 0.1958333333333333315, 0.2000000000000000111, 0.2041666666666666630, 0.2083333333333333426, 0.2124999999999999944, 0.2166666666666666741, 0.2208333333333333259, 0.2250000000000000056, 0.2291666666666666574, 0.2333333333333333370, 0.2374999999999999889, 0.2416666666666666685, 0.2458333333333333204, 0.2500000000000000000, 0.2541666666666666519, 0.2583333333333333592, 0.2625000000000000111, 0.2666666666666666630, 0.2708333333333333148, 0.2750000000000000222, 0.2785089426034975113 ),
 .UNSPECIFIED. ) 
 CURVE ( )  GEOMETRIC_REPRESENTATION_ITEM ( )  RATIONAL_B_SPLINE_CURVE ( ( 0.9683452906431839757, 0.8843625769634950728, 1.000000000000000000, 0.8660254037844387076, 1.000000000000000000, 0.8660254037844387076, 1.000000000000000000, 0.8660254037844387076, 1.000000000000000000, 0.8660254037844387076, 1.000000000000000000, 0.8660254037844387076, 1.000000000000000000, 0.8660254037844387076, 1.000000000000000000, 0.8660254037844387076, 1.000000000000000000, 0.8660254037844387076, 1.000000000000000000, 0.8660254037844387076, 1.000000000000000000, 0.8660254037844387076, 1.000000000000000000, 0.8660254037844387076, 1.000000000000000000, 0.8660254037844387076, 1.000000000000000000, 0.8660254037844387076, 1.000000000000000000, 0.8660254037844387076, 1.000000000000000000, 0.8660254037844387076, 1.000000000000000000, 0.8660254037844387076, 1.000000000000000000, 0.8660254037844387076, 1.000000000000000000, 0.8660254037844387076, 1.000000000000000000, 0.8660254037844387076, 1.000000000000000000, 0.8660254037844387076, 1.000000000000000000, 0.8660254037844387076, 1.000000000000000000, 0.8660254037844387076, 1.000000000000000000, 0.8660254037844387076, 1.000000000000000000, 0.8660254037844387076, 1.000000000000000000, 0.8660254037844387076, 1.000000000000000000, 0.8660254037844387076, 1.000000000000000000, 0.8660254037844387076, 1.000000000000000000, 0.8660254037844387076, 1.000000000000000000, 0.8660254037844387076, 1.000000000000000000, 0.8660254037844387076, 1.000000000000000000, 0.8660254037844387076, 1.000000000000000000, 0.8871737995726820536, 0.9643799166510427234 ) ) 
 REPRESENTATION_ITEM ( '' )  );
#11931 = CARTESIAN_POINT ( 'NONE',  ( 5.110025693318159590, -0.7223781944584523051, 1.879196401790662607 ) ) ;
#11932 = CARTESIAN_POINT ( 'NONE',  ( 3.909285118862667829, 1.805215983022747439, 1.084321332058492571 ) ) ;
#11933 = CARTESIAN_POINT ( 'NONE',  ( 2.442874106818424096, -1.667949397242382448, -0.9418811778915718858 ) ) ;
#11934 = CARTESIAN_POINT ( 'NONE',  ( 10.12374542407608935, 0.2401923788623722134, -4.551898349974264235 ) ) ;
#11935 = CARTESIAN_POINT ( 'NONE',  ( 2.945709429406599966, 1.390870048597905084, 1.394762357610879855 ) ) ;
#11936 = CARTESIAN_POINT ( 'NONE',  ( 5.185809364388858533, 1.945378451193703118, -0.5428193807620449451 ) ) ;
#11937 = CARTESIAN_POINT ( 'NONE',  ( 1.234984068473435892, -1.692697435815498919, 0.7966027930108383615 ) ) ;
#11940 = ORIENTED_EDGE ( 'NONE', *, *, #26674, .T. ) ;
#11939 = CARTESIAN_POINT ( 'NONE',  ( 1.019614524654769872, -0.4619345408787678964, 1.855657206939323789 ) ) ;
#11938 = CARTESIAN_POINT ( 'NONE',  ( 5.109832884134172026, -1.716065896558026216, 0.1740927981267632318 ) ) ;
#11942 = CARTESIAN_POINT ( 'NONE',  ( 5.192409644353875642, 5.160158794608717514, 1.040834085586084257E-14 ) ) ;
#11941 = CARTESIAN_POINT ( 'NONE',  ( 1.401302286655212948, 1.802556353783949517, -1.272968949304439379 ) ) ;
#11943 = CARTESIAN_POINT ( 'NONE',  ( -1.402160292154681736E-14, 1.759375000341421469, -1.575800808251659024 ) ) ;
#11944 = CARTESIAN_POINT ( 'NONE',  ( 8.158255747121103241, 10.54105100977322174, 1.599625672291281386 ) ) ;
#11945 = CARTESIAN_POINT ( 'NONE',  ( -1.393942678861017415, 1.000000000000001332, 1.636894562288534694 ) ) ;
#11946 = CARTESIAN_POINT ( 'NONE',  ( 1.499999999999990896, 3.806250000682819046, 1.214306433183764966E-14 ) ) ;
#11947 = CARTESIAN_POINT ( 'NONE',  ( -4.120788623549732854, 6.895004929861607401, -1.199719254218452047 ) ) ;
#11948 = DIRECTION ( 'NONE',  ( 0.000000000000000000, 0.000000000000000000, 1.000000000000000000 ) ) ;
#11949 = CARTESIAN_POINT ( 'NONE',  ( 2.488806849732328796, 2.007603858877416769, 0.5053560088097220904 ) ) ;
#11950 = CARTESIAN_POINT ( 'NONE',  ( 1.499999999999989120, 2.025000000000019895, 1.214306433183764966E-14 ) ) ;
#11951 = CARTESIAN_POINT ( 'NONE',  ( 6.419949431270806528, 7.448694743692793274, 1.199719254218462483 ) ) ;
#11952 = CARTESIAN_POINT ( 'NONE',  ( -7.660520486921249983, 8.896027641951645748, -1.199719254218446718 ) ) ;
#11953 = CARTESIAN_POINT ( 'NONE',  ( 8.000720045840086669, 8.506797273001177828, 0.7216878364870267237 ) ) ;
#11954 = CARTESIAN_POINT ( 'NONE',  ( 6.094406630213895504, -1.134638919006492275, 1.791192486788994120 ) ) ;
#11955 = CARTESIAN_POINT ( 'NONE',  ( -2.255140518769849223E-14, 3.249999999999988898, -4.336808689942017736E-14 ) ) ;
#11956 = CARTESIAN_POINT ( 'NONE',  ( 0.6823417656249899377, 2.342708333674753618, 1.181850606188767472 ) ) ;
#11957 = ORIENTED_EDGE ( 'NONE', *, *, #98123, .F. ) ;
#11959 = CARTESIAN_POINT ( 'NONE',  ( 4.369805582306193870, 3.992528022312320957, 1.214306433183764966E-14 ) ) ;
#11958 = DIRECTION ( 'NONE',  ( 0.000000000000000000, 0.000000000000000000, 1.000000000000000000 ) ) ;
#11960 = CARTESIAN_POINT ( 'NONE',  ( 4.622422610786712127, 0.4444332032229811325, -1.966343831704894907 ) ) ;
#11961 = CARTESIAN_POINT ( 'NONE',  ( 4.381993024020896854, -1.915445973796879864, -0.04088167158281148100 ) ) ;
#11962 = PRESENTATION_STYLE_ASSIGNMENT (( #160359 ) ) ;
#11963 = CARTESIAN_POINT ( 'NONE',  ( 2.736070936638954176, 2.175344985778558726, 0.2654339622269741295 ) ) ;
#11964 = DIRECTION ( 'NONE',  ( -0.05872483221476467591, 7.952201780260630618E-17, -0.9982742078614211811 ) ) ;
#11965 = CARTESIAN_POINT ( 'NONE',  ( -0.7500000000000006661, 0.3895833340161539149, -1.299038105676652011 ) ) ;
#11966 = CARTESIAN_POINT ( 'NONE',  ( 5.080342566386993219, 0.9961330521413218619, 1.749448578721881198 ) ) ;
#11967 = CARTESIAN_POINT ( 'NONE',  ( -7.230575994789712801, 7.330093503543126054, 0.7998128361456341429 ) ) ;
#11969 = CARTESIAN_POINT ( 'NONE',  ( 0.2984541275833849094, 1.388471424577278235, -1.462460896543740674 ) ) ;
#11968 = CARTESIAN_POINT ( 'NONE',  ( -2.657034918598345730, 5.083329257464595408, -1.082531754730543971 ) ) ;
#11970 = CARTESIAN_POINT ( 'NONE',  ( -1.364683531250000748, 9.171875000341403350, 0.000000000000000000 ) ) ;
#11972 = CARTESIAN_POINT ( 'NONE',  ( -5.582925393777276035, 9.735439736040634173, 0.7998128361456291469 ) ) ;
#11971 = CARTESIAN_POINT ( 'NONE',  ( 3.544548742447044987, -1.707904676211311479, 1.205638247120393247 ) ) ;
#11974 = ORIENTED_EDGE ( 'NONE', *, *, #22906, .T. ) ;
#11973 = CARTESIAN_POINT ( 'NONE',  ( 2.186159124499872597, -1.690733796973374004, -0.3399922242280882245 ) ) ;
#11975 = CARTESIAN_POINT ( 'NONE',  ( 5.642871316567687145, 2.044259226470702462, 0.5637153772257290640 ) ) ;
#11976 = CARTESIAN_POINT ( 'NONE',  ( 4.638861114170084399, 8.563755066507100722, 0.7998128361456462443 ) ) ;
#11977 = CARTESIAN_POINT ( 'NONE',  ( -5.608717438317167847, 5.638785078248324645, 0.4778177780641221228 ) ) ;
#11978 = CARTESIAN_POINT ( 'NONE',  ( 7.768428355093493387, -6.306978362809817718, 7.788485247865709837 ) ) ;
#11979 = CARTESIAN_POINT ( 'NONE',  ( 6.784764760059096567, -8.039737506397907296, -6.649736275991404710 ) ) ;
#11980 = CARTESIAN_POINT ( 'NONE',  ( 6.602984505055297326, 7.662235663108029726, 1.199719254218462483 ) ) ;
#11981 = DIRECTION ( 'NONE',  ( 1.207943261119674327E-30, 2.168404344971008079E-15, 1.000000000000000000 ) ) ;
#11982 = CARTESIAN_POINT ( 'NONE',  ( 1.154613445820645845, 0.3528100842024176620, 1.776585200675658172 ) ) ;
#11983 = CARTESIAN_POINT ( 'NONE',  ( -5.181187258716735577, 9.196468901811520880, 0.7998128361456481317 ) ) ;
#11984 = EDGE_LOOP ( 'NONE', ( #37305, #163075 ) ) ;
#11985 = CARTESIAN_POINT ( 'NONE',  ( 4.542145155778077203, 5.257923088951247159, -1.199719254218452047 ) ) ;
#11986 = ORIENTED_EDGE ( 'NONE', *, *, #17877, .F. ) ;
#11987 = CARTESIAN_POINT ( 'NONE',  ( 4.199993725183334803, 8.122019456014369254, -0.7998128361456362523 ) ) ;
#11988 = CARTESIAN_POINT ( 'NONE',  ( 3.070771698229213698, -1.370002115350689165, 1.185199408711124835 ) ) ;
#11989 = CARTESIAN_POINT ( 'NONE',  ( 6.639320575229291421, 7.052752469465089824, 2.594893258668645952 ) ) ;
#11990 = CARTESIAN_POINT ( 'NONE',  ( -10.99856159529784883, -8.101932402265175526, 0.2004767358929543664 ) ) ;
#11991 = CARTESIAN_POINT ( 'NONE',  ( 4.139348914150634329, 7.410017372392475821, 0.7316189255667099323 ) ) ;
#11992 = CARTESIAN_POINT ( 'NONE',  ( 3.490524873212813795, 1.815147244032933038, 0.4099927795770376693 ) ) ;
#11993 = CARTESIAN_POINT ( 'NONE',  ( 1.106889576528688801, -0.04550283046177550778, 1.915226712711289636 ) ) ;
#11994 = CARTESIAN_POINT ( 'NONE',  ( 0.7799652524137989928, -1.018268764971082430, 1.515009401286564694 ) ) ;
#11995 = AXIS2_PLACEMENT_3D ( 'NONE', #121616, #84759, #200617 ) ;
#11996 = CARTESIAN_POINT ( 'NONE',  ( -10.39230484541323740, 3.447199233515621408, 6.000000000000048850 ) ) ;
#11997 = CARTESIAN_POINT ( 'NONE',  ( -3.931501358282930791, 7.530575984731325612, 0.7216878364870262796 ) ) ;
#11998 = CARTESIAN_POINT ( 'NONE',  ( 2.207884333776653740E-15, 1.500000000682816914, -1.225000000000019851 ) ) ;
#11999 = CARTESIAN_POINT ( 'NONE',  ( 1.419999999999990603, 8.627523663848661428, -2.579999999999989413 ) ) ;
#12000 = CARTESIAN_POINT ( 'NONE',  ( 0.000000000000000000, -0.4330127018922214077, 0.000000000000000000 ) ) ;
#12001 = AXIS2_PLACEMENT_3D ( 'NONE', #81531, #79397, #144447 ) ;
#12002 = CARTESIAN_POINT ( 'NONE',  ( 6.792271770766432404, 10.86814146596211472, 1.040834085586084257E-14 ) ) ;
#12003 = CARTESIAN_POINT ( 'NONE',  ( 6.209808219158968967, 0.5752867347804692111, -1.883509059051315271 ) ) ;
#12004 = CARTESIAN_POINT ( 'NONE',  ( -5.579343907223557331, 6.467988298970945849, 1.199719254218450271 ) ) ;
#12005 = CARTESIAN_POINT ( 'NONE',  ( -3.981404450745295254, 7.309521899770400566, -0.7443278975401018682 ) ) ;
#12006 = EDGE_CURVE ( 'NONE', #164855, #93781, #55325, .T. ) ;
#12007 = CARTESIAN_POINT ( 'NONE',  ( 0.2520486530714799445, 0.8021226228236020273, 1.930841216200715360 ) ) ;
#12008 = CARTESIAN_POINT ( 'NONE',  ( 7.283754839039659146, 9.520799950344851936, -1.599625672291262513 ) ) ;
#12009 = CARTESIAN_POINT ( 'NONE',  ( 5.245112492223927170, -1.652184091924509879, 0.9903546681122497031 ) ) ;
#12010 = CARTESIAN_POINT ( 'NONE',  ( -6.417086777969760902, 6.381022750586497594, 0.7998128361456341429 ) ) ;
#12011 = CARTESIAN_POINT ( 'NONE',  ( 1.219449367515994309, -1.782015241123528826, 0.3957228718986585680 ) ) ;
#12012 = CARTESIAN_POINT ( 'NONE',  ( 2.209865124170300898, -0.4819264253047173541, 2.153463223375853719 ) ) ;
#12013 = CARTESIAN_POINT ( 'NONE',  ( -6.190835592010745181, 6.962597444594667451, 0.8873991478343831174 ) ) ;
#12014 = CARTESIAN_POINT ( 'NONE',  ( 2.925527285498711549, 6.635141943048991742, 0.7998128361456281477 ) ) ;
#12015 = MECHANICAL_DESIGN_GEOMETRIC_PRESENTATION_REPRESENTATION (  '', ( #98457 ), #133123 ) ;
#12016 = CARTESIAN_POINT ( 'NONE',  ( 0.9945129418027212065, 1.939812372797902862, 0.3400383455644633290 ) ) ;
#12017 = CARTESIAN_POINT ( 'NONE',  ( 3.034642427012054444, -1.711418951474739991, 0.9179939537737377142 ) ) ;
#12018 = ORIENTED_EDGE ( 'NONE', *, *, #78925, .T. ) ;
#12019 = CARTESIAN_POINT ( 'NONE',  ( 0.4036724312478366938, 0.3418800534340654118, 1.986742826083332858 ) ) ;
#12021 = CARTESIAN_POINT ( 'NONE',  ( 4.926513725511825648, -1.217676453003987191, 1.407301474667689956 ) ) ;
#12020 = CARTESIAN_POINT ( 'NONE',  ( -5.224688093219839402, 7.188831756880171397, -1.599625672291271394 ) ) ;
#12022 = CARTESIAN_POINT ( 'NONE',  ( 4.552505719138623341, 8.533283448962240669, 0.7998128361456341429 ) ) ;
#12024 = EDGE_CURVE ( 'NONE', #121388, #57555, #62280, .T. ) ;
#12023 = DIRECTION ( 'NONE',  ( 2.949029909160572061E-17, 1.000000000000000000, -8.673600428462354978E-15 ) ) ;
#12025 = CARTESIAN_POINT ( 'NONE',  ( -7.779015489124656568, -5.502990254781792601, -7.777446446097291854 ) ) ;
#12026 = CARTESIAN_POINT ( 'NONE',  ( -4.985647801523292344, 6.839675073242382553, -1.599625672291256295 ) ) ;
#12027 = CARTESIAN_POINT ( 'NONE',  ( -6.424584688029276514, 8.588711117491191871, 1.599625672291269396 ) ) ;
#12028 = CARTESIAN_POINT ( 'NONE',  ( 1.874823134854076923, -0.1115055541827478930, -2.188858692977871279 ) ) ;
#12029 = CARTESIAN_POINT ( 'NONE',  ( 5.016153647376217606, 4.954526798134778254, 0.7216878364870317197 ) ) ;
#12030 = CARTESIAN_POINT ( 'NONE',  ( 0.000000000000000000, 5.499999999999998224, 0.000000000000000000 ) ) ;
#12031 = CARTESIAN_POINT ( 'NONE',  ( 3.211362085483655981, -0.3553965070040401852, 1.790585553824732390 ) ) ;
#12032 = CARTESIAN_POINT ( 'NONE',  ( -4.457933580795036654, 4.095344020549286590, -0.7998128361456221525 ) ) ;
#12033 = CARTESIAN_POINT ( 'NONE',  ( -5.088387723830502196, 4.830873854090670605, -0.7998128361456221525 ) ) ;
#12034 = CARTESIAN_POINT ( 'NONE',  ( -4.728114892278019177, 8.325812319508695936, -0.7463954279460782715 ) ) ;
#12035 = CARTESIAN_POINT ( 'NONE',  ( 6.925078400183558358, 1.280611897634201579, 1.970548662192173506 ) ) ;
#12036 =( GEOMETRIC_REPRESENTATION_CONTEXT ( 3 ) GLOBAL_UNCERTAINTY_ASSIGNED_CONTEXT ( ( #66933 ) ) GLOBAL_UNIT_ASSIGNED_CONTEXT ( ( #170220, #120491, #168099 ) ) REPRESENTATION_CONTEXT ( 'NONE', 'WORKASPACE' ) );
#12037 = CARTESIAN_POINT ( 'NONE',  ( 7.703003830858588863, 12.13858823597705872, -0.7998128361456291469 ) ) ;
#12038 = CARTESIAN_POINT ( 'NONE',  ( 1.207505077391484161, -0.4687122323817956571, 1.868500445134027466 ) ) ;
#12039 = CARTESIAN_POINT ( 'NONE',  ( 6.121922100595678096, 1.933298025717408608, -0.3319332437697538607 ) ) ;
#12040 = CARTESIAN_POINT ( 'NONE',  ( -5.865874016206865882, 9.995270118883347266, 0.000000000000000000 ) ) ;
#12041 = CARTESIAN_POINT ( 'NONE',  ( 6.498435699651741615, 6.475929825882159818, -0.7998128361456281477 ) ) ;
#12042 = CARTESIAN_POINT ( 'NONE',  ( 5.108995794240286159, -0.3219066699026683631, 2.167653318578148358 ) ) ;
#12043 = EDGE_CURVE ( 'NONE', #35130, #84148, #193256, .T. ) ;
#12044 = CYLINDRICAL_SURFACE ( 'NONE', #201574, 1.500000000000000222 ) ;
#12045 = CARTESIAN_POINT ( 'NONE',  ( 4.047765473330780850, 1.496028175931501947, 1.431257568052332729 ) ) ;
#12048 = B_SPLINE_CURVE_WITH_KNOTS ( 'NONE', 3,
 ( #129398, #197492, #195377, #51259, #180196, #32870, #148758, #15530, #113125, #33929, #66398, #17658, #79485, #147699, #116310, #49134, #115251, #179130, #100004, #211599, #30753, #181242, #117383, #98946, #95766, #165000, #161820, #83741, #13409, #82674, #328, #72824, #69608, #6745, #34986, #155163, #153022, #184438, #55522, #138927, #19803, #85887, #137856, #183380, #84815, #151963, #36055, #134670, #101056, #121677, #3535, #167145, #37128, #170326, #5663, #204944, #135715, #118451, #22992, #4597, #21913, #200673, #88022, #86954, #201741, #18731, #154094, #56595, #150904, #2465, #68541, #102135, #185504, #70671, #52322, #71742, #168204, #53382, #119517, #103207, #169269, #203877, #20855, #136781, #202810, #54458, #120602, #186579, #38208, #187642, #104281, #39270, #105364, #171401, #89109, #172484, #108605, #77093, #25142, #189780, #73910, #42497, #123820, #107539, #173571, #78161, #91244, #160487, #41431, #144292, #159418, #12094, #28353, #157304, #210285, #8894, #122757, #188718, #94448, #92327, #74974, #57662, #24071, #59785, #141083, #143220, #40356, #90175, #207093, #58721, #140003, #106460, #60850, #124872, #156240, #190837, #109682, #11018, #7817, #174633, #26209, #158368, #206024, #175685, #9961, #27274, #76038, #142141, #208155, #93381, #125942, #191900, #43562, #209209, #127013, #192972, #44624, #110739, #176739, #29430, #61925, #96582, #182040, #95521, #130197, #198289, #177814, #131249, #128084, #165816, #194041, #161570, #99746, #213469, #197235, #13158, #147445, #65092, #111809, #149565, #79235, #62978, #211354, #98688, #145353, #49931, #129147, #116052, #74, #195123, #113944, #46761, #45694, #81365, #16337, #17399, #83483, #112872, #82418, #14205, #178887, #30500, #33671, #31564, #162630, #148507, #80300, #146397, #114993, #212411, #180991, #66138, #163696, #179940, #196191, #64054, #48875, #47834, #32611, #97639, #164745, #132284, #15278, #35801, #150646, #55266, #185240, #54196, #100802, #187385, #121413, #101878, #3280, #120337, #184181, #202547, #167945, #36863, #171139, #67212, #166888, #186313, #134416, #183124, #1149, #37948, #39016, #22731, #2207, #104020, #70409, #153836, #137596, #105098, #170067, #88847, #18477, #133347, #119256, #21653, #5406, #4342, #51001, #199353, #117121, #69347, #102947, #34730, #84557, #68284, #200420, #52067, #118193, #86691, #152760, #87760, #19546, #71484, #85624, #53123, #151711, #135458, #203614, #169007, #201481, #20605, #136527, #109421, #190577, #159159, #60587, #8634, #158112, #9703, #10758, #106198, #74715, #204684, #192704, #124619, #157046, #93118, #191637, #76831, #56334, #140818, #175426, #57394, #7557, #172225, #43301, #122493, #188455, #6488, #126745, #75780, #206832, #28092, #123559, #73643, #205765, #44360, #189523, #155971, #89918, #27012, #40087, #142952, #23814, #208951, #110482, #139741, #58465, #41169, #154905, #174370, #176481, #72564, #138662, #107278, #173297, #125677, #24879, #90984, #42233, #108348, #25949, #92056, #141887, #207896, #59519, #195933, #45429, #198046, #161303, #97381, #213220, #128874, #127829, #32365, #130997, #145086, #111545, #211090, #77902, #12888, #78966, #177554, #13953, #95254, #62713, #194856, #49675, #46489, #132036, #112611, #115800, #196986, #181788, #214257, #178623, #30233, #94188, #160228, #65888, #63788, #96319 ),
 .UNSPECIFIED., .F., .F.,
 ( 4, 1, 1, 1, 1, 1, 1, 1, 1, 1, 1, 1, 1, 1, 1, 1, 1, 1, 1, 1, 1, 1, 1, 1, 1, 1, 1, 1, 1, 1, 1, 1, 1, 1, 1, 1, 1, 1, 1, 1, 1, 1, 1, 1, 1, 1, 1, 1, 1, 1, 1, 1, 1, 1, 1, 1, 1, 1, 1, 1, 1, 1, 1, 1, 1, 1, 1, 1, 1, 1, 1, 1, 1, 1, 1, 1, 1, 1, 1, 1, 1, 1, 1, 1, 1, 1, 1, 1, 1, 1, 1, 1, 1, 1, 1, 1, 1, 1, 1, 1, 1, 1, 1, 1, 1, 1, 1, 1, 1, 1, 1, 1, 1, 1, 1, 1, 1, 1, 1, 1, 1, 1, 1, 1, 1, 1, 1, 1, 1, 1, 1, 1, 1, 1, 1, 1, 1, 1, 1, 1, 1, 1, 1, 1, 1, 1, 1, 1, 1, 1, 1, 1, 1, 1, 1, 1, 1, 1, 1, 1, 1, 1, 1, 1, 1, 1, 1, 1, 1, 1, 1, 1, 1, 1, 1, 1, 1, 1, 1, 1, 1, 1, 1, 1, 1, 1, 1, 1, 1, 1, 1, 1, 1, 1, 1, 1, 1, 1, 1, 1, 1, 1, 1, 1, 1, 1, 1, 1, 1, 1, 1, 1, 1, 1, 1, 1, 1, 1, 1, 1, 1, 1, 1, 1, 1, 1, 1, 1, 1, 1, 1, 1, 1, 1, 1, 1, 1, 1, 1, 1, 1, 1, 1, 1, 1, 1, 1, 1, 1, 1, 1, 1, 1, 1, 1, 1, 1, 1, 1, 1, 1, 1, 1, 1, 1, 1, 1, 1, 1, 1, 1, 1, 1, 1, 1, 1, 1, 1, 1, 1, 1, 1, 1, 1, 1, 1, 1, 1, 1, 1, 1, 1, 1, 1, 1, 1, 1, 1, 1, 1, 1, 1, 1, 1, 1, 1, 1, 1, 1, 1, 1, 1, 1, 1, 1, 1, 1, 1, 1, 1, 1, 1, 1, 1, 1, 1, 1, 1, 1, 1, 1, 1, 1, 1, 1, 1, 1, 1, 1, 1, 1, 1, 1, 1, 1, 1, 1, 1, 1, 1, 1, 1, 1, 1, 1, 1, 1, 1, 1, 1, 1, 1, 1, 1, 1, 1, 1, 1, 1, 1, 1, 1, 1, 1, 1, 1, 1, 1, 1, 1, 1, 1, 1, 1, 4 ),
 ( 0.000000000000000000, 0.002600063085273907840, 0.005208809393482579861, 0.007813201938950280895, 0.01041611862257568050, 0.01302098276518856741, 0.01562474632808895890, 0.01822919105953027183, 0.02083324087635668453, 0.02343728507989274734, 0.02604173773626635227, 0.02864548761524753420, 0.03125016255115702773, 0.03385383280295282959, 0.03645844125268089125, 0.03906229690237970897, 0.04166656525949016115, 0.04427081591349327910, 0.04687468903198145631, 0.04947928942627017462, 0.05208296534865054783, 0.05468764290212216328, 0.05729137561078536528, 0.05989584521530456201, 0.06249987723257615507, 0.06510392926424246607, 0.06770838613806146045, 0.07031213076997053224, 0.07291680575263978503, 0.07552047744215656389, 0.07812508546332513903, 0.08072894086165181837, 0.08333320924388483431, 0.08593745993457323207, 0.08854133291633270453, 0.09114593330519306369, 0.09374960916840779923, 0.09635428668231969807, 0.09895801939011879267, 0.1015624889210437753, 0.1041665209728785957, 0.1067705729027476208, 0.1093750297965602747, 0.1119787743537518920, 0.1145834493281674554, 0.1171871210017138010, 0.1197917289818775377, 0.1223955844170728779, 0.1249998527215379351, 0.1276041034591044177, 0.1302079763611066199, 0.1328125767709825433, 0.1354162526020633861, 0.1380209301064295735, 0.1406246628425296130, 0.1432291323291436380, 0.1458331644451768827, 0.1484372163025670099, 0.1510416732455448496, 0.1536454177576472568, 0.1562500927529001105, 0.1588537644400710158, 0.1614583724083656635, 0.1640622279099430147, 0.1666664961659596600, 0.1692707469797122277, 0.1718746198314790308, 0.1744792202914958457, 0.1770828961200470730, 0.1796875736439581817, 0.1822913064379278192, 0.1848957759094348730, 0.1874998081190861754, 0.1901038599334289314, 0.1927083169547665342, 0.1953120614513534081, 0.1979167364965291054, 0.2005204082269216870, 0.2031250162124720871, 0.2057288718099357372, 0.2083331400468157457, 0.2109373909660553770, 0.2135412637971000893, 0.2161458643363758370, 0.2187495401919937743, 0.2213542177645327069, 0.2239579506459335456, 0.2265624201315297737, 0.2291664524642116896, 0.2317705042649303715, 0.2343749613938155840, 0.2369787059044528299, 0.2395833810286300269, 0.2421870528318344207, 0.2447916608637582536, 0.2473955165866061623, 0.2499997848336539263, 0.2526040358876752157, 0.2552079087275039293, 0.2578125093751503782, 0.2604161852874245509, 0.2630208629376679097, 0.2656245959360551967, 0.2682290654649299166, 0.2708330979500496172, 0.2734371497665608608, 0.2760416070321756732, 0.2786453515864226738, 0.2812500268186742258, 0.2838536987242743503, 0.2864583068316831627, 0.2890621627094078216, 0.2916664309959213219, 0.2942706822140139789, 0.2968745550921262355, 0.2994791558772498252, 0.3020828318757637354, 0.3046875096327826826, 0.3072912427777066413, 0.3098957123790437307, 0.3124997450460035853, 0.3151037969077182255, 0.3177082543392401592, 0.3203119989666507461, 0.3229166743360447622, 0.3255203463736199843, 0.3281249545856204097, 0.3307288106477103140, 0.3333330790029824242, 0.3359373304144318562, 0.3385412033603223403, 0.3411458043120255135, 0.3437494804263583337, 0.3463541583192197293, 0.3489578916402267250, 0.3515623613432052874, 0.3541663942214042238, 0.3567704461577280162, 0.3593749037843310123, 0.3619786485144548260, 0.3645833240500557237, 0.3671869962491814965, 0.3697916045948764219, 0.3723954608708167080, 0.3749997293241361662, 0.3776039809582251716, 0.3802078540013843488, 0.3828124551487663840, 0.3854161314084936785, 0.3880208094662612184, 0.3906245429928945634, 0.3932290128266905938, 0.3958330459455252637, 0.3984370979858605777, 0.4010415558367163569, 0.4036453006990994852, 0.4062499764299690730, 0.4088536488202184072, 0.4114582573287078326, 0.4140621138479816388, 0.4166663824286341855, 0.4192706343146435644, 0.4218745074845589027, 0.4244791088567174686, 0.4270827852914125256, 0.4296874635431477407, 0.4322911973049493040, 0.4348956672987361882, 0.4374997006876018557, 0.4401037528613486738, 0.4427082109656274023, 0.4453119559898139901, 0.4479166319450127998, 0.4505203045559570407, 0.4531249132563394122, 0.4557287700484292658, 0.4583330387856985322, 0.4609372909529084184, 0.4635411642790657205, 0.4661457659050973201, 0.4687494425443319290, 0.4713541210190953512, 0.4739578550456061690, 0.4765623252285562383, 0.4791663589168480009, 0.4817704112534048067, 0.4843748696402766507, 0.4869786148558097882, 0.4895832910643978519, 0.4921869639256079565, 0.4947915728469811647, 0.4973954299413693159, 0.4999996988645384333, 0.5026039513422294602, 0.5052078248541136407, 0.5078124267631153321, 0.5104161036364611714, 0.5130207823633133879, 0.5156245166840751626, 0.5182289870853604707, 0.5208330211024742029, 0.5234370736312391470, 0.5260415323298749390, 0.5286452777662975500, 0.5312499542573357880, 0.5338536273983837122, 0.5364582365698458144, 0.5390620939960163449, 0.5416663631343685559, 0.5442706159518226894, 0.5468744896789192733, 0.5494790918999890028, 0.5520827690370186946, 0.5546874480450217915, 0.5572911826895774468, 0.5598956533383712131, 0.5624996877137050655, 0.5651037404640770756, 0.5677081995036498130, 0.5703119451905063197, 0.5729166219930570403, 0.5755202954435161278, 0.5781249048941674573, 0.5807287626816063364, 0.5833330320644263267, 0.5859372852509285856, 0.5885411592227242084, 0.5911457617849628088, 0.5937494392152512512, 0.5963541185334689798, 0.5989578535313645480, 0.6015623244568418793, 0.6041663592197970001, 0.6067704122211770024, 0.6093748716308627911, 0.6119786175976995590, 0.6145832947408284008, 0.6171869685302752151, 0.6197915782892181591, 0.6223954364674153528, 0.6249997061239902507, 0.6276039597088286515, 0.6302078339548128350, 0.6328124368873246919, 0.6354161146404495586, 0.6380207942979494451, 0.6406245296787346222, 0.6432290009100736228, 0.6458330360900554901, 0.6484370893718474083, 0.6510415491808263511, 0.6536452954571934093, 0.6562499729699700080, 0.6588536471279848872, 0.6614582572243260516, 0.6640621158227759668, 0.6666663857823964534, 0.6692706397948642305, 0.6718745143445301604, 0.6744791176764239893, 0.6770827957819672838, 0.6796874758078212952, 0.6822912116010506622, 0.6848956831674339885, 0.6874997187938534093, 0.6901037723854651640, 0.6927082326229228038, 0.6953119792383747333, 0.6979166571498732763, 0.7005203317060422208, 0.7031249421688929857, 0.7057288012170955804, 0.7083330715090569996, 0.7109373259784533827, 0.7135412008612989077, 0.7161458046216893081, 0.7187494831092385850, 0.7213541635325240176, 0.7239578997677582617, 0.7265623716983737879, 0.7291664078006476757, 0.7317704617314926274, 0.7343749224266207243, 0.7369786694107173242, 0.7395833477500189934, 0.7421870227339337767, 0.7447916335924112952, 0.7473954931198736329, 0.7499997637734774347, 0.7526040187291080930, 0.7552078939746372788, 0.7578124981926457338, 0.7604161770917949870, 0.7630208579415957981, 0.7656245946484027121, 0.7682290669724446408, 0.7708331035799980135, 0.7734371578794957403, 0.7760416190614934928, 0.7786453664438016675, 0.7812500452399944173, 0.7838537206812543623, 0.7864583319644831150, 0.7890621920007202528, 0.7916664630452742157, 0.7942707185164536998, 0.7968745941541772737, 0.7994791988589329268, 0.8020828781992835887, 0.8046875595046918406, 0.8072912967126475436, 0.8098957694593176271, 0.8124998066015838294, 0.8151038612991610144, 0.8177083229972362810, 0.8203120708073305956, 0.8229167500895105958, 0.8255204260177235742, 0.8281250377548363684, 0.8307288983293719120, 0.8333331697941922522, 0.8359374258102438837, 0.8385413018696807885, 0.8411459070903221091, 0.8437495869014844940, 0.8463542686916004643, 0.8489580064302900686, 0.8515624796287988296, 0.8541665173352209761, 0.8567705724603134065, 0.8593750347036837045, 0.8619787829711476057, 0.8645834627684209073, 0.8671871392132045608, 0.8697917514333429745, 0.8723956125757112989, 0.8749998844901232253, 0.8776041410803804288, 0.8802080175910590443, 0.8828126233567346048, 0.8854163036683286858, 0.8880209859722626442, 0.8906247242712825862, 0.8932291979508502067, 0.8958332362508822921, 0.8984372918329353030, 0.9010417546508288078, 0.9036455034052560675, 0.9062501837467389354, 0.9088538607377212308, 0.9114584734700372781, 0.9140623352097841936, 0.9166666076031229071, 0.9192708647969299873, 0.9218747417883903505, 0.9244793481282622682, 0.9270830289699085736, 0.9296877118167798937, 0.9322914507057830091, 0.9348959248956096868, 0.9374999638185942397, 0.9401040198872741005, 0.9427084833090058069, 0.9453122325795346725, 0.9479169134952544207, 0.9505205910598265584, 0.9531252043308329203, 0.9557290667238423909, 0.9583333396063040688, 0.9609375973010293448, 0.9635414750455153499, 0.9661460823481272664, 0.9687497623469286667, 0.9713544456720903941, 0.9739581901020435417, 0.9765626606554614897, 0.9791666924408860551, 0.9817707657828746992, 0.9843752055175947202, 0.9869789906880002128, 0.9895838567146432174, 0.9921867690109741345, 0.9947911791560083428, 0.9973999138825643263, 0.9999999999999998890 ),
 .UNSPECIFIED. ) ;
#12047 = CARTESIAN_POINT ( 'NONE',  ( -1.402160292154681736E-14, 1.509375000341420359, -1.575800808251659024 ) ) ;
#12046 = PRESENTATION_STYLE_ASSIGNMENT (( #124826 ) ) ;
#12049 = ORIENTED_EDGE ( 'NONE', *, *, #172459, .F. ) ;
#12050 = VERTEX_POINT ( 'NONE', #156507 ) ;
#12051 = CARTESIAN_POINT ( 'NONE',  ( 3.551692777231782561, -1.542557649656286944, 1.704429084079077006 ) ) ;
#12053 = ORIENTED_EDGE ( 'NONE', *, *, #141945, .F. ) ;
#12052 = CARTESIAN_POINT ( 'NONE',  ( 7.510853912290742507, 8.825379654836435606, -1.082531754730537976 ) ) ;
#12055 = CARTESIAN_POINT ( 'NONE',  ( 1.642778471875001811, -1.392708332855374653, 2.845375778867859751 ) ) ;
#12054 = CARTESIAN_POINT ( 'NONE',  ( 5.912764389335563919, 6.070849007079172743, -0.7216878364870458196 ) ) ;
#12056 = DIRECTION ( 'NONE',  ( -1.000000000000000000, 0.000000000000000000, 0.000000000000000000 ) ) ;
#12057 = CARTESIAN_POINT ( 'NONE',  ( -15.75000000000000000, 12.29999999999998295, 3.199999999999997957 ) ) ;
#12058 = CARTESIAN_POINT ( 'NONE',  ( 4.083879184154452169, -1.920976184332440662, -0.2838548334032560683 ) ) ;
#12059 = ORIENTED_EDGE ( 'NONE', *, *, #111106, .T. ) ;
#12061 = CARTESIAN_POINT ( 'NONE',  ( 8.554831740098642001, 12.92446143018304916, 0.7216878364870438212 ) ) ;
#12060 = AXIS2_PLACEMENT_3D ( 'NONE', #146329, #96517, #65028 ) ;
#12062 = ORIENTED_EDGE ( 'NONE', *, *, #108718, .F. ) ;
#12063 = CARTESIAN_POINT ( 'NONE',  ( 4.939673314881130040, -1.814047719456039154, 0.6055163330952323397 ) ) ;
#12064 = CARTESIAN_POINT ( 'NONE',  ( 5.842733193948632220, 0.3409603658401075821, 1.690541223788865510 ) ) ;
#12065 = CARTESIAN_POINT ( 'NONE',  ( 4.487517715496184501, -0.5331711073110931842, 1.944729879240604031 ) ) ;
#12066 = DIRECTION ( 'NONE',  ( 0.000000000000000000, -1.000000000000000000, 0.000000000000000000 ) ) ;
#12067 = CARTESIAN_POINT ( 'NONE',  ( 2.016531038934398445, -1.041976349804032420, -1.945408382319254503 ) ) ;
#12069 = CARTESIAN_POINT ( 'NONE',  ( 3.284841267552055299, 6.405332120898776793, -0.9495590844852130896 ) ) ;
#12068 = CARTESIAN_POINT ( 'NONE',  ( -10.50487009249003378, 11.15010328419353947, 0.7998128361456462443 ) ) ;
#12071 = CARTESIAN_POINT ( 'NONE',  ( 6.468005306911782881, 0.9119784028226736172, 1.516475106587056532 ) ) ;
#12070 = CARTESIAN_POINT ( 'NONE',  ( 1.693425821628431471, -0.7032018978916483309, 1.968960419152628871 ) ) ;
#12072 = CARTESIAN_POINT ( 'NONE',  ( 6.223279759862190730, 1.994869330463379331, 0.2930738960792296233 ) ) ;
#12074 = CARTESIAN_POINT ( 'NONE',  ( 2.871321604122719418, 2.176383266876817046, -0.7197843628353149947 ) ) ;
#12073 = CARTESIAN_POINT ( 'NONE',  ( 5.574337433874081427, 6.532423756721743580, -1.199719254218452047 ) ) ;
#12075 = CARTESIAN_POINT ( 'NONE',  ( 0.8139225777531241546, 1.606474054549825503, 0.6698172574813018310 ) ) ;
#12076 = CARTESIAN_POINT ( 'NONE',  ( 3.041385797112206912, 0.05609166564453024750, 2.120036961950934273 ) ) ;
#12077 = CARTESIAN_POINT ( 'NONE',  ( 1.284279953904121641, 3.300000000000018030, -0.7749999999999892530 ) ) ;
#12078 = CARTESIAN_POINT ( 'NONE',  ( 1.616079437515309136, 0.5095893236424541284, -1.657241410798731440 ) ) ;
#12079 = CARTESIAN_POINT ( 'NONE',  ( -2.353626204688216217E-14, 0.9843750003414547534, 1.570758158831764062 ) ) ;
#12080 = DIRECTION ( 'NONE',  ( 0.000000000000000000, -1.000000000000000000, 0.000000000000000000 ) ) ;
#12081 = CARTESIAN_POINT ( 'NONE',  ( 0.8718042753090318175, -0.3185811321036461363, 2.147578089749022645 ) ) ;
#12082 = CARTESIAN_POINT ( 'NONE',  ( 3.801970467005914678, -1.040791964576088358, -1.727064642965264740 ) ) ;
#12083 = CARTESIAN_POINT ( 'NONE',  ( 5.375000000000002665, 2.052068128417941395, -3.059081846666863488E-13 ) ) ;
#12084 = CARTESIAN_POINT ( 'NONE',  ( -1.500000000000013101, 1.952083334016152527, 0.8660254037844403729 ) ) ;
#12085 = CARTESIAN_POINT ( 'NONE',  ( 6.498663727319215155, -0.5164181641097148612, -1.855934172746701583 ) ) ;
#12086 = CARTESIAN_POINT ( 'NONE',  ( 0.6823417656249934904, 13.44270833367473195, 1.181850606188764807 ) ) ;
#12087 = CARTESIAN_POINT ( 'NONE',  ( 2.953626239309721679, -1.957189270898977762, 1.050815160798105552 ) ) ;
#12088 = ORIENTED_EDGE ( 'NONE', *, *, #192671, .F. ) ;
#12089 = CARTESIAN_POINT ( 'NONE',  ( 6.710064404886807665, -7.791858861492818811, 6.725651841507094275 ) ) ;
#12090 = CARTESIAN_POINT ( 'NONE',  ( 1.499999999999987566, -0.4749999999999823808, 0.000000000000000000 ) ) ;
#12091 = CARTESIAN_POINT ( 'NONE',  ( 9.250740883225924804, 9.686952540052077509, 1.040834085586084257E-14 ) ) ;
#12092 = CARTESIAN_POINT ( 'NONE',  ( 0.07999999999999327094, -9.900000000000005684, 10.99970695577496294 ) ) ;
#12093 = CARTESIAN_POINT ( 'NONE',  ( 5.249435226766168583, 1.738107782858036687, -0.09287461536438243459 ) ) ;
#12094 = CARTESIAN_POINT ( 'NONE',  ( 4.949637131784443866, 1.452432516441283905, 1.319008059494260143 ) ) ;
#12096 = CARTESIAN_POINT ( 'NONE',  ( -6.073689629242160493, 8.109057205581079231, -1.443375672974059665 ) ) ;
#12095 = CARTESIAN_POINT ( 'NONE',  ( 2.496672843210871129, 6.064535417054653266, -0.7998128361456291469 ) ) ;
#12097 = CARTESIAN_POINT ( 'NONE',  ( -15.75000000000000000, 11.29999999999999893, -0.7000000000000009548 ) ) ;
#12098 = CARTESIAN_POINT ( 'NONE',  ( 5.114671183409561728, 1.565253227384774792, -1.633764300155052807 ) ) ;
#12099 = CARTESIAN_POINT ( 'NONE',  ( 1.926308760915905527, 1.058537693354057785, 1.770204612073868145 ) ) ;
#12100 = CARTESIAN_POINT ( 'NONE',  ( -6.612626235163205024, 8.737816579155630592, -1.599625672291263179 ) ) ;
#12101 = VERTEX_POINT ( 'NONE', #105638 ) ;
#12102 = CARTESIAN_POINT ( 'NONE',  ( -1.500000000000013101, 1.702083334016151417, 0.8660254037844403729 ) ) ;
#12103 = CARTESIAN_POINT ( 'NONE',  ( 3.233525009082056201, -1.253693836546897700, -1.388425355430204622 ) ) ;
#12104 = CARTESIAN_POINT ( 'NONE',  ( 2.724952806592676691, 1.721339412077933284, 0.2094855716100688936 ) ) ;
#12105 = CARTESIAN_POINT ( 'NONE',  ( -0.005774900045998726007, -2.292045413227526751, -0.04753075064714216980 ) ) ;
#12106 = CARTESIAN_POINT ( 'NONE',  ( 1.255210933454937283, -1.738917431694649407, 1.358592805172780693 ) ) ;
#12107 = CARTESIAN_POINT ( 'NONE',  ( 3.977527890101069996, 2.036293384626610248, -0.7259696361804208742 ) ) ;
#12108 = CARTESIAN_POINT ( 'NONE',  ( 5.050698599679353862, -1.641444558978710555, -1.037428038565652466 ) ) ;
#12109 = CARTESIAN_POINT ( 'NONE',  ( -1.907519672996902838, 3.236073672982390903, -0.4612874649730039911 ) ) ;
#12110 = SHAPE_REPRESENTATION_RELATIONSHIP ( 'NONE' , 'NONE' ,  #40301, #171430 ) ;
#12111 = LINE ( 'NONE', #65114, #190282 ) ;
#12112 = CARTESIAN_POINT ( 'NONE',  ( 1.360316468749992236, 2.765625000341414896, -4.683753385137379155E-14 ) ) ;
#12113 = CARTESIAN_POINT ( 'NONE',  ( 5.361953999179126740, -0.05229508359532940298, -2.015913028294749942 ) ) ;
#12114 = CARTESIAN_POINT ( 'NONE',  ( -2.440104460335327463, 5.790612937125752424, 1.040834085586084257E-14 ) ) ;
#12115 = CARTESIAN_POINT ( 'NONE',  ( 6.286176778230493589, 10.48562334124426698, 0.7998128361456462443 ) ) ;
#12116 = CARTESIAN_POINT ( 'NONE',  ( 2.677589438261873234, -0.4530478092824203884, -0.1093532045961659316 ) ) ;
#12117 = CARTESIAN_POINT ( 'NONE',  ( 2.894927146036041510, 1.565677646668685696, -0.9388022922067614795 ) ) ;
#12118 = CARTESIAN_POINT ( 'NONE',  ( 2.626236979526615389, -1.269917727785064843, -1.804575601930514139 ) ) ;
#12119 = ORIENTED_EDGE ( 'NONE', *, *, #82075, .T. ) ;
#12120 = CARTESIAN_POINT ( 'NONE',  ( -3.634994581795317536, 7.254927755487573293, 0.000000000000000000 ) ) ;
#12121 = CIRCLE ( 'NONE', #19073, 0.4000000000000010214 ) ;
#12122 = CARTESIAN_POINT ( 'NONE',  ( 1.001543065824772753E-15, -2.559374999522041172, 3.793834371823811669 ) ) ;
#12123 = CARTESIAN_POINT ( 'NONE',  ( -6.496328159242330536, 10.73079995242472862, 0.000000000000000000 ) ) ;
#12124 = CARTESIAN_POINT ( 'NONE',  ( 0.5803392809272100994, 0.9991348162329892757, 1.755301537792392175 ) ) ;
#12125 = CARTESIAN_POINT ( 'NONE',  ( 1.295735140135088281, 1.957893036122235531, -0.8148005001323217478 ) ) ;
#12126 = CARTESIAN_POINT ( 'NONE',  ( -1.878313713276733132, 14.99999999999692157, -12.68000002627077905 ) ) ;
#12127 = ORIENTED_EDGE ( 'NONE', *, *, #102286, .F. ) ;
#12128 = CARTESIAN_POINT ( 'NONE',  ( -6.286140498591554326, 7.362860665558790707, 1.199719254218452047 ) ) ;
#12129 = CARTESIAN_POINT ( 'NONE',  ( 1.727181476345755806, 0.1432717513335572956, -1.855521175285803182 ) ) ;
#12130 = CARTESIAN_POINT ( 'NONE',  ( 3.357615597678655917, 7.068968630600412695, 0.7998128361456321445 ) ) ;
#12131 = CARTESIAN_POINT ( 'NONE',  ( 0.9190830904215805397, 1.997680973563022544, 0.8264451868333838602 ) ) ;
#12132 = CARTESIAN_POINT ( 'NONE',  ( 6.592432824109000222, -0.4393352932590722792, 1.975308225066509049 ) ) ;
#12133 = VERTEX_POINT ( 'NONE', #109950 ) ;
#12134 = VERTEX_POINT ( 'NONE', #206297 ) ;
#12135 = CARTESIAN_POINT ( 'NONE',  ( -9.378489572351046633, 11.96465713920816043, -1.599625672291263179 ) ) ;
#12136 = CARTESIAN_POINT ( 'NONE',  ( 3.510199737632841543, -0.7410081052188906003, -1.668730646197075673 ) ) ;
#12139 = EDGE_LOOP ( 'NONE', ( #143365, #194864, #17986, #174081, #45867, #151216, #71902, #109574 ) ) ;
#12138 = CARTESIAN_POINT ( 'NONE',  ( -4.764280463835226520, 6.994423760310605864, -1.426210198329436851 ) ) ;
#12137 = CARTESIAN_POINT ( 'NONE',  ( -3.644109427023046521, 7.473487774827342278, 0.000000000000000000 ) ) ;
#12140 = CARTESIAN_POINT ( 'NONE',  ( 6.597622414017595638, 6.771646741010207471, 0.1687998040609314243 ) ) ;
#12141 = CARTESIAN_POINT ( 'NONE',  ( 6.134138708105167481, 0.1511139231759016377, -2.010518800921741622 ) ) ;
#12142 = CARTESIAN_POINT ( 'NONE',  ( 5.824118960990139371, 1.775556191179916699, 0.4867722729226392486 ) ) ;
#12143 = CARTESIAN_POINT ( 'NONE',  ( -0.6170404364503389028, 3.500000000000003109, 1.902435570468863801 ) ) ;
#12144 = CARTESIAN_POINT ( 'NONE',  ( 4.442184936073533486, 0.9892916563519343898, -2.085014998049372625 ) ) ;
#12145 = CARTESIAN_POINT ( 'NONE',  ( 6.042093733545556233, 7.078139439671806699, -1.199719254218452047 ) ) ;
#12146 = CARTESIAN_POINT ( 'NONE',  ( 6.098930168602409552, 1.771044849343451633, -1.239067683784184970 ) ) ;
#12147 = CARTESIAN_POINT ( 'NONE',  ( 5.957918438201454059, 9.038323046955323292, -1.199719254218440723 ) ) ;
#12148 = CARTESIAN_POINT ( 'NONE',  ( 1.716251783418326848, 1.812799857666002934, 0.6971432602522424915 ) ) ;
#12149 = VERTEX_POINT ( 'NONE', #205215 ) ;
#12150 = ADVANCED_FACE ( 'NONE', ( #40626 ), #139185, .F. ) ;
#12151 = CARTESIAN_POINT ( 'NONE',  ( 4.341395233127314235, -1.327617041990782010, 1.876015773706960932 ) ) ;
#12153 = STYLED_ITEM ( 'NONE', ( #181723 ), #119978 ) ;
#12152 = CARTESIAN_POINT ( 'NONE',  ( -4.004454267989906668, 5.765225627445230927, 1.599625672291270506 ) ) ;
#12154 = CARTESIAN_POINT ( 'NONE',  ( 4.979306205331720747, 1.745251617482036943, -0.6738592683939447214 ) ) ;
#12155 = ORIENTED_EDGE ( 'NONE', *, *, #31143, .T. ) ;
#12156 = AXIS2_PLACEMENT_3D ( 'NONE', #120248, #134330, #152673 ) ;
#12159 = CARTESIAN_POINT ( 'NONE',  ( -6.459533842268148973, 6.500820668926428958, 0.000000000000000000 ) ) ;
#12158 = CARTESIAN_POINT ( 'NONE',  ( -1.500000000000013101, 0.2020833340161521663, 0.8660254037844403729 ) ) ;
#12157 = CARTESIAN_POINT ( 'NONE',  ( 2.250135261179100343, 0.8981609309555339538, -1.688322754368525747 ) ) ;
#12160 = CARTESIAN_POINT ( 'NONE',  ( 4.371826309796801979, 2.140994599346605742, -0.5347268394074317088 ) ) ;
#12161 = CARTESIAN_POINT ( 'NONE',  ( -4.115954692286631023, 7.559005856764831499, 0.7081028429081294151 ) ) ;
#12162 = CARTESIAN_POINT ( 'NONE',  ( -3.629765072269336201, 7.456752694281346905, -0.3535274064819134421 ) ) ;
#12163 = CARTESIAN_POINT ( 'NONE',  ( 5.763624699140868834, 7.817591130454727200, -1.443375672974078761 ) ) ;
#12164 = CARTESIAN_POINT ( 'NONE',  ( -6.631346530415505036, 7.869564052640446228, 1.082531754730549078 ) ) ;
#12165 = CARTESIAN_POINT ( 'NONE',  ( 1.932829124449897851, 0.1894527445373411501, 1.962211987329742113 ) ) ;
#12166 = CARTESIAN_POINT ( 'NONE',  ( 1.729934149615200312, -2.172323606337727142, 0.7788181121253530126 ) ) ;
#12167 = CARTESIAN_POINT ( 'NONE',  ( 2.558977423257744022, 1.577441344615847951, -1.166261179026031325 ) ) ;
#12168 = CARTESIAN_POINT ( 'NONE',  ( -4.288121723672178476, 8.224835454251337552, -0.7998128361456361413 ) ) ;
#12169 = CARTESIAN_POINT ( 'NONE',  ( 5.752800572348735209, -0.4956410525326099270, -2.002042340502646844 ) ) ;
#12170 = CARTESIAN_POINT ( 'NONE',  ( 5.016153647376205171, 6.875265226737464985, 1.443375672974062551 ) ) ;
#12171 = CARTESIAN_POINT ( 'NONE',  ( 4.366607992053101128, 7.252070536440704096, -1.199719254218448494 ) ) ;
#12172 = VERTEX_POINT ( 'NONE', #175960 ) ;
#12173 = LINE ( 'NONE', #128164, #133224 ) ;
#12174 = DIRECTION ( 'NONE',  ( -0.000000000000000000, -1.000000000000000000, -0.000000000000000000 ) ) ;
#12175 = CARTESIAN_POINT ( 'NONE',  ( 2.345197385039651472, 5.679888015947478941, -0.7216878364870267237 ) ) ;
#12176 = CARTESIAN_POINT ( 'NONE',  ( 2.448294946665624749, -0.9317531996627312907, 1.961122280359078873 ) ) ;
#12177 = CARTESIAN_POINT ( 'NONE',  ( 6.554440917563796987, 6.611545590104705994, -0.7998128361456481317 ) ) ;
#12178 = CARTESIAN_POINT ( 'NONE',  ( 11.34781316621058167, 4.021557182957059773, -3.687128006873058972 ) ) ;
#12179 = CARTESIAN_POINT ( 'NONE',  ( 0.2999999999999981570, 4.050057683544640241, 0.8916696671245876171 ) ) ;
#12180 = CARTESIAN_POINT ( 'NONE',  ( 2.776451973220807279, -1.788819259240326698, -0.5467896145717602296 ) ) ;
#12181 = CARTESIAN_POINT ( 'NONE',  ( 6.432923066502826082, 0.2047513753351773436, 2.151863363619124225 ) ) ;
#12183 = CARTESIAN_POINT ( 'NONE',  ( 6.827182134110205247, 0.5943742033862747798, 1.864010940340610212 ) ) ;
#12182 = CARTESIAN_POINT ( 'NONE',  ( -0.02244404828157658613, -0.004869073801674199918, -2.189079685368473527 ) ) ;
#12184 = CARTESIAN_POINT ( 'NONE',  ( 1.364683531249986537, -0.5947916663252456049, -0.7879004041258309554 ) ) ;
#12185 = CARTESIAN_POINT ( 'NONE',  ( 2.297387027313551489, 1.747684631587187232, -0.7765785915121098393 ) ) ;
#12186 = CARTESIAN_POINT ( 'NONE',  ( 4.399107752292472640, 1.421951945714538867, 1.053510053677222613 ) ) ;
#12187 = CIRCLE ( 'NONE', #39884, 0.5000000000000013323 ) ;
#12188 = CARTESIAN_POINT ( 'NONE',  ( 1.594246750649646494, -1.022002606473694675, 1.616071880676916317 ) ) ;
#12189 = CARTESIAN_POINT ( 'NONE',  ( -5.148345644887285744, 7.029489223833707001, -1.599625672291256295 ) ) ;
#12191 = CARTESIAN_POINT ( 'NONE',  ( 5.255460224911852052, 1.844849436727209469, -0.5155117042133209315 ) ) ;
#12190 = CARTESIAN_POINT ( 'NONE',  ( 7.728718841570989539, -6.124285368609183600, -7.728718841571019738 ) ) ;
#12192 = CARTESIAN_POINT ( 'NONE',  ( 1.499999999999987566, 0.02500000000001806333, 0.000000000000000000 ) ) ;
#12193 = CARTESIAN_POINT ( 'NONE',  ( 6.830521637698823589, -1.212721230272953754, 1.552361911452035503 ) ) ;
#12194 = CARTESIAN_POINT ( 'NONE',  ( -1.500000000000011324, 5.670833333333358262, 0.8660254037844403729 ) ) ;
#12195 = CARTESIAN_POINT ( 'NONE',  ( 5.346441918567009566, 7.700601260040275342, -1.357055567468886670 ) ) ;
#12196 = CARTESIAN_POINT ( 'NONE',  ( 5.612129163471575310, -0.8422657237196762292, -1.670366365510121742 ) ) ;
#12197 = CARTESIAN_POINT ( 'NONE',  ( 1.910518402784128433, 1.353611321597010253, -1.225282022559864625 ) ) ;
#12199 = CARTESIAN_POINT ( 'NONE',  ( 4.633164669693822901, 8.325607986553848150, 0.3865003237762173471 ) ) ;
#12198 = CARTESIAN_POINT ( 'NONE',  ( 4.037865812933420173, -1.521084700717803884, -1.599171214764223636 ) ) ;
#12200 = CARTESIAN_POINT ( 'NONE',  ( 1.364683531249986537, -0.8447916663252468261, -0.7879004041258309554 ) ) ;
#12201 = CARTESIAN_POINT ( 'NONE',  ( 2.471201797017197777, 1.841352583063287529, 0.9297268146766042296 ) ) ;
#12202 = CARTESIAN_POINT ( 'NONE',  ( -7.395082721250053837, 10.71501471051202614, -1.199719254218446718 ) ) ;
#12203 = CARTESIAN_POINT ( 'NONE',  ( 1.500267808745624709, 3.349173475877287753, 0.06648599600050619784 ) ) ;
#12204 = PRESENTATION_LAYER_ASSIGNMENT (  '', '', ( #105616 ) ) ;
#12205 = CARTESIAN_POINT ( 'NONE',  ( 5.508355548902068577, 9.648441583686274470, 0.7998128361456331437 ) ) ;
#12206 = ORIENTED_EDGE ( 'NONE', *, *, #201199, .F. ) ;
#12207 = CARTESIAN_POINT ( 'NONE',  ( 5.389151899530504330, 0.1487064154041470299, 2.065066873896327593 ) ) ;
#12208 = CARTESIAN_POINT ( 'NONE',  ( 1.364683531249986537, 0.2177083336747502595, -0.7879004041258309554 ) ) ;
#12209 = CARTESIAN_POINT ( 'NONE',  ( 2.794378387653595475, -2.155598273342887339, -0.1620501260681943834 ) ) ;
#12210 = CARTESIAN_POINT ( 'NONE',  ( -5.000347810418038996, 7.933946187056884369, 1.064693650161437022 ) ) ;
#12211 = CARTESIAN_POINT ( 'NONE',  ( 3.299477536675638145, 1.824990673169521793, -0.8654797531507262276 ) ) ;
#12212 = CARTESIAN_POINT ( 'NONE',  ( -4.907894938888499148, 6.474487383728022571, 2.499999999999999112 ) ) ;
#12213 = ORIENTED_EDGE ( 'NONE', *, *, #178173, .T. ) ;
#12215 = CARTESIAN_POINT ( 'NONE',  ( 7.293923454472080792, 9.532663335016016148, 1.443375672974076540 ) ) ;
#12214 = CARTESIAN_POINT ( 'NONE',  ( 3.475000000000000533, -1.924999999999999600, 0.000000000000000000 ) ) ;
#12216 = CARTESIAN_POINT ( 'NONE',  ( -7.608060475923978494, 8.905100639113307182, 1.199719254218452047 ) ) ;
#12217 = CARTESIAN_POINT ( 'NONE',  ( 0.7961116948485976730, -0.9110139862544311962, -1.799120828532501326 ) ) ;
#12218 = CARTESIAN_POINT ( 'NONE',  ( 5.724229345562060089, 2.111793275502030554, 0.5857118945327836057 ) ) ;
#12219 = CARTESIAN_POINT ( 'NONE',  ( -0.7500000000000215383, 4.222916667349481123, 1.299038105676671107 ) ) ;
#12220 = CARTESIAN_POINT ( 'NONE',  ( 4.552931727387078631, 0.3324577288378940954, 1.883125075537089854 ) ) ;
#12221 = CARTESIAN_POINT ( 'NONE',  ( -3.079673448598517549, 6.744702790006905424, 1.040834085586084257E-14 ) ) ;
#12222 = CARTESIAN_POINT ( 'NONE',  ( 7.104109303436412226, 7.390475063538369582, 1.040834085586084257E-14 ) ) ;
#12224 = CARTESIAN_POINT ( 'NONE',  ( 2.935172905452135161, -1.650095542580119812, -1.158671029019647358 ) ) ;
#12223 = CARTESIAN_POINT ( 'NONE',  ( -7.958272981097355370, 12.22847621134819285, 0.7216878364870458196 ) ) ;
#12225 = CARTESIAN_POINT ( 'NONE',  ( 1.364683531249996529, 13.52604166700806587, 0.7879004041258405033 ) ) ;
#12226 = CARTESIAN_POINT ( 'NONE',  ( -7.587723245503481095, 8.881373870289390737, 1.199719254218452047 ) ) ;
#12227 = CARTESIAN_POINT ( 'NONE',  ( 4.858271033065001632, 0.6623171007707692182, 1.592740567422048947 ) ) ;
#12228 = CARTESIAN_POINT ( 'NONE',  ( 7.550965208168244125, 7.774157262476569130, -0.7998128361456341429 ) ) ;
#12229 = CARTESIAN_POINT ( 'NONE',  ( 9.897088948295943212, 11.60932053017587506, 1.082531754730548412 ) ) ;
#12230 = FACE_OUTER_BOUND ( 'NONE', #214105, .T. ) ;
#12231 = CARTESIAN_POINT ( 'NONE',  ( 2.378026000468616452, 5.267601517901375097, 0.8449283794987967333 ) ) ;
#12232 = CARTESIAN_POINT ( 'NONE',  ( 0.6024989291013755910, 2.064475859885641640, 0.1558578049991043990 ) ) ;
#12233 = CARTESIAN_POINT ( 'NONE',  ( 6.830528382861658088, -1.277203763263988101, 1.630111558092485868 ) ) ;
#12234 = VERTEX_POINT ( 'NONE', #124087 ) ;
#12235 = CARTESIAN_POINT ( 'NONE',  ( 6.217428747564047065, 1.510149904227086504, 1.000116013982331076 ) ) ;
#12236 = CARTESIAN_POINT ( 'NONE',  ( 5.611095471209277541, 7.639640364534566075, 1.599625672291268286 ) ) ;
#12237 = DIRECTION ( 'NONE',  ( 0.3162277660168373861, -0.9486832980505139901, 0.000000000000000000 ) ) ;
#12238 = CARTESIAN_POINT ( 'NONE',  ( 6.059207019112636594, -1.526464042762348594, 0.9750640111952106892 ) ) ;
#12239 = CARTESIAN_POINT ( 'NONE',  ( 4.692530563661249765, 8.488719734331187539, 0.000000000000000000 ) ) ;
#12240 = CARTESIAN_POINT ( 'NONE',  ( 11.99957350801783562, 7.640677523568208507, 0.4513943822151063046 ) ) ;
#12241 = CARTESIAN_POINT ( 'NONE',  ( 3.047022719409075986, -1.791863632763015968, -1.261349808265788797 ) ) ;
#12242 = ORIENTED_EDGE ( 'NONE', *, *, #7783, .T. ) ;
#12244 = CARTESIAN_POINT ( 'NONE',  ( 7.889955328148847258, 11.29236608522730911, -1.199719254218446718 ) ) ;
#12243 = CARTESIAN_POINT ( 'NONE',  ( 1.064813361795993618, 1.487921858168140377, -1.278797858372302088 ) ) ;
#12245 = CARTESIAN_POINT ( 'NONE',  ( 5.448823958578076443, -1.733895640293681373, -0.8146214837579464074 ) ) ;
#12246 = FACE_OUTER_BOUND ( 'NONE', #86439, .T. ) ;
#12247 = CARTESIAN_POINT ( 'NONE',  ( -6.378792857440260811, 6.837131066116997502, 0.5844455422965456615 ) ) ;
#12248 = FILL_AREA_STYLE_COLOUR ( '', #108722 ) ;
#12249 = CARTESIAN_POINT ( 'NONE',  ( -1.402160292154681736E-14, -0.1781249996585796136, 1.575800808251672791 ) ) ;
#12251 = ORIENTED_EDGE ( 'NONE', *, *, #442, .T. ) ;
#12250 = CARTESIAN_POINT ( 'NONE',  ( 4.636525346193557162, 7.392734756325715750, -1.082531754730549078 ) ) ;
#12252 = CARTESIAN_POINT ( 'NONE',  ( -8.432808358020034589, 10.86136238915529084, 1.443375672974064550 ) ) ;
#12253 = CARTESIAN_POINT ( 'NONE',  ( 1.956163130892615731, 2.155914767609674598, -0.1587918856347721730 ) ) ;
#12254 = CARTESIAN_POINT ( 'NONE',  ( -3.634467696915153034, 6.397906858779740524, 1.199719254218452935 ) ) ;
#12255 = CARTESIAN_POINT ( 'NONE',  ( 5.560252395380198998, 9.501061871336672127, 0.7216878364870317197 ) ) ;
#12256 = CARTESIAN_POINT ( 'NONE',  ( 2.115964440355810439, -0.8579360106165806465, -1.611413330227830176 ) ) ;
#12257 = CARTESIAN_POINT ( 'NONE',  ( -0.2104748580754166598, -0.006608320950483163522, -2.103482951484026753 ) ) ;
#12258 = CARTESIAN_POINT ( 'NONE',  ( 4.911078036072877850, 1.588895129109271442, 0.8988584441092376531 ) ) ;
#12259 = CARTESIAN_POINT ( 'NONE',  ( 9.742269887272128059, 13.15996534559037912, -8.088430353861673083 ) ) ;
#12260 = VERTEX_POINT ( 'NONE', #11293 ) ;
#12261 = CARTESIAN_POINT ( 'NONE',  ( 3.543367420142525148, 1.781686863328624026, -0.8397465311346365979 ) ) ;
#12262 = ORIENTED_EDGE ( 'NONE', *, *, #30664, .T. ) ;
#12263 = CARTESIAN_POINT ( 'NONE',  ( 6.198774611348529362, 1.617120784385807974, 1.075137550886333004 ) ) ;
#12264 = VERTEX_POINT ( 'NONE', #173837 ) ;
#12265 = CARTESIAN_POINT ( 'NONE',  ( -6.720001414228860881, 7.869031733802326123, -1.199719254218452047 ) ) ;
#12267 = CARTESIAN_POINT ( 'NONE',  ( 7.008396152629535081, -6.708819892820519826, -6.400381488218290116 ) ) ;
#12266 = CARTESIAN_POINT ( 'NONE',  ( -4.288121723672178476, 8.224835454251337552, -0.7998128361456362523 ) ) ;
#12269 = ADVANCED_FACE ( 'NONE', ( #56857 ), #158705, .F. ) ;
#12268 = CARTESIAN_POINT ( 'NONE',  ( 5.994113310573177422, 10.00723293906178846, 0.000000000000000000 ) ) ;
#12270 = CARTESIAN_POINT ( 'NONE',  ( 3.545477442914763078, -1.765841875850767906, 0.7343832577718923948 ) ) ;
#12271 = CARTESIAN_POINT ( 'NONE',  ( 4.675513026854819287, 7.080785086760167601, -1.371149936167876282 ) ) ;
#12272 = DIRECTION ( 'NONE',  ( -0.6507913734559630514, -0.7592566023653011253, 0.000000000000000000 ) ) ;
#12273 = CARTESIAN_POINT ( 'NONE',  ( 0.1478802723770406002, -1.707511933842900564, -1.397569297917726550 ) ) ;
#12274 = CARTESIAN_POINT ( 'NONE',  ( 4.863935948449842783, 0.6292040250746065988, -1.912316011988722586 ) ) ;
#12275 = CARTESIAN_POINT ( 'NONE',  ( 0.08865135991732026044, -9.916958638733639475, 9.499586356067553083 ) ) ;
#12276 = CARTESIAN_POINT ( 'NONE',  ( 6.393173274427864428, 1.585754722747900969, -0.9045919592586546543 ) ) ;
#12277 = CARTESIAN_POINT ( 'NONE',  ( 0.5552397518338060278, 1.722184604005328357, -1.148819969904082861 ) ) ;
#12278 = CARTESIAN_POINT ( 'NONE',  ( -7.619319141200077361, 9.912291636198670375, 1.443375672974090751 ) ) ;
#12279 = CARTESIAN_POINT ( 'NONE',  ( -5.917914848013369422, 7.154962168230770025, -1.123475595150375650 ) ) ;
#12280 = DIRECTION ( 'NONE',  ( -0.8002608041566210417, 0.5996521035822340862, 0.000000000000000000 ) ) ;
#12281 = CARTESIAN_POINT ( 'NONE',  ( 3.285556943750000514, -3.113541666188709645, 1.896917185911906722 ) ) ;
#12282 = CARTESIAN_POINT ( 'NONE',  ( 7.284808609244363353, 7.393364887073558656, 0.7998128361456341429 ) ) ;
#12283 = CARTESIAN_POINT ( 'NONE',  ( 1.364683531249997417, 11.54687500034139802, 2.602085213965210642E-15 ) ) ;
#12284 = CARTESIAN_POINT ( 'NONE',  ( -5.447678794592645701, 5.250046769979851646, 0.000000000000000000 ) ) ;
#12286 = CARTESIAN_POINT ( 'NONE',  ( -7.282664789195997912, 8.525472337930658284, 1.199719254218452047 ) ) ;
#12285 = CARTESIAN_POINT ( 'NONE',  ( -5.000000000000000888, 0.2350621082554960051, -0.7749999999999935829 ) ) ;
#12287 = CARTESIAN_POINT ( 'NONE',  ( 4.078545790824074757, -0.6587176911285116399, 1.604389539659875297 ) ) ;
#12288 = CARTESIAN_POINT ( 'NONE',  ( -5.752737250900127997, 5.605948302338584099, 0.000000000000000000 ) ) ;
#12289 = CARTESIAN_POINT ( 'NONE',  ( 1.569279613544020568, 1.823957739939351619, 0.9794188589333228112 ) ) ;
#12290 = EDGE_CURVE ( 'NONE', #7674, #49203, #193677, .T. ) ;
#12291 = CARTESIAN_POINT ( 'NONE',  ( 2.109133483290903222, 0.003435389629122351501, 2.117403154539731602 ) ) ;
#12292 = CARTESIAN_POINT ( 'NONE',  ( 4.059776932288224671, 6.823824623389866950, 1.199719254218462483 ) ) ;
#12293 = CARTESIAN_POINT ( 'NONE',  ( 9.088043039861931405, 9.497138389460751284, 1.040834085586084257E-14 ) ) ;
#12294 = CARTESIAN_POINT ( 'NONE',  ( 4.650083499807233345, 5.295740330745369207, -7.499999999999997335 ) ) ;
#12295 = CARTESIAN_POINT ( 'NONE',  ( 0.4441182907778543631, -0.9332952320128800050, 1.734295555568473368 ) ) ;
#12296 = CARTESIAN_POINT ( 'NONE',  ( 5.132834705836428313, 6.694876404991986441, 1.408819685294822932 ) ) ;
#12297 = CARTESIAN_POINT ( 'NONE',  ( 3.687454593236936251, 7.245854758844324728, -0.7216878364870267237 ) ) ;
#12299 = DIRECTION ( 'NONE',  ( -8.638326563840809144E-31, -5.962633348652903386E-61, 1.000000000000000000 ) ) ;
#12298 = CARTESIAN_POINT ( 'NONE',  ( 3.475000000000000533, -0.8750000000000007772, 0.000000000000000000 ) ) ;
#12300 = CARTESIAN_POINT ( 'NONE',  ( 2.537429240164018385, -1.699656577751871289, -1.538240582240576693 ) ) ;
#12301 = CARTESIAN_POINT ( 'NONE',  ( 1.119449510670032177, -1.781678707675336870, 0.3977030049751931196 ) ) ;
#12302 = CARTESIAN_POINT ( 'NONE',  ( 3.023589307540079041, -0.3687504995396119201, 1.876329818327879817 ) ) ;
#12303 = CARTESIAN_POINT ( 'NONE',  ( 4.532168488718122390, 8.509556680138327778, 0.7998128361456271485 ) ) ;
#12304 = CARTESIAN_POINT ( 'NONE',  ( 7.104109303436412226, 7.390475063538369582, 1.040834085586084257E-14 ) ) ;
#12305 = CARTESIAN_POINT ( 'NONE',  ( -8.296699936558862731, 11.76690146170562201, 1.199719254218453823 ) ) ;
#12306 = CARTESIAN_POINT ( 'NONE',  ( 2.074478728756317114, 0.8647236062047275462, 1.818190761793165189 ) ) ;
#12307 = CARTESIAN_POINT ( 'NONE',  ( 1.709737484509077365, 0.5745576563440238926, -1.875703277996950469 ) ) ;
#12308 = CARTESIAN_POINT ( 'NONE',  ( -9.429859533504656000, 10.96025652963230534, -1.199719254218441611 ) ) ;
#12309 = CARTESIAN_POINT ( 'NONE',  ( -6.042130013184518589, 10.20090211535728031, -0.7998128361456291469 ) ) ;
#12310 = CARTESIAN_POINT ( 'NONE',  ( -7.657759090810044356, -5.412329794880681888, -7.842350841322879518 ) ) ;
#12312 = CARTESIAN_POINT ( 'NONE',  ( 2.940057854958120220, 1.756256042272446694, 0.2183286820098342407 ) ) ;
#12311 = CARTESIAN_POINT ( 'NONE',  ( 4.681631697639319079, -0.9857103537862299536, 1.843662662672640007 ) ) ;
#12313 = CARTESIAN_POINT ( 'NONE',  ( -7.247736482493067456, 14.00000000000182254, 10.57961706324693019 ) ) ;
#12315 = CARTESIAN_POINT ( 'NONE',  ( 0.006183538434290089709, -0.9405624870862170361, -1.977291442860461768 ) ) ;
#12314 = CARTESIAN_POINT ( 'NONE',  ( 1.566565198595117892, 8.754658464387805594, -2.463935442259830744 ) ) ;
#12316 = CARTESIAN_POINT ( 'NONE',  ( 4.136439897933008147, -1.512742658674090857, 0.8602829033797516622 ) ) ;
#12317 = CARTESIAN_POINT ( 'NONE',  ( 9.185812768458653466, 10.67553530374532045, 1.199719254218453823 ) ) ;
#12318 = CARTESIAN_POINT ( 'NONE',  ( -0.1104750535120268551, 0.2303756098476944791, -2.137063993957021513 ) ) ;
#12319 = CARTESIAN_POINT ( 'NONE',  ( 4.112396791320716005, 0.5851491843551993588, -1.632232688200731197 ) ) ;
#12320 = CARTESIAN_POINT ( 'NONE',  ( 4.176368576274028577, -1.112882343535037677, -1.864130199707826785 ) ) ;
#12321 = CARTESIAN_POINT ( 'NONE',  ( 3.171717870593107058, 5.787755718078879674, -1.199719254218446718 ) ) ;
#12322 = CARTESIAN_POINT ( 'NONE',  ( 0.3568547849697421004, -1.996003273109921983, -0.7069239421778094057 ) ) ;
#12324 = VECTOR ( 'NONE', #175241, 1000.000000000000000 ) ;
#12323 = CARTESIAN_POINT ( 'NONE',  ( 6.218749999999983125, -0.7852924748301916003, 1.895863743164212467 ) ) ;
#12325 = CARTESIAN_POINT ( 'NONE',  ( 1.499999999999990896, 5.306250000682820378, 1.214306433183764966E-14 ) ) ;
#12326 = CARTESIAN_POINT ( 'NONE',  ( 3.803666480526507687, -0.5600534170543782775, 1.843171563392527856 ) ) ;
#12327 = CARTESIAN_POINT ( 'NONE',  ( 0.7500000000000006661, 9.614583334016129967, 1.299038105676657340 ) ) ;
#12328 = CARTESIAN_POINT ( 'NONE',  ( 0.6104036325267605534, -0.7939654203579590286, 2.074740863049700845 ) ) ;
#12329 = VERTEX_POINT ( 'NONE', #153044 ) ;
#12330 = CARTESIAN_POINT ( 'NONE',  ( 6.883263157960333167, 4.698395927207251077, 2.408847447403542841 ) ) ;
#12331 = CARTESIAN_POINT ( 'NONE',  ( -1.500000000000011324, 3.420833333333355597, 0.8660254037844403729 ) ) ;
#12332 = CARTESIAN_POINT ( 'NONE',  ( 6.972971076130050072, 7.029554431773520129, 1.040834085586084257E-14 ) ) ;
#12333 = CARTESIAN_POINT ( 'NONE',  ( 2.420824200137431603, -0.8528996238171372424, -2.051222908810364842 ) ) ;
#12334 = CARTESIAN_POINT ( 'NONE',  ( 11.78331023100045627, 11.29999999999998117, 1.799999999999999600 ) ) ;
#12335 = CARTESIAN_POINT ( 'NONE',  ( 7.619319141200070256, 8.951922421897323900, 1.082531754730558626 ) ) ;
#12336 = CARTESIAN_POINT ( 'NONE',  ( -8.785320351530977234, 13.19336481018743079, 1.040834085586084257E-14 ) ) ;
#12337 = CARTESIAN_POINT ( 'NONE',  ( 4.740510986633625024, 5.559626234941203116, -1.199719254218450271 ) ) ;
#12338 = MECHANICAL_DESIGN_GEOMETRIC_PRESENTATION_REPRESENTATION (  '', ( #88444 ), #57349 ) ;
#12339 = CARTESIAN_POINT ( 'NONE',  ( 0.8443752267504719411, 0.3905955241953715795, -1.978051186352240309 ) ) ;
#12341 = CARTESIAN_POINT ( 'NONE',  ( 5.898899852458296955, 0.3987951208904988443, 2.023601990196000955 ) ) ;
#12340 = CARTESIAN_POINT ( 'NONE',  ( 7.214910300766615769, 11.56914578420308715, -0.7998128361456291469 ) ) ;
#12342 = PLANE ( 'NONE',  #213339 ) ;
#12343 = CARTESIAN_POINT ( 'NONE',  ( -3.307299406729781399, 5.945934176904983381, -1.199719254218452935 ) ) ;
#12344 = CARTESIAN_POINT ( 'NONE',  ( -0.7499999999999972244, 4.889583334016150751, -1.299038105676652899 ) ) ;
#12345 = CARTESIAN_POINT ( 'NONE',  ( -1.402160292154681736E-14, 0.6968750003414164729, -1.575800808251659024 ) ) ;
#12346 = CARTESIAN_POINT ( 'NONE',  ( 0.8074156707096367125, -1.761990802586909766, 0.1653023320123351292 ) ) ;
#12347 = CARTESIAN_POINT ( 'NONE',  ( 6.381516696256908538, -0.4728550111133908995, -1.668365442416564814 ) ) ;
#12348 = CARTESIAN_POINT ( 'NONE',  ( 5.671390581117805141, 1.043574818874394294, 1.392714124641497131 ) ) ;
#12349 = CARTESIAN_POINT ( 'NONE',  ( 2.490095330609965796, -2.286454923436448183, -0.1652806634409968445 ) ) ;
#12350 = CARTESIAN_POINT ( 'NONE',  ( -1.364683531250014514, -0.2614583329919080157, -0.7879004041258359514 ) ) ;
#12351 = CARTESIAN_POINT ( 'NONE',  ( 1.605144257462550517, -1.827384369528777031, 0.2241066044648756805 ) ) ;
#12352 = AXIS2_PLACEMENT_3D ( 'NONE', #49112, #199592, #181222 ) ;
#12353 = FACE_BOUND ( 'NONE', #150257, .T. ) ;
#12354 = CARTESIAN_POINT ( 'NONE',  ( 2.063248287022978467, 0.3151258922809499485, -1.798016661460503984 ) ) ;
#12355 = CARTESIAN_POINT ( 'NONE',  ( 2.936172824561166905, -1.650081981912490336, -1.158688413653415239 ) ) ;
#12356 = CARTESIAN_POINT ( 'NONE',  ( -3.375617059678305054, 5.921675088724528635, 1.082531754730560403 ) ) ;
#12357 = CARTESIAN_POINT ( 'NONE',  ( 1.060776890969020059, -1.982532595227912475, -0.9341070725938580566 ) ) ;
#12358 = CARTESIAN_POINT ( 'NONE',  ( 8.724581073908543871, 13.71543862355972188, -7.774732811725550974 ) ) ;
#12359 = CARTESIAN_POINT ( 'NONE',  ( 4.208114709606614490, -2.100488694582537619, 0.1524824656061254391 ) ) ;
#12360 = CARTESIAN_POINT ( 'NONE',  ( -7.549192604710863286, 7.701812881784464437, -0.7998128361456291469 ) ) ;
#12361 = CARTESIAN_POINT ( 'NONE',  ( 7.210140354588870260, 13.96302891847841998, 9.188013455993196743 ) ) ;
#12362 = CARTESIAN_POINT ( 'NONE',  ( 1.504437137538238600, 2.067909592606699487, 0.1035681241481553605 ) ) ;
#12363 = CARTESIAN_POINT ( 'NONE',  ( 5.515469562660962666, 5.329135999392899947, 0.7998128361456341429 ) ) ;
#12364 = CARTESIAN_POINT ( 'NONE',  ( -1.360316468750048635, -0.5989583329919208055, -0.7853790794159082322 ) ) ;
#12365 = CARTESIAN_POINT ( 'NONE',  ( 4.547591073264711348, -1.938359017324686961, 0.8602097090630379528 ) ) ;
#12366 = CONTEXT_DEPENDENT_SHAPE_REPRESENTATION ( #166759, #130326 ) ;
#12367 = CARTESIAN_POINT ( 'NONE',  ( 6.568987803155795113, -1.671525225137669102, -0.7347104647430282576 ) ) ;
#12368 = EDGE_LOOP ( 'NONE', ( #184683, #94107, #112603, #60116 ) ) ;
#12369 = CARTESIAN_POINT ( 'NONE',  ( -4.145761110728687804, 8.058748072483927771, -0.7998128361456481317 ) ) ;
#12370 = CARTESIAN_POINT ( 'NONE',  ( 10.07387183015377197, 11.71160420905630062, -1.199719254218440723 ) ) ;
#12371 = CARTESIAN_POINT ( 'NONE',  ( 7.309254211098767051, 7.700087132469628948, 0.7216878364870267237 ) ) ;
#12372 = CARTESIAN_POINT ( 'NONE',  ( -1.737500000000000266, -1.764583332377417380, -3.009438278150923907 ) ) ;
#12373 = CARTESIAN_POINT ( 'NONE',  ( -5.555090253297260361, 7.504024600312024340, 1.599625672291269396 ) ) ;
#12374 = CARTESIAN_POINT ( 'NONE',  ( -0.06965283525045895541, -2.176852707449424607, 0.4419662969857121038 ) ) ;
#12375 = CARTESIAN_POINT ( 'NONE',  ( 1.360533241671294746, 0.8531190763820644118, 1.925603555557230617 ) ) ;
#12376 = CARTESIAN_POINT ( 'NONE',  ( -4.817943484809863008, 6.714296380401858499, 1.599625672291263179 ) ) ;
#12377 = CARTESIAN_POINT ( 'NONE',  ( 9.399880572976245574, 9.860948844760784482, 0.7998128361456462443 ) ) ;
#12378 = CARTESIAN_POINT ( 'NONE',  ( 4.750749981963457991, -0.4049220142380467458, -1.816192249911535272 ) ) ;
#12379 = CARTESIAN_POINT ( 'NONE',  ( 7.751511138711133064, 10.06651563329490529, -1.599625672291262513 ) ) ;
#12380 = CARTESIAN_POINT ( 'NONE',  ( -0.5151611981367305582, 4.156673609434548666, -0.3998388334338457972 ) ) ;
#12381 = CARTESIAN_POINT ( 'NONE',  ( -2.823841133396259639, 6.516508098929413961, -0.7998128361456481317 ) ) ;
#12382 = CARTESIAN_POINT ( 'NONE',  ( -3.789667630219657912, 4.380032642466370696, 1.199719254218462483 ) ) ;
#12383 = CARTESIAN_POINT ( 'NONE',  ( -1.808247988047325228, 2.517446015412732940, 2.499984125739859842 ) ) ;
#12384 = FACE_OUTER_BOUND ( 'NONE', #87810, .T. ) ;
#12386 = CARTESIAN_POINT ( 'NONE',  ( 2.453501617077270769, 1.514643136537169310, 1.246875331876770243 ) ) ;
#12385 = CARTESIAN_POINT ( 'NONE',  ( -6.531277313481209212, 8.642909503859968368, 1.599625672291283607 ) ) ;
#12387 = CARTESIAN_POINT ( 'NONE',  ( 0.7960496800812133511, -0.7770375076890515542, 2.017388685454111652 ) ) ;
#12389 = CARTESIAN_POINT ( 'NONE',  ( -6.024621019446552594, 6.066914679173425640, 0.6088392743194663836 ) ) ;
#12388 = CARTESIAN_POINT ( 'NONE',  ( -5.906512197408906317, 6.919960980845699439, -1.199719254218453823 ) ) ;
#12390 = CARTESIAN_POINT ( 'NONE',  ( 1.364683531249986537, -0.1364583329919154264, 0.7879004041258500513 ) ) ;
#12391 = CARTESIAN_POINT ( 'NONE',  ( 2.969770354771487320, 1.463018481607085475, 0.9301108516524180247 ) ) ;
#12392 = CARTESIAN_POINT ( 'NONE',  ( 2.571852248423611709, -1.665254919270848344, -0.5056227470447529626 ) ) ;
#12393 = CARTESIAN_POINT ( 'NONE',  ( 7.131225611108096274, 8.382479970123348778, 1.082531754730558626 ) ) ;
#12394 = CARTESIAN_POINT ( 'NONE',  ( -11.83256397649420677, 7.177290438377375459, -1.867481893931521419 ) ) ;
#12395 = ADVANCED_FACE ( 'NONE', ( #4619, #70691 ), #88045, .T. ) ;
#12396 = CARTESIAN_POINT ( 'NONE',  ( 0.9837497097957871306, 1.861730512597782550, 0.7742002051285418185 ) ) ;
#12397 = CARTESIAN_POINT ( 'NONE',  ( 6.925078400183577010, 2.950057911518182419, 2.596529392604688180 ) ) ;
#12398 = CARTESIAN_POINT ( 'NONE',  ( -4.716257332707368910, 6.595662536282280719, -1.599625672291271394 ) ) ;
#12399 = CARTESIAN_POINT ( 'NONE',  ( 1.533988556244444856, 0.9736202887896376890, -1.714215200822625684 ) ) ;
#12401 = CARTESIAN_POINT ( 'NONE',  ( -6.129694847154222970, 7.284303755502281597, -1.082531754730549967 ) ) ;
#12400 = CARTESIAN_POINT ( 'NONE',  ( 5.959226163113887864, -1.611951592244726950, 1.028742869173946861 ) ) ;
#12402 = CARTESIAN_POINT ( 'NONE',  ( -7.065207446052822249, 7.415365906582643163, -0.7216878364870338292 ) ) ;
#12403 = CARTESIAN_POINT ( 'NONE',  ( 6.821687566331318564, 7.987665577921906568, 1.199719254218452935 ) ) ;
#12404 = EDGE_CURVE ( 'NONE', #35104, #168888, #100027, .T. ) ;
#12405 = CARTESIAN_POINT ( 'NONE',  ( -6.444921918449773024, 8.612437886315108315, 1.599625672291269396 ) ) ;
#12406 = CARTESIAN_POINT ( 'NONE',  ( 1.436200859769844129, -1.123848162932556072, -1.677891559433869473 ) ) ;
#12407 = DIRECTION ( 'NONE',  ( 1.276756478318932585E-15, -1.000000000000000000, 1.665334536937738262E-16 ) ) ;
#12408 = CARTESIAN_POINT ( 'NONE',  ( 4.946439154741203659, 2.300974901101384695, 0.1755221459238848203 ) ) ;
#12409 = CARTESIAN_POINT ( 'NONE',  ( 6.355910407107248083, -0.6622273607519140182, 1.846833223631501264 ) ) ;
#12410 = CARTESIAN_POINT ( 'NONE',  ( 2.922649740298603138, -1.356309479035762378, 1.417576456850026867 ) ) ;
#12411 = CARTESIAN_POINT ( 'NONE',  ( 7.248805684800777804, 11.60869039890961218, 1.040834085586084257E-14 ) ) ;
#12412 = CARTESIAN_POINT ( 'NONE',  ( -9.568394635444461116, 15.10427918654218082, 7.242253469826407830 ) ) ;
#12413 = VERTEX_POINT ( 'NONE', #155185 ) ;
#12414 = CARTESIAN_POINT ( 'NONE',  ( 0.9720387486300664515, -0.9465246498777776241, 1.894042457640370491 ) ) ;
#12416 = CARTESIAN_POINT ( 'NONE',  ( -8.830438121202295321, 9.196599317691152464, -0.7998128361456291469 ) ) ;
#12415 = CARTESIAN_POINT ( 'NONE',  ( -5.135841261478327979, 4.886236314679810455, 0.7998128361456341429 ) ) ;
#12417 = CARTESIAN_POINT ( 'NONE',  ( 0.3394786764520755784, 1.835982197492795898, 0.1384515631646099088 ) ) ;
#12418 = ORIENTED_EDGE ( 'NONE', *, *, #20075, .F. ) ;
#12419 = CARTESIAN_POINT ( 'NONE',  ( 11.96976056191701154, 7.637744957010472291, -0.8800080678311683613 ) ) ;
#12420 = CARTESIAN_POINT ( 'NONE',  ( 3.181995841446764839, 2.068044944583770306, -0.4684364081647199307 ) ) ;
#12421 = CARTESIAN_POINT ( 'NONE',  ( -1.001543065824772872E-14, 4.243750000682819490, 1.732050807568877637 ) ) ;
#12422 = CARTESIAN_POINT ( 'NONE',  ( 9.101601193475611140, 9.512956235343358102, -0.7998128361456221525 ) ) ;
#12423 =( NAMED_UNIT ( * ) SI_UNIT ( $, .STERADIAN. ) SOLID_ANGLE_UNIT ( ) );
#12424 = CARTESIAN_POINT ( 'NONE',  ( 3.532544388643095612, 2.009728383178956523, 0.4550750861811359571 ) ) ;
#12426 = CARTESIAN_POINT ( 'NONE',  ( 0.06366010765614799061, -1.203631707120488947, 1.393476991864414760 ) ) ;
#12425 = CARTESIAN_POINT ( 'NONE',  ( -8.715193815486133033, 9.062147627688959872, 0.7998128361456462443 ) ) ;
#12427 = CARTESIAN_POINT ( 'NONE',  ( -1.201851678989727383E-14, 3.696875000341422801, -1.575800808251660134 ) ) ;
#12428 = DIRECTION ( 'NONE',  ( -0.000000000000000000, 1.000000000000000000, -0.000000000000000000 ) ) ;
#12429 = CARTESIAN_POINT ( 'NONE',  ( 1.494007359806955204, 4.332045425165421904, 0.1499524099050986436 ) ) ;
#12430 = B_SPLINE_CURVE_WITH_KNOTS ( 'NONE', 3,
 ( #41626, #71936, #172680, #106653 ),
 .UNSPECIFIED., .F., .F.,
 ( 4, 4 ),
 ( -3.662496629072134259E-08, 0.0006801242851315174049 ),
 .UNSPECIFIED. ) ;
#12431 = CARTESIAN_POINT ( 'NONE',  ( 0.5224629442122545875, -1.184049029929446828, -1.862174541895257995 ) ) ;
#12432 = CARTESIAN_POINT ( 'NONE',  ( 2.759333473672697767, -1.967098484071924558, -1.117512413888957612 ) ) ;
#12433 = CARTESIAN_POINT ( 'NONE',  ( -9.815740026613967828, 10.55404424057886636, -0.7216878364870267237 ) ) ;
#12435 = EDGE_CURVE ( 'NONE', #7968, #210693, #178891, .T. ) ;
#12434 = CARTESIAN_POINT ( 'NONE',  ( 2.373076535756658778, -1.577936908029322849, -0.8897043057118164677 ) ) ;
#12436 = CARTESIAN_POINT ( 'NONE',  ( 2.764735878068668384, -0.1456047134679704924, -1.910273805325033436 ) ) ;
#12437 = CARTESIAN_POINT ( 'NONE',  ( 3.842288295254093100, -1.023014542950370975, 1.799900136785845817 ) ) ;
#12438 = CARTESIAN_POINT ( 'NONE',  ( -1.402160292154681736E-14, 2.259375000341416140, -1.575800808251660134 ) ) ;
#12439 = CARTESIAN_POINT ( 'NONE',  ( 1.744934968351062210, -1.666494570726485991, 1.053036000364399483 ) ) ;
#12440 = CARTESIAN_POINT ( 'NONE',  ( 6.270143248794765256, 0.9928014866268529692, 1.650855525168734461 ) ) ;
#12441 = CARTESIAN_POINT ( 'NONE',  ( 2.676452114398766291, -1.789519730395791486, -0.5449050523786898026 ) ) ;
#12443 = CARTESIAN_POINT ( 'NONE',  ( 4.669458948634179762, 8.398658883068243597, -0.5498995856093937817 ) ) ;
#12442 = CARTESIAN_POINT ( 'NONE',  ( 1.665117554179825321, -1.629454703905337087, 1.634364892973801719 ) ) ;
#12444 = CARTESIAN_POINT ( 'NONE',  ( 3.068646357036347361, 1.349867735329785434, -1.281425607799644206 ) ) ;
#12445 = CARTESIAN_POINT ( 'NONE',  ( -1.201851678989727383E-14, 2.696875000341417916, -1.575800808251660134 ) ) ;
#12446 = MECHANICAL_DESIGN_GEOMETRIC_PRESENTATION_REPRESENTATION (  '', ( #64121 ), #91953 ) ;
#12447 = CARTESIAN_POINT ( 'NONE',  ( 6.021949879679938000, 2.032782779420911456, -0.3490252056354887222 ) ) ;
#12448 = CARTESIAN_POINT ( 'NONE',  ( -4.629219384062206011, 7.488174150459498968, -1.199719254218452047 ) ) ;
#12449 = CARTESIAN_POINT ( 'NONE',  ( 7.613066949273408213, 8.840665181362512115, -1.199719254218441611 ) ) ;
#12450 = CARTESIAN_POINT ( 'NONE',  ( -1.315333408008317884, 3.546208470693949621, 0.4024190470832751387 ) ) ;
#12451 =( BOUNDED_CURVE ( )  B_SPLINE_CURVE ( 2, ( #177571, #78985, #154125, #123848, #23024 ),
 .UNSPECIFIED., .F., .T. ) 
 B_SPLINE_CURVE_WITH_KNOTS ( ( 3, 2, 3 ),
 ( 0.01092446968156909545, 0.01250000000000000069, 0.01386088777671199215 ),
 .UNSPECIFIED. ) 
 CURVE ( )  GEOMETRIC_REPRESENTATION_ITEM ( )  RATIONAL_B_SPLINE_CURVE ( ( 0.9369925407309220855, 0.9493405508230827738, 1.000000000000000000, 0.9562421463088763840, 0.9410680661649857282 ) ) 
 REPRESENTATION_ITEM ( '' )  );
#12452 = CARTESIAN_POINT ( 'NONE',  ( 6.598663424749101836, -0.5579900645847408747, -2.030628608299019700 ) ) ;
#12453 = VECTOR ( 'NONE', #107570, 1000.000000000000000 ) ;
#12454 = ADVANCED_FACE ( 'NONE', ( #206049 ), #109701, .T. ) ;
#12455 = CARTESIAN_POINT ( 'NONE',  ( 0.6823417656249917140, 4.405208333674755394, 1.181850606188765695 ) ) ;
#12456 = CARTESIAN_POINT ( 'NONE',  ( 6.450466699499744827, 0.6713059571747861387, 2.054807225473152865 ) ) ;
#12457 = CARTESIAN_POINT ( 'NONE',  ( 6.410808175004245157, -0.5408338447881118061, -1.945826018873537455 ) ) ;
#12458 = CARTESIAN_POINT ( 'NONE',  ( 1.364683531249988757, 0.1343750003414204142, 0.000000000000000000 ) ) ;
#12459 = CARTESIAN_POINT ( 'NONE',  ( -4.934804725694236893, 4.859619722839116918, -0.7216878364870207285 ) ) ;
#12460 = EDGE_CURVE ( 'NONE', #141559, #71915, #153009, .T. ) ;
#12463 = CARTESIAN_POINT ( 'NONE',  ( 5.368665641331531013, 5.365790791082654998, -0.7216878364870207285 ) ) ;
#12462 = CARTESIAN_POINT ( 'NONE',  ( 6.825078400183556937, 1.302289051367941708, 1.872899343898648983 ) ) ;
#12461 = CARTESIAN_POINT ( 'NONE',  ( 6.387826650694035990, 7.481494509678370264, -1.199719254218452047 ) ) ;
#12464 = CARTESIAN_POINT ( 'NONE',  ( -5.815521545619021460, 5.749472989502435460, -0.7998128361456362523 ) ) ;
#12465 = CARTESIAN_POINT ( 'NONE',  ( 4.716029918043215474, 1.032482702726954527, -1.731993998903176957 ) ) ;
#12466 = CARTESIAN_POINT ( 'NONE',  ( -8.311311860377216476, 9.655284244316948872, -1.199719254218446718 ) ) ;
#12468 = CARTESIAN_POINT ( 'NONE',  ( -7.892254816486440561, 8.380254505421877553, 0.000000000000000000 ) ) ;
#12467 = CARTESIAN_POINT ( 'NONE',  ( -9.083599731475995753, 11.62061899152058686, 1.443375672974064550 ) ) ;
#12469 = CARTESIAN_POINT ( 'NONE',  ( 1.364683531249990311, 5.613541667008087543, 0.7879004041258500513 ) ) ;
#12471 = CARTESIAN_POINT ( 'NONE',  ( -0.6823417656250039265, 9.567708333674735499, -1.181850606188755259 ) ) ;
#12470 = CARTESIAN_POINT ( 'NONE',  ( 5.664953204072169513, -1.952404353424816774, -0.9282482345986733385 ) ) ;
#12472 = CARTESIAN_POINT ( 'NONE',  ( 10.20634067979172421, 1.972237431424189724, -5.892633538921025149 ) ) ;
#12473 = CARTESIAN_POINT ( 'NONE',  ( -11.32659722783424705, 6.354439326305993951, -3.967491859357531236 ) ) ;
#12474 = MANIFOLD_SOLID_BREP ( 'Fillet1', #43064 ) ;
#12476 = CARTESIAN_POINT ( 'NONE',  ( 6.538686444676896414, -1.556836737174282836, 1.281159629702780078 ) ) ;
#12475 = CARTESIAN_POINT ( 'NONE',  ( -6.195713011320790109, 9.211787032307496403, -1.082531754730537976 ) ) ;
#12477 = CARTESIAN_POINT ( 'NONE',  ( -1.364683531250000748, -0.9281249996585805295, 0.000000000000000000 ) ) ;
#12478 = CARTESIAN_POINT ( 'NONE',  ( 0.7500000000000006661, 8.916666666666669627, -1.299038105676657340 ) ) ;
#12479 = CARTESIAN_POINT ( 'NONE',  ( 1.541173760317329666, -1.247365581009220126, -1.191596266039594010 ) ) ;
#12480 = CARTESIAN_POINT ( 'NONE',  ( 5.820193082016415609, 10.01225203898631655, 0.000000000000000000 ) ) ;
#12481 = CARTESIAN_POINT ( 'NONE',  ( 4.355912491740495440, 8.303924683664389406, 0.000000000000000000 ) ) ;
#12482 = CARTESIAN_POINT ( 'NONE',  ( -11.90622689666433942, 8.910945625224377054, -1.226100016398791404 ) ) ;
#12483 = CARTESIAN_POINT ( 'NONE',  ( 0.5613125002107671735, 1.751697300359332798, -0.2511290008074765212 ) ) ;
#12484 = CARTESIAN_POINT ( 'NONE',  ( 1.137358842852369545, -0.04729656459989117767, 2.012689239070045488 ) ) ;
#12485 = CARTESIAN_POINT ( 'NONE',  ( -15.75000000000000000, 13.40000000000000036, -3.200000000000001510 ) ) ;
#12487 = VECTOR ( 'NONE', #136922, 1000.000000000000000 ) ;
#12486 = CARTESIAN_POINT ( 'NONE',  ( 3.610573252990852744, -0.8922430012947217826, -2.018528625508857921 ) ) ;
#12488 = CARTESIAN_POINT ( 'NONE',  ( 5.647405056649561494, 1.918175650701968937, -1.016889183816371611 ) ) ;
#12489 = EDGE_LOOP ( 'NONE', ( #157261, #153499, #210964, #130672 ) ) ;
#12490 = CARTESIAN_POINT ( 'NONE',  ( 1.499999999999987121, -0.2458333333333099502, 0.8660254037844524744 ) ) ;
#12491 = CARTESIAN_POINT ( 'NONE',  ( 7.578644679914702031, 10.82520731233375955, 1.082531754730558626 ) ) ;
#12493 = CARTESIAN_POINT ( 'NONE',  ( 3.251577527157409886, 1.966640965408305686, -0.4445242805125593222 ) ) ;
#12492 = CARTESIAN_POINT ( 'NONE',  ( 2.983181628360128013, -1.960071735995170927, -0.8095406527153580223 ) ) ;
#12495 = VERTEX_POINT ( 'NONE', #106481 ) ;
#12494 = CARTESIAN_POINT ( 'NONE',  ( 3.744242849288460295, 0.9642487561531964957, -1.533428966541541039 ) ) ;
#12496 = CARTESIAN_POINT ( 'NONE',  ( 6.658989722967328717, 7.797851427330578566, 1.199719254218452935 ) ) ;
#12497 = EDGE_LOOP ( 'NONE', ( #125717, #95681, #200545, #165254 ) ) ;
#12498 = CARTESIAN_POINT ( 'NONE',  ( 0.6197280442463182215, -0.9970892369244135356, -1.582582228963416382 ) ) ;
#12499 = CARTESIAN_POINT ( 'NONE',  ( 5.636439174979242850, 7.598931675607687453, -1.599625672291262513 ) ) ;
#12500 =( GEOMETRIC_REPRESENTATION_CONTEXT ( 3 ) GLOBAL_UNCERTAINTY_ASSIGNED_CONTEXT ( ( #135990 ) ) GLOBAL_UNIT_ASSIGNED_CONTEXT ( ( #89847, #188378, #6415 ) ) REPRESENTATION_CONTEXT ( 'NONE', 'WORKASPACE' ) );
#12502 = CARTESIAN_POINT ( 'NONE',  ( 1.481495926510235206, -0.6419399793253840469, 1.805124470068826037 ) ) ;
#12501 = CARTESIAN_POINT ( 'NONE',  ( -4.952806187693842510, 4.672695395264567786, 0.7998128361456341429 ) ) ;
#12503 = CARTESIAN_POINT ( 'NONE',  ( 1.499999999999981126, 3.504166666666683749, 0.8660254037844571373 ) ) ;
#12504 = CARTESIAN_POINT ( 'NONE',  ( 5.020596955762157698, 4.751784624677624080, 1.040834085586084257E-14 ) ) ;
#12505 = CARTESIAN_POINT ( 'NONE',  ( -1.364683531250000748, 2.071875000341422357, 1.214306433183764966E-14 ) ) ;
#12506 = DIRECTION ( 'NONE',  ( 0.000000000000000000, 0.000000000000000000, 1.000000000000000000 ) ) ;
#12507 = CARTESIAN_POINT ( 'NONE',  ( -9.671043645249580933, 10.17730576241299900, 0.7998128361456462443 ) ) ;
#12508 = AXIS2_PLACEMENT_3D ( 'NONE', #43016, #39793, #142656 ) ;
#12509 = CARTESIAN_POINT ( 'NONE',  ( 5.032170685167933755, 1.114402916724830161, -1.852182961850391774 ) ) ;
#12510 = CARTESIAN_POINT ( 'NONE',  ( -4.828112100242291760, 6.726159765073026264, -1.443375672974066548 ) ) ;
#12511 = CARTESIAN_POINT ( 'NONE',  ( -5.088052786878465739, 9.158088361325352977, 0.000000000000000000 ) ) ;
#12512 = CARTESIAN_POINT ( 'NONE',  ( 2.848016566918720294, -1.427295477286108394, -1.568503593382633454 ) ) ;
#12514 = CARTESIAN_POINT ( 'NONE',  ( -11.36817070414822695, 5.406007704794011381, -5.610921796774237968 ) ) ;
#12513 = LINE ( 'NONE', #129565, #6796 ) ;
#12515 = CARTESIAN_POINT ( 'NONE',  ( 4.446526809179438544, 0.5226573815438217974, 1.900768696068744434 ) ) ;
#12516 = CARTESIAN_POINT ( 'NONE',  ( 6.533470333208203584, -0.1312131129157616261, 1.882018712217728318 ) ) ;
#12517 = ORIENTED_EDGE ( 'NONE', *, *, #115159, .T. ) ;
#12518 = CARTESIAN_POINT ( 'NONE',  ( 5.507064729579815854, -0.04930729212004316547, 2.116909390494752685 ) ) ;
#12519 = CARTESIAN_POINT ( 'NONE',  ( 6.877413706903859669, -0.1509731808640407125, 1.936391978998742269 ) ) ;
#12520 = CARTESIAN_POINT ( 'NONE',  ( 2.115084705647510610, -1.883649903580833174, 0.4717843263111404783 ) ) ;
#12521 = ORIENTED_EDGE ( 'NONE', *, *, #31725, .F. ) ;
#12522 = DIRECTION ( 'NONE',  ( 1.039099362110107450E-15, 1.000000000000000000, -4.583713267641621330E-32 ) ) ;
#12523 = CARTESIAN_POINT ( 'NONE',  ( 5.851225812749518695, 8.984124660586543243, -1.199719254218452047 ) ) ;
#12525 = CARTESIAN_POINT ( 'NONE',  ( 5.147291874682557555, 9.156924287104992288, 0.7998128361456462443 ) ) ;
#12524 = CARTESIAN_POINT ( 'NONE',  ( 1.992240001063511290, -0.5588421479580056861, -2.014483121414586186 ) ) ;
#12527 = EDGE_CURVE ( 'NONE', #89074, #55892, #134968, .T. ) ;
#12526 = CARTESIAN_POINT ( 'NONE',  ( 8.188198428010544205, 8.517596018959260107, 0.000000000000000000 ) ) ;
#12529 = ORIENTED_EDGE ( 'NONE', *, *, #76048, .T. ) ;
#12528 = CARTESIAN_POINT ( 'NONE',  ( 0.5745104438982637785, -1.313040981126518902, 1.248171054211825171 ) ) ;
#12530 = CARTESIAN_POINT ( 'NONE',  ( 4.934293700819583073, 1.136511309699510308, -1.891595316245115788 ) ) ;
#12531 = CARTESIAN_POINT ( 'NONE',  ( -0.3183146091065937600, -6.808378554901762136, -10.86152993230180996 ) ) ;
#12532 = CARTESIAN_POINT ( 'NONE',  ( 3.434799832723956392, 2.152550277175222515, 0.4854691814954179563 ) ) ;
#12533 = CARTESIAN_POINT ( 'NONE',  ( 1.225099565173026761, 1.686864977381890451, 0.9006792851762451813 ) ) ;
#12534 =( BOUNDED_SURFACE ( )  B_SPLINE_SURFACE ( 3, 2, ( 
 ( #121731, #72874, #172539 ),
 ( #5719, #71796, #138980 ),
 ( #124930, #205003, #56649 ),
 ( #122811, #156290, #188770 ),
 ( #24124, #90226, #7874 ),
 ( #73962, #140056, #123870 ) ),
 .UNSPECIFIED., .F., .F., .T. ) 
 B_SPLINE_SURFACE_WITH_KNOTS ( ( 4, 2, 4 ),
 ( 3, 3 ),
 ( 0.000000000000000000, 0.002122857551078452965, 0.004245715102156905930 ),
 ( 0.000000000000000000, 1.000000000000000000 ),
 .UNSPECIFIED. ) 
 GEOMETRIC_REPRESENTATION_ITEM ( )  RATIONAL_B_SPLINE_SURFACE ( (
 ( 1.000000000000000000, 0.7806433624857582743, 1.000000000000000000),
 ( 1.000000000000000000, 0.7860453980259710649, 1.000000000000000000),
 ( 1.000000000000000000, 0.7924770197564218188, 1.000000000000000000),
 ( 1.000000000000000000, 0.8094762427233131996, 1.000000000000000000),
 ( 1.000000000000000000, 0.8200718518785218292, 1.000000000000000000),
 ( 1.000000000000000000, 0.8343063410434344851, 1.000000000000000000) ) ) 
 REPRESENTATION_ITEM ( '' )  SURFACE ( )  );
#12535 = CARTESIAN_POINT ( 'NONE',  ( 7.913155211870404493, 12.38376484715752213, 0.7998128361456462443 ) ) ;
#12536 = CARTESIAN_POINT ( 'NONE',  ( 4.422371208857902580, 0.9731212702417373350, 1.827393648576709717 ) ) ;
#12537 = CARTESIAN_POINT ( 'NONE',  ( 2.887745953747706373, 1.527789104365802286, 1.529575784674996886 ) ) ;
#12538 = CARTESIAN_POINT ( 'NONE',  ( 5.249643141573060667, 2.189086832579402842, -0.1069518675670885766 ) ) ;
#12539 = CYLINDRICAL_SURFACE ( 'NONE', #100355, 2.750000000000000444 ) ;
#12540 = CARTESIAN_POINT ( 'NONE',  ( 6.062430963966053632, 7.101866208495718702, -1.199719254218452047 ) ) ;
#12541 = DIRECTION ( 'NONE',  ( 0.000000000000000000, 1.000000000000000000, 0.000000000000000000 ) ) ;
#12542 = CARTESIAN_POINT ( 'NONE',  ( -4.817943484809863008, 6.714296380401858499, 1.599625672291263179 ) ) ;
#12543 = CARTESIAN_POINT ( 'NONE',  ( 0.4752326960846975923, -2.001511663014220677, -0.2440270837566413387 ) ) ;
#12544 = CARTESIAN_POINT ( 'NONE',  ( -9.842856333841300653, 10.58567993234409421, 0.7216878364870438212 ) ) ;
#12545 = CARTESIAN_POINT ( 'NONE',  ( 6.222266154028957885, 6.224008365980749247, 0.7998128361456352531 ) ) ;
#12546 = CARTESIAN_POINT ( 'NONE',  ( 4.276279003695676373, -1.059865903354087813, -1.778221194881628220 ) ) ;
#12547 = CARTESIAN_POINT ( 'NONE',  ( 3.316937275718701894, 1.741877725598478976, 0.8232385001258867296 ) ) ;
#12548 = CARTESIAN_POINT ( 'NONE',  ( -0.07068620461728526705, -1.560437159073333468, -1.276799021846956705 ) ) ;
#12549 = CARTESIAN_POINT ( 'NONE',  ( 4.473300617505036492, 7.306268922809479704, -1.199719254218452047 ) ) ;
#12550 = CARTESIAN_POINT ( 'NONE',  ( 9.452508394161716510, 3.481540833006149249, 7.393820799723206605 ) ) ;
#12551 = CARTESIAN_POINT ( 'NONE',  ( 3.537912347765668208, 1.245987026601946157, 1.525231921242198307 ) ) ;
#12552 = CARTESIAN_POINT ( 'NONE',  ( -0.02321191073820921824, -0.1601477211686137825, -2.156400265872604471 ) ) ;
#12553 = CARTESIAN_POINT ( 'NONE',  ( 4.582524934692378871, -1.771534430979417429, -0.4408631061849078714 ) ) ;
#12554 = PRODUCT_DEFINITION_SHAPE ( 'NONE', 'NONE',  #214420 ) ;
#12555 = CARTESIAN_POINT ( 'NONE',  ( 7.377044979611483200, 7.779176362401098999, -0.7216878364870317197 ) ) ;
#12556 = CARTESIAN_POINT ( 'NONE',  ( 3.185802909086937973, 6.660594460669327255, 0.7216878364870317197 ) ) ;
#12557 = CARTESIAN_POINT ( 'NONE',  ( -7.781453819600577582, 8.043060642480948985, 0.000000000000000000 ) ) ;
#12558 = CARTESIAN_POINT ( 'NONE',  ( 5.204350862799327793, 7.165104988056252289, -1.599625672291281386 ) ) ;
#12559 = ORIENTED_EDGE ( 'NONE', *, *, #167354, .T. ) ;
#12561 = CARTESIAN_POINT ( 'NONE',  ( 4.570568844821727872, 0.7744313447282255014, 1.858482759491510095 ) ) ;
#12560 = CARTESIAN_POINT ( 'NONE',  ( 1.856743374925871715, 0.3135980649527739250, -1.814175028193690808 ) ) ;
#12562 = CARTESIAN_POINT ( 'NONE',  ( 0.4217922253725381321, 0.8825364984147118230, 2.122365683989856588 ) ) ;
#12563 = CARTESIAN_POINT ( 'NONE',  ( 4.961744919065853132, -0.5270168765720646409, 1.889542207339139024 ) ) ;
#12564 = CARTESIAN_POINT ( 'NONE',  ( -5.682838942422375084, 9.781729199468104596, 0.000000000000000000 ) ) ;
#12565 = DIRECTION ( 'NONE',  ( 1.224646799147360603E-16, 1.000000000000000000, -8.546850786086437571E-32 ) ) ;
#12566 =( GEOMETRIC_REPRESENTATION_CONTEXT ( 3 ) GLOBAL_UNCERTAINTY_ASSIGNED_CONTEXT ( ( #66671 ) ) GLOBAL_UNIT_ASSIGNED_CONTEXT ( ( #76426, #142535, #177137 ) ) REPRESENTATION_CONTEXT ( 'NONE', 'WORKASPACE' ) );
#12567 = CARTESIAN_POINT ( 'NONE',  ( -4.308793891044708779, 3.921347715840572956, 1.214306433183764966E-14 ) ) ;
#12568 = SURFACE_STYLE_USAGE ( .BOTH. , #165224 ) ;
#12569 = CARTESIAN_POINT ( 'NONE',  ( -5.204350862799341115, 7.165104988056252289, -1.599625672291271394 ) ) ;
#12571 = CARTESIAN_POINT ( 'NONE',  ( 0.4791068267422092797, 1.747065859276742072, -0.6691465683838908607 ) ) ;
#12570 = CARTESIAN_POINT ( 'NONE',  ( 1.435225040761441972, -1.516673362169782990, -1.439332739067126443 ) ) ;
#12572 = CARTESIAN_POINT ( 'NONE',  ( -7.968844136639799736, -5.196967604326695245, 7.583016927391841300 ) ) ;
#12573 = CARTESIAN_POINT ( 'NONE',  ( -0.1106727585416227011, 0.2327126083698972114, -2.036986407471320426 ) ) ;
#12574 = CARTESIAN_POINT ( 'NONE',  ( 0.4677839449492172674, -1.637930601595443125, -0.5889144675248291216 ) ) ;
#12575 = CARTESIAN_POINT ( 'NONE',  ( 6.531277313481192337, 8.642909503859968368, 1.599625672291281386 ) ) ;
#12577 = CARTESIAN_POINT ( 'NONE',  ( -6.972266317189433020E-16, 1.750000000682810475, -1.225000000000013634 ) ) ;
#12576 = CARTESIAN_POINT ( 'NONE',  ( 0.000000000000000000, -2.000000000000001776, 0.000000000000000000 ) ) ;
#12578 = CARTESIAN_POINT ( 'NONE',  ( 1.681838029686154146, -0.9247999101687879309, 1.455793735983588633 ) ) ;
#12579 = CARTESIAN_POINT ( 'NONE',  ( 1.417800074541092137, -1.221294057239637576, -1.819523406426680090 ) ) ;
#12580 = CARTESIAN_POINT ( 'NONE',  ( 3.651171877326536030, -1.804458330144659950, 1.270265763067345066 ) ) ;
#12581 = CARTESIAN_POINT ( 'NONE',  ( -10.22593938286385296, 3.000029897349846930, -7.498676971688964521 ) ) ;
#12582 = CARTESIAN_POINT ( 'NONE',  ( 1.217902493145516463, 0.4257177869225349243, -2.128761017034991543 ) ) ;
#12583 = CARTESIAN_POINT ( 'NONE',  ( -1.123270288254055060, 3.033552654332631437, 0.7749999999939940487 ) ) ;
#12584 = CARTESIAN_POINT ( 'NONE',  ( 2.888026961012623239, -2.114693475102703779, 0.1087559668010943809 ) ) ;
#12585 = CARTESIAN_POINT ( 'NONE',  ( 6.639320575229251453, 2.090987163941595561, 2.106969785032047238 ) ) ;
#12586 = ORIENTED_EDGE ( 'NONE', *, *, #179634, .T. ) ;
#12588 = CARTESIAN_POINT ( 'NONE',  ( 1.364683531249986537, -0.3239583329919163424, 0.7879004041258500513 ) ) ;
#12587 = CARTESIAN_POINT ( 'NONE',  ( 3.615000845857639256, -0.1676676331447447266, 2.286275989141072440 ) ) ;
#12589 =( LENGTH_UNIT ( ) NAMED_UNIT ( * ) SI_UNIT ( .MILLI., .METRE. ) );
#12590 = CARTESIAN_POINT ( 'NONE',  ( 3.867100128395839942, 5.534702787927018974, -1.599625672291255185 ) ) ;
#12591 = CARTESIAN_POINT ( 'NONE',  ( 5.971364366153397718, -1.903789954562478792, -1.144205655003695643 ) ) ;
#12592 = CARTESIAN_POINT ( 'NONE',  ( -6.019457014787517046, 9.006155036351978893, 1.082531754730548412 ) ) ;
#12593 = ADVANCED_FACE ( 'NONE', ( #55545 ), #4940, .T. ) ;
#12594 = MECHANICAL_DESIGN_GEOMETRIC_PRESENTATION_REPRESENTATION (  '', ( #50633 ), #74777 ) ;
#12595 = CARTESIAN_POINT ( 'NONE',  ( 5.680503174445848735, 5.729601246382692636, 1.040834085586084257E-14 ) ) ;
#12596 = CARTESIAN_POINT ( 'NONE',  ( -8.175203438916030407, 8.640084888264587093, 0.7216878364870578100 ) ) ;
#12597 = CARTESIAN_POINT ( 'NONE',  ( 5.736508392357904107, 5.865217010605237924, 0.000000000000000000 ) ) ;
#12599 = ORIENTED_EDGE ( 'NONE', *, *, #203560, .T. ) ;
#12598 = TOROIDAL_SURFACE ( 'NONE', #29942, 11.92000000000000171, 0.08000000000000000167 ) ;
#12600 = CARTESIAN_POINT ( 'NONE',  ( 4.131482539099665452, 0.5404898895830790861, 1.942541833525657680 ) ) ;
#12602 = CARTESIAN_POINT ( 'NONE',  ( 2.413000123442359701, -1.597275988187638607, 1.305004441579124208 ) ) ;
#12601 = CARTESIAN_POINT ( 'NONE',  ( 6.474182045725470402, 7.511966127223233869, -1.199719254218446718 ) ) ;
#12603 = FACE_OUTER_BOUND ( 'NONE', #6103, .T. ) ;
#12604 = CARTESIAN_POINT ( 'NONE',  ( 4.624739795592929248, 6.488892076315451618, -1.443375672974068769 ) ) ;
#12605 = FACE_OUTER_BOUND ( 'NONE', #146731, .T. ) ;
#12606 = CARTESIAN_POINT ( 'NONE',  ( -1.364683531249997417, 4.759375000341424133, 1.214306433183764966E-14 ) ) ;
#12607 = CARTESIAN_POINT ( 'NONE',  ( 5.507841377412062478, -0.9828142975771281264, -1.958786091674463714 ) ) ;
#12608 = CARTESIAN_POINT ( 'NONE',  ( 2.373672848961404735, -0.3474683332905931232, -1.986100487175908258 ) ) ;
#12609 = CARTESIAN_POINT ( 'NONE',  ( 2.366542893654680402, 0.08848056876738576160, -1.839231530397527736 ) ) ;
#12610 = CARTESIAN_POINT ( 'NONE',  ( 6.388916700537700777, 8.476822122092563916, 1.599625672291281386 ) ) ;
#12611 = PRESENTATION_STYLE_ASSIGNMENT (( #180461 ) ) ;
#12612 = CARTESIAN_POINT ( 'NONE',  ( 5.245057492501287832, -1.564903486862476489, 0.9398553879134128319 ) ) ;
#12613 = CARTESIAN_POINT ( 'NONE',  ( 6.258435431136967431, 1.928752767684217106, -0.5880170417187426946 ) ) ;
#12614 = CARTESIAN_POINT ( 'NONE',  ( -7.985916173649233230, 9.275655943134292869, -1.199719254218446718 ) ) ;
#12616 = CARTESIAN_POINT ( 'NONE',  ( -6.282224075085783177, 8.422623735723785643, 1.599625672291269396 ) ) ;
#12615 = CARTESIAN_POINT ( 'NONE',  ( 5.875896723904014962, 1.342229061679913071, 1.821250878268846352 ) ) ;
#12617 = CARTESIAN_POINT ( 'NONE',  ( 0.9441299549096024979, 0.8517545906277513845, -1.926334332536754346 ) ) ;
#12618 = CARTESIAN_POINT ( 'NONE',  ( -5.250750630242457362, 9.347902511916677426, 0.000000000000000000 ) ) ;
#12619 = CARTESIAN_POINT ( 'NONE',  ( 8.426556166093362776, 9.789735934319136135, -1.199719254218446718 ) ) ;
#12620 = CARTESIAN_POINT ( 'NONE',  ( 7.038091138825468107, 8.344099429118761790, -1.082531754730548412 ) ) ;
#12621 = DIRECTION ( 'NONE',  ( 1.000000000000000000, 0.000000000000000000, 0.000000000000000000 ) ) ;
#12622 = CARTESIAN_POINT ( 'NONE',  ( -6.581593504430098385, 9.765943957555402122, -1.199719254218440723 ) ) ;
#12623 = UNCERTAINTY_MEASURE_WITH_UNIT (LENGTH_MEASURE( 1.000000000000000082E-05 ), #103543, 'distance_accuracy_value', 'NONE');
#12624 = CARTESIAN_POINT ( 'NONE',  ( 3.404766800216717737, 6.348112014766642552, 1.069586989871921467 ) ) ;
#12625 = CARTESIAN_POINT ( 'NONE',  ( 8.392133896734671694, 8.893170422386358354, 0.7216878364870458196 ) ) ;
#12626 = CARTESIAN_POINT ( 'NONE',  ( 4.005937425286727027, 7.819599604358462130, 0.1919598339409686050 ) ) ;
#12627 = CARTESIAN_POINT ( 'NONE',  ( -9.978437869977959451, 10.74385839117019614, -0.7216878364870267237 ) ) ;
#12629 = CARTESIAN_POINT ( 'NONE',  ( 2.988771237642441569, -1.320003323290209751, 1.786578734224959497 ) ) ;
#12628 = CARTESIAN_POINT ( 'NONE',  ( 1.336355901170083849, -1.182550835430173919, -1.760063440837428272 ) ) ;
#12630 = CARTESIAN_POINT ( 'NONE',  ( 3.250441568315368457, 6.417235977211314335, -0.9123035412251535581 ) ) ;
#12631 = CARTESIAN_POINT ( 'NONE',  ( -6.231907884136888676, 7.299589282028351001, -1.199719254218453823 ) ) ;
#12632 = CARTESIAN_POINT ( 'NONE',  ( 5.666418135507635512, 8.698239360479199433, 1.199719254218462483 ) ) ;
#12633 = CARTESIAN_POINT ( 'NONE',  ( 3.807043925254738781, -1.605251362286563177, 1.127602784832412386 ) ) ;
#12634 = CARTESIAN_POINT ( 'NONE',  ( 5.286789834324991055, 8.255339675766103724, -1.199719254218452935 ) ) ;
#12635 = CARTESIAN_POINT ( 'NONE',  ( -5.155981903556834389, 6.496760599866445496, 1.199444197134313272 ) ) ;
#12636 = CARTESIAN_POINT ( 'NONE',  ( 4.630273154266905777, 5.360739087188218122, 1.199719254218464037 ) ) ;
#12637 = CARTESIAN_POINT ( 'NONE',  ( -4.340018570150309785, 7.117086527600392287, -1.082531754730551743 ) ) ;
#12640 = ORIENTED_EDGE ( 'NONE', *, *, #170841, .T. ) ;
#12639 = CARTESIAN_POINT ( 'NONE',  ( -6.561783159334137139, 8.678499657355050800, -1.443375672974059665 ) ) ;
#12638 = TOROIDAL_SURFACE ( 'NONE', #164794, 11.91999999999999993, 0.08000000000000000167 ) ;
#12641 = CARTESIAN_POINT ( 'NONE',  ( 2.355864820516640812, -1.574449018071517825, -1.420800595792824028 ) ) ;
#12642 = CARTESIAN_POINT ( 'NONE',  ( -4.261005416444848315, 8.193199762486115034, 0.7998128361456352531 ) ) ;
#12643 = CARTESIAN_POINT ( 'NONE',  ( 4.663041391408608405, -1.929494027986548454, -0.9748474430888448561 ) ) ;
#12644 = CARTESIAN_POINT ( 'NONE',  ( 2.348939331405873077, 0.4892633877765646400, -1.774999737812533063 ) ) ;
#12645 = CARTESIAN_POINT ( 'NONE',  ( -4.609732581575539889, 6.945374051331699938, 1.198810113796699328 ) ) ;
#12646 = CARTESIAN_POINT ( 'NONE',  ( 0.6823417656249882723, -0.2614583329919109578, -1.181850606188749264 ) ) ;
#12647 = CARTESIAN_POINT ( 'NONE',  ( 5.208843366089195293, -0.2500283176610699210, 1.722145524253251514 ) ) ;
#12648 = CARTESIAN_POINT ( 'NONE',  ( 6.727182134110186063, 1.310238205575515957, 1.828849833172506489 ) ) ;
#12649 = CARTESIAN_POINT ( 'NONE',  ( 3.863710590214593399, 7.451486755318259547, 1.040834085586084257E-14 ) ) ;
#12650 = SURFACE_SIDE_STYLE ('',( #194608 ) ) ;
#12651 = CARTESIAN_POINT ( 'NONE',  ( 3.204151765443470357, -2.159293047372488950, 0.1044485798024074874 ) ) ;
#12652 = CARTESIAN_POINT ( 'NONE',  ( 5.729842239849809893, -1.821464125411855761, -0.8645900286049985617 ) ) ;
#12653 = CARTESIAN_POINT ( 'NONE',  ( -7.971831134711019118, 12.24429405723079967, 0.000000000000000000 ) ) ;
#12654 = CARTESIAN_POINT ( 'NONE',  ( 2.167066695894452888, -1.976221826324360498, -0.8764929760368763700 ) ) ;
#12655 = CARTESIAN_POINT ( 'NONE',  ( 4.253168938266341570, -1.637241709590877781, -1.097755751903241483 ) ) ;
#12656 = CARTESIAN_POINT ( 'NONE',  ( 4.774914120469089696, 1.810774457899359202, -0.7023516835302608952 ) ) ;
#12659 = ORIENTED_EDGE ( 'NONE', *, *, #199415, .T. ) ;
#12658 = CARTESIAN_POINT ( 'NONE',  ( 8.024185963717927805, -5.166862990899748986, -7.524604700374135646 ) ) ;
#12657 = CARTESIAN_POINT ( 'NONE',  ( -8.636180661780660017, 11.09863007687603087, -1.443375672974058777 ) ) ;
#12660 = CARTESIAN_POINT ( 'NONE',  ( -6.740338644649361832, 7.892758502626242567, -1.199719254218452047 ) ) ;
#12661 = ADVANCED_FACE ( 'NONE', ( #161591 ), #96601, .T. ) ;
#12663 = VERTEX_POINT ( 'NONE', #143237 ) ;
#12662 = CARTESIAN_POINT ( 'NONE',  ( -5.276058054373441664, 6.184431147304315424, -1.199719254218453823 ) ) ;
#12664 = CARTESIAN_POINT ( 'NONE',  ( -7.605760987142072160, 10.85684300409898384, 1.082531754730549967 ) ) ;
#12665 = CARTESIAN_POINT ( 'NONE',  ( 0.8334014933106950185, 0.1641056870149599223, 2.200712145998296343 ) ) ;
#12666 = CARTESIAN_POINT ( 'NONE',  ( 0.000000000000000000, -1.246874999522042948, -3.793834371823813001 ) ) ;
#12667 = CARTESIAN_POINT ( 'NONE',  ( 5.946142449018281262, -0.8852437533515828960, 1.750773106858094952 ) ) ;
#12668 = CARTESIAN_POINT ( 'NONE',  ( -1.500000000000013101, 3.660416667349488673, -0.8660254037844313801 ) ) ;
#12669 = CARTESIAN_POINT ( 'NONE',  ( 5.018332763094478288, 6.785885375482345161, -1.424093192218821136 ) ) ;
#12670 = CARTESIAN_POINT ( 'NONE',  ( 0.07499057489264347731, 1.360887136235461758, -2.209073988085366480 ) ) ;
#12671 = CARTESIAN_POINT ( 'NONE',  ( 4.997927640213790212, -0.6233917918176261619, -1.732523409203725828 ) ) ;
#12672 = ORIENTED_EDGE ( 'NONE', *, *, #61478, .T. ) ;
#12673 = CARTESIAN_POINT ( 'NONE',  ( -1.360316468750034868, -0.8802083329919301313, -0.7853790794159242195 ) ) ;
#12674 = CARTESIAN_POINT ( 'NONE',  ( -8.019811557683421910, 9.315200557840817908, 1.199719254218462483 ) ) ;
#12675 = DIRECTION ( 'NONE',  ( 0.000000000000000000, -1.000000000000000000, -9.023263958591317418E-17 ) ) ;
#12676 = CARTESIAN_POINT ( 'NONE',  ( 5.818629517237746462, -0.7649446623404360102, -1.977987144599784086 ) ) ;
#12677 = CARTESIAN_POINT ( 'NONE',  ( 7.721398836998367265, -6.134628647623499909, -7.721398836998390358 ) ) ;
#12678 = CARTESIAN_POINT ( 'NONE',  ( 3.499976210622149253, 7.235056012367825140, 0.7998128361456321445 ) ) ;
#12679 = CARTESIAN_POINT ( 'NONE',  ( 6.046181036401986120, 2.058226046012123334, 0.1054989004632029409 ) ) ;
#12682 = CARTESIAN_POINT ( 'NONE',  ( 3.684953445348177148, 1.336164438771630714, 1.267087564277062484 ) ) ;
#12681 = CARTESIAN_POINT ( 'NONE',  ( 1.644728535064543529, -0.2685211301156094632, -1.841439677390522389 ) ) ;
#12680 = SURFACE_STYLE_FILL_AREA ( #143817 ) ;
#12683 = CARTESIAN_POINT ( 'NONE',  ( 8.015895134177609904, 10.37496362800581018, 1.599625672291281386 ) ) ;
#12684 = FILL_AREA_STYLE_COLOUR ( '', #72343 ) ;
#12685 = CARTESIAN_POINT ( 'NONE',  ( -6.631873415740034083, 7.766215735565355160, 1.199719254218452047 ) ) ;
#12687 = ORIENTED_EDGE ( 'NONE', *, *, #41532, .T. ) ;
#12686 = CARTESIAN_POINT ( 'NONE',  ( -10.34804403480111290, -6.705807696129545192, 1.138412281109779656E-15 ) ) ;
#12688 = CARTESIAN_POINT ( 'NONE',  ( 3.651171877326536030, -1.804458330144659950, 1.270265763067345066 ) ) ;
#12689 = CARTESIAN_POINT ( 'NONE',  ( 6.362609103649501385, -1.606607173180201187, 1.593162483179947575 ) ) ;
#12690 = CARTESIAN_POINT ( 'NONE',  ( -5.409340102172518705, 9.254721185935849803, 0.000000000000000000 ) ) ;
#12691 = CARTESIAN_POINT ( 'NONE',  ( 5.308800944376626418, -0.4481363076810992996, -1.755139329022289196 ) ) ;
#12692 = CARTESIAN_POINT ( 'NONE',  ( 6.456256392861089211, -1.172487466661990663, 1.515489988593403226 ) ) ;
#12693 = CARTESIAN_POINT ( 'NONE',  ( -5.908535366263003574, 4.807949608181244727, -2.499999999999995115 ) ) ;
#12694 = CARTESIAN_POINT ( 'NONE',  ( 6.209813078548920728, -1.856259414618817383, 0.2309603555875269776 ) ) ;
#12695 = CARTESIAN_POINT ( 'NONE',  ( -0.0004021858452125243177, 15.43212108951242634, 11.92774328084775171 ) ) ;
#12696 = CARTESIAN_POINT ( 'NONE',  ( 5.875818619555242428, 1.057306330162042451, 1.419162741687775231 ) ) ;
#12697 = CARTESIAN_POINT ( 'NONE',  ( 1.516814941429758701, 0.2024661778830244008, 2.006371303556075958 ) ) ;
#12699 = CARTESIAN_POINT ( 'NONE',  ( 2.842513320990670778, 2.090244732995512944, 0.2570852942500467808 ) ) ;
#12698 = CARTESIAN_POINT ( 'NONE',  ( -10.01677656239806247, 10.58066083241955901, 0.7998128361456462443 ) ) ;
#12700 = EDGE_CURVE ( 'NONE', #95577, #60775, #94466, .T. ) ;
#12701 = CARTESIAN_POINT ( 'NONE',  ( 9.420217803396747414, 9.884675613584706255, 0.7998128361456462443 ) ) ;
#12703 = CARTESIAN_POINT ( 'NONE',  ( -9.341731535015849630, 10.85744053139533349, 1.199719254218462483 ) ) ;
#12702 = CARTESIAN_POINT ( 'NONE',  ( 0.7499999999999867883, -0.9333333333333138082, -1.299038105676652011 ) ) ;
#12704 = DIRECTION ( 'NONE',  ( 1.000000000000000000, 1.725633230170963762E-31, 8.638326563840814399E-31 ) ) ;
#12705 = CARTESIAN_POINT ( 'NONE',  ( 2.601824576204377681, 1.431331034542600245, 1.425341822903106515 ) ) ;
#12706 = CARTESIAN_POINT ( 'NONE',  ( -0.6823417656250212460, 3.801041667008085767, 1.181850606188767472 ) ) ;
#12707 = EDGE_CURVE ( 'NONE', #160219, #138893, #179794, .T. ) ;
#12708 = CARTESIAN_POINT ( 'NONE',  ( 2.659370686574860976, 6.254349567645977714, -0.7998128361456291469 ) ) ;
#12709 = CARTESIAN_POINT ( 'NONE',  ( 3.673254355229157664, 0.05708692194854488033, -2.161017345153878999 ) ) ;
#12710 = CARTESIAN_POINT ( 'NONE',  ( 4.764381983412778688E-15, 12.71875000068279782, -1.499999999999998446 ) ) ;
#12712 = DIRECTION ( 'NONE',  ( -0.7592566023653016805, -0.6507913734559627184, 0.000000000000000000 ) ) ;
#12711 = CARTESIAN_POINT ( 'NONE',  ( 6.831329296439236032, 9.063246493969506545, -1.599625672291267398 ) ) ;
#12713 =( BOUNDED_SURFACE ( )  B_SPLINE_SURFACE ( 3, 2, ( 
 ( #74486, #192479, #193561 ),
 ( #91827, #157886, #11601 ),
 ( #110252, #207672, #144859 ),
 ( #191411, #143795, #30006 ),
 ( #158936, #93959, #58232 ),
 ( #45204, #140592, #111318 ) ),
 .UNSPECIFIED., .F., .F., .T. ) 
 B_SPLINE_SURFACE_WITH_KNOTS ( ( 4, 2, 4 ),
 ( 3, 3 ),
 ( 0.000000000000000000, 0.0003766365702389427254, 0.0007532731404778854507 ),
 ( 0.000000000000000000, 1.000000000000000000 ),
 .UNSPECIFIED. ) 
 GEOMETRIC_REPRESENTATION_ITEM ( )  RATIONAL_B_SPLINE_SURFACE ( (
 ( 1.000000000000000000, 0.7452309222762957264, 1.000000000000000000),
 ( 1.000000000000000000, 0.7451892422671834160, 1.000000000000000000),
 ( 1.000000000000000000, 0.7429606254238495522, 1.000000000000000000),
 ( 1.000000000000000000, 0.7311462761265991039, 1.000000000000000000),
 ( 1.000000000000000000, 0.7212257702791121661, 1.000000000000000000),
 ( 1.000000000000000000, 0.7071067811865475727, 1.000000000000000000) ) ) 
 REPRESENTATION_ITEM ( '' )  SURFACE ( )  );
#12714 = CARTESIAN_POINT ( 'NONE',  ( 8.554831740098659765, 10.04335378727902395, 1.082531754730558626 ) ) ;
#12716 = CARTESIAN_POINT ( 'NONE',  ( 0.000000000000000000, 11.29999999999999893, 0.000000000000000000 ) ) ;
#12715 = CARTESIAN_POINT ( 'NONE',  ( 0.5202908490967810273, 2.147468835798187037, -0.3191156193892603632 ) ) ;
#12717 = CARTESIAN_POINT ( 'NONE',  ( -7.375272376154101472, 7.706831981708990753, -0.7216878364870278340 ) ) ;
#12718 =( GEOMETRIC_REPRESENTATION_CONTEXT ( 3 ) GLOBAL_UNCERTAINTY_ASSIGNED_CONTEXT ( ( #81898 ) ) GLOBAL_UNIT_ASSIGNED_CONTEXT ( ( #108750, #88165, #193124 ) ) REPRESENTATION_CONTEXT ( 'NONE', 'WORKASPACE' ) );
#12719 = CARTESIAN_POINT ( 'NONE',  ( -1.364683531250000748, 1.009375000341421247, 0.000000000000000000 ) ) ;
#12720 = CARTESIAN_POINT ( 'NONE',  ( 2.595491417077447238, -0.6846416945752286098, 2.081959150545972914 ) ) ;
#12721 = CARTESIAN_POINT ( 'NONE',  ( 6.883263157960367806, 2.959656548886806071, 2.506466465954690914 ) ) ;
#12722 = CARTESIAN_POINT ( 'NONE',  ( 3.028476438156304962, 1.258033425225786983, -1.880328901638250505 ) ) ;
#12723 = CARTESIAN_POINT ( 'NONE',  ( -7.694415870955439551, 8.935572256658169010, 1.199719254218462483 ) ) ;
#12724 = CARTESIAN_POINT ( 'NONE',  ( -4.758548728272219641, 4.653987725846768342, 0.7216878364870317197 ) ) ;
#12725 = CARTESIAN_POINT ( 'NONE',  ( -1.364683531250012516, 3.051041667008083547, -0.7879004041258289570 ) ) ;
#12726 = CARTESIAN_POINT ( 'NONE',  ( 5.779562687394081522, 7.242644825714458001, 1.188994900607452054 ) ) ;
#12727 = CARTESIAN_POINT ( 'NONE',  ( -1.500000000000015099, 12.47916666666666607, -0.8660254037844309360 ) ) ;
#12728 = CARTESIAN_POINT ( 'NONE',  ( 6.455090533882185788, 8.624301270986276080, -1.443375672974078761 ) ) ;
#12729 = CARTESIAN_POINT ( 'NONE',  ( 4.340886628629798238, -1.540457278443696509, 0.8709714020649069743 ) ) ;
#12730 = CARTESIAN_POINT ( 'NONE',  ( 8.585337585951586803, 11.03931315507545108, -1.599625672291255185 ) ) ;
#12731 = CARTESIAN_POINT ( 'NONE',  ( 0.3234443461216755522, -0.1028566021752069376, 2.103582624919388078 ) ) ;
#12732 = CARTESIAN_POINT ( 'NONE',  ( -1.364683531250000748, 9.859375000341398021, 0.000000000000000000 ) ) ;
#12733 = CARTESIAN_POINT ( 'NONE',  ( -4.098307573080856692, 8.003385611894792362, 0.7998128361456352531 ) ) ;
#12734 = CARTESIAN_POINT ( 'NONE',  ( 5.905875104417893873, -1.122515283938491537, -1.674877678029200068 ) ) ;
#12735 = ORIENTED_EDGE ( 'NONE', *, *, #136253, .F. ) ;
#12736 = CARTESIAN_POINT ( 'NONE',  ( 9.748476143425788720, 11.33197590787365172, -1.199719254218440723 ) ) ;
#12738 = CARTESIAN_POINT ( 'NONE',  ( 3.643291952642300213, -1.415932857957047375, -1.222571138756740838 ) ) ;
#12737 = VECTOR ( 'NONE', #139743, 1000.000000000000000 ) ;
#12739 = CARTESIAN_POINT ( 'NONE',  ( 3.045825399726837635, 1.460771095745692527, 1.467265538693182991 ) ) ;
#12740 = CARTESIAN_POINT ( 'NONE',  ( -6.929625909916163451, 7.257187447756535903, 0.7216878364870317197 ) ) ;
#12741 = CARTESIAN_POINT ( 'NONE',  ( 9.752392566931574081, 10.27221283770866300, -0.7998128361456281477 ) ) ;
#12742 = CARTESIAN_POINT ( 'NONE',  ( -1.573645197550657349, 8.680485584337372273, 2.500000000000011102 ) ) ;
#12743 = CARTESIAN_POINT ( 'NONE',  ( 9.681420934716557625, 3.864711529694057290, 7.090140244710065431 ) ) ;
#12744 = CARTESIAN_POINT ( 'NONE',  ( 6.209879897626497502, -2.145988306206991325, 0.2596296833028768347 ) ) ;
#12745 = B_SPLINE_CURVE_WITH_KNOTS ( 'NONE', 3,
 ( #197392, #145505, #49034, #115154, #32771, #66301, #132450 ),
 .UNSPECIFIED., .F., .F.,
 ( 4, 3, 4 ),
 ( 0.0001126021370636952904, 0.0006031550062628992376, 0.002006790698585253496 ),
 .UNSPECIFIED. ) ;
#12746 = CARTESIAN_POINT ( 'NONE',  ( -1.364683531250012516, 5.051041667008085767, -0.7879004041258300672 ) ) ;
#12747 = CARTESIAN_POINT ( 'NONE',  ( 2.857805160684105950, -0.6180756922911297968, 1.862011555624979886 ) ) ;
#12748 = CARTESIAN_POINT ( 'NONE',  ( 0.8255457999647041190, -1.462224166115761337, 1.388270745661695837 ) ) ;
#12749 = CARTESIAN_POINT ( 'NONE',  ( -3.526002468005825286, 6.271364091718859335, -1.199719254218450271 ) ) ;
#12751 =( NAMED_UNIT ( * ) PLANE_ANGLE_UNIT ( ) SI_UNIT ( $, .RADIAN. ) );
#12750 = CARTESIAN_POINT ( 'NONE',  ( 7.086107841436786181, 11.41887624831828418, 1.040834085586084257E-14 ) ) ;
#12752 = CARTESIAN_POINT ( 'NONE',  ( 0.8955150854165813135, -0.6789544621725839280, 1.743152336062703256 ) ) ;
#12753 = CARTESIAN_POINT ( 'NONE',  ( 0.6823417656249917140, 3.592708333674754506, 1.181850606188765695 ) ) ;
#12754 = CARTESIAN_POINT ( 'NONE',  ( 2.830340462983381489, -0.9960867002655849900, -1.749474899777081704 ) ) ;
#12756 = CARTESIAN_POINT ( 'NONE',  ( 2.689187139871064502, 1.790190400678292715, 1.130151903539077463 ) ) ;
#12755 = CARTESIAN_POINT ( 'NONE',  ( -5.422898255786193111, 8.310169817517122581, -1.082531754730544860 ) ) ;
#12757 = CARTESIAN_POINT ( 'NONE',  ( 1.474199074347493310, 7.377996015708387034, 4.279257749350846574 ) ) ;
#12758 = CARTESIAN_POINT ( 'NONE',  ( 4.281733463571851139, -1.982135700070002615, 0.5980053909793592304 ) ) ;
#12759 = CARTESIAN_POINT ( 'NONE',  ( 3.573456005653643519, 6.326726552307992080, -1.199719254218453823 ) ) ;
#12761 = CARTESIAN_POINT ( 'NONE',  ( 2.517010073631369860, 6.088262185878572375, -0.7998128361456281477 ) ) ;
#12760 = CARTESIAN_POINT ( 'NONE',  ( 0.3629773032866591143, 0.2007434131479734207, -2.081070348792604108 ) ) ;
#12763 = ORIENTED_EDGE ( 'NONE', *, *, #151345, .T. ) ;
#12762 = CARTESIAN_POINT ( 'NONE',  ( 5.842758758449526191, 0.3585452818064547853, 1.789846783968067845 ) ) ;
#12764 = CARTESIAN_POINT ( 'NONE',  ( 7.553864141108259211, 11.96459193126834464, 1.040834085586084257E-14 ) ) ;
#12765 = CARTESIAN_POINT ( 'NONE',  ( 4.957044826796043857, 6.512741263610869247, -2.500000000000437428 ) ) ;
#12766 = CARTESIAN_POINT ( 'NONE',  ( 10.74631150800302670, 10.90885146202907663, -5.675916053542507278 ) ) ;
#12767 = CARTESIAN_POINT ( 'NONE',  ( 6.756857042228312515, -1.710155547305733492, 1.394389531264042414 ) ) ;
#12768 = CARTESIAN_POINT ( 'NONE',  ( -1.364683531250014514, 10.65104166700806942, -0.7879004041258335089 ) ) ;
#12769 = CARTESIAN_POINT ( 'NONE',  ( 4.881465217424630687, 0.1836680969147831965, -1.903426456924644183 ) ) ;
#12771 = CARTESIAN_POINT ( 'NONE',  ( -8.459397779922852578, 11.95671561229694824, 1.199719254218453823 ) ) ;
#12770 = CIRCLE ( 'NONE', #133904, 0.07999999999999980738 ) ;
#12772 = CARTESIAN_POINT ( 'NONE',  ( 5.900823170445728572, 7.907379670318584353, 1.599625672291267398 ) ) ;
#12773 = CARTESIAN_POINT ( 'NONE',  ( 1.360316468749961594, 2.026041667008099623, 0.7853790794158520550 ) ) ;
#12774 = CARTESIAN_POINT ( 'NONE',  ( 4.650083499362880346, 4.527444958785877382, 0.7216878364870317197 ) ) ;
#12775 = CARTESIAN_POINT ( 'NONE',  ( -3.147653791585727667, 8.920000000000001705, -2.419999999999998597 ) ) ;
#12776 = CARTESIAN_POINT ( 'NONE',  ( 5.847644326195776010, 5.716673223516856694, -0.7998128361456281477 ) ) ;
#12777 = VERTEX_POINT ( 'NONE', #30520 ) ;
#12778 = VECTOR ( 'NONE', #53984, 1000.000000000000000 ) ;
#12779 = CARTESIAN_POINT ( 'NONE',  ( -6.237633190739009237, 9.434933268240943249, 1.199719254218452047 ) ) ;
#12780 = CARTESIAN_POINT ( 'NONE',  ( 4.745289220334846902, -1.444806058459674691, -1.188008360142885245 ) ) ;
#12781 = CARTESIAN_POINT ( 'NONE',  ( 0.07700591528354226722, 2.040803078245361224, -2.328119179575589559 ) ) ;
#12782 = CARTESIAN_POINT ( 'NONE',  ( 7.018280793729500644, 8.217024343219755167, -1.199719254218452047 ) ) ;
#12783 = CARTESIAN_POINT ( 'NONE',  ( -0.3866937364864243554, 3.956598013261175772, 11.53692321988874170 ) ) ;
#12784 = CARTESIAN_POINT ( 'NONE',  ( -5.520246714036333380, 7.462180650995058784, 1.249303437716933196 ) ) ;
#12785 = CARTESIAN_POINT ( 'NONE',  ( -7.049876689426121779, 7.327203680526343632, -0.7216878364870278340 ) ) ;
#12786 = CARTESIAN_POINT ( 'NONE',  ( 3.497113557321089861, 6.167384019261527683, -1.199719254218446718 ) ) ;
#12787 = CARTESIAN_POINT ( 'NONE',  ( 1.586696308167453662, 1.896558138806573757, 0.5304675795299080843 ) ) ;
#12788 = CARTESIAN_POINT ( 'NONE',  ( 3.901970389206737444, -1.039011544341267745, -1.727992587138134306 ) ) ;
#12789 = CARTESIAN_POINT ( 'NONE',  ( -6.995117189646935962, 10.24838825697502109, 1.199719254218453823 ) ) ;
#12790 = CARTESIAN_POINT ( 'NONE',  ( 3.867818961648523235, 7.734482231890414283, 1.040834085586084257E-14 ) ) ;
#12791 = CARTESIAN_POINT ( 'NONE',  ( -11.88168509644349058, 11.37999999999999901, -1.685788023084331400 ) ) ;
#12792 = CARTESIAN_POINT ( 'NONE',  ( 3.873126987144244193, 2.063651454400210028, -0.7377723227853100196 ) ) ;
#12793 = CARTESIAN_POINT ( 'NONE',  ( -5.582187619986996197, 5.827946089707462640, -0.5328595319416041809 ) ) ;
#12794 = CARTESIAN_POINT ( 'NONE',  ( 2.133698649363345190, -1.256510270340875035, -1.460289853754138445 ) ) ;
#12795 = CARTESIAN_POINT ( 'NONE',  ( -9.622536337397040285, 12.24937836509514710, 1.599625672291281386 ) ) ;
#12796 = CARTESIAN_POINT ( 'NONE',  ( 1.150222622689965446, 3.097854968409793130, 0.7749999999993734123 ) ) ;
#12797 = CARTESIAN_POINT ( 'NONE',  ( 0.1329588055935396196, 0.2493489391296536684, -1.880683181770840262 ) ) ;
#12798 = CARTESIAN_POINT ( 'NONE',  ( 4.584065335196271462, 5.481069324884694005, 1.082531754730549078 ) ) ;
#12799 = CARTESIAN_POINT ( 'NONE',  ( 6.936968151686458306, 11.24487994360957188, 0.7998128361456462443 ) ) ;
#12800 = CARTESIAN_POINT ( 'NONE',  ( 4.774442650306744085, 8.721933525333202653, -0.7998128361456281477 ) ) ;
#12801 = CARTESIAN_POINT ( 'NONE',  ( -4.588905297609556122, 8.492063665195846767, -0.2916239738018167604 ) ) ;
#12802 = CARTESIAN_POINT ( 'NONE',  ( 4.258669648468268676, 7.982548666606070320, 0.7216878364870257245 ) ) ;
#12803 = ORIENTED_EDGE ( 'NONE', *, *, #68702, .F. ) ;
#12805 = CARTESIAN_POINT ( 'NONE',  ( 2.016272687986338852, -2.012595170092303043, 0.05167081324058443031 ) ) ;
#12804 = CARTESIAN_POINT ( 'NONE',  ( 5.460457653299121361, -1.667157065227730106, -0.7818181906407914994 ) ) ;
#12806 = CARTESIAN_POINT ( 'NONE',  ( 3.989890550291860016, 2.181093686755405603, 0.7249921343481547931 ) ) ;
#12808 = CARTESIAN_POINT ( 'NONE',  ( 1.973285428892736171, -0.2338459910692871346, 1.846151439588203935 ) ) ;
#12807 = CARTESIAN_POINT ( 'NONE',  ( -0.02880301295726198432, 6.946859453142047336, -2.868871865197111681 ) ) ;
#12809 = CARTESIAN_POINT ( 'NONE',  ( 3.285556943750000514, -2.763541666188707335, 1.896917185911906500 ) ) ;
#12810 = DIRECTION ( 'NONE',  ( -1.000000000000000000, 0.000000000000000000, 0.000000000000000000 ) ) ;
#12811 = CARTESIAN_POINT ( 'NONE',  ( 5.414289803398987466, -1.912571729023364364, 0.006307610287324683096 ) ) ;
#12812 = CARTESIAN_POINT ( 'NONE',  ( -6.835281999583978418, 11.12624609948998966, -0.7998128361456291469 ) ) ;
#12813 = CARTESIAN_POINT ( 'NONE',  ( -5.153507786970267013, 8.066157280557016307, -1.082531754730549967 ) ) ;
#12815 = CARTESIAN_POINT ( 'NONE',  ( 2.957714569337116295, 1.861795396119047208, -0.1817069356538636715 ) ) ;
#12814 = CARTESIAN_POINT ( 'NONE',  ( 4.388279639374990104, -0.4598052185818923832, -2.039381826187444791 ) ) ;
#12816 = CARTESIAN_POINT ( 'NONE',  ( 7.321039761699430493, 7.643560598178549270, -0.7216878364870257245 ) ) ;
#12817 = CARTESIAN_POINT ( 'NONE',  ( 1.874158809982156670, 3.299964346911599122, 0.3999999999999681033 ) ) ;
#12818 = DIRECTION ( 'NONE',  ( 0.000000000000000000, 8.546850786086437571E-32, 1.000000000000000000 ) ) ;
#12819 = CARTESIAN_POINT ( 'NONE',  ( 4.758271111750849158, 0.6642134669661412527, 1.592074403417756301 ) ) ;
#12820 = CARTESIAN_POINT ( 'NONE',  ( -6.600121851754250812, 6.594563670001734046, 0.7998128361456341429 ) ) ;
#12821 =( NAMED_UNIT ( * ) SI_UNIT ( $, .STERADIAN. ) SOLID_ANGLE_UNIT ( ) );
#12822 = DIRECTION ( 'NONE',  ( -1.000000000000000000, 0.000000000000000000, 0.000000000000000000 ) ) ;
#12823 = CARTESIAN_POINT ( 'NONE',  ( 6.245327377194020535, 0.3399632236478037917, -1.987496870419297013 ) ) ;
#12824 = DIRECTION ( 'NONE',  ( 0.6507913734559627184, -0.7592566023653016805, 0.000000000000000000 ) ) ;
#12825 = CARTESIAN_POINT ( 'NONE',  ( 5.647405056649561494, 1.918175650701968937, -1.016889183816371611 ) ) ;
#12826 = CARTESIAN_POINT ( 'NONE',  ( 4.494645072041675071, -0.4025399330690944133, -1.780595394402582077 ) ) ;
#12827 = CARTESIAN_POINT ( 'NONE',  ( 1.199968502355329703, 0.8001272530510428194, -1.791371145023381350 ) ) ;
#12828 = CARTESIAN_POINT ( 'NONE',  ( 6.298082486376491929, -1.000091913425070311, -1.866304853008766917 ) ) ;
#12829 = EDGE_CURVE ( 'NONE', #201145, #201330, #197257, .T. ) ;
#12830 = CARTESIAN_POINT ( 'NONE',  ( 0.6823417656249917140, 4.155208333674755394, 1.181850606188765695 ) ) ;
#12831 = CARTESIAN_POINT ( 'NONE',  ( 3.998264212729667033, 7.812795105822084807, 0.04491226807220529554 ) ) ;
#12832 = CARTESIAN_POINT ( 'NONE',  ( 6.726816770674637347, 10.99970333242910669, -0.7998128361456291469 ) ) ;
#12833 = CARTESIAN_POINT ( 'NONE',  ( 2.807414684038778141, 1.817529592918063708, -1.092056846721880969 ) ) ;
#12834 = CARTESIAN_POINT ( 'NONE',  ( -3.145128448690317935, 5.652771709238564313, -1.082531754730549967 ) ) ;
#12835 = EDGE_CURVE ( 'NONE', #102037, #84082, #179943, .T. ) ;
#12836 = CARTESIAN_POINT ( 'NONE',  ( 2.093037498677865482, 1.000000000000000888, -11.70868840297833025 ) ) ;
#12837 = CARTESIAN_POINT ( 'NONE',  ( -4.894130264408866893, 6.732904613275549899, -1.443375672974051449 ) ) ;
#12838 = CARTESIAN_POINT ( 'NONE',  ( 1.059532578591013463, 1.690300726139557952, 1.195051122980017144 ) ) ;
#12840 = CARTESIAN_POINT ( 'NONE',  ( 0.7500000000000006661, 14.44791666734946567, -1.299038105676657340 ) ) ;
#12839 = DIRECTION ( 'NONE',  ( -0.000000000000000000, 1.000000000000000000, -0.000000000000000000 ) ) ;
#12842 = VERTEX_POINT ( 'NONE', #209226 ) ;
#12841 = CARTESIAN_POINT ( 'NONE',  ( 2.262617597476920039, 2.220861250988148683, 0.05131716197829398751 ) ) ;
#12843 = CARTESIAN_POINT ( 'NONE',  ( 0.9327830709247152408, -1.816692068203207056, -1.408362870467388950 ) ) ;
#12845 = CARTESIAN_POINT ( 'NONE',  ( 5.752800572348735209, -0.4956410525326099270, -2.002042340502646844 ) ) ;
#12844 = CARTESIAN_POINT ( 'NONE',  ( 4.383363735919856730, 4.008345868194933104, -0.7998128361456211532 ) ) ;
#12847 = CARTESIAN_POINT ( 'NONE',  ( 3.475000000000000533, -1.574999999999999956, 0.000000000000000000 ) ) ;
#12846 = CARTESIAN_POINT ( 'NONE',  ( 5.017399365509065845, 8.011327138806002779, -1.199719254218450271 ) ) ;
#12848 = CARTESIAN_POINT ( 'NONE',  ( 5.417364897112183719, 8.477953592343014932, 1.199719254218451159 ) ) ;
#12849 = CARTESIAN_POINT ( 'NONE',  ( 0.2329586101569866563, 2.046406029004425253, -2.262590835625963415 ) ) ;
#12850 = CARTESIAN_POINT ( 'NONE',  ( 5.688959394570705541, 1.398425918548395153, 1.197878823674280779 ) ) ;
#12851 = CARTESIAN_POINT ( 'NONE',  ( 3.246287715468270108, 5.874753870433235825, 1.199719254218450271 ) ) ;
#12852 = PRESENTATION_STYLE_ASSIGNMENT (( #49640 ) ) ;
#12853 = CARTESIAN_POINT ( 'NONE',  ( 3.012419478190906830, 1.250452035320260835, -1.188195685136491875 ) ) ;
#12854 = CARTESIAN_POINT ( 'NONE',  ( 0.7257964430846426396, 0.8128130212789463904, -1.845628942776005088 ) ) ;
#12855 = CARTESIAN_POINT ( 'NONE',  ( 1.635759689059889554, 0.7259864748365916221, 2.181091778573934103 ) ) ;
#12856 = CARTESIAN_POINT ( 'NONE',  ( -0.6823417656249969321, 4.530208333674755394, -1.181850606188749264 ) ) ;
#12857 = CARTESIAN_POINT ( 'NONE',  ( 2.337552072221838362, -2.021662389422747452, 1.015643474128526291 ) ) ;
#12858 = CARTESIAN_POINT ( 'NONE',  ( 4.688165273298999125, -0.9932770932522380081, 1.857119049063939320 ) ) ;
#12859 = CARTESIAN_POINT ( 'NONE',  ( -7.322812365156824654, 8.676274193172000437, 1.082531754730549078 ) ) ;
#12860 = CARTESIAN_POINT ( 'NONE',  ( 3.655294433216628391, 0.4326292253380575881, -1.715882644387234590 ) ) ;
#12861 = AXIS2_PLACEMENT_3D ( 'NONE', #129983, #127864, #163472 ) ;
#12862 = CARTESIAN_POINT ( 'NONE',  ( 6.661133543015731462, 6.665743976473484267, -0.7998128361456281477 ) ) ;
#12864 = CARTESIAN_POINT ( 'NONE',  ( 0.2172540613933468812, -0.1060665143617581102, 2.289936275665432674 ) ) ;
#12863 = CARTESIAN_POINT ( 'NONE',  ( 4.597623488365603528, 5.496887170248887067, -1.082531754730548412 ) ) ;
#12865 = CARTESIAN_POINT ( 'NONE',  ( 4.980324010294663317, -0.2286266671043569454, -1.826820671449409295 ) ) ;
#12866 = CARTESIAN_POINT ( 'NONE',  ( -4.894657149733403045, 5.669187081899118574, -1.199719254218446718 ) ) ;
#12867 = CARTESIAN_POINT ( 'NONE',  ( 5.138177029454836564, 7.977995053463880382, 1.082531754730558626 ) ) ;
#12868 = CARTESIAN_POINT ( 'NONE',  ( -1.499999999999997780, 4.150000000000021672, 1.214306433183764966E-14 ) ) ;
#12869 = CARTESIAN_POINT ( 'NONE',  ( 4.980524279605372584, -0.2661484459187679064, -2.175167798947100994 ) ) ;
#12870 = CARTESIAN_POINT ( 'NONE',  ( -5.610376637956639101, 5.439860920571172542, 0.000000000000000000 ) ) ;
#12871 = CARTESIAN_POINT ( 'NONE',  ( -11.86145016429273014, 10.19999999999999929, 1.099999999999996980 ) ) ;
#12872 = CARTESIAN_POINT ( 'NONE',  ( 5.100855621065027101, 7.816023350749504495, -1.153872196553248131 ) ) ;
#12873 = CARTESIAN_POINT ( 'NONE',  ( 0.6823417656249917140, 4.842708333674755394, 1.181850606188765695 ) ) ;
#12874 = CARTESIAN_POINT ( 'NONE',  ( 2.930207584894477080, 1.069882305642521514, -1.601919868193351082 ) ) ;
#12875 = CARTESIAN_POINT ( 'NONE',  ( 1.364683531249996529, 8.463541667008065872, 0.7879004041258405033 ) ) ;
#12876 = CARTESIAN_POINT ( 'NONE',  ( -3.741687207691642314, 6.348756928073427730, 1.082531754730560403 ) ) ;
#12877 = CARTESIAN_POINT ( 'NONE',  ( 0.07096481000732741962, 0.8580841460674984988, 2.049194762706497031 ) ) ;
#12878 = CARTESIAN_POINT ( 'NONE',  ( -5.316205630334263965, 7.295602216847000498, -1.443375672974066548 ) ) ;
#12879 = ORIENTED_EDGE ( 'NONE', *, *, #207859, .T. ) ;
#12881 = DIRECTION ( 'NONE',  ( 0.7797859179643623628, 0.6260462619842697141, 0.000000000000000000 ) ) ;
#12880 = CARTESIAN_POINT ( 'NONE',  ( -5.492461627311929995, 5.580495784718250363, 0.000000000000000000 ) ) ;
#12882 = CARTESIAN_POINT ( 'NONE',  ( 5.691725559638619814, 5.534767995866836543, 1.040834085586084257E-14 ) ) ;
#12883 = CARTESIAN_POINT ( 'NONE',  ( 4.769174622299096278, 4.736660945536613099, -0.4712523532527379544 ) ) ;
#12884 = CARTESIAN_POINT ( 'NONE',  ( 0.000000000000000000, -5.199999999999996625, 0.000000000000000000 ) ) ;
#12885 = CARTESIAN_POINT ( 'NONE',  ( -1.364683531250012516, 3.592708333674750509, 0.7879004041258379498 ) ) ;
#12886 = CARTESIAN_POINT ( 'NONE',  ( 2.348798421458723862, 0.4629176777091792983, -1.677682632058958845 ) ) ;
#12887 = CARTESIAN_POINT ( 'NONE',  ( 3.542423274920540432, 7.354853930707762721, -1.734723475976807094E-15 ) ) ;
#12888 = CARTESIAN_POINT ( 'NONE',  ( 0.4847190467827041105, 1.876267867961832980, 0.5731238010058883336 ) ) ;
#12889 = CARTESIAN_POINT ( 'NONE',  ( 0.6823417656249882723, 1.238541667008083547, -1.181850606188749264 ) ) ;
#12890 = CARTESIAN_POINT ( 'NONE',  ( 4.255647627037052709E-16, 0.5000000000000004441, 3.475000000000000089 ) ) ;
#12891 = CARTESIAN_POINT ( 'NONE',  ( -8.947491310014823895, 12.52615806407091803, 1.199719254218462483 ) ) ;
#12892 = CARTESIAN_POINT ( 'NONE',  ( -7.185458225118419584, 7.485382138834033583, 1.040834085586084257E-14 ) ) ;
#12893 = CARTESIAN_POINT ( 'NONE',  ( 5.383715653711652394, 1.448795075966866852, 1.604530791579752202 ) ) ;
#12895 = VERTEX_POINT ( 'NONE', #46781 ) ;
#12894 = CARTESIAN_POINT ( 'NONE',  ( -0.2104748580754201015, 5.720428293583295520, -2.697747842008205943 ) ) ;
#12896 = CARTESIAN_POINT ( 'NONE',  ( 1.364683531249990311, 4.134375000341417028, 1.214306433183764966E-14 ) ) ;
#12897 = CARTESIAN_POINT ( 'NONE',  ( 0.6845637836509765872, -0.2226890396202323152, -1.857165095135074218 ) ) ;
#12898 = CARTESIAN_POINT ( 'NONE',  ( 6.345060247669167097, -0.9239052495037097801, 1.466952517609141138 ) ) ;
#12900 = CARTESIAN_POINT ( 'NONE',  ( 3.280998142716429200, 1.980384277226649559, -0.9389412094223739125 ) ) ;
#12899 = CARTESIAN_POINT ( 'NONE',  ( -1.360316468750032870, 0.6614583336747411613, 0.7853790794158620470 ) ) ;
#12901 = CARTESIAN_POINT ( 'NONE',  ( 2.784532256742262568, -1.187036312555936890, 1.978742884264461654 ) ) ;
#12902 = CARTESIAN_POINT ( 'NONE',  ( 5.624313186929686736, 1.231095119260311677, -1.652465237140358090 ) ) ;
#12903 = CARTESIAN_POINT ( 'NONE',  ( 1.728360517318433542, 0.1903740514868361433, 1.932600189055997619 ) ) ;
#12904 = CARTESIAN_POINT ( 'NONE',  ( -7.348156068482412095, 7.675196289425353591, 1.040834085586084257E-14 ) ) ;
#12905 = CARTESIAN_POINT ( 'NONE',  ( 4.689424523294686509, 8.358602041046323095, -0.7454045323363467368 ) ) ;
#12906 = CARTESIAN_POINT ( 'NONE',  ( -6.776370306708066948, -7.161464053357560644, -6.781144757626046626 ) ) ;
#12907 = EDGE_CURVE ( 'NONE', #40132, #100951, #62610, .T. ) ;
#12908 = CARTESIAN_POINT ( 'NONE',  ( 3.814780496183818315, -0.6684712460508880350, -2.012520831323429515 ) ) ;
#12909 = FILL_AREA_STYLE ('',( #59539 ) ) ;
#12910 = CARTESIAN_POINT ( 'NONE',  ( 2.496720397819631732, -1.994071314890283553, 0.2986276487200872354 ) ) ;
#12911 = CARTESIAN_POINT ( 'NONE',  ( -6.209271164934474285, 6.346497235286081562, 1.040834085586084257E-14 ) ) ;
#12912 = CARTESIAN_POINT ( 'NONE',  ( 5.702238492974306183, -2.206952906645575307, -0.005361432510411765114 ) ) ;
#12913 = CARTESIAN_POINT ( 'NONE',  ( 1.642778471875000035, -1.013541666188708223, -2.845375778867859751 ) ) ;
#12914 = CARTESIAN_POINT ( 'NONE',  ( -2.306635926208834508, -3.112620303657281262, -2.512400949369866687 ) ) ;
#12915 = DIRECTION ( 'NONE',  ( 0.000000000000000000, 1.000000000000000000, 0.000000000000000000 ) ) ;
#12916 = CARTESIAN_POINT ( 'NONE',  ( -7.937372586157736443, 8.224965870130965584, 0.7998128361456341429 ) ) ;
#12918 = FACE_OUTER_BOUND ( 'NONE', #67370, .T. ) ;
#12917 = CARTESIAN_POINT ( 'NONE',  ( -4.688377817131518910, 8.372325690950924937, 0.6434091164432588217 ) ) ;
#12919 = CARTESIAN_POINT ( 'NONE',  ( -10.90754186426655004, 4.636108433425621733, 4.485516275142084730 ) ) ;
#12920 = VERTEX_POINT ( 'NONE', #196213 ) ;
#12921 = CARTESIAN_POINT ( 'NONE',  ( 4.153237585930975584, -1.712380083513395768, -1.146421031332397922 ) ) ;
#12922 = CARTESIAN_POINT ( 'NONE',  ( 4.132297641190314508, 7.622816840561035256, -0.7610026044957002300 ) ) ;
#12923 = CARTESIAN_POINT ( 'NONE',  ( -0.01181297548617084130, -7.619382996155810162, 9.500232605409157927 ) ) ;
#12924 = CARTESIAN_POINT ( 'NONE',  ( -6.091691091241777656, 6.001394449403842479, 0.7998128361456341429 ) ) ;
#12925 = CARTESIAN_POINT ( 'NONE',  ( 3.580727245018202165, -1.354872245433702105, 1.497987768207516668 ) ) ;
#12926 = CARTESIAN_POINT ( 'NONE',  ( 0.7499999999999885647, 1.066666666666687968, -1.299038105676652899 ) ) ;
#12928 = CARTESIAN_POINT ( 'NONE',  ( 8.703971430293332645, 12.13808852110884118, -1.082531754730543083 ) ) ;
#12927 = CARTESIAN_POINT ( 'NONE',  ( -5.167592825464113915, 6.057888380243431570, 1.199719254218452935 ) ) ;
#12929 = CARTESIAN_POINT ( 'NONE',  ( 7.145310649601935182, 8.294949498412453437, -1.199719254218446718 ) ) ;
#12930 = CARTESIAN_POINT ( 'NONE',  ( 3.291920626085430346, -0.8366078139741841557, 1.883634853023412825 ) ) ;
#12931 = CARTESIAN_POINT ( 'NONE',  ( 2.602185585689294367, -0.1948409242511044692, 2.006959980107574371 ) ) ;
#12932 = VERTEX_POINT ( 'NONE', #61944 ) ;
#12933 = EDGE_CURVE ( 'NONE', #157191, #187611, #14224, .T. ) ;
#12934 = DIRECTION ( 'NONE',  ( -0.9755242178752412396, 0.1319352118352180581, 0.1759136157802891343 ) ) ;
#12935 = CARTESIAN_POINT ( 'NONE',  ( 3.669453130792974971, 7.432779085900453886, 1.040834085586084257E-14 ) ) ;
#12936 = AXIS2_PLACEMENT_3D ( 'NONE', #22540, #134215, #200224 ) ;
#12938 = EDGE_LOOP ( 'NONE', ( #193587, #178495, #123906, #201563, #24468, #210579 ) ) ;
#12937 = CARTESIAN_POINT ( 'NONE',  ( -0.2914054381963274709, 8.170846587879108114, -1.980990740193308675 ) ) ;
#12939 = CARTESIAN_POINT ( 'NONE',  ( 2.600935288962639369, 0.9528664403582010056, -1.776738882381201812 ) ) ;
#12940 = CARTESIAN_POINT ( 'NONE',  ( 2.255570300226293234, 0.7868700230135963203, 1.664660379391752043 ) ) ;
#12941 = CARTESIAN_POINT ( 'NONE',  ( 6.340462157465731607, 2.182225300935904055, 0.3281612982340698093 ) ) ;
#12942 = CARTESIAN_POINT ( 'NONE',  ( 6.222266154028957885, 6.224008365980749247, 0.7998128361456352531 ) ) ;
#12943 = CARTESIAN_POINT ( 'NONE',  ( 2.407699484934812784, -0.4761397456576694776, 2.108333575599189214 ) ) ;
#12944 = CARTESIAN_POINT ( 'NONE',  ( -4.039966587192274083, 5.736380323189513852, 1.443375672974064550 ) ) ;
#12945 = CARTESIAN_POINT ( 'NONE',  ( 4.751218706475199838, 0.2043725092088227169, -2.107420708596031922 ) ) ;
#12946 = AXIS2_PLACEMENT_3D ( 'NONE', #173418, #193900, #126865 ) ;
#12947 = CARTESIAN_POINT ( 'NONE',  ( 2.548584303619909175, 2.101849941811538169, -0.9302779420137051725 ) ) ;
#12948 = ORIENTED_EDGE ( 'NONE', *, *, #136122, .F. ) ;
#12949 = CARTESIAN_POINT ( 'NONE',  ( 5.335766472694944973, 4.384919054141800387, -2.499999999999995115 ) ) ;
#12950 = CARTESIAN_POINT ( 'NONE',  ( 1.024039198018782626, 1.117340804906666873, -1.500143343703803422 ) ) ;
#12951 = CARTESIAN_POINT ( 'NONE',  ( 5.401234739183408351, 1.611344100708357097, 1.135629011227519358 ) ) ;
#12953 = CARTESIAN_POINT ( 'NONE',  ( 7.876924059415351564, 12.13356913605253240, -0.7216878364870267237 ) ) ;
#12952 = CARTESIAN_POINT ( 'NONE',  ( -1.201851678989727383E-14, 3.071875000341420137, 1.575800808251672791 ) ) ;
#12955 = CARTESIAN_POINT ( 'NONE',  ( 0.03028722099337673168, -1.361824662662258767, -1.737358624739212543 ) ) ;
#12954 = CARTESIAN_POINT ( 'NONE',  ( -7.172426956829277778, 8.326585190177668849, -1.199719254218452935 ) ) ;
#12956 = EDGE_CURVE ( 'NONE', #155393, #174410, #162653, .T. ) ;
#12957 = CARTESIAN_POINT ( 'NONE',  ( 6.285608408418759119, -1.950803066209889636, 0.6937918898708083093 ) ) ;
#12958 = CARTESIAN_POINT ( 'NONE',  ( 5.900823170445728572, 7.907379670318584353, 1.599625672291267398 ) ) ;
#12959 = CARTESIAN_POINT ( 'NONE',  ( -5.065942953000576843, 9.062017211809330064, -0.7998128361456231517 ) ) ;
#12960 = AXIS2_PLACEMENT_3D ( 'NONE', #121436, #39036, #189541 ) ;
#12961 = CARTESIAN_POINT ( 'NONE',  ( 6.639320575229258559, 7.052241914652472410, 2.701414248926166994 ) ) ;
#12962 = CARTESIAN_POINT ( 'NONE',  ( 5.032083864297879572, 1.014306426666331529, -1.690397665970795105 ) ) ;
#12963 = CARTESIAN_POINT ( 'NONE',  ( 6.533471379370169529, -0.1492333671020330821, 1.986230151431379598 ) ) ;
#12964 = CARTESIAN_POINT ( 'NONE',  ( 0.7499999999999885647, 0.3479166673494848983, -1.299038105676652899 ) ) ;
#12965 = CARTESIAN_POINT ( 'NONE',  ( 4.160959874251066282, -1.711463231979272859, 1.548185629304731581 ) ) ;
#12966 = EDGE_CURVE ( 'NONE', #12329, #157711, #152263, .T. ) ;
#12967 = CARTESIAN_POINT ( 'NONE',  ( 1.973554268250839350, -0.2567932339846226708, 2.046489673661837205 ) ) ;
#12968 = CARTESIAN_POINT ( 'NONE',  ( 7.971831135155394321, 8.402817200543854170, -0.7216878364870267237 ) ) ;
#12969 = CARTESIAN_POINT ( 'NONE',  ( 4.529305835417093640, 7.441884687032027657, -1.199719254218450271 ) ) ;
#12970 = CARTESIAN_POINT ( 'NONE',  ( 3.549202351727371862, 7.362762853649070571, -0.7998128361456362523 ) ) ;
#12971 = CARTESIAN_POINT ( 'NONE',  ( 1.364683531249986537, 2.467708333674753174, -0.7879004041258239610 ) ) ;
#12972 = CARTESIAN_POINT ( 'NONE',  ( 4.415115299905642665, 5.179997933758551554, -1.199719254218450271 ) ) ;
#12973 = CARTESIAN_POINT ( 'NONE',  ( 5.463572716182824252, 7.397254140345190798, 1.443375672974062551 ) ) ;
#12974 = CARTESIAN_POINT ( 'NONE',  ( 4.211506895594858690, -1.802957179857124448, -1.209418758558492568 ) ) ;
#12975 = CARTESIAN_POINT ( 'NONE',  ( -3.246376473470825363, -0.8887487162375362626, 0.5058895364790267912 ) ) ;
#12977 = CARTESIAN_POINT ( 'NONE',  ( 4.265079090171526310, 1.784866007061826298, -0.4516350764028759235 ) ) ;
#12976 = CARTESIAN_POINT ( 'NONE',  ( -4.609409038966253647, 4.479991421656468908, -0.7216878364870207285 ) ) ;
#12979 = CARTESIAN_POINT ( 'NONE',  ( 6.720655732516647163, 3.705577233864749687, 2.340827588962008488 ) ) ;
#12978 = CARTESIAN_POINT ( 'NONE',  ( -11.89844258446855285, 11.32852689329959439, 1.560502987793273233 ) ) ;
#12980 = CARTESIAN_POINT ( 'NONE',  ( 5.548420995840112724, -1.728225626343689925, 1.347513067664840358 ) ) ;
#12981 = CARTESIAN_POINT ( 'NONE',  ( -10.98550897202509269, 11.25719568827052974, -1.591908179352835351 ) ) ;
#12982 = CARTESIAN_POINT ( 'NONE',  ( 6.227429363453246935, -2.132905367568146637, 0.7551758973065140212 ) ) ;
#12983 = ORIENTED_EDGE ( 'NONE', *, *, #167761, .F. ) ;
#12984 = CARTESIAN_POINT ( 'NONE',  ( -4.031038109533945146, 7.773819255970239261, -0.5157005294549130703 ) ) ;
#12985 = CARTESIAN_POINT ( 'NONE',  ( 5.004104291928844539, 8.031804922028364047, 1.127571413376940335 ) ) ;
#12986 = CARTESIAN_POINT ( 'NONE',  ( -6.441532379824190357, 6.687744995982559892, 0.7216878364870257245 ) ) ;
#12987 = CARTESIAN_POINT ( 'NONE',  ( 5.085717018901939390, 5.105960408239938353, 0.000000000000000000 ) ) ;
#12988 = CARTESIAN_POINT ( 'NONE',  ( 0.8656337812406755816, 0.8672032905003168590, 1.542741919674812223 ) ) ;
#12989 = CARTESIAN_POINT ( 'NONE',  ( 5.127594652646677353, -0.2932247039480195827, 1.991498814599843792 ) ) ;
#12990 = CARTESIAN_POINT ( 'NONE',  ( 5.133733721068893807, 9.141106441222381918, 1.040834085586084257E-14 ) ) ;
#12991 = CARTESIAN_POINT ( 'NONE',  ( 4.577239374156605756, 0.002566705667105330900, -2.106147099847696325 ) ) ;
#12992 = CARTESIAN_POINT ( 'NONE',  ( 2.319824818950954270, 0.9007672528749611773, -1.690582045118453225 ) ) ;
#12993 = CARTESIAN_POINT ( 'NONE',  ( 2.361091307074211887, 5.906356958228550447, 0.7998128361456462443 ) ) ;
#12994 = CARTESIAN_POINT ( 'NONE',  ( 2.682036910502568539, -1.131707915740775672, -1.611748346588251168 ) ) ;
#12995 = CARTESIAN_POINT ( 'NONE',  ( 5.256120111591911837, 0.8147005317804748570, -1.848364005614275163 ) ) ;
#12996 = CARTESIAN_POINT ( 'NONE',  ( 1.410794581852807150, 1.648159533202856686, 0.8848386531258023435 ) ) ;
#12999 = ORIENTED_EDGE ( 'NONE', *, *, #158482, .F. ) ;
#12998 = CARTESIAN_POINT ( 'NONE',  ( 0.9492982845318720386, -1.727743609841876360, 0.8201845251225792222 ) ) ;
#12997 = CARTESIAN_POINT ( 'NONE',  ( 4.898908426394765314, 1.431408964483871227, -0.9620984105884394788 ) ) ;
#13001 = CARTESIAN_POINT ( 'NONE',  ( 3.212919216758630014, 6.692230152952963529, 0.000000000000000000 ) ) ;
#13000 = CARTESIAN_POINT ( 'NONE',  ( 1.383733252933561086, 2.037972573443189717, -0.8472329510355591786 ) ) ;
#13002 = CARTESIAN_POINT ( 'NONE',  ( 1.364683531249986537, 1.967708333674750731, -0.7879004041258239610 ) ) ;
#13003 = CARTESIAN_POINT ( 'NONE',  ( 9.023114925094663619, 10.48572115315399245, 1.199719254218453823 ) ) ;
#13004 = CARTESIAN_POINT ( 'NONE',  ( 11.48243876534946217, 12.30000000000000071, -3.200000000000001510 ) ) ;
#13005 = CARTESIAN_POINT ( 'NONE',  ( 0.9486429539266817423, 3.167910930033676298, -1.028101543437250465 ) ) ;
#13006 = CARTESIAN_POINT ( 'NONE',  ( -4.303094902415906198, 7.389312076987425648, -1.073240500945132236 ) ) ;
#13007 = CARTESIAN_POINT ( 'NONE',  ( 6.121949425127414024, 2.040613181561203859, -0.3481179853092666865 ) ) ;
#13008 = CARTESIAN_POINT ( 'NONE',  ( 1.012269475826784060, 2.068064858651061932, -0.09981174449213289779 ) ) ;
#13009 = CARTESIAN_POINT ( 'NONE',  ( -0.7500000000000215383, 1.941666666666688634, 1.299038105676659116 ) ) ;
#13010 = CARTESIAN_POINT ( 'NONE',  ( 6.498435699651741615, 6.475929825882159818, -0.7998128361456281477 ) ) ;
#13011 = CARTESIAN_POINT ( 'NONE',  ( -6.551614543901706611, 8.666636272683888365, 1.599625672291283607 ) ) ;
#13012 = CARTESIAN_POINT ( 'NONE',  ( 4.030516805012513082, 7.924296382481737844, 0.000000000000000000 ) ) ;
#13013 = CARTESIAN_POINT ( 'NONE',  ( 4.951869195850400196, -1.499954228463634465, -1.499123153458590929 ) ) ;
#13014 = CARTESIAN_POINT ( 'NONE',  ( 3.790386463472274148, 6.579812086429759788, 1.199719254218452047 ) ) ;
#13015 = CARTESIAN_POINT ( 'NONE',  ( -0.6823417656249969321, 3.217708333674754062, -1.181850606188749264 ) ) ;
#13016 = CARTESIAN_POINT ( 'NONE',  ( -1.500000000000013101, 3.879166666666685970, -0.8660254037844313801 ) ) ;
#13018 = CARTESIAN_POINT ( 'NONE',  ( 3.816783937446950770, 4.411668334231586996, 1.199719254218464037 ) ) ;
#13017 = DIRECTION ( 'NONE',  ( -5.551115123125764829E-17, 0.000000000000000000, 1.000000000000000000 ) ) ;
#13019 = CARTESIAN_POINT ( 'NONE',  ( 4.376327261493318410, -0.3474131038204917310, 1.985796694155849362 ) ) ;
#13020 = CARTESIAN_POINT ( 'NONE',  ( 3.503066848181853654, -0.1354201214893405170, 1.910964455010273344 ) ) ;
#13021 = DIRECTION ( 'NONE',  ( 0.000000000000000000, -0.7071067811865540120, -0.7071067811865410224 ) ) ;
#13022 = CARTESIAN_POINT ( 'NONE',  ( 2.999763140970079345, -2.188934734890151113, 0.1099877568606702771 ) ) ;
#13023 = CARTESIAN_POINT ( 'NONE',  ( -0.1399997263889594112, -0.002789056014654289761, -2.000146600338557956 ) ) ;
#13024 = CARTESIAN_POINT ( 'NONE',  ( -1.500000000000013101, 0.2020833340161521663, 0.8660254037844403729 ) ) ;
#13025 = CARTESIAN_POINT ( 'NONE',  ( 4.851819109577236055, -1.426696570994885116, -1.420647396805594820 ) ) ;
#13026 = CARTESIAN_POINT ( 'NONE',  ( -6.775324078527193983, 8.927630729746953264, -1.599625672291263179 ) ) ;
#13028 = CARTESIAN_POINT ( 'NONE',  ( 5.378551862015316765, -0.5151900214499178787, -2.053461258077380336 ) ) ;
#13027 = CARTESIAN_POINT ( 'NONE',  ( -2.304522924643024773, 5.632434478818063361, 0.7216878364870317197 ) ) ;
#13029 = CARTESIAN_POINT ( 'NONE',  ( -0.6823417656250003738, 8.963541667008065872, 1.181850606188754593 ) ) ;
#13031 = CARTESIAN_POINT ( 'NONE',  ( -6.607619761813764647, 8.802252036906432764, 1.599625672291269396 ) ) ;
#13030 = CARTESIAN_POINT ( 'NONE',  ( 3.034800296023100419, -1.842769725714489493, 0.9876625208589999705 ) ) ;
#13033 = ORIENTED_EDGE ( 'NONE', *, *, #58125, .T. ) ;
#13032 = CARTESIAN_POINT ( 'NONE',  ( 2.168594647197068070, -1.575507694510763335, -0.7022964154167319339 ) ) ;
#13034 = CARTESIAN_POINT ( 'NONE',  ( 5.484674493353773883, -1.343714522216314489, 1.640574901390474460 ) ) ;
#13035 = CARTESIAN_POINT ( 'NONE',  ( 4.625302960556422427, 8.547937220624488575, 1.040834085586084257E-14 ) ) ;
#13036 = CARTESIAN_POINT ( 'NONE',  ( 0.4465194593917843902, 3.080450244942134486, 0.4155024747329351120 ) ) ;
#13037 = CARTESIAN_POINT ( 'NONE',  ( -0.1298625177950053222, -9.252181021551008300, 9.620122301472909143 ) ) ;
#13038 = CARTESIAN_POINT ( 'NONE',  ( 6.993308306550549247, 7.053281200597435685, 1.040834085586084257E-14 ) ) ;
#13039 = ORIENTED_EDGE ( 'NONE', *, *, #136104, .F. ) ;
#13040 = CARTESIAN_POINT ( 'NONE',  ( 1.279995097189621012, 4.016078936648800557, -0.4728108786798641550 ) ) ;
#13041 = EDGE_CURVE ( 'NONE', #78057, #62036, #180828, .T. ) ;
#13043 = CARTESIAN_POINT ( 'NONE',  ( 1.435880962511564718, -1.006192904286895340, -1.506089461148002018 ) ) ;
#13042 = CARTESIAN_POINT ( 'NONE',  ( 4.193214648376505593, 8.114110533073061404, 0.000000000000000000 ) ) ;
#13044 = CARTESIAN_POINT ( 'NONE',  ( -6.175902666224832416, 7.163973517805802160, -1.199719254218446718 ) ) ;
#13045 = VECTOR ( 'NONE', #20795, 1000.000000000000000 ) ;
#13046 = CARTESIAN_POINT ( 'NONE',  ( 3.517450787741589036, 6.191110788085444128, -1.199719254218446718 ) ) ;
#13047 = EDGE_LOOP ( 'NONE', ( #78155, #136377, #87269, #184872 ) ) ;
#13048 = CARTESIAN_POINT ( 'NONE',  ( 4.389807875774629942, 8.343469298370917997, 0.7998128361456271485 ) ) ;
#13049 = CARTESIAN_POINT ( 'NONE',  ( 2.736723853829028830, 1.706320744115387811, 0.6085963735071827641 ) ) ;
#13050 = CARTESIAN_POINT ( 'NONE',  ( -4.711399975388157024, 5.243183351676022674, -1.000706908094962433 ) ) ;
#13051 = CARTESIAN_POINT ( 'NONE',  ( 0.000000000000000000, -5.223431457505076203, 0.000000000000000000 ) ) ;
#13052 = CARTESIAN_POINT ( 'NONE',  ( 4.847318722290685500, 6.704483692258053296, 1.249926399124022147 ) ) ;
#13053 = CARTESIAN_POINT ( 'NONE',  ( 3.683913666659529795, -1.106983821303194171, -1.495880402381715824 ) ) ;
#13054 = CARTESIAN_POINT ( 'NONE',  ( 1.440887319015681012, -1.643870157486097217, -0.9831960898977005758 ) ) ;
#13055 = CARTESIAN_POINT ( 'NONE',  ( 6.821331454403446237, -0.1310627394537598467, 1.896496729248610125 ) ) ;
#13056 = CARTESIAN_POINT ( 'NONE',  ( -11.04536101718726293, 10.90000000000000036, 1.099999999999996758 ) ) ;
#13057 = CARTESIAN_POINT ( 'NONE',  ( -0.4461809497497640775, 3.122791860410086606, 1.949595486268987043 ) ) ;
#13059 = CIRCLE ( 'NONE', #68404, 10.86343145750506700 ) ;
#13058 = CIRCLE ( 'NONE', #44172, 3.100000000000000089 ) ;
#13060 = CARTESIAN_POINT ( 'NONE',  ( 4.594558193676899549, 8.374302254291812631, 0.02480325318809234458 ) ) ;
#13061 = CARTESIAN_POINT ( 'NONE',  ( -4.117449517434937256, 3.977532912766735151, 0.4210360159884243281 ) ) ;
#13062 = CARTESIAN_POINT ( 'NONE',  ( 8.432808358020025707, 9.900993174853955026, 1.082531754730558626 ) ) ;
#13063 = CARTESIAN_POINT ( 'NONE',  ( 5.770349169015823954, -0.8820018971720828826, -1.760941755123719421 ) ) ;
#13064 = CARTESIAN_POINT ( 'NONE',  ( -5.766295404513795297, 5.621766148221195358, 0.7998128361456341429 ) ) ;
#13065 = CARTESIAN_POINT ( 'NONE',  ( -9.579665964947855272, -7.246166700193438892, 1.021860547567587929E-14 ) ) ;
#13066 = CARTESIAN_POINT ( 'NONE',  ( 6.667925998804712151, -1.351855065013835455, 1.725503752137508284 ) ) ;
#13067 = PLANE ( 'NONE',  #136646 ) ;
#13068 = CARTESIAN_POINT ( 'NONE',  ( 5.649420354817641154, -1.518837414639911065, -1.184835060848010713 ) ) ;
#13069 = CARTESIAN_POINT ( 'NONE',  ( -6.398558430645608475, 9.552403038140164782, -1.199719254218440723 ) ) ;
#13070 = CARTESIAN_POINT ( 'NONE',  ( 1.184280053745472738, -1.780106929851841491, -0.4042017716930704219 ) ) ;
#13071 = CARTESIAN_POINT ( 'NONE',  ( 2.157103830005083100, -1.704838622333640030, 1.401371054633032909 ) ) ;
#13072 = CARTESIAN_POINT ( 'NONE',  ( -6.328041841479842056, 6.870487382198048998, 0.6860574420480938240 ) ) ;
#13073 = CARTESIAN_POINT ( 'NONE',  ( -0.01753026575586694516, -1.247696154478775021, 1.449428981083925150 ) ) ;
#13074 = ORIENTED_EDGE ( 'NONE', *, *, #68041, .T. ) ;
#13075 = ORIENTED_EDGE ( 'NONE', *, *, #194704, .T. ) ;
#13076 = CARTESIAN_POINT ( 'NONE',  ( 0.5726248362980547180, 1.360856580973464069, -1.424029402571887148 ) ) ;
#13077 = CARTESIAN_POINT ( 'NONE',  ( 1.171315778946733888, 1.157996810922466313, 1.558895349155087873 ) ) ;
#13078 = ORIENTED_EDGE ( 'NONE', *, *, #149988, .F. ) ;
#13079 = CARTESIAN_POINT ( 'NONE',  ( 0.2982036909132765867, -1.844429998007334648, 0.8144978490535054183 ) ) ;
#13081 = CARTESIAN_POINT ( 'NONE',  ( 5.348444835920818541, -1.846650980718677726, -0.2298375257220597323 ) ) ;
#13080 = CARTESIAN_POINT ( 'NONE',  ( -6.317173229324657413, 6.334733287159020954, 0.000000000000000000 ) ) ;
#13082 = CARTESIAN_POINT ( 'NONE',  ( 4.766573523656222555, 7.718696989977711809, 1.199719254218452047 ) ) ;
#13083 = CARTESIAN_POINT ( 'NONE',  ( -1.806654366501805775, 2.518449987798942136, 2.500000000000000444 ) ) ;
#13084 = CARTESIAN_POINT ( 'NONE',  ( 4.065119107856408398, 3.982580166312400749, -0.7566012008942292200 ) ) ;
#13085 = CARTESIAN_POINT ( 'NONE',  ( -3.554208825076827782, 7.298327395898266623, 0.7998128361456341429 ) ) ;
#13086 = CARTESIAN_POINT ( 'NONE',  ( -7.435720902452096936, 7.639705572474380091, 0.000000000000000000 ) ) ;
#13088 = B_SPLINE_CURVE_WITH_KNOTS ( 'NONE', 3,
 ( #43907, #194396, #79581, #82776 ),
 .UNSPECIFIED., .F., .F.,
 ( 4, 4 ),
 ( 2.669248499352272927E-16, 7.241384396125430216E-05 ),
 .UNSPECIFIED. ) ;
#13087 = CARTESIAN_POINT ( 'NONE',  ( 1.734175692058033347, 2.168326105380265378, 0.3173973903456903112 ) ) ;
#13089 = CARTESIAN_POINT ( 'NONE',  ( 2.901081683644312736, 6.328419697652925002, 0.7216878364870338292 ) ) ;
#13090 = DIRECTION ( 'NONE',  ( 0.000000000000000000, 0.000000000000000000, 1.000000000000000000 ) ) ;
#13091 = DIRECTION ( 'NONE',  ( 0.000000000000000000, 1.000000000000000000, 0.000000000000000000 ) ) ;
#13092 = CARTESIAN_POINT ( 'NONE',  ( 1.875362892791394787, 1.747422460009705913, -0.5287960245906262458 ) ) ;
#13093 = CARTESIAN_POINT ( 'NONE',  ( -3.002240950422295995, 5.590032644546251817, -1.199719254218452935 ) ) ;
#13094 = CARTESIAN_POINT ( 'NONE',  ( -3.578462479003122976, 6.262291094557191684, 1.199719254218464037 ) ) ;
#13095 = AXIS2_PLACEMENT_3D ( 'NONE', #34513, #919, #49703 ) ;
#13096 = CARTESIAN_POINT ( 'NONE',  ( -0.2903009011402963302, 2.705340922360735423, -2.053590887664075382 ) ) ;
#13097 = CARTESIAN_POINT ( 'NONE',  ( 6.509000000000034980, 7.629137130509102249, 2.699999999999993516 ) ) ;
#13098 = CARTESIAN_POINT ( 'NONE',  ( 8.971744963941056028, 11.49012176272984931, 1.599625672291281386 ) ) ;
#13099 = CARTESIAN_POINT ( 'NONE',  ( 1.348133503156129454, 1.924256495421622359, 0.09534579948072999245 ) ) ;
#13100 = CARTESIAN_POINT ( 'NONE',  ( 5.946142449018281262, -0.8852437533515828960, 1.750773106858094952 ) ) ;
#13102 = EDGE_CURVE ( 'NONE', #12133, #207685, #12111, .T. ) ;
#13101 = PRESENTATION_LAYER_ASSIGNMENT (  '', '', ( #196501 ) ) ;
#13103 = CARTESIAN_POINT ( 'NONE',  ( -8.864333505236459132, 9.236143932397675727, 1.040834085586084257E-14 ) ) ;
#13104 = CARTESIAN_POINT ( 'NONE',  ( 5.555090253297246150, 7.504024600312024340, 1.599625672291267398 ) ) ;
#13105 = CARTESIAN_POINT ( 'NONE',  ( 5.319949580897746166, 1.306013235697962571, -1.759773446019400778 ) ) ;
#13106 = ADVANCED_FACE ( 'NONE', ( #128103 ), #114302, .T. ) ;
#13107 = B_SPLINE_CURVE_WITH_KNOTS ( 'NONE', 3,
 ( #139886, #205916, #136679, #57550, #202704, #123708, #117968, #115830, #133124, #149338 ),
 .UNSPECIFIED., .F., .F.,
 ( 4, 1, 1, 1, 1, 1, 1, 4 ),
 ( 0.000000000000000000, 0.09487947018404768729, 0.1878442364269655440, 0.2584026419818104547, 0.3617053504666527530, 0.5211417612611924932, 0.7337075935910832847, 1.000000000000000000 ),
 .UNSPECIFIED. ) ;
#13108 = CARTESIAN_POINT ( 'NONE',  ( 4.684505768721569652, 5.424010470718658716, -1.199719254218452047 ) ) ;
#13109 = CARTESIAN_POINT ( 'NONE',  ( 3.854399998794607818, -2.067664388167046674, -0.1065051105964970740 ) ) ;
#13111 = CARTESIAN_POINT ( 'NONE',  ( 1.364683531249988757, 1.196875000341421469, 0.000000000000000000 ) ) ;
#13110 = CARTESIAN_POINT ( 'NONE',  ( -4.624999999999992895, 3.300000000000025135, 1.214306433183764966E-14 ) ) ;
#13112 = ORIENTED_EDGE ( 'NONE', *, *, #188476, .F. ) ;
#13113 = CARTESIAN_POINT ( 'NONE',  ( 4.201969167805962968, 2.101520711257957252, 0.9317802909727909144 ) ) ;
#13115 = ORIENTED_EDGE ( 'NONE', *, *, #35015, .T. ) ;
#13114 = CARTESIAN_POINT ( 'NONE',  ( 5.978782553946477840, 9.919070713005490703, 1.040834085586084257E-14 ) ) ;
#13117 = CARTESIAN_POINT ( 'NONE',  ( -3.285556943750000070, -0.8093749995220431703, 0.000000000000000000 ) ) ;
#13116 = CARTESIAN_POINT ( 'NONE',  ( 5.804299160426222848, 7.865044668620976509, -1.443375672974078761 ) ) ;
#13118 = CARTESIAN_POINT ( 'NONE',  ( -7.653681110113423891, -5.402328468025351604, -7.847520364415503380 ) ) ;
#13119 = CARTESIAN_POINT ( 'NONE',  ( 3.661996979482002867, -1.303408580024501218, 1.439711300692345652 ) ) ;
#13120 = VERTEX_POINT ( 'NONE', #144310 ) ;
#13121 = CARTESIAN_POINT ( 'NONE',  ( 4.690757960648224589, 6.495636925554817864, 1.443375672974062551 ) ) ;
#13122 = ADVANCED_FACE ( 'NONE', ( #210308 ), #111832, .T. ) ;
#13123 = VERTEX_POINT ( 'NONE', #109699 ) ;
#13124 = CARTESIAN_POINT ( 'NONE',  ( 4.957238921819991262, -1.637161358497842389, 0.9882132959125531357 ) ) ;
#13125 = DIRECTION ( 'NONE',  ( -1.276756478318932585E-15, 1.000000000000000000, -1.665334536937738262E-16 ) ) ;
#13126 = CARTESIAN_POINT ( 'NONE',  ( 6.563511714949607168, 0.2886701521849396879, -1.700279369998755508 ) ) ;
#13127 = CARTESIAN_POINT ( 'NONE',  ( 5.014861385384292269, 0.1531656238677771009, 2.010801456750747285 ) ) ;
#13128 = CARTESIAN_POINT ( 'NONE',  ( -3.325722479477156934, 7.699077257575940081, 2.499999999999999112 ) ) ;
#13129 = CARTESIAN_POINT ( 'NONE',  ( 2.227434312139275896, 0.001603268854937638837, 2.207063162490217056 ) ) ;
#13131 = CARTESIAN_POINT ( 'NONE',  ( -3.662110889467009578, 7.286563447771212232, 0.7216878364870338292 ) ) ;
#13130 = CARTESIAN_POINT ( 'NONE',  ( -8.292783513053063160, 12.82666453187061073, 0.7998128361456481317 ) ) ;
#13133 = CARTESIAN_POINT ( 'NONE',  ( 0.2327837997007513038, -1.621012357304358220, 0.7108589729635225174 ) ) ;
#13132 = CARTESIAN_POINT ( 'NONE',  ( 2.203177794981598492, -0.4570653145323905764, 2.039892330567660839 ) ) ;
#13134 = CARTESIAN_POINT ( 'NONE',  ( 6.082657761774013849, -0.6767167302549759178, 1.899617564980569995 ) ) ;
#13136 = CARTESIAN_POINT ( 'NONE',  ( 3.556809736639905406, -2.021263576298555797, -1.081171400725000398 ) ) ;
#13135 = CARTESIAN_POINT ( 'NONE',  ( 6.059568310664962709, 6.034194215389424798, 0.7998128361456352531 ) ) ;
#13137 = CARTESIAN_POINT ( 'NONE',  ( 0.7611566575390321665, 0.8540426286860869354, 1.516288903859766890 ) ) ;
#13138 = AXIS2_PLACEMENT_3D ( 'NONE', #37985, #7592, #185280 ) ;
#13139 = CARTESIAN_POINT ( 'NONE',  ( -2.609770642201835855, -0.3830433331901521576, -0.1872689674646474400 ) ) ;
#13140 = CARTESIAN_POINT ( 'NONE',  ( 0.9481301099739076754, 1.159027798429014045, 1.289721149823976676 ) ) ;
#13141 = CARTESIAN_POINT ( 'NONE',  ( 1.360316468749939833, 0.02604166700813021276, 0.7853790794158660438 ) ) ;
#13142 = CARTESIAN_POINT ( 'NONE',  ( -11.44779965693287416, 12.60313923201275799, 3.599999932275866676 ) ) ;
#13143 =( BOUNDED_SURFACE ( )  B_SPLINE_SURFACE ( 3, 3, ( 
 ( #28499, #94590, #160632, #66020, #12233, #45839, #42643, #33555, #111959, #98567, #16213, #148390, #132169, #17282, #198175, #83358, #207239, #174776, #168884, #70293, #19423, #4223, #152638, #37823, #85502, #119136, #136409, #22615, #53001, #184061, #121290, #150526, #50877, #202425, #67090, #151589, #186190, #117000, #201360, #87645, #137477, #1025, #20488, #54080, #203491, #200300, #134293, #38892, #120216, #2087, #103901, #149443, #100686, #34616, #153715, #169947, #133225, #5283, #3156, #21535, #199230, #71361, #55144, #187266, #166764, #104978, #185118, #18359, #182999, #84437, #35679, #171018, #36743, #86574, #68161, #69228, #102829, #51952, #118074, #135346, #101757, #167824, #191516, #110356, #89802, #59399, #157992, #26890, #10631, #208830, #43181, #142823, #126617, #76706, #58339, #174250, #189401, #25822, #106076, #88724, #156923, #173177, #155846, #92994, #7433, #140697, #73514, #125555, #154782, #9581, #175303, #109294, #123439, #206711, #8512, #159038, #44235, #192580, #139616, #204560, #172099, #122372, #124495, #205639, #60460, #190454, #176360, #42113, #6366, #207772, #41043, #188329, #72435, #138536, #56208, #57278, #39969, #107152, #23692, #24757, #90859, #74593, #108225, #91932, #75657, #141764, #27967, #163303, #131903, #12758, #113552, #62586, #161172, #177422, #146010, #48495, #127696, #46361, #114614, #197911, #143898, #14884, #95123, #148127, #80979, #78832, #144953, #194722, #210959, #111418, #61530, #213089, #147068, #128749, #94061, #160101, #195800, #196857, #162241, #11704, #96190, #112481, #178490, #180605, #64719, #193656, #214127, #82033, #30100, #15950, #65756, #29040, #130861, #212021, #32230, #77778, #13827, #45299, #179555, #79901, #63664, #47437, #129818, #209892, #31176, #97249, #98301, #164366, #49539, #115665, #181659, #71100, #33286, #200041, #51692, #117814, #68965, #37559, #3960, #36485, #85236, #54883, #83094, #183804, #2892, #35414, #135084, #152382, #101492, #52738, #84172, #99370, #150261, #167562, #201097, #165422, #21280, #19162, #87385, #18084, #70028, #136143, #103639, #151324, #50605, #118872, #184858, #153453, #102562, #182730, #17018, #116731, #149173, #132959, #137218, #34349, #168622, #20224, #5026, #86310, #202161, #53819, #119949, #185924, #169691, #203239, #750, #66816, #198962, #100422, #166493, #1829, #67888, #134033, #155589, #92743, #122104, #22350, #124243, #38635, #57020, #157735, #88462, #172918, #59144, #109036, #187004, #206454, #107971, #175055, #171833, #105808, #10384, #190202, #188069, #41861, #121037, #72172, #6102, #125302, #91682, #104713, #191261, #123188, #9332, #170761, #173999, #25571, #75404, #138280, #141517, #24493, #204295, #154523, #55951, #7173, #42926, #90604, #58081, #140443, #189149, #8256, #207525, #39698, #40786, #208575, #23426, #26642, #142568, #89537, #158787, #76460, #73244, #139351, #205381, #106891, #156664, #74339, #48257, #29862, #145778, #160925, #211781, #77527, #60208, #128511, #144712, #61284, #64484, #193416, #112239, #45060, #30936, #126369, #129571, #146828, #97012, #94872, #178249, #194479, #14646, #15709, #164126, #111171, #176116, #143648, #93810, #95945, #177172, #80740, #162000, #130626, #13589, #192328, #62350, #46122, #196618, #11454, #79663, #110105, #98071, #63419, #195558, #47194, #163065, #27716, #113309 ),
 ( #28789, #12519, #81795, #179315, #127445, #212847, #43987, #209643, #159851, #114371, #180366, #78592, #31990, #147878, #210724, #197665, #134835, #2640, #200838, #165174, #52489, #117554, #99124, #65517, #33047, #100174, #3701, #183548, #84985, #18901, #1573, #101232, #184606, #132711, #67634, #87120, #131662, #102302, #21024, #501, #36223, #68713, #152133, #135885, #119689, #168375, #53556, #37303, #201904, #35155, #151076, #166239, #118619, #16768, #213894, #133781, #83912, #66569, #69777, #198716, #51434, #50362, #19972, #49309, #86056, #185674, #103377, #34103, #167314, #199789, #169439, #115426, #181417, #116485, #82852, #148928, #182474, #17829, #150003, #107714, #188885, #157480, #40526, #153191, #155328, #6912, #9075, #104453, #72989, #202982, #191006, #122927, #139092, #205119, #41603, #106630, #42673, #140174, #89280, #172659, #25318, #24234, #74083, #23164, #7992, #156405, #173741, #56762, #90336, #206196, #26383, #57824, #187813, #125051, #154268, #123986, #189953, #4763, #54623, #91419, #75149, #141259, #207267, #58898, #108781, #174807, #55686, #70840, #121842, #136956, #120770, #186750, #38372, #170500, #22083, #204037, #88194, #5842, #71913, #171567, #138022, #39439, #105533, #64235, #29605, #93551, #76206, #175865, #208326, #43738, #196369, #159595, #95691, #211527, #127189, #126112, #30678, #195304, #59957, #11193, #63162, #61028, #130379, #158534, #143386, #78338, #94623, #160666, #113053, #14389, #92495, #13337, #48009, #77274, #177992, #193156, #209384, #27453, #210465, #179059, #192072, #110910, #96761, #114126, #109851, #79412, #44806, #212597, #145529, #176916, #28531, #12261, #144461, #62103, #128262, #129328, #46935, #194224, #10131, #142316, #45868, #162812, #111990, #161746, #80480, #146580, #180118, #118373, #84741, #131416, #3463, #85810, #132471, #19731, #151889, #115178, #150829, #149754, #184361, #81543, #66326, #197416, #183301, #99933, #1331, #51182, #16518, #147626, #82601, #65270, #165995, #168129, #213644, #100980, #31743, #135640, #97817, #50118, #116238, #182228, #133533, #102064, #68470, #181173, #49058, #32798, #201661, #98872, #34908, #2391, #198473, #164925, #35983, #134597, #148686, #255, #200598, #33852, #69533, #163881, #17580, #83663, #67392, #199540, #52245, #53310, #15456, #167069, #119442, #117305, #18661, #5584, #104204, #120522, #89030, #205951, #70593, #203796, #57583, #141008, #86877, #172404, #38132, #91169, #23992, #170251, #87944, #137778, #21836, #54384, #4520, #156160, #90095, #71664, #185429, #103132, #138845, #139924, #105283, #169190, #39192, #154018, #55442, #123741, #7741, #136708, #157228, #25067, #121594, #173491, #8823, #186501, #73828, #155085, #189702, #20782, #187566, #202733, #122677, #171319, #6671, #204862, #22914, #152944, #72748, #56517, #188640, #107465, #40270, #106381, #37048, #74899, #41355, #207016, #58647, #209137, #12016, #195043, #161496, #193966, #28277, #212338, #26135, #126935, #160411, #60776, #78089, #95447, #192893, #210210, #27200, #124801, #93307, #44549, #144214, #108529, #178810, #176665, #30425, #175613, #13076, #79156, #46680, #143143, #208079, #110664, #94371, #96510, #61846, #125866, #174559, #128013, #45614, #111730, #177737, #145272, #43488, #29352, #190760, #42424, #211279, #146323, #191825, #62902, #129072, #112798, #162560 ),
 ( #92247, #14132, #80224, #158295, #9886, #75962, #142065, #59706, #159342, #109607, #10939, #77014, #99672, #47759, #118119, #115983, #184104, #114920, #100731, #18404, #200344, #82345, #147374, #148436, #132211, #35724, #1074, #65022, #113873, #213400, #179868, #15206, #167869, #131177, #67139, #183046, #98615, #97568, #2132, #166810, #31493, #197167, #34661, #32540, #101800, #130132, #180919, #49856, #66069, #198220, #84480, #51993, #63978, #199281, #19467, #48803, #149491, #164676, #16260, #4, #181971, #150570, #163625, #33601, #68207, #85543, #81297, #50923, #165741, #151634, #117049, #17328, #83409, #133273, #134339, #196120, #36786, #191299, #59178, #103945, #3200, #135383, #171058, #175091, #137515, #136451, #42967, #201404, #141551, #9368, #207558, #168929, #125336, #121332, #102870, #69269, #20532, #169988, #10422, #187308, #91718, #22654, #5323, #105018, #109075, #202468, #71403, #93849, #53043, #26679, #27754, #4264, #92781, #75439, #158826, #142605, #126404, #76494, #60247, #44023, #208614, #38935, #157768, #21574, #192364, #86614, #119176, #203532, #87680, #70334, #110141, #54121, #55186, #120257, #176154, #185162, #152682, #186233, #37867, #153753, #211818, #79698, #114405, #115463, #49344, #144750, #61324, #177211, #193455, #63455, #210762, #180404, #195594, #164160, #47229, #159887, #162034, #13625, #15745, #111208, #145811, #209680, #197702, #129609, #113346, #179351, #48293, #30973, #181454, #146866, #95982, #97048, #32023, #163101, #80778, #29896, #14681, #212887, #98108, #64518, #130664, #196653, #33084, #81830, #194512, #131696, #160961, #127484, #147913, #77566, #213929, #65551, #45099, #11494, #143688, #28824, #94912, #12551, #78626, #62382, #128546, #46160, #112273, #178288, #100207, #102338, #99159, #50398, #198751, #103412, #200878, #183583, #152167, #17865, #69811, #82887, #20007, #168410, #86091, #116518, #3736, #2677, #182508, #165212, #132748, #199827, #169473, #68749, #34138, #35191, #167350, #70876, #36259, #166274, #148963, #83948, #535, #150039, #203016, #1610, #135917, #201936, #133813, #67669, #37339, #53592, #66602, #51468, #119726, #117592, #136989, #16802, #101266, #85022, #18937, #151111, #185705, #21058, #134871, #87155, #54658, #52523, #184641, #118656, #153226, #4796, #120806, #186783, #138057, #56794, #125087, #208363, #154300, #25353, #105572, #158571, #91453, #171604, #155360, #205151, #23198, #121876, #71947, #9109, #157514, #139124, #38409, #170534, #206232, #5874, #191045, #75185, #42710, #6945, #122963, #108818, #141297, #204070, #10170, #92531, #188922, #26419, #76244, #187847, #207306, #156443, #174842, #88231, #73026, #55722, #189987, #106667, #8027, #57859, #89313, #39473, #40560, #172691, #24269, #142353, #90374, #107752, #104491, #59994, #22119, #74117, #140213, #124021, #41638, #126147, #58929, #173778, #95729, #65301, #93591, #194260, #13372, #128298, #145563, #162846, #45906, #63196, #94658, #192110, #160701, #112024, #79446, #175900, #31779, #29644, #97851, #28570, #14424, #146611, #114160, #210503, #129360, #78375, #195338, #209420, #43774, #178026, #62138, #193193, #196402, #110947, #161781, #176954, #80514, #109887, #46970, #64270, #212629, #12295, #211561, #113086, #130415, #147661, #81578, #144495, #159635, #61065, #11232, #179092, #30714, #48047, #96797 ),
 ( #180153, #163914, #15490, #213678, #27491, #77311, #143424, #127224, #44841, #150861, #52280, #1361, #200632, #134628, #19760, #67423, #101014, #118407, #4553, #34942, #166028, #103161, #132505, #32830, #184393, #49092, #133566, #168162, #98907, #183337, #69562, #119474, #197451, #2423, #36013, #185462, #182261, #116272, #20814, #102092, #198503, #85842, #131450, #82634, #16551, #135672, #18692, #199572, #151919, #50148, #3492, #115212, #201697, #53340, #37082, #148718, #169222, #167105, #288, #181202, #164959, #17613, #86910, #84774, #68500, #152978, #51216, #66359, #33886, #99964, #117340, #83699, #149787, #173522, #92279, #71699, #41385, #139954, #8849, #207047, #190791, #25096, #124825, #108559, #58677, #40306, #174587, #73860, #137811, #205979, #70627, #21870, #170282, #74929, #172436, #155120, #123772, #203830, #107496, #54414, #57614, #189733, #91197, #87976, #157257, #188673, #154050, #136738, #104236, #171354, #141039, #106414, #156193, #90126, #72779, #24024, #42453, #55475, #138878, #158324, #202764, #26163, #120555, #121629, #186534, #38163, #5617, #187598, #39225, #105316, #22948, #89062, #6702, #7769, #204896, #56549, #122710, #27229, #9917, #78115, #94401, #10971, #14160, #143173, #61874, #209166, #195072, #75991, #79186, #96538, #46712, #44579, #128039, #144245, #178841, #179896, #113901, #60804, #125896, #93336, #43516, #193994, #126965, #30453, #45643, #80254, #111760, #142096, #12045, #210237, #146353, #175643, #177766, #59738, #47788, #29381, #95476, #161524, #112825, #13109, #31519, #211307, #160440, #145301, #162585, #62932, #129100, #212365, #64007, #130156, #196147, #97593, #208108, #191855, #109639, #159372, #110693, #77044, #192923, #176692, #28305, #81322, #99703, #200375, #65048, #1107, #101831, #151663, #15234, #34689, #150600, #3235, #34, #148465, #2161, #114946, #68237, #67168, #48832, #147400, #197193, #49887, #167900, #133303, #100759, #183077, #165774, #50954, #134371, #82375, #17357, #36818, #213426, #52023, #185193, #164702, #118149, #18436, #19498, #85574, #69300, #184133, #135413, #201434, #53075, #199308, #166840, #116012, #84512, #180946, #163652, #83441, #33630, #16290, #119209, #66098, #117078, #132240, #35757, #131205, #32568, #98645, #198248, #181998, #149521, #22685, #57351, #58418, #206786, #87715, #4295, #120292, #136480, #154857, #153786, #123514, #138612, #107233, #204636, #102899, #105055, #171091, #173254, #54153, #88797, #152713, #140771, #72516, #6439, #56286, #205715, #122446, #124571, #89872, #38969, #188404, #189479, #40042, #23767, #187341, #172177, #106151, #41121, #155924, #7509, #73591, #190532, #139693, #137550, #74668, #103977, #70366, #24835, #20562, #90934, #157000, #202503, #8587, #168958, #86645, #186265, #37900, #170020, #21607, #5356, #71438, #203568, #55220, #121365, #45381, #42188, #207849, #141844, #46440, #143978, #126697, #95201, #175380, #12838, #25898, #177503, #111497, #160180, #76783, #13905, #43254, #158067, #29116, #174323, #192658, #78912, #9655, #94142, #194804, #30179, #108303, #127780, #161251, #96270, #93071, #26965, #146090, #145034, #109373, #211037, #92009, #59475, #125632, #112559, #209969, #44312, #62663, #159113, #128822, #75731, #178572, #162320, #79986, #191593, #212101, #11781, #10714, #142905, #208905, #60538, #63738, #77854 ),
 ( #110434, #129896, #176436, #28048, #61610, #193735, #199044, #84257, #67970, #18170, #49622, #99449, #98380, #165506, #81060, #195881, #214209, #82114, #130946, #166581, #48577, #197996, #114693, #133043, #47519, #837, #100506, #50691, #164443, #115747, #131987, #182817, #51776, #200123, #180687, #163389, #213171, #147145, #181737, #32312, #34433, #33368, #150342, #17098, #113632, #83176, #149259, #1911, #64800, #66903, #14963, #179637, #116815, #134114, #31257, #97331, #196937, #16030, #148207, #65838, #128480, #47163, #194448, #95916, #45026, #29832, #178217, #63389, #111139, #144681, #161970, #48231, #77496, #94841, #210692, #158758, #14614, #12488, #80711, #11420, #211751, #129543, #96983, #193382, #43956, #177140, #28757, #146801, #112209, #176084, #10353, #110072, #76429, #126337, #64455, #27682, #13560, #79632, #209609, #208544, #113278, #195525, #142538, #93780, #145750, #143615, #212818, #26611, #61252, #160892, #78561, #62321, #179284, #163033, #175024, #30909, #130599, #159817, #46092, #127410, #196588, #92712, #60179, #192297, #79568, #181327, #198624, #212755, #182378, #17730, #95850, #115336, #16676, #83819, #80645, #14548, #133688, #32955, #30841, #99029, #29765, #195464, #129482, #34008, #131571, #114280, #82761, #162969, #405, #13493, #165085, #148834, #66478, #47093, #132617, #147783, #113211, #161906, #63321, #130534, #100083, #213799, #50271, #49216, #31901, #197572, #116389, #146737, #97978, #117463, #145687, #166144, #51338, #96918, #149912, #1479, #67545, #199693, #211685, #179216, #64389, #196525, #48168, #65422, #180277, #164037, #15612, #81700, #183456, #37211, #53461, #184512, #187721, #102215, #20932, #168281, #154174, #35062, #38282, #55598, #71819, #205027, #36132, #5741, #104359, #121753, #105445, #89188, #137929, #23072, #6821, #171481, #153100, #54533, #69688, #120678, #200752, #101133, #103285, #119598, #19881, #39349, #85965, #87028, #152040, #203950, #167221, #170404, #155239, #72900, #3610, #4675, #169347, #139005, #56673, #18807, #135792, #84893, #52401, #2545, #70749, #201816, #150980, #136861, #68620, #202885, #134743, #185581, #186656, #118528, #21993, #88103, #172562, #160568, #92403, #124956, #42582, #11100, #158442, #12176, #109760, #58801, #76117, #209289, #142222, #43646, #207177, #191979, #126019, #77176, #190918, #10043, #175769, #210371, #26289, #157388, #94530, #123895, #24145, #27362, #40434, #90248, #59867, #143298, #91328, #60936, #110817, #188798, #208235, #93463, #176822, #173651, #107620, #78248, #159502, #189863, #127093, #122837, #73986, #7898, #193056, #44710, #108686, #28437, #41506, #144371, #106536, #156314, #140081, #206104, #57737, #25225, #8980, #75054, #141168, #174715, #162719, #66227, #180027, #147532, #81455, #64142, #163783, #32697, #195208, #130286, #149654, #128167, #31648, #96667, #33759, #63068, #177899, #65176, #194129, #111895, #213553, #16424, #30585, #160, #50017, #45778, #131331, #48965, #116141, #112959, #46845, #165902, #197325, #129236, #115083, #62011, #13248, #161653, #132374, #15362, #146482, #181079, #178970, #98779, #29512, #164834, #82504, #148591, #79321, #198376, #97725, #145437, #95605, #211437, #14291, #182130, #99836, #17486, #83572, #196274, #80386, #212501, #47921, #114033, #88930, #67297, #104105, #22817, #2294, #186398, #70496 ),
 ( #119345, #1235, #117211, #3368, #36955, #151794, #169090, #38035, #69437, #86780, #118278, #133436, #184263, #135543, #103035, #199443, #55347, #53214, #121499, #52150, #170155, #21741, #137680, #19635, #84643, #85706, #201568, #187471, #152851, #68371, #51086, #150734, #183208, #166976, #105186, #134503, #4426, #120424, #35889, #34814, #153921, #87850, #100889, #200507, #5491, #101965, #39101, #18567, #168031, #185332, #20689, #136612, #71572, #203701, #202637, #54287, #171222, #107359, #139820, #23893, #188539, #125762, #207977, #41251, #154985, #72650, #108433, #56416, #27098, #191724, #93205, #123642, #24965, #159236, #59604, #40169, #126830, #209032, #173381, #143037, #60667, #89999, #43380, #58543, #10837, #204764, #189605, #106283, #92139, #8716, #124698, #174453, #205850, #122577, #57483, #172304, #74801, #76911, #156050, #9785, #6570, #44445, #138746, #91067, #157127, #140902, #42317, #192787, #109501, #75857, #190656, #28174, #7639, #206913, #26029, #158194, #141965, #175508, #110563, #176565, #73724, #94270, #211171, #14029, #130026, #77987, #148332, #146220, #214332, #145166, #131076, #48702, #16156, #112693, #177641, #178704, #162453, #65964, #31384, #95341, #144110, #29249, #210104, #45512, #198121, #161391, #97460, #213300, #128958, #127911, #32441, #197064, #61744, #12974, #64927, #62796, #132113, #160310, #194937, #80115, #96403, #212238, #114816, #82241, #11914, #15102, #49752, #79050, #179768, #46574, #30318, #63871, #196017, #180814, #193863, #81190, #111628, #115879, #47653, #147268, #113764, #181864, #98509, #163515, #164571, #101700, #169893, #149387, #102774, #33500, #137419, #99573, #51895, #118018, #184007, #135291, #103845, #70238, #168830, #151532, #121241, #970, #35621, #69171, #167770, #201305, #4168, #19367, #119083, #150471, #165637, #2032, #85447, #52945, #17225, #87591, #3100, #153663, #84384, #136353, #202373, #21482, #185063, #116944, #36688, #20434, #5231, #86517, #34560, #83302, #182944, #67035, #199172, #203438, #100630, #152582, #54022, #68101, #133172, #186136, #120161, #50818, #166707, #37771, #134237, #71306, #18298, #200245, #55092, #189351, #40991, #207728, #109251, #187211, #108176, #76664, #172047, #58291, #7381, #106025, #122319, #90808, #59351, #72386, #174202, #154729, #208784, #39916, #25774, #23640, #92948, #91887, #89748, #155797, #139562, #73461, #56156, #6312, #157942, #9534, #205589, #38840, #104923, #140645, #88670, #125507, #75608, #191470, #57226, #123386, #43137, #141719, #138485, #158994, #26844, #107102, #175259, #10589, #188276, #142778, #156872, #60414, #22564, #173125, #204507, #124447, #24706, #8458, #206658, #74546, #190406, #42062, #170964, #100117, #192535, #195757, #1515, #166179, #161128, #178450, #46321, #83856, #84929, #18844, #111375, #27922, #143855, #160056, #30058, #177379, #149945, #162199, #133724, #13786, #126575, #128708, #194677, #199730, #77733, #112437, #176317, #167258, #96148, #79860, #145969, #17767, #211981, #151018, #113508, #62545, #63621, #67579, #129775, #47395, #210919, #179516, #34044, #51376, #117499, #183490, #35099, #2585, #101170, #12715, #44189, #127651, #94017, #110309, #11660, #209847, #61486, #193615, #95079, #45256, #28993, #78789, #144912, #55631, #56704, #119634, #53497, #172598, #71856, #69724, #137963, #68655, #19916 ),
 ( #86001, #121787, #186689, #168321, #134778, #102247, #169382, #72933, #38317, #154207, #88137, #70784, #170440, #39383, #201852, #136897, #156349, #200787, #171512, #90280, #135828, #105479, #203984, #6854, #205062, #188832, #23106, #122871, #106570, #40468, #104393, #5777, #20967, #187754, #152075, #52438, #202926, #153136, #185618, #139037, #37250, #120716, #103320, #89221, #22027, #24177, #155274, #4709, #118564, #184548, #36170, #3645, #54568, #87064, #11133, #110850, #92435, #192014, #143328, #95638, #126051, #42612, #194164, #9011, #123930, #77210, #140112, #57769, #159535, #176857, #190948, #160604, #210406, #74021, #93495, #209322, #62048, #58834, #207210, #111931, #60969, #75087, #127125, #7933, #173683, #107654, #12207, #109796, #158474, #193095, #141199, #44744, #206138, #28470, #94562, #78278, #25259, #144406, #43677, #91359, #189898, #41540, #108721, #128203, #175803, #45811, #27395, #10074, #177932, #29546, #124989, #76150, #157420, #174748, #26321, #142254, #208266, #59899, #16459, #99871, #83607, #67328, #50055, #1271, #199475, #149688, #131362, #32732, #47954, #98813, #179005, #161689, #15396, #31684, #162757, #165934, #80421, #213586, #146520, #132410, #13283, #82539, #33793, #198412, #196310, #65211, #81488, #116177, #117242, #51119, #212538, #63103, #30619, #195243, #197357, #64179, #182162, #49000, #17519, #115118, #79356, #163818, #147565, #133473, #112992, #181114, #211469, #183242, #164865, #148627, #193, #66262, #145474, #34846, #129271, #46880, #130320, #96708, #14331, #114069, #180061, #97760, #185365, #169126, #72685, #38070, #101998, #84680, #184297, #2330, #52185, #204800, #168068, #104140, #5522, #135578, #134533, #39134, #203734, #68406, #19668, #71603, #69471, #138780, #167009, #151829, #86814, #103071, #20720, #121535, #22851, #100921, #21773, #56451, #85747, #186432, #201600, #3402, #35922, #4458, #187505, #200539, #87882, #118311, #122611, #53248, #153955, #119378, #6604, #137714, #36988, #152880, #70528, #136645, #202671, #54319, #55380, #105217, #120460, #18601, #150768, #170187, #171256, #88965, #155020, #188574, #8756, #124736, #126867, #93240, #139855, #11949, #94306, #140938, #28213, #160347, #123677, #159274, #158229, #192825, #90032, #74838, #205885, #191761, #108468, #9820, #59641, #25002, #156091, #91104, #73760, #174490, #176601, #7676, #109541, #40206, #144146, #106316, #58581, #190695, #42356, #142000, #110600, #76948, #175545, #75896, #127948, #57519, #26066, #208015, #92179, #125799, #10873, #43416, #27134, #157165, #172340, #206952, #143073, #189639, #41290, #209066, #60702, #44483, #23928, #107398, #78021, #173420, #210138, #61782, #65996, #162492, #63904, #132146, #32470, #79085, #165670, #33532, #80151, #181896, #99604, #62834, #98542, #97494, #198152, #29282, #14064, #145203, #131107, #47685, #163551, #213330, #178741, #95375, #30354, #13008, #113797, #115911, #161425, #48735, #193901, #83335, #45549, #212269, #130059, #196053, #81222, #49785, #16191, #114848, #15134, #67067, #211209, #179799, #147304, #31418, #64955, #164605, #197094, #180848, #96441, #111665, #146256, #82272, #148367, #177672, #17259, #214366, #149420, #1003, #128996, #194973, #46609, #112730, #2066, #3135, #201339, #104956, #70271, #134271, #116979, #68138, #34596, #84417, #22595, #200279, #136387 ) ),
 .UNSPECIFIED., .T., .F., .F. ) 
 B_SPLINE_SURFACE_WITH_KNOTS ( ( 4, 3, 4 ),
 ( 4, 1, 1, 1, 1, 1, 1, 1, 1, 1, 1, 1, 1, 1, 1, 1, 1, 1, 1, 1, 1, 1, 1, 1, 1, 1, 1, 1, 1, 1, 1, 1, 1, 1, 1, 1, 1, 1, 1, 1, 1, 1, 1, 1, 1, 1, 1, 1, 1, 1, 1, 1, 1, 1, 1, 1, 1, 1, 1, 1, 1, 1, 1, 1, 1, 1, 1, 1, 1, 1, 1, 1, 1, 1, 1, 1, 1, 1, 1, 1, 1, 1, 1, 1, 1, 1, 1, 1, 1, 1, 1, 1, 1, 1, 1, 1, 1, 1, 1, 1, 1, 1, 1, 1, 1, 1, 1, 1, 1, 1, 1, 1, 1, 1, 1, 1, 1, 1, 1, 1, 1, 1, 1, 1, 1, 1, 1, 1, 1, 1, 1, 1, 1, 1, 1, 1, 1, 1, 1, 1, 1, 1, 1, 1, 1, 1, 1, 1, 1, 1, 1, 1, 1, 1, 1, 1, 1, 1, 1, 1, 1, 1, 1, 1, 1, 1, 1, 1, 1, 1, 1, 1, 1, 1, 1, 1, 1, 1, 1, 1, 1, 1, 1, 1, 1, 1, 1, 1, 1, 1, 1, 1, 1, 1, 1, 1, 1, 1, 1, 1, 1, 1, 1, 1, 1, 1, 1, 1, 1, 1, 1, 1, 1, 1, 1, 1, 1, 1, 1, 1, 1, 1, 1, 1, 1, 1, 1, 1, 1, 1, 1, 1, 1, 1, 1, 1, 1, 1, 1, 1, 1, 1, 1, 1, 1, 1, 1, 1, 1, 1, 1, 1, 1, 1, 1, 1, 1, 1, 1, 1, 1, 1, 1, 1, 1, 1, 1, 1, 1, 1, 1, 1, 1, 1, 1, 1, 1, 1, 1, 1, 1, 1, 1, 1, 1, 1, 1, 1, 1, 1, 1, 1, 1, 1, 1, 1, 1, 1, 1, 1, 1, 1, 1, 1, 1, 1, 1, 1, 1, 1, 1, 1, 1, 1, 1, 1, 1, 1, 1, 1, 1, 1, 1, 1, 1, 1, 1, 1, 1, 1, 1, 1, 1, 1, 1, 1, 1, 1, 1, 1, 1, 1, 1, 1, 1, 1, 1, 1, 1, 1, 1, 1, 1, 1, 1, 1, 1, 1, 1, 1, 1, 1, 1, 1, 1, 1, 1, 1, 1, 1, 1, 1, 1, 1, 1, 1, 1, 1, 1, 1, 1, 1, 1, 1, 4 ),
 ( 0.000000000000000000, 0.5000000000000000000, 1.000000000000000000 ),
 ( 0.000000000000000000, 0.002599974731368114196, 0.005208790931971673047, 0.007813145979665977320, 0.01041652777592116073, 0.01302061325022423749, 0.01562498222773845216, 0.01822909327250534645, 0.02083329118620782031, 0.02343750764584028035, 0.02604160881127103033, 0.02864587273906003470, 0.03124992668191499748, 0.03385418289307650513, 0.03645825757725845717, 0.03906249379052053466, 0.04166666320740203266, 0.04427081823557592333, 0.04687506849204003262, 0.04947913642841410276, 0.05208339700068515682, 0.05468745344639398126, 0.05729170333903113588, 0.05989581325979084075, 0.06250002080062810883, 0.06510424464624173235, 0.06770834408375023261, 0.07031260355790951155, 0.07291665769283758869, 0.07552091454841564078, 0.07812498837240108851, 0.08072922377910608793, 0.08333339284475561881, 0.08593754734057650058, 0.08854179710653446722, 0.09114586450482109470, 0.09375012458370637902, 0.09635418052565795921, 0.09895842987840544613, 0.1015625393267825388, 0.1041667463075427041, 0.1067709697059155277, 0.1093750686050062593, 0.1119793276133541904, 0.1145833812402851093, 0.1171876375884709082, 0.1197917109360151500, 0.1223959458003068407, 0.1250001144218755300, 0.1276042683764700425, 0.1302085177025434359, 0.1328125845892443313, 0.1354168441945610146, 0.1380208996559441903, 0.1406251484930516882, 0.1432292574929059925, 0.1458334639374244401, 0.1484376869122458475, 0.1510417852965526830, 0.1536460438630466996, 0.1562500970055218374, 0.1588543528702505148, 0.1614584257649260002, 0.1640626601106844606, 0.1666668283118819260, 0.1692709817489688462, 0.1718752306590244638, 0.1744792970577103974, 0.1770835562133957763, 0.1796876112177483997, 0.1822918595631332073, 0.1848959681380851483, 0.1875001740701665309, 0.1901043966452301559, 0.1927084945383780445, 0.1953127526869259389, 0.1979168053684795814, 0.2005210607736844508, 0.2031251332390507092, 0.2057293670901427229, 0.2083335348946688259, 0.2109376878379560227, 0.2135419363558502259, 0.2161460022900811573, 0.2187502610200618980, 0.2213543155909112325, 0.2239585634684796434, 0.2265626716421396125, 0.2291668770855771753, 0.2317710992846666596, 0.2343751967102698508, 0.2369794544647692847, 0.2395835067089256143, 0.2421877616785296505, 0.2447918337381362330, 0.2473960671184182170, 0.2500002345499632850, 0.2526043870231480248, 0.2552086351727278490, 0.2578127006660536624, 0.2604169589942467167, 0.2630210131551104502, 0.2656252605887587936, 0.2682293683847277177, 0.2708335733633049913, 0.2734377952101950116, 0.2760418921918580404, 0.2786461495761977103, 0.2812502014064713896, 0.2838544559643880194, 0.2864585276417753179, 0.2890627605750938911, 0.2916669276573394809, 0.2942710796841097043, 0.2968753274892133587, 0.2994793925651746958, 0.3020836505154881335, 0.3046877042898750165, 0.3072919513034905736, 0.3098960587453611915, 0.3125002632828523530, 0.3151044848013095923, 0.3177085813626279731, 0.3203128384006882490, 0.3229168898405855304, 0.3255211440107198539, 0.3281252153294201834, 0.3307294478396133885, 0.3333336145962333963, 0.3359377662002681064, 0.3385420136847264727, 0.3411460783668558427, 0.3437503359631899347, 0.3463543893746011126, 0.3489586359920627823, 0.3515627431034201722, 0.3541669472235909888, 0.3567711684373747749, 0.3593752646019360286, 0.3619795213175900916, 0.3645835723906095116, 0.3671878261968588575, 0.3697918971803975663, 0.3723961292912953969, 0.3750002957459567798, 0.3776044469509276524, 0.3802086941385645069, 0.3828127584503868142, 0.3854170157166348365, 0.3880210687885642384, 0.3906253150337437030, 0.3932294218381663375, 0.3958336255647753599, 0.3984378464976386924, 0.4010419422890235119, 0.4036461987061379930, 0.4062502494357712601, 0.4088545029020263510, 0.4114585735739221262, 0.4140628053093475813, 0.4166669714857112461, 0.4192711223152827404, 0.4218753692299160307, 0.4244794331949501842, 0.4270836901549991405, 0.4296877429109347002, 0.4322919888076972583, 0.4348960953287579478, 0.4375002986855570652, 0.4401045193612476147, 0.4427086148030301427, 0.4453128709454660106, 0.4479169213551993378, 0.4505211745053449013, 0.4531252448891109341, 0.4557294762728811288, 0.4583336421946030970, 0.4609377926724337327, 0.4635420393378766879, 0.4661461029796354349, 0.4687503596573671660, 0.4713544121207915438, 0.4739586576929967765, 0.4765627639542633909, 0.4791669669649988861, 0.4817711874072597711, 0.4843752825230089321, 0.4869795384146229367, 0.4895835885279371524, 0.4921878413858530310, 0.4947919115049980165, 0.4973961425609249032, 0.5000003082516567554, 0.5026044584014001115, 0.5052087048414615200, 0.5078127681834534446, 0.5104170246027455171, 0.5130210767971369323, 0.5156253220686399796, 0.5182294280936764475, 0.5208336307820899957, 0.5234378510146604491, 0.5260419458279406157, 0.5286462014925853437, 0.5312502513329574461, 0.5338545039225196520, 0.5364585738005485105, 0.5390628045524396006, 0.5416669700358295314, 0.5442711198811350792, 0.5468753661196208427, 0.5494794291853500878, 0.5520836853700766822, 0.5546877373189100791, 0.5572919823135623618, 0.5598960881259297251, 0.5625002905157588939, 0.5651045105623757614, 0.5677086050967478092, 0.5703128605582734600, 0.5729169101491768945, 0.5755211624942581095, 0.5781252321546730411, 0.5807294626263322934, 0.5833336279260263879, 0.5859377774905402125, 0.5885420235512536236, 0.5911460863642216124, 0.5937503423382545220, 0.5963543940650019026, 0.5989586388066517886, 0.6015627444299086468, 0.6041669465448881171, 0.6067711664292861906, 0.6093752607083083861, 0.6119795159905627724, 0.6145835653554690969, 0.6171878174799397820, 0.6197918869462408775, 0.6223961171614702526, 0.6250002823011129305, 0.6276044316084782304, 0.6302086775152213605, 0.6328127400989277396, 0.6354169958861367595, 0.6380210474142689048, 0.6406252919267632073, 0.6432293973844667168, 0.6458335992483292820, 0.6484378189942425763, 0.6510419130414711875, 0.6536461681683013447, 0.6562502173306804520, 0.6588544692584096252, 0.6614585385540960871, 0.6640627685366956579, 0.6666669335399304508, 0.6692710826137896474, 0.6718753283903641238, 0.6744793907683068745, 0.6770836463925611337, 0.6796876977455479363, 0.6822919420527318035, 0.6848960473684391204, 0.6875002490049163528, 0.6901044686360783276, 0.6927085624750688453, 0.6953128174703216979, 0.6979168664536427036, 0.7005211182084990496, 0.7031251873570698585, 0.7057294171308388098, 0.7083335820213095824, 0.7109377308853042088, 0.7135419765555117699, 0.7161460387511890957, 0.7187502942363581671, 0.7213543454376690756, 0.7239585895633880996, 0.7265626947606567132, 0.7291668961934797411, 0.7317711157336249661, 0.7343752093879328813, 0.7369794642754557978, 0.7395835131031885945, 0.7421877647090413532, 0.7447918337339959338, 0.7473960633227341166, 0.7500002281240860658, 0.7526043768018576552, 0.7552086223895014827, 0.7578126844264116979, 0.7604169397963658206, 0.7630209908694718379, 0.7656252348375721661, 0.7682293399399604539, 0.7708335411928610714, 0.7734377606657260040, 0.7760418541589074737, 0.7786461089625497101, 0.7812501576581653007, 0.7838544091388848223, 0.7864584780637244865, 0.7890627074912324179, 0.7916668722271122949, 0.7942710207423038238, 0.7968752662711893198, 0.7994793281728324041, 0.8020835834514440377, 0.8046876344198176101, 0.8072918782541467220, 0.8098959832852158369, 0.8125001843819276148, 0.8151044038112509327, 0.8177084971668638902, 0.8203127519104773668, 0.8229168004974481976, 0.8255210518769072747, 0.8281251207251358881, 0.8307293500152160837, 0.8333335147092740813, 0.8359376630855301915, 0.8385419085794658667, 0.8411459703693440204, 0.8437502255804886220, 0.8463542764676049712, 0.8489585201920134550, 0.8515626251753276588, 0.8541668261395859441, 0.8567710455491102106, 0.8593751387907155870, 0.8619793934981552219, 0.8645834419999574028, 0.8671876933020320477, 0.8697917620971562513, 0.8723959912736143352, 0.8750001559495040881, 0.8776043042104727521, 0.8802085496932706699, 0.8828126113948897569, 0.8854168665624462253, 0.8880209173917842369, 0.8906251610301256783, 0.8932292659892527853, 0.8958334668447968108, 0.8984376862582688084, 0.9010417794094305322, 0.9036460341045560174, 0.9062500825446693220, 0.9088543337932389887, 0.9114584025587700866, 0.9140626316454156797, 0.9166667963267953745, 0.9192709444961273402, 0.9218751899916067805, 0.9244792516284782158, 0.9270835067763207871, 0.9296875575713596795, 0.9322918011475309630, 0.9348959061060417852, 0.9375001068764983181, 0.9401043263176916964, 0.9427084194022110619, 0.9453126741091559815, 0.9479167225106870376, 0.9505209737258253355, 0.9531250424882484751, 0.9557292715345466760, 0.9583334362123939743, 0.9609375841976093291, 0.9635418299546441023, 0.9661458919105455623, 0.9687501459642621215, 0.9713541960184646218, 0.9739584433044384815, 0.9765625494917742344, 0.9791667425299969141, 0.9817709508269629737, 0.9843750450459556323, 0.9869794226472197174, 0.9895834977571079660, 0.9921868632736227100, 0.9947912224625704569, 0.9974000159472320437, 1.000000000000000000 ),
 .UNSPECIFIED. ) 
 GEOMETRIC_REPRESENTATION_ITEM ( )  RATIONAL_B_SPLINE_SURFACE ( (
 ( 1.000000000000000000, 1.000000000000000000, 1.000000000000000000, 1.000000000000000222, 0.9999999999999997780, 1.000000000000000444, 0.9999999999999997780, 1.000000000000000222, 0.9999999999999996669, 1.000000000000000000, 1.000000000000000000, 1.000000000000000222, 1.000000000000000000, 1.000000000000000000, 0.9999999999999997780, 1.000000000000000000, 1.000000000000000000, 1.000000000000000000, 0.9999999999999997780, 1.000000000000000444, 0.9999999999999997780, 1.000000000000000222, 1.000000000000000000, 0.9999999999999997780, 1.000000000000000000, 1.000000000000000222, 0.9999999999999997780, 1.000000000000000222, 0.9999999999999997780, 1.000000000000000222, 1.000000000000000000, 0.9999999999999997780, 1.000000000000000444, 0.9999999999999997780, 1.000000000000000222, 0.9999999999999997780, 1.000000000000000444, 1.000000000000000000, 1.000000000000000000, 1.000000000000000000, 1.000000000000000000, 1.000000000000000000, 1.000000000000000000, 0.9999999999999997780, 1.000000000000000222, 0.9999999999999996669, 1.000000000000000444, 0.9999999999999994449, 1.000000000000000222, 1.000000000000000000, 1.000000000000000000, 1.000000000000000000, 1.000000000000000000, 1.000000000000000000, 0.9999999999999996669, 1.000000000000000444, 0.9999999999999997780, 1.000000000000000222, 0.9999999999999996669, 1.000000000000000000, 1.000000000000000000, 1.000000000000000222, 0.9999999999999997780, 1.000000000000000000, 1.000000000000000222, 0.9999999999999997780, 1.000000000000000000, 0.9999999999999997780, 1.000000000000000222, 0.9999999999999997780, 1.000000000000000444, 0.9999999999999994449, 1.000000000000000444, 0.9999999999999997780, 0.9999999999999997780, 1.000000000000000444, 0.9999999999999996669, 1.000000000000000000, 1.000000000000000000, 1.000000000000000000, 1.000000000000000000, 1.000000000000000222, 1.000000000000000000, 1.000000000000000000, 0.9999999999999996669, 1.000000000000000222, 1.000000000000000000, 0.9999999999999997780, 0.9999999999999997780, 0.9999999999999997780, 1.000000000000000000, 1.000000000000000222, 0.9999999999999997780, 1.000000000000000222, 0.9999999999999996669, 1.000000000000000444, 0.9999999999999997780, 1.000000000000000222, 1.000000000000000222, 0.9999999999999997780, 1.000000000000000222, 1.000000000000000000, 0.9999999999999997780, 1.000000000000000444, 1.000000000000000000, 1.000000000000000000, 1.000000000000000222, 1.000000000000000000, 1.000000000000000000, 1.000000000000000222, 0.9999999999999993339, 1.000000000000000444, 1.000000000000000222, 0.9999999999999997780, 1.000000000000000000, 1.000000000000000222, 1.000000000000000444, 1.000000000000000000, 1.000000000000000222, 0.9999999999999997780, 1.000000000000000222, 0.9999999999999997780, 1.000000000000000222, 1.000000000000000000, 0.9999999999999997780, 0.9999999999999996669, 1.000000000000000444, 0.9999999999999997780, 1.000000000000000444, 0.9999999999999997780, 1.000000000000000222, 1.000000000000000222, 1.000000000000000000, 0.9999999999999997780, 1.000000000000000222, 0.9999999999999997780, 1.000000000000000000, 1.000000000000000000, 1.000000000000000000, 0.9999999999999997780, 1.000000000000000222, 1.000000000000000000, 1.000000000000000000, 1.000000000000000000, 1.000000000000000222, 1.000000000000000222, 0.9999999999999994449, 1.000000000000000222, 1.000000000000000000, 0.9999999999999994449, 1.000000000000000444, 0.9999999999999997780, 1.000000000000000222, 0.9999999999999996669, 1.000000000000000444, 1.000000000000000000, 0.9999999999999996669, 1.000000000000000444, 0.9999999999999997780, 1.000000000000000000, 1.000000000000000444, 1.000000000000000000, 1.000000000000000222, 0.9999999999999996669, 1.000000000000000000, 0.9999999999999997780, 0.9999999999999997780, 1.000000000000000222, 1.000000000000000000, 1.000000000000000444, 0.9999999999999996669, 1.000000000000000222, 0.9999999999999997780, 0.9999999999999997780, 1.000000000000000444, 0.9999999999999997780, 1.000000000000000444, 0.9999999999999996669, 1.000000000000000222, 0.9999999999999996669, 1.000000000000000222, 0.9999999999999997780, 1.000000000000000444, 1.000000000000000222, 0.9999999999999996669, 1.000000000000000444, 0.9999999999999996669, 1.000000000000000000, 0.9999999999999997780, 1.000000000000000000, 1.000000000000000000, 1.000000000000000222, 0.9999999999999994449, 1.000000000000000444, 0.9999999999999993339, 1.000000000000000666, 0.9999999999999994449, 1.000000000000000222, 1.000000000000000222, 1.000000000000000000, 1.000000000000000000, 0.9999999999999997780, 1.000000000000000222, 0.9999999999999996669, 1.000000000000000222, 0.9999999999999996669, 1.000000000000000222, 1.000000000000000000, 1.000000000000000222, 0.9999999999999997780, 1.000000000000000222, 1.000000000000000222, 1.000000000000000000, 0.9999999999999997780, 1.000000000000000222, 1.000000000000000222, 1.000000000000000000, 1.000000000000000000, 1.000000000000000222, 0.9999999999999997780, 1.000000000000000000, 1.000000000000000222, 0.9999999999999996669, 0.9999999999999997780, 1.000000000000000222, 0.9999999999999997780, 1.000000000000000000, 0.9999999999999997780, 0.9999999999999997780, 1.000000000000000222, 1.000000000000000000, 1.000000000000000000, 1.000000000000000222, 0.9999999999999996669, 1.000000000000000444, 1.000000000000000000, 1.000000000000000222, 0.9999999999999997780, 1.000000000000000222, 0.9999999999999997780, 1.000000000000000444, 0.9999999999999997780, 1.000000000000000222, 0.9999999999999997780, 1.000000000000000222, 0.9999999999999997780, 1.000000000000000222, 1.000000000000000000, 1.000000000000000222, 1.000000000000000000, 1.000000000000000000, 1.000000000000000222, 1.000000000000000000, 1.000000000000000000, 0.9999999999999997780, 1.000000000000000000, 1.000000000000000444, 0.9999999999999996669, 1.000000000000000222, 0.9999999999999997780, 1.000000000000000000, 0.9999999999999997780, 1.000000000000000222, 1.000000000000000222, 1.000000000000000000, 1.000000000000000000, 0.9999999999999996669, 1.000000000000000444, 0.9999999999999997780, 1.000000000000000000, 1.000000000000000222, 0.9999999999999996669, 1.000000000000000444, 1.000000000000000000, 0.9999999999999997780, 1.000000000000000222, 0.9999999999999997780, 1.000000000000000000, 1.000000000000000000, 1.000000000000000000, 1.000000000000000000, 1.000000000000000000, 1.000000000000000222, 1.000000000000000444, 0.9999999999999997780, 1.000000000000000222, 1.000000000000000000, 1.000000000000000444, 0.9999999999999997780, 1.000000000000000222, 0.9999999999999997780, 1.000000000000000222, 0.9999999999999997780, 1.000000000000000222, 1.000000000000000000, 1.000000000000000222, 1.000000000000000222, 1.000000000000000222, 0.9999999999999997780, 1.000000000000000222, 0.9999999999999997780, 1.000000000000000222, 0.9999999999999997780, 1.000000000000000444, 0.9999999999999996669, 1.000000000000000444, 1.000000000000000000, 1.000000000000000000, 0.9999999999999997780, 1.000000000000000222, 1.000000000000000000, 0.9999999999999997780, 1.000000000000000000, 0.9999999999999997780, 1.000000000000000222, 1.000000000000000000, 1.000000000000000000, 1.000000000000000222, 0.9999999999999997780, 1.000000000000000444, 0.9999999999999996669, 1.000000000000000222, 1.000000000000000222, 0.9999999999999997780, 1.000000000000000000, 0.9999999999999997780, 1.000000000000000000, 0.9999999999999996669, 1.000000000000000444, 0.9999999999999997780, 1.000000000000000222, 1.000000000000000000, 1.000000000000000000, 1.000000000000000000, 0.9999999999999997780, 0.9999999999999997780, 1.000000000000000000, 0.9999999999999997780, 1.000000000000000444, 0.9999999999999996669, 1.000000000000000222, 1.000000000000000000, 1.000000000000000444, 1.000000000000000222, 1.000000000000000000, 0.9999999999999997780, 1.000000000000000222, 1.000000000000000444, 0.9999999999999997780, 1.000000000000000222, 0.9999999999999997780, 1.000000000000000000, 1.000000000000000000, 1.000000000000000222, 0.9999999999999997780, 1.000000000000000222, 1.000000000000000000, 1.000000000000000222, 0.9999999999999997780, 1.000000000000000000, 1.000000000000000222, 1.000000000000000000, 1.000000000000000222, 1.000000000000000000, 1.000000000000000000, 0.9999999999999997780, 1.000000000000000444, 0.9999999999999997780, 1.000000000000000000, 1.000000000000000000, 1.000000000000000444, 0.9999999999999996669, 1.000000000000000222, 1.000000000000000000, 0.9999999999999996669, 1.000000000000000444, 0.9999999999999996669, 1.000000000000000444, 0.9999999999999997780, 1.000000000000000222, 0.9999999999999997780, 1.000000000000000222, 1.000000000000000222, 1.000000000000000222, 1.000000000000000000, 1.000000000000000000, 1.000000000000000000),
 ( 0.3333333333333333703, 0.3333333333333333703, 0.3333333333333334259, 0.3333333333333334259, 0.3333333333333333703, 0.3333333333333334259, 0.3333333333333333148, 0.3333333333333333703, 0.3333333333333333148, 0.3333333333333333703, 0.3333333333333333703, 0.3333333333333334259, 0.3333333333333333703, 0.3333333333333333703, 0.3333333333333333703, 0.3333333333333333703, 0.3333333333333333703, 0.3333333333333333148, 0.3333333333333333703, 0.3333333333333334814, 0.3333333333333333148, 0.3333333333333334259, 0.3333333333333333148, 0.3333333333333334259, 0.3333333333333332593, 0.3333333333333335369, 0.3333333333333333703, 0.3333333333333333703, 0.3333333333333333703, 0.3333333333333333703, 0.3333333333333333703, 0.3333333333333333703, 0.3333333333333334259, 0.3333333333333333703, 0.3333333333333333703, 0.3333333333333333703, 0.3333333333333334814, 0.3333333333333333703, 0.3333333333333333703, 0.3333333333333333703, 0.3333333333333334259, 0.3333333333333332593, 0.3333333333333334814, 0.3333333333333332593, 0.3333333333333334259, 0.3333333333333332038, 0.3333333333333335369, 0.3333333333333332593, 0.3333333333333334814, 0.3333333333333333703, 0.3333333333333333148, 0.3333333333333333703, 0.3333333333333333703, 0.3333333333333333148, 0.3333333333333333148, 0.3333333333333334814, 0.3333333333333332593, 0.3333333333333334259, 0.3333333333333332593, 0.3333333333333333703, 0.3333333333333333703, 0.3333333333333334259, 0.3333333333333333148, 0.3333333333333333148, 0.3333333333333334259, 0.3333333333333333703, 0.3333333333333333703, 0.3333333333333333703, 0.3333333333333334814, 0.3333333333333332038, 0.3333333333333335924, 0.3333333333333332593, 0.3333333333333335369, 0.3333333333333333148, 0.3333333333333332593, 0.3333333333333335924, 0.3333333333333332038, 0.3333333333333333703, 0.3333333333333333703, 0.3333333333333334259, 0.3333333333333333148, 0.3333333333333334259, 0.3333333333333333703, 0.3333333333333334259, 0.3333333333333332038, 0.3333333333333333703, 0.3333333333333333703, 0.3333333333333333703, 0.3333333333333332593, 0.3333333333333333703, 0.3333333333333333148, 0.3333333333333334259, 0.3333333333333333148, 0.3333333333333334259, 0.3333333333333333148, 0.3333333333333334814, 0.3333333333333333703, 0.3333333333333334259, 0.3333333333333333703, 0.3333333333333333148, 0.3333333333333333703, 0.3333333333333334259, 0.3333333333333333148, 0.3333333333333334814, 0.3333333333333334259, 0.3333333333333333703, 0.3333333333333334259, 0.3333333333333333703, 0.3333333333333334259, 0.3333333333333334814, 0.3333333333333332038, 0.3333333333333334259, 0.3333333333333334259, 0.3333333333333333703, 0.3333333333333333148, 0.3333333333333334259, 0.3333333333333334259, 0.3333333333333334259, 0.3333333333333333703, 0.3333333333333333148, 0.3333333333333334259, 0.3333333333333333703, 0.3333333333333334259, 0.3333333333333333703, 0.3333333333333333148, 0.3333333333333332593, 0.3333333333333334259, 0.3333333333333333148, 0.3333333333333335369, 0.3333333333333332593, 0.3333333333333334814, 0.3333333333333334259, 0.3333333333333334259, 0.3333333333333333148, 0.3333333333333334259, 0.3333333333333333148, 0.3333333333333333148, 0.3333333333333333703, 0.3333333333333333703, 0.3333333333333332593, 0.3333333333333334259, 0.3333333333333333148, 0.3333333333333333703, 0.3333333333333334259, 0.3333333333333333148, 0.3333333333333334814, 0.3333333333333332593, 0.3333333333333333703, 0.3333333333333334259, 0.3333333333333332038, 0.3333333333333335369, 0.3333333333333333703, 0.3333333333333333703, 0.3333333333333333148, 0.3333333333333334259, 0.3333333333333333703, 0.3333333333333332593, 0.3333333333333335369, 0.3333333333333332593, 0.3333333333333333703, 0.3333333333333334814, 0.3333333333333333703, 0.3333333333333334259, 0.3333333333333332593, 0.3333333333333334259, 0.3333333333333332593, 0.3333333333333333703, 0.3333333333333334259, 0.3333333333333333703, 0.3333333333333334814, 0.3333333333333332593, 0.3333333333333333703, 0.3333333333333333703, 0.3333333333333333703, 0.3333333333333334259, 0.3333333333333333148, 0.3333333333333334259, 0.3333333333333332593, 0.3333333333333333703, 0.3333333333333332593, 0.3333333333333334814, 0.3333333333333333703, 0.3333333333333334259, 0.3333333333333334259, 0.3333333333333332593, 0.3333333333333334814, 0.3333333333333333148, 0.3333333333333333148, 0.3333333333333333148, 0.3333333333333333703, 0.3333333333333333703, 0.3333333333333334259, 0.3333333333333332593, 0.3333333333333335369, 0.3333333333333332038, 0.3333333333333335924, 0.3333333333333332593, 0.3333333333333334814, 0.3333333333333333703, 0.3333333333333333703, 0.3333333333333333703, 0.3333333333333333148, 0.3333333333333334259, 0.3333333333333333703, 0.3333333333333333703, 0.3333333333333333148, 0.3333333333333333703, 0.3333333333333333148, 0.3333333333333333703, 0.3333333333333332593, 0.3333333333333334259, 0.3333333333333333703, 0.3333333333333334259, 0.3333333333333333148, 0.3333333333333334259, 0.3333333333333333703, 0.3333333333333334259, 0.3333333333333334259, 0.3333333333333334259, 0.3333333333333332593, 0.3333333333333334259, 0.3333333333333333703, 0.3333333333333333148, 0.3333333333333333148, 0.3333333333333335369, 0.3333333333333332593, 0.3333333333333333148, 0.3333333333333333703, 0.3333333333333333148, 0.3333333333333334814, 0.3333333333333333703, 0.3333333333333334814, 0.3333333333333333703, 0.3333333333333332593, 0.3333333333333334259, 0.3333333333333333703, 0.3333333333333335369, 0.3333333333333333148, 0.3333333333333334259, 0.3333333333333333148, 0.3333333333333335924, 0.3333333333333332593, 0.3333333333333334259, 0.3333333333333334259, 0.3333333333333333703, 0.3333333333333333703, 0.3333333333333334259, 0.3333333333333334259, 0.3333333333333334259, 0.3333333333333333703, 0.3333333333333333703, 0.3333333333333334259, 0.3333333333333333148, 0.3333333333333333703, 0.3333333333333332038, 0.3333333333333334259, 0.3333333333333334814, 0.3333333333333332593, 0.3333333333333333703, 0.3333333333333333148, 0.3333333333333334814, 0.3333333333333332593, 0.3333333333333334259, 0.3333333333333333703, 0.3333333333333333703, 0.3333333333333333703, 0.3333333333333333148, 0.3333333333333334259, 0.3333333333333333703, 0.3333333333333333148, 0.3333333333333334259, 0.3333333333333332038, 0.3333333333333334259, 0.3333333333333333703, 0.3333333333333333703, 0.3333333333333333703, 0.3333333333333334259, 0.3333333333333333148, 0.3333333333333333703, 0.3333333333333333703, 0.3333333333333333703, 0.3333333333333333703, 0.3333333333333334259, 0.3333333333333334814, 0.3333333333333332593, 0.3333333333333333703, 0.3333333333333334259, 0.3333333333333334814, 0.3333333333333333148, 0.3333333333333333703, 0.3333333333333333703, 0.3333333333333334259, 0.3333333333333333148, 0.3333333333333334814, 0.3333333333333333148, 0.3333333333333334814, 0.3333333333333333703, 0.3333333333333334814, 0.3333333333333333148, 0.3333333333333334259, 0.3333333333333332593, 0.3333333333333335369, 0.3333333333333333148, 0.3333333333333334814, 0.3333333333333333148, 0.3333333333333334259, 0.3333333333333333703, 0.3333333333333333148, 0.3333333333333333703, 0.3333333333333333703, 0.3333333333333334259, 0.3333333333333333148, 0.3333333333333334259, 0.3333333333333333148, 0.3333333333333334814, 0.3333333333333333148, 0.3333333333333334259, 0.3333333333333334259, 0.3333333333333333703, 0.3333333333333334259, 0.3333333333333333703, 0.3333333333333333703, 0.3333333333333335369, 0.3333333333333332593, 0.3333333333333334259, 0.3333333333333333703, 0.3333333333333333703, 0.3333333333333333148, 0.3333333333333335369, 0.3333333333333333148, 0.3333333333333334259, 0.3333333333333333703, 0.3333333333333333703, 0.3333333333333334259, 0.3333333333333333148, 0.3333333333333333703, 0.3333333333333333148, 0.3333333333333333148, 0.3333333333333334814, 0.3333333333333332593, 0.3333333333333334259, 0.3333333333333333703, 0.3333333333333334814, 0.3333333333333334259, 0.3333333333333333148, 0.3333333333333333703, 0.3333333333333333703, 0.3333333333333335369, 0.3333333333333333148, 0.3333333333333334259, 0.3333333333333333703, 0.3333333333333333148, 0.3333333333333334259, 0.3333333333333334259, 0.3333333333333333703, 0.3333333333333333703, 0.3333333333333334259, 0.3333333333333334259, 0.3333333333333333703, 0.3333333333333333148, 0.3333333333333334259, 0.3333333333333333703, 0.3333333333333334814, 0.3333333333333333703, 0.3333333333333333703, 0.3333333333333333703, 0.3333333333333334259, 0.3333333333333333148, 0.3333333333333333703, 0.3333333333333334259, 0.3333333333333334259, 0.3333333333333333148, 0.3333333333333333703, 0.3333333333333333148, 0.3333333333333333703, 0.3333333333333335369, 0.3333333333333333148, 0.3333333333333334259, 0.3333333333333333703, 0.3333333333333334259, 0.3333333333333333148, 0.3333333333333333148, 0.3333333333333335369, 0.3333333333333333703, 0.3333333333333333148, 0.3333333333333333703, 0.3333333333333333703),
 ( 0.3333333333333333703, 0.3333333333333333703, 0.3333333333333334259, 0.3333333333333334259, 0.3333333333333333703, 0.3333333333333334259, 0.3333333333333333148, 0.3333333333333333703, 0.3333333333333333148, 0.3333333333333333703, 0.3333333333333333703, 0.3333333333333334259, 0.3333333333333333703, 0.3333333333333333703, 0.3333333333333333703, 0.3333333333333333703, 0.3333333333333333703, 0.3333333333333333148, 0.3333333333333333703, 0.3333333333333334814, 0.3333333333333333148, 0.3333333333333334259, 0.3333333333333333148, 0.3333333333333334259, 0.3333333333333332593, 0.3333333333333335369, 0.3333333333333333703, 0.3333333333333333703, 0.3333333333333333703, 0.3333333333333333703, 0.3333333333333333703, 0.3333333333333333703, 0.3333333333333334259, 0.3333333333333333703, 0.3333333333333333703, 0.3333333333333333703, 0.3333333333333334814, 0.3333333333333333703, 0.3333333333333333703, 0.3333333333333333703, 0.3333333333333334259, 0.3333333333333332593, 0.3333333333333334814, 0.3333333333333332593, 0.3333333333333334259, 0.3333333333333332038, 0.3333333333333335369, 0.3333333333333332593, 0.3333333333333334814, 0.3333333333333333703, 0.3333333333333333148, 0.3333333333333333703, 0.3333333333333333703, 0.3333333333333333148, 0.3333333333333333148, 0.3333333333333334814, 0.3333333333333332593, 0.3333333333333334259, 0.3333333333333332593, 0.3333333333333333703, 0.3333333333333333703, 0.3333333333333334259, 0.3333333333333333148, 0.3333333333333333148, 0.3333333333333334259, 0.3333333333333333703, 0.3333333333333333703, 0.3333333333333333703, 0.3333333333333334814, 0.3333333333333332038, 0.3333333333333335924, 0.3333333333333332593, 0.3333333333333335369, 0.3333333333333333148, 0.3333333333333332593, 0.3333333333333335924, 0.3333333333333332038, 0.3333333333333333703, 0.3333333333333333703, 0.3333333333333334259, 0.3333333333333333148, 0.3333333333333334259, 0.3333333333333333703, 0.3333333333333334259, 0.3333333333333332038, 0.3333333333333333703, 0.3333333333333333703, 0.3333333333333333703, 0.3333333333333332593, 0.3333333333333333703, 0.3333333333333333148, 0.3333333333333334259, 0.3333333333333333148, 0.3333333333333334259, 0.3333333333333333148, 0.3333333333333334814, 0.3333333333333333703, 0.3333333333333334259, 0.3333333333333333703, 0.3333333333333333148, 0.3333333333333333703, 0.3333333333333334259, 0.3333333333333333148, 0.3333333333333334814, 0.3333333333333334259, 0.3333333333333333703, 0.3333333333333334259, 0.3333333333333333703, 0.3333333333333334259, 0.3333333333333334814, 0.3333333333333332038, 0.3333333333333334259, 0.3333333333333334259, 0.3333333333333333703, 0.3333333333333333148, 0.3333333333333334259, 0.3333333333333334259, 0.3333333333333334259, 0.3333333333333333703, 0.3333333333333333148, 0.3333333333333334259, 0.3333333333333333703, 0.3333333333333334259, 0.3333333333333333703, 0.3333333333333333148, 0.3333333333333332593, 0.3333333333333334259, 0.3333333333333333148, 0.3333333333333335369, 0.3333333333333332593, 0.3333333333333334814, 0.3333333333333334259, 0.3333333333333334259, 0.3333333333333333148, 0.3333333333333334259, 0.3333333333333333148, 0.3333333333333333148, 0.3333333333333333703, 0.3333333333333333703, 0.3333333333333332593, 0.3333333333333334259, 0.3333333333333333148, 0.3333333333333333703, 0.3333333333333334259, 0.3333333333333333148, 0.3333333333333334814, 0.3333333333333332593, 0.3333333333333333703, 0.3333333333333334259, 0.3333333333333332038, 0.3333333333333335369, 0.3333333333333333703, 0.3333333333333333703, 0.3333333333333333148, 0.3333333333333334259, 0.3333333333333333703, 0.3333333333333332593, 0.3333333333333335369, 0.3333333333333332593, 0.3333333333333333703, 0.3333333333333334814, 0.3333333333333333703, 0.3333333333333334259, 0.3333333333333332593, 0.3333333333333334259, 0.3333333333333332593, 0.3333333333333333703, 0.3333333333333334259, 0.3333333333333333703, 0.3333333333333334814, 0.3333333333333332593, 0.3333333333333333703, 0.3333333333333333703, 0.3333333333333333703, 0.3333333333333334259, 0.3333333333333333148, 0.3333333333333334259, 0.3333333333333332593, 0.3333333333333333703, 0.3333333333333332593, 0.3333333333333334814, 0.3333333333333333703, 0.3333333333333334259, 0.3333333333333334259, 0.3333333333333332593, 0.3333333333333334814, 0.3333333333333333148, 0.3333333333333333148, 0.3333333333333333148, 0.3333333333333333703, 0.3333333333333333703, 0.3333333333333334259, 0.3333333333333332593, 0.3333333333333335369, 0.3333333333333332038, 0.3333333333333335924, 0.3333333333333332593, 0.3333333333333334814, 0.3333333333333333703, 0.3333333333333333703, 0.3333333333333333703, 0.3333333333333333148, 0.3333333333333334259, 0.3333333333333333703, 0.3333333333333333703, 0.3333333333333333148, 0.3333333333333333703, 0.3333333333333333148, 0.3333333333333333703, 0.3333333333333332593, 0.3333333333333334259, 0.3333333333333333703, 0.3333333333333334259, 0.3333333333333333148, 0.3333333333333334259, 0.3333333333333333703, 0.3333333333333334259, 0.3333333333333334259, 0.3333333333333334259, 0.3333333333333332593, 0.3333333333333334259, 0.3333333333333333703, 0.3333333333333333148, 0.3333333333333333148, 0.3333333333333335369, 0.3333333333333332593, 0.3333333333333333148, 0.3333333333333333703, 0.3333333333333333148, 0.3333333333333334814, 0.3333333333333333703, 0.3333333333333334814, 0.3333333333333333703, 0.3333333333333332593, 0.3333333333333334259, 0.3333333333333333703, 0.3333333333333335369, 0.3333333333333333148, 0.3333333333333334259, 0.3333333333333333148, 0.3333333333333335924, 0.3333333333333332593, 0.3333333333333334259, 0.3333333333333334259, 0.3333333333333333703, 0.3333333333333333703, 0.3333333333333334259, 0.3333333333333334259, 0.3333333333333334259, 0.3333333333333333703, 0.3333333333333333703, 0.3333333333333334259, 0.3333333333333333148, 0.3333333333333333703, 0.3333333333333332038, 0.3333333333333334259, 0.3333333333333334814, 0.3333333333333332593, 0.3333333333333333703, 0.3333333333333333148, 0.3333333333333334814, 0.3333333333333332593, 0.3333333333333334259, 0.3333333333333333703, 0.3333333333333333703, 0.3333333333333333703, 0.3333333333333333148, 0.3333333333333334259, 0.3333333333333333703, 0.3333333333333333148, 0.3333333333333334259, 0.3333333333333332038, 0.3333333333333334259, 0.3333333333333333703, 0.3333333333333333703, 0.3333333333333333703, 0.3333333333333334259, 0.3333333333333333148, 0.3333333333333333703, 0.3333333333333333703, 0.3333333333333333703, 0.3333333333333333703, 0.3333333333333334259, 0.3333333333333334814, 0.3333333333333332593, 0.3333333333333333703, 0.3333333333333334259, 0.3333333333333334814, 0.3333333333333333148, 0.3333333333333333703, 0.3333333333333333703, 0.3333333333333334259, 0.3333333333333333148, 0.3333333333333334814, 0.3333333333333333148, 0.3333333333333334814, 0.3333333333333333703, 0.3333333333333334814, 0.3333333333333333148, 0.3333333333333334259, 0.3333333333333332593, 0.3333333333333335369, 0.3333333333333333148, 0.3333333333333334814, 0.3333333333333333148, 0.3333333333333334259, 0.3333333333333333703, 0.3333333333333333148, 0.3333333333333333703, 0.3333333333333333703, 0.3333333333333334259, 0.3333333333333333148, 0.3333333333333334259, 0.3333333333333333148, 0.3333333333333334814, 0.3333333333333333148, 0.3333333333333334259, 0.3333333333333334259, 0.3333333333333333703, 0.3333333333333334259, 0.3333333333333333703, 0.3333333333333333703, 0.3333333333333335369, 0.3333333333333332593, 0.3333333333333334259, 0.3333333333333333703, 0.3333333333333333703, 0.3333333333333333148, 0.3333333333333335369, 0.3333333333333333148, 0.3333333333333334259, 0.3333333333333333703, 0.3333333333333333703, 0.3333333333333334259, 0.3333333333333333148, 0.3333333333333333703, 0.3333333333333333148, 0.3333333333333333148, 0.3333333333333334814, 0.3333333333333332593, 0.3333333333333334259, 0.3333333333333333703, 0.3333333333333334814, 0.3333333333333334259, 0.3333333333333333148, 0.3333333333333333703, 0.3333333333333333703, 0.3333333333333335369, 0.3333333333333333148, 0.3333333333333334259, 0.3333333333333333703, 0.3333333333333333148, 0.3333333333333334259, 0.3333333333333334259, 0.3333333333333333703, 0.3333333333333333703, 0.3333333333333334259, 0.3333333333333334259, 0.3333333333333333703, 0.3333333333333333148, 0.3333333333333334259, 0.3333333333333333703, 0.3333333333333334814, 0.3333333333333333703, 0.3333333333333333703, 0.3333333333333333703, 0.3333333333333334259, 0.3333333333333333148, 0.3333333333333333703, 0.3333333333333334259, 0.3333333333333334259, 0.3333333333333333148, 0.3333333333333333703, 0.3333333333333333148, 0.3333333333333333703, 0.3333333333333335369, 0.3333333333333333148, 0.3333333333333334259, 0.3333333333333333703, 0.3333333333333334259, 0.3333333333333333148, 0.3333333333333333148, 0.3333333333333335369, 0.3333333333333333703, 0.3333333333333333148, 0.3333333333333333703, 0.3333333333333333703),
 ( 1.000000000000000000, 1.000000000000000000, 1.000000000000000000, 1.000000000000000222, 0.9999999999999997780, 1.000000000000000444, 0.9999999999999997780, 1.000000000000000222, 0.9999999999999996669, 1.000000000000000000, 1.000000000000000000, 1.000000000000000222, 1.000000000000000000, 1.000000000000000000, 0.9999999999999997780, 1.000000000000000000, 1.000000000000000000, 1.000000000000000000, 0.9999999999999997780, 1.000000000000000444, 0.9999999999999997780, 1.000000000000000222, 1.000000000000000000, 0.9999999999999997780, 1.000000000000000000, 1.000000000000000222, 0.9999999999999997780, 1.000000000000000222, 0.9999999999999997780, 1.000000000000000222, 1.000000000000000000, 0.9999999999999997780, 1.000000000000000444, 0.9999999999999997780, 1.000000000000000222, 0.9999999999999997780, 1.000000000000000444, 1.000000000000000000, 1.000000000000000000, 1.000000000000000000, 1.000000000000000000, 1.000000000000000000, 1.000000000000000000, 0.9999999999999997780, 1.000000000000000222, 0.9999999999999996669, 1.000000000000000444, 0.9999999999999994449, 1.000000000000000222, 1.000000000000000000, 1.000000000000000000, 1.000000000000000000, 1.000000000000000000, 1.000000000000000000, 0.9999999999999996669, 1.000000000000000444, 0.9999999999999997780, 1.000000000000000222, 0.9999999999999996669, 1.000000000000000000, 1.000000000000000000, 1.000000000000000222, 0.9999999999999997780, 1.000000000000000000, 1.000000000000000222, 0.9999999999999997780, 1.000000000000000000, 0.9999999999999997780, 1.000000000000000222, 0.9999999999999997780, 1.000000000000000444, 0.9999999999999994449, 1.000000000000000444, 0.9999999999999997780, 0.9999999999999997780, 1.000000000000000444, 0.9999999999999996669, 1.000000000000000000, 1.000000000000000000, 1.000000000000000000, 1.000000000000000000, 1.000000000000000222, 1.000000000000000000, 1.000000000000000000, 0.9999999999999996669, 1.000000000000000222, 1.000000000000000000, 0.9999999999999997780, 0.9999999999999997780, 0.9999999999999997780, 1.000000000000000000, 1.000000000000000222, 0.9999999999999997780, 1.000000000000000222, 0.9999999999999996669, 1.000000000000000444, 0.9999999999999997780, 1.000000000000000222, 1.000000000000000222, 0.9999999999999997780, 1.000000000000000222, 1.000000000000000000, 0.9999999999999997780, 1.000000000000000444, 1.000000000000000000, 1.000000000000000000, 1.000000000000000222, 1.000000000000000000, 1.000000000000000000, 1.000000000000000222, 0.9999999999999993339, 1.000000000000000444, 1.000000000000000222, 0.9999999999999997780, 1.000000000000000000, 1.000000000000000222, 1.000000000000000444, 1.000000000000000000, 1.000000000000000222, 0.9999999999999997780, 1.000000000000000222, 0.9999999999999997780, 1.000000000000000222, 1.000000000000000000, 0.9999999999999997780, 0.9999999999999996669, 1.000000000000000444, 0.9999999999999997780, 1.000000000000000444, 0.9999999999999997780, 1.000000000000000222, 1.000000000000000222, 1.000000000000000000, 0.9999999999999997780, 1.000000000000000222, 0.9999999999999997780, 1.000000000000000000, 1.000000000000000000, 1.000000000000000000, 0.9999999999999997780, 1.000000000000000222, 1.000000000000000000, 1.000000000000000000, 1.000000000000000000, 1.000000000000000222, 1.000000000000000222, 0.9999999999999994449, 1.000000000000000222, 1.000000000000000000, 0.9999999999999994449, 1.000000000000000444, 0.9999999999999997780, 1.000000000000000222, 0.9999999999999996669, 1.000000000000000444, 1.000000000000000000, 0.9999999999999996669, 1.000000000000000444, 0.9999999999999997780, 1.000000000000000000, 1.000000000000000444, 1.000000000000000000, 1.000000000000000222, 0.9999999999999996669, 1.000000000000000000, 0.9999999999999997780, 0.9999999999999997780, 1.000000000000000222, 1.000000000000000000, 1.000000000000000444, 0.9999999999999996669, 1.000000000000000222, 0.9999999999999997780, 0.9999999999999997780, 1.000000000000000444, 0.9999999999999997780, 1.000000000000000444, 0.9999999999999996669, 1.000000000000000222, 0.9999999999999996669, 1.000000000000000222, 0.9999999999999997780, 1.000000000000000444, 1.000000000000000222, 0.9999999999999996669, 1.000000000000000444, 0.9999999999999996669, 1.000000000000000000, 0.9999999999999997780, 1.000000000000000000, 1.000000000000000000, 1.000000000000000222, 0.9999999999999994449, 1.000000000000000444, 0.9999999999999993339, 1.000000000000000666, 0.9999999999999994449, 1.000000000000000222, 1.000000000000000222, 1.000000000000000000, 1.000000000000000000, 0.9999999999999997780, 1.000000000000000222, 0.9999999999999996669, 1.000000000000000222, 0.9999999999999996669, 1.000000000000000222, 1.000000000000000000, 1.000000000000000222, 0.9999999999999997780, 1.000000000000000222, 1.000000000000000222, 1.000000000000000000, 0.9999999999999997780, 1.000000000000000222, 1.000000000000000222, 1.000000000000000000, 1.000000000000000000, 1.000000000000000222, 0.9999999999999997780, 1.000000000000000000, 1.000000000000000222, 0.9999999999999996669, 0.9999999999999997780, 1.000000000000000222, 0.9999999999999997780, 1.000000000000000000, 0.9999999999999997780, 0.9999999999999997780, 1.000000000000000222, 1.000000000000000000, 1.000000000000000000, 1.000000000000000222, 0.9999999999999996669, 1.000000000000000444, 1.000000000000000000, 1.000000000000000222, 0.9999999999999997780, 1.000000000000000222, 0.9999999999999997780, 1.000000000000000444, 0.9999999999999997780, 1.000000000000000222, 0.9999999999999997780, 1.000000000000000222, 0.9999999999999997780, 1.000000000000000222, 1.000000000000000000, 1.000000000000000222, 1.000000000000000000, 1.000000000000000000, 1.000000000000000222, 1.000000000000000000, 1.000000000000000000, 0.9999999999999997780, 1.000000000000000000, 1.000000000000000444, 0.9999999999999996669, 1.000000000000000222, 0.9999999999999997780, 1.000000000000000000, 0.9999999999999997780, 1.000000000000000222, 1.000000000000000222, 1.000000000000000000, 1.000000000000000000, 0.9999999999999996669, 1.000000000000000444, 0.9999999999999997780, 1.000000000000000000, 1.000000000000000222, 0.9999999999999996669, 1.000000000000000444, 1.000000000000000000, 0.9999999999999997780, 1.000000000000000222, 0.9999999999999997780, 1.000000000000000000, 1.000000000000000000, 1.000000000000000000, 1.000000000000000000, 1.000000000000000000, 1.000000000000000222, 1.000000000000000444, 0.9999999999999997780, 1.000000000000000222, 1.000000000000000000, 1.000000000000000444, 0.9999999999999997780, 1.000000000000000222, 0.9999999999999997780, 1.000000000000000222, 0.9999999999999997780, 1.000000000000000222, 1.000000000000000000, 1.000000000000000222, 1.000000000000000222, 1.000000000000000222, 0.9999999999999997780, 1.000000000000000222, 0.9999999999999997780, 1.000000000000000222, 0.9999999999999997780, 1.000000000000000444, 0.9999999999999996669, 1.000000000000000444, 1.000000000000000000, 1.000000000000000000, 0.9999999999999997780, 1.000000000000000222, 1.000000000000000000, 0.9999999999999997780, 1.000000000000000000, 0.9999999999999997780, 1.000000000000000222, 1.000000000000000000, 1.000000000000000000, 1.000000000000000222, 0.9999999999999997780, 1.000000000000000444, 0.9999999999999996669, 1.000000000000000222, 1.000000000000000222, 0.9999999999999997780, 1.000000000000000000, 0.9999999999999997780, 1.000000000000000000, 0.9999999999999996669, 1.000000000000000444, 0.9999999999999997780, 1.000000000000000222, 1.000000000000000000, 1.000000000000000000, 1.000000000000000000, 0.9999999999999997780, 0.9999999999999997780, 1.000000000000000000, 0.9999999999999997780, 1.000000000000000444, 0.9999999999999996669, 1.000000000000000222, 1.000000000000000000, 1.000000000000000444, 1.000000000000000222, 1.000000000000000000, 0.9999999999999997780, 1.000000000000000222, 1.000000000000000444, 0.9999999999999997780, 1.000000000000000222, 0.9999999999999997780, 1.000000000000000000, 1.000000000000000000, 1.000000000000000222, 0.9999999999999997780, 1.000000000000000222, 1.000000000000000000, 1.000000000000000222, 0.9999999999999997780, 1.000000000000000000, 1.000000000000000222, 1.000000000000000000, 1.000000000000000222, 1.000000000000000000, 1.000000000000000000, 0.9999999999999997780, 1.000000000000000444, 0.9999999999999997780, 1.000000000000000000, 1.000000000000000000, 1.000000000000000444, 0.9999999999999996669, 1.000000000000000222, 1.000000000000000000, 0.9999999999999996669, 1.000000000000000444, 0.9999999999999996669, 1.000000000000000444, 0.9999999999999997780, 1.000000000000000222, 0.9999999999999997780, 1.000000000000000222, 1.000000000000000222, 1.000000000000000222, 1.000000000000000000, 1.000000000000000000, 1.000000000000000000),
 ( 0.3333333333333333703, 0.3333333333333333703, 0.3333333333333334259, 0.3333333333333334259, 0.3333333333333333703, 0.3333333333333334259, 0.3333333333333333148, 0.3333333333333333703, 0.3333333333333333148, 0.3333333333333333703, 0.3333333333333333703, 0.3333333333333334259, 0.3333333333333333703, 0.3333333333333333703, 0.3333333333333333703, 0.3333333333333333703, 0.3333333333333333703, 0.3333333333333333148, 0.3333333333333333703, 0.3333333333333334814, 0.3333333333333333148, 0.3333333333333334259, 0.3333333333333333148, 0.3333333333333334259, 0.3333333333333332593, 0.3333333333333335369, 0.3333333333333333703, 0.3333333333333333703, 0.3333333333333333703, 0.3333333333333333703, 0.3333333333333333703, 0.3333333333333333703, 0.3333333333333334259, 0.3333333333333333703, 0.3333333333333333703, 0.3333333333333333703, 0.3333333333333334814, 0.3333333333333333703, 0.3333333333333333703, 0.3333333333333333703, 0.3333333333333334259, 0.3333333333333332593, 0.3333333333333334814, 0.3333333333333332593, 0.3333333333333334259, 0.3333333333333332038, 0.3333333333333335369, 0.3333333333333332593, 0.3333333333333334814, 0.3333333333333333703, 0.3333333333333333148, 0.3333333333333333703, 0.3333333333333333703, 0.3333333333333333148, 0.3333333333333333148, 0.3333333333333334814, 0.3333333333333332593, 0.3333333333333334259, 0.3333333333333332593, 0.3333333333333333703, 0.3333333333333333703, 0.3333333333333334259, 0.3333333333333333148, 0.3333333333333333148, 0.3333333333333334259, 0.3333333333333333703, 0.3333333333333333703, 0.3333333333333333703, 0.3333333333333334814, 0.3333333333333332038, 0.3333333333333335924, 0.3333333333333332593, 0.3333333333333335369, 0.3333333333333333148, 0.3333333333333332593, 0.3333333333333335924, 0.3333333333333332038, 0.3333333333333333703, 0.3333333333333333703, 0.3333333333333334259, 0.3333333333333333148, 0.3333333333333334259, 0.3333333333333333703, 0.3333333333333334259, 0.3333333333333332038, 0.3333333333333333703, 0.3333333333333333703, 0.3333333333333333703, 0.3333333333333332593, 0.3333333333333333703, 0.3333333333333333148, 0.3333333333333334259, 0.3333333333333333148, 0.3333333333333334259, 0.3333333333333333148, 0.3333333333333334814, 0.3333333333333333703, 0.3333333333333334259, 0.3333333333333333703, 0.3333333333333333148, 0.3333333333333333703, 0.3333333333333334259, 0.3333333333333333148, 0.3333333333333334814, 0.3333333333333334259, 0.3333333333333333703, 0.3333333333333334259, 0.3333333333333333703, 0.3333333333333334259, 0.3333333333333334814, 0.3333333333333332038, 0.3333333333333334259, 0.3333333333333334259, 0.3333333333333333703, 0.3333333333333333148, 0.3333333333333334259, 0.3333333333333334259, 0.3333333333333334259, 0.3333333333333333703, 0.3333333333333333148, 0.3333333333333334259, 0.3333333333333333703, 0.3333333333333334259, 0.3333333333333333703, 0.3333333333333333148, 0.3333333333333332593, 0.3333333333333334259, 0.3333333333333333148, 0.3333333333333335369, 0.3333333333333332593, 0.3333333333333334814, 0.3333333333333334259, 0.3333333333333334259, 0.3333333333333333148, 0.3333333333333334259, 0.3333333333333333148, 0.3333333333333333148, 0.3333333333333333703, 0.3333333333333333703, 0.3333333333333332593, 0.3333333333333334259, 0.3333333333333333148, 0.3333333333333333703, 0.3333333333333334259, 0.3333333333333333148, 0.3333333333333334814, 0.3333333333333332593, 0.3333333333333333703, 0.3333333333333334259, 0.3333333333333332038, 0.3333333333333335369, 0.3333333333333333703, 0.3333333333333333703, 0.3333333333333333148, 0.3333333333333334259, 0.3333333333333333703, 0.3333333333333332593, 0.3333333333333335369, 0.3333333333333332593, 0.3333333333333333703, 0.3333333333333334814, 0.3333333333333333703, 0.3333333333333334259, 0.3333333333333332593, 0.3333333333333334259, 0.3333333333333332593, 0.3333333333333333703, 0.3333333333333334259, 0.3333333333333333703, 0.3333333333333334814, 0.3333333333333332593, 0.3333333333333333703, 0.3333333333333333703, 0.3333333333333333703, 0.3333333333333334259, 0.3333333333333333148, 0.3333333333333334259, 0.3333333333333332593, 0.3333333333333333703, 0.3333333333333332593, 0.3333333333333334814, 0.3333333333333333703, 0.3333333333333334259, 0.3333333333333334259, 0.3333333333333332593, 0.3333333333333334814, 0.3333333333333333148, 0.3333333333333333148, 0.3333333333333333148, 0.3333333333333333703, 0.3333333333333333703, 0.3333333333333334259, 0.3333333333333332593, 0.3333333333333335369, 0.3333333333333332038, 0.3333333333333335924, 0.3333333333333332593, 0.3333333333333334814, 0.3333333333333333703, 0.3333333333333333703, 0.3333333333333333703, 0.3333333333333333148, 0.3333333333333334259, 0.3333333333333333703, 0.3333333333333333703, 0.3333333333333333148, 0.3333333333333333703, 0.3333333333333333148, 0.3333333333333333703, 0.3333333333333332593, 0.3333333333333334259, 0.3333333333333333703, 0.3333333333333334259, 0.3333333333333333148, 0.3333333333333334259, 0.3333333333333333703, 0.3333333333333334259, 0.3333333333333334259, 0.3333333333333334259, 0.3333333333333332593, 0.3333333333333334259, 0.3333333333333333703, 0.3333333333333333148, 0.3333333333333333148, 0.3333333333333335369, 0.3333333333333332593, 0.3333333333333333148, 0.3333333333333333703, 0.3333333333333333148, 0.3333333333333334814, 0.3333333333333333703, 0.3333333333333334814, 0.3333333333333333703, 0.3333333333333332593, 0.3333333333333334259, 0.3333333333333333703, 0.3333333333333335369, 0.3333333333333333148, 0.3333333333333334259, 0.3333333333333333148, 0.3333333333333335924, 0.3333333333333332593, 0.3333333333333334259, 0.3333333333333334259, 0.3333333333333333703, 0.3333333333333333703, 0.3333333333333334259, 0.3333333333333334259, 0.3333333333333334259, 0.3333333333333333703, 0.3333333333333333703, 0.3333333333333334259, 0.3333333333333333148, 0.3333333333333333703, 0.3333333333333332038, 0.3333333333333334259, 0.3333333333333334814, 0.3333333333333332593, 0.3333333333333333703, 0.3333333333333333148, 0.3333333333333334814, 0.3333333333333332593, 0.3333333333333334259, 0.3333333333333333703, 0.3333333333333333703, 0.3333333333333333703, 0.3333333333333333148, 0.3333333333333334259, 0.3333333333333333703, 0.3333333333333333148, 0.3333333333333334259, 0.3333333333333332038, 0.3333333333333334259, 0.3333333333333333703, 0.3333333333333333703, 0.3333333333333333703, 0.3333333333333334259, 0.3333333333333333148, 0.3333333333333333703, 0.3333333333333333703, 0.3333333333333333703, 0.3333333333333333703, 0.3333333333333334259, 0.3333333333333334814, 0.3333333333333332593, 0.3333333333333333703, 0.3333333333333334259, 0.3333333333333334814, 0.3333333333333333148, 0.3333333333333333703, 0.3333333333333333703, 0.3333333333333334259, 0.3333333333333333148, 0.3333333333333334814, 0.3333333333333333148, 0.3333333333333334814, 0.3333333333333333703, 0.3333333333333334814, 0.3333333333333333148, 0.3333333333333334259, 0.3333333333333332593, 0.3333333333333335369, 0.3333333333333333148, 0.3333333333333334814, 0.3333333333333333148, 0.3333333333333334259, 0.3333333333333333703, 0.3333333333333333148, 0.3333333333333333703, 0.3333333333333333703, 0.3333333333333334259, 0.3333333333333333148, 0.3333333333333334259, 0.3333333333333333148, 0.3333333333333334814, 0.3333333333333333148, 0.3333333333333334259, 0.3333333333333334259, 0.3333333333333333703, 0.3333333333333334259, 0.3333333333333333703, 0.3333333333333333703, 0.3333333333333335369, 0.3333333333333332593, 0.3333333333333334259, 0.3333333333333333703, 0.3333333333333333703, 0.3333333333333333148, 0.3333333333333335369, 0.3333333333333333148, 0.3333333333333334259, 0.3333333333333333703, 0.3333333333333333703, 0.3333333333333334259, 0.3333333333333333148, 0.3333333333333333703, 0.3333333333333333148, 0.3333333333333333148, 0.3333333333333334814, 0.3333333333333332593, 0.3333333333333334259, 0.3333333333333333703, 0.3333333333333334814, 0.3333333333333334259, 0.3333333333333333148, 0.3333333333333333703, 0.3333333333333333703, 0.3333333333333335369, 0.3333333333333333148, 0.3333333333333334259, 0.3333333333333333703, 0.3333333333333333148, 0.3333333333333334259, 0.3333333333333334259, 0.3333333333333333703, 0.3333333333333333703, 0.3333333333333334259, 0.3333333333333334259, 0.3333333333333333703, 0.3333333333333333148, 0.3333333333333334259, 0.3333333333333333703, 0.3333333333333334814, 0.3333333333333333703, 0.3333333333333333703, 0.3333333333333333703, 0.3333333333333334259, 0.3333333333333333148, 0.3333333333333333703, 0.3333333333333334259, 0.3333333333333334259, 0.3333333333333333148, 0.3333333333333333703, 0.3333333333333333148, 0.3333333333333333703, 0.3333333333333335369, 0.3333333333333333148, 0.3333333333333334259, 0.3333333333333333703, 0.3333333333333334259, 0.3333333333333333148, 0.3333333333333333148, 0.3333333333333335369, 0.3333333333333333703, 0.3333333333333333148, 0.3333333333333333703, 0.3333333333333333703),
 ( 0.3333333333333333703, 0.3333333333333333703, 0.3333333333333334259, 0.3333333333333334259, 0.3333333333333333703, 0.3333333333333334259, 0.3333333333333333148, 0.3333333333333333703, 0.3333333333333333148, 0.3333333333333333703, 0.3333333333333333703, 0.3333333333333334259, 0.3333333333333333703, 0.3333333333333333703, 0.3333333333333333703, 0.3333333333333333703, 0.3333333333333333703, 0.3333333333333333148, 0.3333333333333333703, 0.3333333333333334814, 0.3333333333333333148, 0.3333333333333334259, 0.3333333333333333148, 0.3333333333333334259, 0.3333333333333332593, 0.3333333333333335369, 0.3333333333333333703, 0.3333333333333333703, 0.3333333333333333703, 0.3333333333333333703, 0.3333333333333333703, 0.3333333333333333703, 0.3333333333333334259, 0.3333333333333333703, 0.3333333333333333703, 0.3333333333333333703, 0.3333333333333334814, 0.3333333333333333703, 0.3333333333333333703, 0.3333333333333333703, 0.3333333333333334259, 0.3333333333333332593, 0.3333333333333334814, 0.3333333333333332593, 0.3333333333333334259, 0.3333333333333332038, 0.3333333333333335369, 0.3333333333333332593, 0.3333333333333334814, 0.3333333333333333703, 0.3333333333333333148, 0.3333333333333333703, 0.3333333333333333703, 0.3333333333333333148, 0.3333333333333333148, 0.3333333333333334814, 0.3333333333333332593, 0.3333333333333334259, 0.3333333333333332593, 0.3333333333333333703, 0.3333333333333333703, 0.3333333333333334259, 0.3333333333333333148, 0.3333333333333333148, 0.3333333333333334259, 0.3333333333333333703, 0.3333333333333333703, 0.3333333333333333703, 0.3333333333333334814, 0.3333333333333332038, 0.3333333333333335924, 0.3333333333333332593, 0.3333333333333335369, 0.3333333333333333148, 0.3333333333333332593, 0.3333333333333335924, 0.3333333333333332038, 0.3333333333333333703, 0.3333333333333333703, 0.3333333333333334259, 0.3333333333333333148, 0.3333333333333334259, 0.3333333333333333703, 0.3333333333333334259, 0.3333333333333332038, 0.3333333333333333703, 0.3333333333333333703, 0.3333333333333333703, 0.3333333333333332593, 0.3333333333333333703, 0.3333333333333333148, 0.3333333333333334259, 0.3333333333333333148, 0.3333333333333334259, 0.3333333333333333148, 0.3333333333333334814, 0.3333333333333333703, 0.3333333333333334259, 0.3333333333333333703, 0.3333333333333333148, 0.3333333333333333703, 0.3333333333333334259, 0.3333333333333333148, 0.3333333333333334814, 0.3333333333333334259, 0.3333333333333333703, 0.3333333333333334259, 0.3333333333333333703, 0.3333333333333334259, 0.3333333333333334814, 0.3333333333333332038, 0.3333333333333334259, 0.3333333333333334259, 0.3333333333333333703, 0.3333333333333333148, 0.3333333333333334259, 0.3333333333333334259, 0.3333333333333334259, 0.3333333333333333703, 0.3333333333333333148, 0.3333333333333334259, 0.3333333333333333703, 0.3333333333333334259, 0.3333333333333333703, 0.3333333333333333148, 0.3333333333333332593, 0.3333333333333334259, 0.3333333333333333148, 0.3333333333333335369, 0.3333333333333332593, 0.3333333333333334814, 0.3333333333333334259, 0.3333333333333334259, 0.3333333333333333148, 0.3333333333333334259, 0.3333333333333333148, 0.3333333333333333148, 0.3333333333333333703, 0.3333333333333333703, 0.3333333333333332593, 0.3333333333333334259, 0.3333333333333333148, 0.3333333333333333703, 0.3333333333333334259, 0.3333333333333333148, 0.3333333333333334814, 0.3333333333333332593, 0.3333333333333333703, 0.3333333333333334259, 0.3333333333333332038, 0.3333333333333335369, 0.3333333333333333703, 0.3333333333333333703, 0.3333333333333333148, 0.3333333333333334259, 0.3333333333333333703, 0.3333333333333332593, 0.3333333333333335369, 0.3333333333333332593, 0.3333333333333333703, 0.3333333333333334814, 0.3333333333333333703, 0.3333333333333334259, 0.3333333333333332593, 0.3333333333333334259, 0.3333333333333332593, 0.3333333333333333703, 0.3333333333333334259, 0.3333333333333333703, 0.3333333333333334814, 0.3333333333333332593, 0.3333333333333333703, 0.3333333333333333703, 0.3333333333333333703, 0.3333333333333334259, 0.3333333333333333148, 0.3333333333333334259, 0.3333333333333332593, 0.3333333333333333703, 0.3333333333333332593, 0.3333333333333334814, 0.3333333333333333703, 0.3333333333333334259, 0.3333333333333334259, 0.3333333333333332593, 0.3333333333333334814, 0.3333333333333333148, 0.3333333333333333148, 0.3333333333333333148, 0.3333333333333333703, 0.3333333333333333703, 0.3333333333333334259, 0.3333333333333332593, 0.3333333333333335369, 0.3333333333333332038, 0.3333333333333335924, 0.3333333333333332593, 0.3333333333333334814, 0.3333333333333333703, 0.3333333333333333703, 0.3333333333333333703, 0.3333333333333333148, 0.3333333333333334259, 0.3333333333333333703, 0.3333333333333333703, 0.3333333333333333148, 0.3333333333333333703, 0.3333333333333333148, 0.3333333333333333703, 0.3333333333333332593, 0.3333333333333334259, 0.3333333333333333703, 0.3333333333333334259, 0.3333333333333333148, 0.3333333333333334259, 0.3333333333333333703, 0.3333333333333334259, 0.3333333333333334259, 0.3333333333333334259, 0.3333333333333332593, 0.3333333333333334259, 0.3333333333333333703, 0.3333333333333333148, 0.3333333333333333148, 0.3333333333333335369, 0.3333333333333332593, 0.3333333333333333148, 0.3333333333333333703, 0.3333333333333333148, 0.3333333333333334814, 0.3333333333333333703, 0.3333333333333334814, 0.3333333333333333703, 0.3333333333333332593, 0.3333333333333334259, 0.3333333333333333703, 0.3333333333333335369, 0.3333333333333333148, 0.3333333333333334259, 0.3333333333333333148, 0.3333333333333335924, 0.3333333333333332593, 0.3333333333333334259, 0.3333333333333334259, 0.3333333333333333703, 0.3333333333333333703, 0.3333333333333334259, 0.3333333333333334259, 0.3333333333333334259, 0.3333333333333333703, 0.3333333333333333703, 0.3333333333333334259, 0.3333333333333333148, 0.3333333333333333703, 0.3333333333333332038, 0.3333333333333334259, 0.3333333333333334814, 0.3333333333333332593, 0.3333333333333333703, 0.3333333333333333148, 0.3333333333333334814, 0.3333333333333332593, 0.3333333333333334259, 0.3333333333333333703, 0.3333333333333333703, 0.3333333333333333703, 0.3333333333333333148, 0.3333333333333334259, 0.3333333333333333703, 0.3333333333333333148, 0.3333333333333334259, 0.3333333333333332038, 0.3333333333333334259, 0.3333333333333333703, 0.3333333333333333703, 0.3333333333333333703, 0.3333333333333334259, 0.3333333333333333148, 0.3333333333333333703, 0.3333333333333333703, 0.3333333333333333703, 0.3333333333333333703, 0.3333333333333334259, 0.3333333333333334814, 0.3333333333333332593, 0.3333333333333333703, 0.3333333333333334259, 0.3333333333333334814, 0.3333333333333333148, 0.3333333333333333703, 0.3333333333333333703, 0.3333333333333334259, 0.3333333333333333148, 0.3333333333333334814, 0.3333333333333333148, 0.3333333333333334814, 0.3333333333333333703, 0.3333333333333334814, 0.3333333333333333148, 0.3333333333333334259, 0.3333333333333332593, 0.3333333333333335369, 0.3333333333333333148, 0.3333333333333334814, 0.3333333333333333148, 0.3333333333333334259, 0.3333333333333333703, 0.3333333333333333148, 0.3333333333333333703, 0.3333333333333333703, 0.3333333333333334259, 0.3333333333333333148, 0.3333333333333334259, 0.3333333333333333148, 0.3333333333333334814, 0.3333333333333333148, 0.3333333333333334259, 0.3333333333333334259, 0.3333333333333333703, 0.3333333333333334259, 0.3333333333333333703, 0.3333333333333333703, 0.3333333333333335369, 0.3333333333333332593, 0.3333333333333334259, 0.3333333333333333703, 0.3333333333333333703, 0.3333333333333333148, 0.3333333333333335369, 0.3333333333333333148, 0.3333333333333334259, 0.3333333333333333703, 0.3333333333333333703, 0.3333333333333334259, 0.3333333333333333148, 0.3333333333333333703, 0.3333333333333333148, 0.3333333333333333148, 0.3333333333333334814, 0.3333333333333332593, 0.3333333333333334259, 0.3333333333333333703, 0.3333333333333334814, 0.3333333333333334259, 0.3333333333333333148, 0.3333333333333333703, 0.3333333333333333703, 0.3333333333333335369, 0.3333333333333333148, 0.3333333333333334259, 0.3333333333333333703, 0.3333333333333333148, 0.3333333333333334259, 0.3333333333333334259, 0.3333333333333333703, 0.3333333333333333703, 0.3333333333333334259, 0.3333333333333334259, 0.3333333333333333703, 0.3333333333333333148, 0.3333333333333334259, 0.3333333333333333703, 0.3333333333333334814, 0.3333333333333333703, 0.3333333333333333703, 0.3333333333333333703, 0.3333333333333334259, 0.3333333333333333148, 0.3333333333333333703, 0.3333333333333334259, 0.3333333333333334259, 0.3333333333333333148, 0.3333333333333333703, 0.3333333333333333148, 0.3333333333333333703, 0.3333333333333335369, 0.3333333333333333148, 0.3333333333333334259, 0.3333333333333333703, 0.3333333333333334259, 0.3333333333333333148, 0.3333333333333333148, 0.3333333333333335369, 0.3333333333333333703, 0.3333333333333333148, 0.3333333333333333703, 0.3333333333333333703),
 ( 1.000000000000000000, 1.000000000000000000, 1.000000000000000000, 1.000000000000000222, 0.9999999999999997780, 1.000000000000000444, 0.9999999999999997780, 1.000000000000000222, 0.9999999999999996669, 1.000000000000000000, 1.000000000000000000, 1.000000000000000222, 1.000000000000000000, 1.000000000000000000, 0.9999999999999997780, 1.000000000000000000, 1.000000000000000000, 1.000000000000000000, 0.9999999999999997780, 1.000000000000000444, 0.9999999999999997780, 1.000000000000000222, 1.000000000000000000, 0.9999999999999997780, 1.000000000000000000, 1.000000000000000222, 0.9999999999999997780, 1.000000000000000222, 0.9999999999999997780, 1.000000000000000222, 1.000000000000000000, 0.9999999999999997780, 1.000000000000000444, 0.9999999999999997780, 1.000000000000000222, 0.9999999999999997780, 1.000000000000000444, 1.000000000000000000, 1.000000000000000000, 1.000000000000000000, 1.000000000000000000, 1.000000000000000000, 1.000000000000000000, 0.9999999999999997780, 1.000000000000000222, 0.9999999999999996669, 1.000000000000000444, 0.9999999999999994449, 1.000000000000000222, 1.000000000000000000, 1.000000000000000000, 1.000000000000000000, 1.000000000000000000, 1.000000000000000000, 0.9999999999999996669, 1.000000000000000444, 0.9999999999999997780, 1.000000000000000222, 0.9999999999999996669, 1.000000000000000000, 1.000000000000000000, 1.000000000000000222, 0.9999999999999997780, 1.000000000000000000, 1.000000000000000222, 0.9999999999999997780, 1.000000000000000000, 0.9999999999999997780, 1.000000000000000222, 0.9999999999999997780, 1.000000000000000444, 0.9999999999999994449, 1.000000000000000444, 0.9999999999999997780, 0.9999999999999997780, 1.000000000000000444, 0.9999999999999996669, 1.000000000000000000, 1.000000000000000000, 1.000000000000000000, 1.000000000000000000, 1.000000000000000222, 1.000000000000000000, 1.000000000000000000, 0.9999999999999996669, 1.000000000000000222, 1.000000000000000000, 0.9999999999999997780, 0.9999999999999997780, 0.9999999999999997780, 1.000000000000000000, 1.000000000000000222, 0.9999999999999997780, 1.000000000000000222, 0.9999999999999996669, 1.000000000000000444, 0.9999999999999997780, 1.000000000000000222, 1.000000000000000222, 0.9999999999999997780, 1.000000000000000222, 1.000000000000000000, 0.9999999999999997780, 1.000000000000000444, 1.000000000000000000, 1.000000000000000000, 1.000000000000000222, 1.000000000000000000, 1.000000000000000000, 1.000000000000000222, 0.9999999999999993339, 1.000000000000000444, 1.000000000000000222, 0.9999999999999997780, 1.000000000000000000, 1.000000000000000222, 1.000000000000000444, 1.000000000000000000, 1.000000000000000222, 0.9999999999999997780, 1.000000000000000222, 0.9999999999999997780, 1.000000000000000222, 1.000000000000000000, 0.9999999999999997780, 0.9999999999999996669, 1.000000000000000444, 0.9999999999999997780, 1.000000000000000444, 0.9999999999999997780, 1.000000000000000222, 1.000000000000000222, 1.000000000000000000, 0.9999999999999997780, 1.000000000000000222, 0.9999999999999997780, 1.000000000000000000, 1.000000000000000000, 1.000000000000000000, 0.9999999999999997780, 1.000000000000000222, 1.000000000000000000, 1.000000000000000000, 1.000000000000000000, 1.000000000000000222, 1.000000000000000222, 0.9999999999999994449, 1.000000000000000222, 1.000000000000000000, 0.9999999999999994449, 1.000000000000000444, 0.9999999999999997780, 1.000000000000000222, 0.9999999999999996669, 1.000000000000000444, 1.000000000000000000, 0.9999999999999996669, 1.000000000000000444, 0.9999999999999997780, 1.000000000000000000, 1.000000000000000444, 1.000000000000000000, 1.000000000000000222, 0.9999999999999996669, 1.000000000000000000, 0.9999999999999997780, 0.9999999999999997780, 1.000000000000000222, 1.000000000000000000, 1.000000000000000444, 0.9999999999999996669, 1.000000000000000222, 0.9999999999999997780, 0.9999999999999997780, 1.000000000000000444, 0.9999999999999997780, 1.000000000000000444, 0.9999999999999996669, 1.000000000000000222, 0.9999999999999996669, 1.000000000000000222, 0.9999999999999997780, 1.000000000000000444, 1.000000000000000222, 0.9999999999999996669, 1.000000000000000444, 0.9999999999999996669, 1.000000000000000000, 0.9999999999999997780, 1.000000000000000000, 1.000000000000000000, 1.000000000000000222, 0.9999999999999994449, 1.000000000000000444, 0.9999999999999993339, 1.000000000000000666, 0.9999999999999994449, 1.000000000000000222, 1.000000000000000222, 1.000000000000000000, 1.000000000000000000, 0.9999999999999997780, 1.000000000000000222, 0.9999999999999996669, 1.000000000000000222, 0.9999999999999996669, 1.000000000000000222, 1.000000000000000000, 1.000000000000000222, 0.9999999999999997780, 1.000000000000000222, 1.000000000000000222, 1.000000000000000000, 0.9999999999999997780, 1.000000000000000222, 1.000000000000000222, 1.000000000000000000, 1.000000000000000000, 1.000000000000000222, 0.9999999999999997780, 1.000000000000000000, 1.000000000000000222, 0.9999999999999996669, 0.9999999999999997780, 1.000000000000000222, 0.9999999999999997780, 1.000000000000000000, 0.9999999999999997780, 0.9999999999999997780, 1.000000000000000222, 1.000000000000000000, 1.000000000000000000, 1.000000000000000222, 0.9999999999999996669, 1.000000000000000444, 1.000000000000000000, 1.000000000000000222, 0.9999999999999997780, 1.000000000000000222, 0.9999999999999997780, 1.000000000000000444, 0.9999999999999997780, 1.000000000000000222, 0.9999999999999997780, 1.000000000000000222, 0.9999999999999997780, 1.000000000000000222, 1.000000000000000000, 1.000000000000000222, 1.000000000000000000, 1.000000000000000000, 1.000000000000000222, 1.000000000000000000, 1.000000000000000000, 0.9999999999999997780, 1.000000000000000000, 1.000000000000000444, 0.9999999999999996669, 1.000000000000000222, 0.9999999999999997780, 1.000000000000000000, 0.9999999999999997780, 1.000000000000000222, 1.000000000000000222, 1.000000000000000000, 1.000000000000000000, 0.9999999999999996669, 1.000000000000000444, 0.9999999999999997780, 1.000000000000000000, 1.000000000000000222, 0.9999999999999996669, 1.000000000000000444, 1.000000000000000000, 0.9999999999999997780, 1.000000000000000222, 0.9999999999999997780, 1.000000000000000000, 1.000000000000000000, 1.000000000000000000, 1.000000000000000000, 1.000000000000000000, 1.000000000000000222, 1.000000000000000444, 0.9999999999999997780, 1.000000000000000222, 1.000000000000000000, 1.000000000000000444, 0.9999999999999997780, 1.000000000000000222, 0.9999999999999997780, 1.000000000000000222, 0.9999999999999997780, 1.000000000000000222, 1.000000000000000000, 1.000000000000000222, 1.000000000000000222, 1.000000000000000222, 0.9999999999999997780, 1.000000000000000222, 0.9999999999999997780, 1.000000000000000222, 0.9999999999999997780, 1.000000000000000444, 0.9999999999999996669, 1.000000000000000444, 1.000000000000000000, 1.000000000000000000, 0.9999999999999997780, 1.000000000000000222, 1.000000000000000000, 0.9999999999999997780, 1.000000000000000000, 0.9999999999999997780, 1.000000000000000222, 1.000000000000000000, 1.000000000000000000, 1.000000000000000222, 0.9999999999999997780, 1.000000000000000444, 0.9999999999999996669, 1.000000000000000222, 1.000000000000000222, 0.9999999999999997780, 1.000000000000000000, 0.9999999999999997780, 1.000000000000000000, 0.9999999999999996669, 1.000000000000000444, 0.9999999999999997780, 1.000000000000000222, 1.000000000000000000, 1.000000000000000000, 1.000000000000000000, 0.9999999999999997780, 0.9999999999999997780, 1.000000000000000000, 0.9999999999999997780, 1.000000000000000444, 0.9999999999999996669, 1.000000000000000222, 1.000000000000000000, 1.000000000000000444, 1.000000000000000222, 1.000000000000000000, 0.9999999999999997780, 1.000000000000000222, 1.000000000000000444, 0.9999999999999997780, 1.000000000000000222, 0.9999999999999997780, 1.000000000000000000, 1.000000000000000000, 1.000000000000000222, 0.9999999999999997780, 1.000000000000000222, 1.000000000000000000, 1.000000000000000222, 0.9999999999999997780, 1.000000000000000000, 1.000000000000000222, 1.000000000000000000, 1.000000000000000222, 1.000000000000000000, 1.000000000000000000, 0.9999999999999997780, 1.000000000000000444, 0.9999999999999997780, 1.000000000000000000, 1.000000000000000000, 1.000000000000000444, 0.9999999999999996669, 1.000000000000000222, 1.000000000000000000, 0.9999999999999996669, 1.000000000000000444, 0.9999999999999996669, 1.000000000000000444, 0.9999999999999997780, 1.000000000000000222, 0.9999999999999997780, 1.000000000000000222, 1.000000000000000222, 1.000000000000000222, 1.000000000000000000, 1.000000000000000000, 1.000000000000000000) ) ) 
 REPRESENTATION_ITEM ( '' )  SURFACE ( )  );
#13144 = CARTESIAN_POINT ( 'NONE',  ( 1.487047289068929246, 2.092300142875534341, 0.5796043027312002272 ) ) ;
#13145 = CARTESIAN_POINT ( 'NONE',  ( 2.219935720625454412, 0.9462983093676997637, -1.780669029686342331 ) ) ;
#13146 = CARTESIAN_POINT ( 'NONE',  ( 5.406250000000002665, 1.895863743163962223, -0.7852924748302683167 ) ) ;
#13147 = CARTESIAN_POINT ( 'NONE',  ( -1.500000000000013101, 2.160416667349489561, -0.8660254037844313801 ) ) ;
#13148 = CARTESIAN_POINT ( 'NONE',  ( 6.516243422921982109, -0.9108434941001318785, -1.697579817862464147 ) ) ;
#13149 = CARTESIAN_POINT ( 'NONE',  ( 1.364683531249996529, 12.71354166700806232, 0.7879004041258405033 ) ) ;
#13150 = CARTESIAN_POINT ( 'NONE',  ( 3.041495853084168921, 0.05845243686668395028, 2.220815690970390222 ) ) ;
#13151 = ORIENTED_EDGE ( 'NONE', *, *, #240, .T. ) ;
#13152 = CARTESIAN_POINT ( 'NONE',  ( -9.578796289607002024, -9.978085408363298825, 0.1296641399399101613 ) ) ;
#13153 = CARTESIAN_POINT ( 'NONE',  ( -1.500000000000015099, -0.6208333333333116988, -0.8660254037844383745 ) ) ;
#13154 = CARTESIAN_POINT ( 'NONE',  ( 7.214910300766615769, 11.56914578420308715, -0.7998128361456291469 ) ) ;
#13155 = CARTESIAN_POINT ( 'NONE',  ( 0.6823417656249882723, -1.157291666325249713, 1.181850606188755259 ) ) ;
#13156 = AXIS2_PLACEMENT_3D ( 'NONE', #103741, #87490, #6203 ) ;
#13157 = CARTESIAN_POINT ( 'NONE',  ( 5.671390581117805141, 1.043574818874394294, 1.392714124641497131 ) ) ;
#13158 = CARTESIAN_POINT ( 'NONE',  ( 3.824618516750320385, -1.319357783791510919, 1.452116237791359232 ) ) ;
#13160 = CARTESIAN_POINT ( 'NONE',  ( -7.239690840017442675, 7.548653522882887934, 0.7216878364870317197 ) ) ;
#13159 = CARTESIAN_POINT ( 'NONE',  ( 2.900554798319789906, 5.471398800426671372, 1.199719254218452047 ) ) ;
#13161 = CARTESIAN_POINT ( 'NONE',  ( -1.445379498298575260, 4.137219402008315505, 0.4160626371120850209 ) ) ;
#13162 = CARTESIAN_POINT ( 'NONE',  ( 4.165478197628463164, 0.2823181557158191968, -2.244685958880874743 ) ) ;
#13163 = CARTESIAN_POINT ( 'NONE',  ( 1.715356188534086224, -1.767971037936959089, -1.062312629515406170 ) ) ;
#13164 = CARTESIAN_POINT ( 'NONE',  ( -5.669280788808708671, 9.765911353585494226, 0.7998128361456481317 ) ) ;
#13165 = CARTESIAN_POINT ( 'NONE',  ( 2.712116605023757288, -2.238012884330255581, 0.3312714459411686962 ) ) ;
#13166 = VERTEX_POINT ( 'NONE', #175703 ) ;
#13167 = CARTESIAN_POINT ( 'NONE',  ( -1.402160292154681736E-14, 1.618750000682814827, -1.732050807568863648 ) ) ;
#13168 = CARTESIAN_POINT ( 'NONE',  ( 3.901501827272614964, -0.5455803081039903857, 1.789184164884791706 ) ) ;
#13169 = CARTESIAN_POINT ( 'NONE',  ( 2.215074966175926363, 1.682300057933778126, 0.4202854259360877531 ) ) ;
#13170 = CARTESIAN_POINT ( 'NONE',  ( 6.515165533258342023, -2.126321577054360201, 0.5302794918828001025 ) ) ;
#13171 = CARTESIAN_POINT ( 'NONE',  ( 6.458097596740710600, 2.302054065074070177, -0.1608065221961554325 ) ) ;
#13172 = B_SPLINE_CURVE_WITH_KNOTS ( 'NONE', 3,
 ( #80272, #145323, #146370, #48851 ),
 .UNSPECIFIED., .F., .F.,
 ( 4, 4 ),
 ( 0.01196238986099508982, 0.01242187503699302212 ),
 .UNSPECIFIED. ) ;
#13173 = CARTESIAN_POINT ( 'NONE',  ( 3.749029689823797806, -1.768526636652943296, 1.242828150824742961 ) ) ;
#13174 = CARTESIAN_POINT ( 'NONE',  ( 5.015543440151827959, -1.040391601716946557, -1.639569664018299289 ) ) ;
#13175 = CARTESIAN_POINT ( 'NONE',  ( -2.779058300676980675, 5.225689869889666106, -1.082531754730543083 ) ) ;
#13177 = UNCERTAINTY_MEASURE_WITH_UNIT (LENGTH_MEASURE( 1.000000000000000082E-05 ), #106243, 'distance_accuracy_value', 'NONE');
#13176 = CARTESIAN_POINT ( 'NONE',  ( 6.344977084850584426, -1.580176071495458023, 1.000667393836668362 ) ) ;
#13178 = PRESENTATION_STYLE_ASSIGNMENT (( #194059 ) ) ;
#13179 = CARTESIAN_POINT ( 'NONE',  ( 4.618273733618881494, 6.903169301580018846, 1.208453198238930382 ) ) ;
#13180 = CARTESIAN_POINT ( 'NONE',  ( -11.84668730067608600, 13.39999999999998259, 1.399999999999998579 ) ) ;
#13181 = EDGE_CURVE ( 'NONE', #159273, #176022, #202247, .T. ) ;
#13182 = CARTESIAN_POINT ( 'NONE',  ( 0.6801582343749883464, 2.473958333674766585, 1.178068619123824323 ) ) ;
#13183 = CARTESIAN_POINT ( 'NONE',  ( 5.590470263882489910, -0.4872053753022275169, 1.956560708789633285 ) ) ;
#13184 = CARTESIAN_POINT ( 'NONE',  ( -9.480175724453545172, 12.08329098332774265, 1.599625672291281386 ) ) ;
#13185 = CARTESIAN_POINT ( 'NONE',  ( 7.690499447449630210, 9.995335326823163058, 1.599625672291281386 ) ) ;
#13186 = CARTESIAN_POINT ( 'NONE',  ( 11.97181042169640897, 12.22000000000000064, 0.8318531151397160484 ) ) ;
#13187 = CARTESIAN_POINT ( 'NONE',  ( 3.387140609607977026, 1.650079954178599539, -0.7815607168924765258 ) ) ;
#13188 = DIRECTION ( 'NONE',  ( 0.000000000000000000, 0.000000000000000000, 1.000000000000000000 ) ) ;
#13189 = EDGE_LOOP ( 'NONE', ( #126180, #83708, #68325, #174794 ) ) ;
#13191 = MANIFOLD_SOLID_BREP ( 'Cut-Revolve1', #101781 ) ;
#13190 = CARTESIAN_POINT ( 'NONE',  ( -5.112833325684920993, 6.097965313788082931, -1.082531754730549967 ) ) ;
#13192 = CARTESIAN_POINT ( 'NONE',  ( 3.285556943749998737, -3.492708332855374742, -1.896917185911906500 ) ) ;
#13193 = CARTESIAN_POINT ( 'NONE',  ( -6.835281999583978418, 11.12624609948998966, -0.7998128361456291469 ) ) ;
#13194 = CARTESIAN_POINT ( 'NONE',  ( 0.6330766797960291070, 1.867852534778514428, 0.7690482435470397116 ) ) ;
#13195 = CARTESIAN_POINT ( 'NONE',  ( 1.366058183223411771, 0.6122477967837879342, -2.030190212274018524 ) ) ;
#13196 = EDGE_LOOP ( 'NONE', ( #154646, #111216, #105783, #111891 ) ) ;
#13197 = CARTESIAN_POINT ( 'NONE',  ( -4.450819567036169211, 8.414649604842665553, -0.7998128361456362523 ) ) ;
#13198 = CARTESIAN_POINT ( 'NONE',  ( 2.342426049922683884, -1.823874001192757666, -0.3686824239186973218 ) ) ;
#13199 = CARTESIAN_POINT ( 'NONE',  ( 4.599240423533799138, 6.388866465587984322, 1.599625672291267398 ) ) ;
#13200 = CARTESIAN_POINT ( 'NONE',  ( 6.473517581629535833, 1.972881934646727231, -0.5958391983454867091 ) ) ;
#13201 = CARTESIAN_POINT ( 'NONE',  ( 6.029922689959810178, -1.701949372586025744, 1.081063231324945528 ) ) ;
#13202 = ORIENTED_EDGE ( 'NONE', *, *, #124581, .T. ) ;
#13203 = ORIENTED_EDGE ( 'NONE', *, *, #212409, .T. ) ;
#13204 = ORIENTED_EDGE ( 'NONE', *, *, #81172, .F. ) ;
#13205 = CARTESIAN_POINT ( 'NONE',  ( -9.001723924469462901, 12.58942944760136484, -1.199719254218446718 ) ) ;
#13206 = CARTESIAN_POINT ( 'NONE',  ( 3.914527900857078357, 1.289819402409349669, -1.292354223553587644 ) ) ;
#13207 = VECTOR ( 'NONE', #45628, 1000.000000000000000 ) ;
#13210 = ORIENTED_EDGE ( 'NONE', *, *, #102718, .T. ) ;
#13209 = CARTESIAN_POINT ( 'NONE',  ( -5.969600656924041182, 6.101865228085409321, -0.7346798775042752139 ) ) ;
#13208 = CARTESIAN_POINT ( 'NONE',  ( -3.481411583659053566, 7.283673624236017830, 0.000000000000000000 ) ) ;
#13211 = CARTESIAN_POINT ( 'NONE',  ( 6.459053645710411296, 6.863086831863287607, 0.6637952124323226455 ) ) ;
#13212 = CARTESIAN_POINT ( 'NONE',  ( 5.923203835008548523, 0.8145033986626595279, 1.844426808122232142 ) ) ;
#13213 = CARTESIAN_POINT ( 'NONE',  ( 5.402248404572855378, 1.391679675130308880, -1.205515946264820615 ) ) ;
#13214 = CARTESIAN_POINT ( 'NONE',  ( 0.07680821025391781909, 4.096870002413341538, -2.365840309731046975 ) ) ;
#13215 = CARTESIAN_POINT ( 'NONE',  ( 3.809432652880593739, 1.978559473273227232, 1.187534574604662607 ) ) ;
#13216 = CARTESIAN_POINT ( 'NONE',  ( 6.852720297064418986, 6.959538199522133262, 0.7998128361456331437 ) ) ;
#13217 = CARTESIAN_POINT ( 'NONE',  ( 5.571600594950134600, 2.084881007647599205, -0.5705972643132785072 ) ) ;
#13218 = CARTESIAN_POINT ( 'NONE',  ( 6.632963465583686435, 8.761543347979550589, -1.599625672291262513 ) ) ;
#13219 = CARTESIAN_POINT ( 'NONE',  ( 0.8900594323104525918, -0.4731300603538539096, -1.883416623991182481 ) ) ;
#13220 = ORIENTED_EDGE ( 'NONE', *, *, #116206, .T. ) ;
#13221 = CARTESIAN_POINT ( 'NONE',  ( 4.165566195501821056, -0.7159155550505342802, -2.184124419653421523 ) ) ;
#13222 = CYLINDRICAL_SURFACE ( 'NONE', #176127, 8.500000000000000000 ) ;
#13223 = CARTESIAN_POINT ( 'NONE',  ( -7.370792787684826486, 8.628288336167626582, -1.199719254218452047 ) ) ;
#13224 = CARTESIAN_POINT ( 'NONE',  ( 4.627732503263369601, -1.150995203733524930, -1.474563928533303869 ) ) ;
#13225 = EDGE_LOOP ( 'NONE', ( #109414, #214149, #122485, #212579, #28246 ) ) ;
#13226 = AXIS2_PLACEMENT_3D ( 'NONE', #18445, #17366, #83450 ) ;
#13229 = CARTESIAN_POINT ( 'NONE',  ( -6.069210040772897052, 7.109775131437022999, -1.199719254218453823 ) ) ;
#13228 = CARTESIAN_POINT ( 'NONE',  ( 0.7499999999999885647, 0.01458333401615358182, 1.299038105676657340 ) ) ;
#13227 = CARTESIAN_POINT ( 'NONE',  ( 1.863391182279940494, -1.538030936729195552, -1.136358088520472931 ) ) ;
#13230 = CARTESIAN_POINT ( 'NONE',  ( 4.073040751519330094, -2.058760688187323495, -0.7953439701907027981 ) ) ;
#13231 = EDGE_CURVE ( 'NONE', #71477, #92865, #179495, .T. ) ;
#13232 = CARTESIAN_POINT ( 'NONE',  ( 6.883263157960408662, 2.979503955789930547, 2.299731230128279513 ) ) ;
#13233 = CARTESIAN_POINT ( 'NONE',  ( 7.334597915313080918, 9.580116872663850813, 1.040834085586084257E-14 ) ) ;
#13234 = CARTESIAN_POINT ( 'NONE',  ( 5.343321937117211817, 9.247976336696488886, 0.000000000000000000 ) ) ;
#13235 = CARTESIAN_POINT ( 'NONE',  ( -3.623053363349869382, 5.249981562040033189, 1.599625672291267398 ) ) ;
#13236 = CARTESIAN_POINT ( 'NONE',  ( -5.085717018457573957, 8.947437264926888290, 0.7216878364870267237 ) ) ;
#13237 = CARTESIAN_POINT ( 'NONE',  ( 2.003138245156708130, 1.636809484843353868, 1.098402624201348488 ) ) ;
#13238 = CARTESIAN_POINT ( 'NONE',  ( 0.8687466845767909396, 1.140460243972157395, 2.005982166855703852 ) ) ;
#13239 = CARTESIAN_POINT ( 'NONE',  ( 3.068751266904270025, 1.422870340827029345, -1.350941015047700366 ) ) ;
#13240 = FACE_OUTER_BOUND ( 'NONE', #186738, .T. ) ;
#13241 = CARTESIAN_POINT ( 'NONE',  ( 5.137578304370245874, 1.926469575665398448, -0.7373178810637993630 ) ) ;
#13242 = CARTESIAN_POINT ( 'NONE',  ( 5.368665641331531013, 5.365790791082654998, -0.7216878364870207285 ) ) ;
#13243 = CARTESIAN_POINT ( 'NONE',  ( 6.201928923608456046, 6.200281597156833691, 0.7998128361456352531 ) ) ;
#13244 = ORIENTED_EDGE ( 'NONE', *, *, #120497, .F. ) ;
#13245 = CARTESIAN_POINT ( 'NONE',  ( 1.364683531249988535, 5.717708333674752730, -0.7879004041258300672 ) ) ;
#13246 = CARTESIAN_POINT ( 'NONE',  ( 10.85353573482951717, -6.836568542495036205, -0.4635785636673637189 ) ) ;
#13247 = CARTESIAN_POINT ( 'NONE',  ( 10.07387183015377197, 11.71160420905630062, -1.199719254218440723 ) ) ;
#13248 = CARTESIAN_POINT ( 'NONE',  ( 0.8136159317379263456, -1.833160233796997218, -1.162963494187698510 ) ) ;
#13249 = DIRECTION ( 'NONE',  ( 0.000000000000000000, 0.000000000000000000, 1.000000000000000000 ) ) ;
#13250 = ADVANCED_FACE ( 'NONE', ( #18963 ), #49281, .T. ) ;
#13251 = CARTESIAN_POINT ( 'NONE',  ( 11.57407876878489716, 2.018041202053835637, -3.760646157729463646 ) ) ;
#13252 = CARTESIAN_POINT ( 'NONE',  ( -6.905598479220833141, -7.287292266636207216, 6.905598479220857122 ) ) ;
#13253 = CARTESIAN_POINT ( 'NONE',  ( 2.952262541859524969, 0.6266372353985818489, 1.762611677789377440 ) ) ;
#13254 = CARTESIAN_POINT ( 'NONE',  ( 6.784453917077649443, -2.118420112955111456, -0.4290502581522498415 ) ) ;
#13256 = CARTESIAN_POINT ( 'NONE',  ( 6.827182134110233669, 2.103728865748891508, 2.021873693915546610 ) ) ;
#13255 = SURFACE_STYLE_USAGE ( .BOTH. , #98787 ) ;
#13257 = CARTESIAN_POINT ( 'NONE',  ( -1.402160292154681736E-14, -0.5531249996585814177, -1.575800808251665908 ) ) ;
#13258 = CARTESIAN_POINT ( 'NONE',  ( 2.772007568003355793, 1.902874960710929431, -0.1895390408453850317 ) ) ;
#13259 = CARTESIAN_POINT ( 'NONE',  ( 4.469463222250699808, 1.716395428585426153, -0.4311418314640375615 ) ) ;
#13260 = CARTESIAN_POINT ( 'NONE',  ( 1.787617358713189386, 1.829539840090635749, -0.5563488465884156575 ) ) ;
#13261 = CARTESIAN_POINT ( 'NONE',  ( -6.579784621333750749, 6.570836901177822931, 0.7998128361456341429 ) ) ;
#13263 = CARTESIAN_POINT ( 'NONE',  ( 5.448823958578076443, -1.733895640293681373, -0.8146214837579464074 ) ) ;
#13262 = CARTESIAN_POINT ( 'NONE',  ( 7.960263458884762500, -6.452016312668102493, -7.960263458884791810 ) ) ;
#13264 = CARTESIAN_POINT ( 'NONE',  ( 0.2212536527127808295, -1.848710500310095872, -0.9322282823912150240 ) ) ;
#13265 = CARTESIAN_POINT ( 'NONE',  ( 0.7499999999999920064, 5.233333333333353821, 1.299038105676669330 ) ) ;
#13266 = CARTESIAN_POINT ( 'NONE',  ( 2.461320219219771843, -1.760565900816572826, 1.181798851529712646 ) ) ;
#13267 = CARTESIAN_POINT ( 'NONE',  ( 4.963960565410041603, 8.060099936542098220, -1.154953748940761971 ) ) ;
#13268 = CARTESIAN_POINT ( 'NONE',  ( 4.856247981345184428, 0.7163626499266174674, 1.728251504774950709 ) ) ;
#13270 = ORIENTED_EDGE ( 'NONE', *, *, #5165, .T. ) ;
#13269 = CARTESIAN_POINT ( 'NONE',  ( 1.154616158753757338, -1.440623569337009968, 1.121372061650728558 ) ) ;
#13272 = CARTESIAN_POINT ( 'NONE',  ( 5.107728353013315292, 7.811434107096660640, 1.148430247377411728 ) ) ;
#13271 = CARTESIAN_POINT ( 'NONE',  ( 5.127635347277352373, -2.096377701570474539, 0.6897739467496829535 ) ) ;
#13273 = CARTESIAN_POINT ( 'NONE',  ( -1.402160292154681736E-14, -0.5531249996585814177, -1.575800808251665908 ) ) ;
#13274 = CARTESIAN_POINT ( 'NONE',  ( 1.434110160756268737, 1.226943730116908160, 1.657962230405624515 ) ) ;
#13275 = CARTESIAN_POINT ( 'NONE',  ( 6.986529229743720926, 7.045372277656132276, -0.7998128361456281477 ) ) ;
#13276 = CARTESIAN_POINT ( 'NONE',  ( -7.330154606482786050, 11.70359747420527619, 0.000000000000000000 ) ) ;
#13277 = SURFACE_SIDE_STYLE ('',( #130315 ) ) ;
#13278 = CARTESIAN_POINT ( 'NONE',  ( 1.400363088670474765, 3.349293939923656982, 0.06128031220414761893 ) ) ;
#13279 = ADVANCED_FACE ( 'NONE', ( #131843 ), #136074, .T. ) ;
#13280 = CARTESIAN_POINT ( 'NONE',  ( -1.420000000000021911, 6.280000000000042881, 2.873333333333347728 ) ) ;
#13281 = CARTESIAN_POINT ( 'NONE',  ( 5.182959862174088883, 9.268813282503625572, 0.7998128361456331437 ) ) ;
#13282 = EDGE_LOOP ( 'NONE', ( #34437, #147889, #139099, #39048 ) ) ;
#13283 = CARTESIAN_POINT ( 'NONE',  ( 4.439934286204096914, 1.349936692791346093, 1.569845735447549906 ) ) ;
#13284 = CARTESIAN_POINT ( 'NONE',  ( 1.364683531249986537, -1.073958332991911790, 0.7879004041258500513 ) ) ;
#13285 = CARTESIAN_POINT ( 'NONE',  ( 2.126461914815626297, 1.246462439515462650, -1.765816729463750123 ) ) ;
#13286 = CARTESIAN_POINT ( 'NONE',  ( -6.033312665451926904, 7.071988487544162538, -1.043104321438679039 ) ) ;
#13287 = CARTESIAN_POINT ( 'NONE',  ( 3.440107494509841768, -1.204893485711604484, -1.620726792054197452 ) ) ;
#13288 = CARTESIAN_POINT ( 'NONE',  ( 6.620655732516651071, 4.689394895873098434, 2.736297475404291024 ) ) ;
#13289 = VERTEX_POINT ( 'NONE', #185859 ) ;
#13291 = CARTESIAN_POINT ( 'NONE',  ( 7.375272376154084597, 9.627570410311676596, -1.443375672974057666 ) ) ;
#13290 = CARTESIAN_POINT ( 'NONE',  ( 1.737500000000001155, -0.9333333333333346804, 3.009438278150922130 ) ) ;
#13292 = CARTESIAN_POINT ( 'NONE',  ( -4.963693635934603776, 4.963599794778024155, 0.000000000000000000 ) ) ;
#13293 = CARTESIAN_POINT ( 'NONE',  ( 1.411342602523330214, -1.897109289313268166, 0.6839406069230756779 ) ) ;
#13294 = CARTESIAN_POINT ( 'NONE',  ( 5.530878137806295669, -1.981686641427220286, 0.9361944923952856268 ) ) ;
#13295 = CARTESIAN_POINT ( 'NONE',  ( -1.500000000000011324, 4.702083334016148974, 0.8660254037844403729 ) ) ;
#13296 = CARTESIAN_POINT ( 'NONE',  ( 4.289254230599209627, -0.005406649120142519548, -1.912571728590661380 ) ) ;
#13297 = CARTESIAN_POINT ( 'NONE',  ( -3.684065054611367351, 5.321161868511784299, -1.599625672291256295 ) ) ;
#13298 = CARTESIAN_POINT ( 'NONE',  ( 6.493992390821439642, 7.639041213122241381, -1.082531754730543971 ) ) ;
#13300 = CARTESIAN_POINT ( 'NONE',  ( 1.775017769237042353, 1.753020666602569166, -0.9963212463810557917 ) ) ;
#13299 = CARTESIAN_POINT ( 'NONE',  ( -9.951321562306267410, 10.71222269888655987, 1.040834085586084257E-14 ) ) ;
#13301 = CARTESIAN_POINT ( 'NONE',  ( -0.6823417656250003738, 14.21354166700806232, 1.181850606188754593 ) ) ;
#13302 = CARTESIAN_POINT ( 'NONE',  ( -5.517242166118370150, 5.401480380085008193, 0.7998128361456281477 ) ) ;
#13303 = CARTESIAN_POINT ( 'NONE',  ( 4.805503449324158183, -0.4579143662744952770, 1.662777411968613839 ) ) ;
#13304 = DIRECTION ( 'NONE',  ( 0.000000000000000000, 0.000000000000000000, 1.000000000000000000 ) ) ;
#13305 = CARTESIAN_POINT ( 'NONE',  ( 9.571693261567961741, 11.22969222899322617, 1.082531754730548412 ) ) ;
#13306 = DIRECTION ( 'NONE',  ( 0.000000000000000000, -1.000000000000000000, 0.000000000000000000 ) ) ;
#13307 = CARTESIAN_POINT ( 'NONE',  ( 4.650610384687404952, 5.384465856012134566, 1.199719254218462483 ) ) ;
#13308 = CARTESIAN_POINT ( 'NONE',  ( 6.116136693540529912, 10.14959355252369910, 1.530808498934192557E-16 ) ) ;
#13309 = CARTESIAN_POINT ( 'NONE',  ( 1.059532578591013463, 1.690300726139557952, 1.195051122980017144 ) ) ;
#13310 = ORIENTED_EDGE ( 'NONE', *, *, #98482, .T. ) ;
#13311 = CARTESIAN_POINT ( 'NONE',  ( 5.232992382607310589, 1.676000702356477134, 0.6878641890804160219 ) ) ;
#13312 = CARTESIAN_POINT ( 'NONE',  ( 4.692003678781083487, 7.631698837623355658, -1.199719254218450271 ) ) ;
#13313 = CARTESIAN_POINT ( 'NONE',  ( 0.000000000000000000, 9.719999999999998863, 0.000000000000000000 ) ) ;
#13314 = CARTESIAN_POINT ( 'NONE',  ( 6.569024019911770651, -1.395121139060730542, 1.155258474184825745 ) ) ;
#13315 = CARTESIAN_POINT ( 'NONE',  ( 5.194182247366869731, 7.153241603385088965, 1.443375672974064550 ) ) ;
#13316 = AXIS2_PLACEMENT_3D ( 'NONE', #40178, #150741, #2303 ) ;
#13317 = CARTESIAN_POINT ( 'NONE',  ( -1.201851678989727383E-14, 3.259375000341420581, -1.575800808251660134 ) ) ;
#13318 = CARTESIAN_POINT ( 'NONE',  ( 3.328257738700185264, 2.138080787187321086, 0.4799892483983853042 ) ) ;
#13319 = ORIENTED_EDGE ( 'NONE', *, *, #200558, .T. ) ;
#13321 = CARTESIAN_POINT ( 'NONE',  ( 8.646349277213076334, 11.11049346154719508, 1.599625672291281386 ) ) ;
#13320 = CARTESIAN_POINT ( 'NONE',  ( 0.6956633456795427994, -1.384754418207832405, -1.389998539416361423 ) ) ;
#13322 = CARTESIAN_POINT ( 'NONE',  ( 4.429236352518686637, -1.483253864829991775, -1.212251590588450112 ) ) ;
#13323 = CARTESIAN_POINT ( 'NONE',  ( -0.4000000000000045186, 3.099999999999991651, -0.3423093779010097926 ) ) ;
#13324 = CARTESIAN_POINT ( 'NONE',  ( -0.6823417656250003738, 0.4677083336747517306, -1.181850606188749264 ) ) ;
#13326 = ORIENTED_EDGE ( 'NONE', *, *, #167509, .F. ) ;
#13325 = CARTESIAN_POINT ( 'NONE',  ( 4.338245966692901412, 8.005111361209628740, -0.7216878364870197293 ) ) ;
#13327 = CARTESIAN_POINT ( 'NONE',  ( -9.653042183249972652, 10.36423008998754192, -0.7216878364870267237 ) ) ;
#13328 = CARTESIAN_POINT ( 'NONE',  ( 1.587033755777764510, -0.3173376132806354222, -2.138153673666403964 ) ) ;
#13329 = CARTESIAN_POINT ( 'NONE',  ( -3.610214042988883598, 7.433943160120816351, 0.7998128361456352531 ) ) ;
#13330 = CARTESIAN_POINT ( 'NONE',  ( 3.854260808034858155, 7.718664386007802136, -0.7998128361456362523 ) ) ;
#13331 = CARTESIAN_POINT ( 'NONE',  ( 1.975362765405625609, 1.747911882041437659, -0.5268472171036930884 ) ) ;
#13332 = CARTESIAN_POINT ( 'NONE',  ( -5.101945877444165944, 4.846691699973280976, 0.000000000000000000 ) ) ;
#13333 = CARTESIAN_POINT ( 'NONE',  ( 4.770415466175468744, -1.191763575130764696, 1.382976834283907053 ) ) ;
#13335 = CARTESIAN_POINT ( 'NONE',  ( 9.263363473337784981, 13.05588735459848948, -8.991178861817273216 ) ) ;
#13334 =( BOUNDED_SURFACE ( )  B_SPLINE_SURFACE ( 3, 2, ( 
 ( #16974, #1789, #47401 ),
 ( #113513, #34307, #129781 ),
 ( #114576, #63627, #15914 ),
 ( #64682, #150217, #130828 ),
 ( #81997, #79865, #132917 ),
 ( #182689, #33248, #131865 ),
 ( #196820, #148084, #48462 ),
 ( #145974, #214089, #198922 ),
 ( #195762, #194684, #100382 ),
 ( #49504, #112442, #147031 ),
 ( #96153, #712, #128713 ),
 ( #166454, #163267, #180568 ),
 ( #83055, #32190, #65717 ),
 ( #213053, #99332, #116690 ) ),
 .UNSPECIFIED., .F., .F., .T. ) 
 B_SPLINE_SURFACE_WITH_KNOTS ( ( 4, 2, 2, 2, 2, 2, 4 ),
 ( 3, 3 ),
 ( 0.000000000000000000, 0.0002390010041311323369, 0.0004780020082622646739, 0.0009560040165245293478, 0.001195005020655661712, 0.001434006024786793967, 0.001912008033049058696 ),
 ( 0.000000000000000000, 1.000000000000000000 ),
 .UNSPECIFIED. ) 
 GEOMETRIC_REPRESENTATION_ITEM ( )  RATIONAL_B_SPLINE_SURFACE ( (
 ( 1.000000000000000000, 0.4915962107220576138, 1.000000000000000000),
 ( 1.000000000000000000, 0.4903111309377842786, 1.000000000000000000),
 ( 1.000000000000000000, 0.5057854813392340665, 1.000000000000000000),
 ( 1.000000000000000000, 0.5532305778937406382, 1.000000000000000000),
 ( 1.000000000000000000, 0.5846576190772416748, 1.000000000000000000),
 ( 1.000000000000000000, 0.6796638612371262989, 1.000000000000000000),
 ( 1.000000000000000000, 0.7435379557940102746, 1.000000000000000000),
 ( 1.000000000000000000, 0.8106661767825046327, 1.000000000000000000),
 ( 1.000000000000000000, 0.8285023559304793839, 1.000000000000000000),
 ( 1.000000000000000000, 0.8541358093762889681, 1.000000000000000000),
 ( 1.000000000000000000, 0.8615977546921151919, 1.000000000000000000),
 ( 1.000000000000000000, 0.8740883989870674720, 1.000000000000000000),
 ( 1.000000000000000000, 0.8700938199806586004, 1.000000000000000000),
 ( 1.000000000000000000, 0.8708456909032173954, 1.000000000000000000) ) ) 
 REPRESENTATION_ITEM ( '' )  SURFACE ( )  );
#13336 = ORIENTED_EDGE ( 'NONE', *, *, #133615, .T. ) ;
#13337 = CARTESIAN_POINT ( 'NONE',  ( 3.894935592111925526, 0.2864876570476772022, 1.948460325470881660 ) ) ;
#13338 = ORIENTED_EDGE ( 'NONE', *, *, #108573, .F. ) ;
#13339 = CARTESIAN_POINT ( 'NONE',  ( 6.497608386930124880, -1.941524946301041554, 0.05238333795444527485 ) ) ;
#13340 = ORIENTED_EDGE ( 'NONE', *, *, #3077, .F. ) ;
#13341 = CARTESIAN_POINT ( 'NONE',  ( -5.399890319992785237, 9.521898816625391504, 0.7998128361456291469 ) ) ;
#13343 = CARTESIAN_POINT ( 'NONE',  ( 4.922192346260840345, -2.110166376318895587, 0.2103620946037400852 ) ) ;
#13342 = CARTESIAN_POINT ( 'NONE',  ( 6.638652492546827766, 7.774124658506663010, 1.199719254218452047 ) ) ;
#13344 = CARTESIAN_POINT ( 'NONE',  ( 7.810905894804431426, 8.285347430126213553, 0.000000000000000000 ) ) ;
#13345 = CARTESIAN_POINT ( 'NONE',  ( 3.352119889487484183, 0.8575151890419380196, -1.709291564166728783 ) ) ;
#13346 = CARTESIAN_POINT ( 'NONE',  ( 4.800107077129743161, 6.969409711611327829, -1.408023891483715317 ) ) ;
#13347 = CARTESIAN_POINT ( 'NONE',  ( -9.500385102287568273, -7.162053774861992572, 0.01083140255525295165 ) ) ;
#13348 = ORIENTED_EDGE ( 'NONE', *, *, #46280, .F. ) ;
#13349 = CARTESIAN_POINT ( 'NONE',  ( 3.067887898442204442, 6.801229324816399746, 0.7998128361456271485 ) ) ;
#13350 = CARTESIAN_POINT ( 'NONE',  ( 5.092444288794719220, -1.116435683446183713, 1.674956235503543889 ) ) ;
#13351 = CARTESIAN_POINT ( 'NONE',  ( -4.495875322732098667, 7.242909153342021789, -1.312876762094741245 ) ) ;
#13352 = CARTESIAN_POINT ( 'NONE',  ( 6.621730190220365131, -1.769489810573118049, 0.4491385735008179836 ) ) ;
#13353 = CARTESIAN_POINT ( 'NONE',  ( 0.6431357727456864515, -0.2518013131528433757, -2.054909676291870380 ) ) ;
#13354 = CARTESIAN_POINT ( 'NONE',  ( -7.375272376154081932, 10.58793962461302485, -1.082531754730543971 ) ) ;
#13355 = CIRCLE ( 'NONE', #47879, 2.021340551328831392 ) ;
#13356 = CARTESIAN_POINT ( 'NONE',  ( -6.146561906247310247, 6.992958819738270826, -0.9370148970899976337 ) ) ;
#13357 = CARTESIAN_POINT ( 'NONE',  ( 11.41176686791169104, 11.25950803486853502, -3.404018756831829418 ) ) ;
#13358 = CARTESIAN_POINT ( 'NONE',  ( 3.285556943749998737, -3.055208332855376518, -1.896917185911906722 ) ) ;
#13359 = CARTESIAN_POINT ( 'NONE',  ( 6.856673000209174695, 9.022537805042615489, 1.599625672291281386 ) ) ;
#13360 = DIRECTION ( 'NONE',  ( 0.000000000000000000, 0.000000000000000000, -1.000000000000000000 ) ) ;
#13361 = EDGE_CURVE ( 'NONE', #178392, #132967, #145557, .T. ) ;
#13362 = CARTESIAN_POINT ( 'NONE',  ( 1.364683531249996529, 10.52604166700806765, 0.7879004041258405033 ) ) ;
#13363 = CARTESIAN_POINT ( 'NONE',  ( -4.141125853970233806, 6.918731698685530063, -1.199719254218452047 ) ) ;
#13365 = CARTESIAN_POINT ( 'NONE',  ( -7.553827861469316396, 8.841829255582865699, -1.199719254218452047 ) ) ;
#13364 = CARTESIAN_POINT ( 'NONE',  ( -11.94105722165071093, 11.02582762082958467, -1.187919369849417484 ) ) ;
#13366 = CARTESIAN_POINT ( 'NONE',  ( 3.304998880318401167, 1.097559245703746855, -1.342624595404175780 ) ) ;
#13367 = CARTESIAN_POINT ( 'NONE',  ( -4.283486466913726254, 7.084819080452935403, -1.199719254218452047 ) ) ;
#13368 = CARTESIAN_POINT ( 'NONE',  ( 1.217730340897508645, 0.4076058164220326407, -2.029561569317724690 ) ) ;
#13369 = CARTESIAN_POINT ( 'NONE',  ( 2.267339977356534142, 1.934377090824404455, -0.8611398932509596316 ) ) ;
#13370 = CARTESIAN_POINT ( 'NONE',  ( 7.588813295347141441, 9.876701482703580837, -1.599625672291262513 ) ) ;
#13371 = CARTESIAN_POINT ( 'NONE',  ( -5.467155955761412223, 6.078795959345912436, -0.9674530110256196469 ) ) ;
#13372 = CARTESIAN_POINT ( 'NONE',  ( 1.094512790084944287, 1.939365640515663181, 0.3419967617025142514 ) ) ;
#13373 = CARTESIAN_POINT ( 'NONE',  ( 4.401803827585060169, 7.348580664174646060, 1.190671039528957253 ) ) ;
#13374 = CARTESIAN_POINT ( 'NONE',  ( 4.026408433578586354, 7.641300905909586660, 1.040834085586084257E-14 ) ) ;
#13376 = DIRECTION ( 'NONE',  ( 0.000000000000000000, 0.000000000000000000, -1.000000000000000000 ) ) ;
#13375 = CARTESIAN_POINT ( 'NONE',  ( 0.000000000000000000, -3.237499999999997602, -4.012584370867899430 ) ) ;
#13377 = CARTESIAN_POINT ( 'NONE',  ( 2.695625570186571895, -0.7177931702126126856, 2.177047689787997342 ) ) ;
#13378 = CARTESIAN_POINT ( 'NONE',  ( 0.5920835508136900183, -1.811502216344462735, -0.2265648652611390590 ) ) ;
#13379 = CARTESIAN_POINT ( 'NONE',  ( 3.638835171272115421, 1.817485770107383436, 0.5952672491930725007 ) ) ;
#13380 = CARTESIAN_POINT ( 'NONE',  ( 6.879836604291781121, 6.991173891287354003, -0.7998128361456341429 ) ) ;
#13381 = CARTESIAN_POINT ( 'NONE',  ( 6.385527161912102123, 9.433236874664039817, -1.082531754730537976 ) ) ;
#13382 = CARTESIAN_POINT ( 'NONE',  ( 1.459241111239812705, -1.698469834904120290, 1.080578982646386743 ) ) ;
#13383 = CARTESIAN_POINT ( 'NONE',  ( 2.658977320520792276, 1.578554556127611308, -1.164590279592196298 ) ) ;
#13384 = CARTESIAN_POINT ( 'NONE',  ( -9.053093885623068715, 11.58502883802551153, -1.599625672291263179 ) ) ;
#13385 = CARTESIAN_POINT ( 'NONE',  ( -7.874588291438845644, 8.081441182967111558, -0.7998128361456291469 ) ) ;
#13386 = CARTESIAN_POINT ( 'NONE',  ( -11.07629303812015564, 5.828651784584821804, 4.512940454653985967 ) ) ;
#13388 = CARTESIAN_POINT ( 'NONE',  ( 3.942089010115860326, 1.761346036062165332, 0.1732582469678861092 ) ) ;
#13387 = CARTESIAN_POINT ( 'NONE',  ( 4.945306066807232170, 0.6564501001628511023, -1.984974157428524899 ) ) ;
#13389 = CARTESIAN_POINT ( 'NONE',  ( -9.898321827460007327, 14.00000000000624034, 7.924999999990797406 ) ) ;
#13390 = CARTESIAN_POINT ( 'NONE',  ( 6.456980045808101032, 0.3985590825250818203, -2.257207781175464056 ) ) ;
#13391 = CARTESIAN_POINT ( 'NONE',  ( 4.083748955185668272, -1.721791984697383482, -0.2523947965055831633 ) ) ;
#13392 = CARTESIAN_POINT ( 'NONE',  ( 7.703003830858588863, 12.13858823597705872, -0.7998128361456291469 ) ) ;
#13393 = TOROIDAL_SURFACE ( 'NONE', #155201, 0.8300000000000010703, 0.08000000000000000167 ) ;
#13394 = CARTESIAN_POINT ( 'NONE',  ( -7.662794434365309826, -5.790678129197943669, 7.045261094876549279 ) ) ;
#13395 = CARTESIAN_POINT ( 'NONE',  ( 4.938689436542594180, 0.9992198110298566860, 1.416717458774526373 ) ) ;
#13396 = CARTESIAN_POINT ( 'NONE',  ( 4.650930581473819991, -0.4712930505080668575, -2.119270573956061554 ) ) ;
#13397 = CARTESIAN_POINT ( 'NONE',  ( 3.440018289565364817, 5.036440642624797626, 1.599625672291267398 ) ) ;
#13398 = CARTESIAN_POINT ( 'NONE',  ( 5.946499988598237252, -1.422611626450220434, 1.429444749906971790 ) ) ;
#13399 = CARTESIAN_POINT ( 'NONE',  ( 5.031250000000002665, -0.7852924748302606561, -1.895863743163967108 ) ) ;
#13400 = CARTESIAN_POINT ( 'NONE',  ( -1.201851678989727383E-14, 5.118750000682815937, -1.732050807568863648 ) ) ;
#13401 = CARTESIAN_POINT ( 'NONE',  ( 2.854421793556624731, 0.6472853923233500284, 1.814523859438036624 ) ) ;
#13402 = CARTESIAN_POINT ( 'NONE',  ( 1.499999999999993117, 9.885416667349465669, 0.8660254037844409281 ) ) ;
#13403 = CARTESIAN_POINT ( 'NONE',  ( 0.08310686162707729696, -1.445780664108237801, 1.686489957186103839 ) ) ;
#13404 = ORIENTED_EDGE ( 'NONE', *, *, #158984, .F. ) ;
#13405 = CARTESIAN_POINT ( 'NONE',  ( 6.983263157960370116, 1.266851337794393961, 2.060309365732877485 ) ) ;
#13406 = CARTESIAN_POINT ( 'NONE',  ( -1.500000000000013101, 2.420833333333359150, 0.8660254037844403729 ) ) ;
#13407 = CARTESIAN_POINT ( 'NONE',  ( 4.476163270806094552, 8.373940915915776273, 0.7998128361456462443 ) ) ;
#13408 = CARTESIAN_POINT ( 'NONE',  ( 3.000855645084123946, -2.188801376007823762, -0.3777086580352209122 ) ) ;
#13409 = CARTESIAN_POINT ( 'NONE',  ( 6.408651779211167465, 0.6141799454031526828, 1.863335524608072502 ) ) ;
#13410 = CARTESIAN_POINT ( 'NONE',  ( 7.456621297836072415, 9.722477485607340597, 1.443375672974076540 ) ) ;
#13411 = CIRCLE ( 'NONE', #82676, 0.07999999999999971023 ) ;
#13412 = CARTESIAN_POINT ( 'NONE',  ( 0.7500000000000006661, 10.19791666734946922, -1.299038105676657340 ) ) ;
#13413 = CARTESIAN_POINT ( 'NONE',  ( 5.415556014015861841, 5.282846535965431300, -0.7998128361456481317 ) ) ;
#13414 = CARTESIAN_POINT ( 'NONE',  ( 0.03578008775950020093, -1.617816776142148250, 1.203357013023528932 ) ) ;
#13416 = CARTESIAN_POINT ( 'NONE',  ( 5.353991443295786468, -0.7455691153513328562, 1.923382134945450295 ) ) ;
#13415 = CARTESIAN_POINT ( 'NONE',  ( 10.38962578677386084, 11.01565159419135043, 0.000000000000000000 ) ) ;
#13417 = CARTESIAN_POINT ( 'NONE',  ( 1.499999999999964695, 5.295833333333357373, -0.8660254037844461461 ) ) ;
#13418 = CARTESIAN_POINT ( 'NONE',  ( -3.765413976293358278, 5.416068943807445635, 1.599625672291267398 ) ) ;
#13419 = CARTESIAN_POINT ( 'NONE',  ( -1.500000000000011324, 5.410416667349489117, -0.8660254037844313801 ) ) ;
#13420 = CARTESIAN_POINT ( 'NONE',  ( 1.364683531249986537, 0.3635416670080869328, 0.7879004041258500513 ) ) ;
#13421 = CARTESIAN_POINT ( 'NONE',  ( 6.925078400183548588, 0.0006614011395407459748, 1.855452278108092656 ) ) ;
#13422 = CARTESIAN_POINT ( 'NONE',  ( 6.328739007766592373, 0.6541968508507016722, -1.606262126034884608 ) ) ;
#13423 = CARTESIAN_POINT ( 'NONE',  ( 5.548340067360077121, -1.366870494764490296, 1.077293122972399431 ) ) ;
#13424 = CARTESIAN_POINT ( 'NONE',  ( 5.007038802148489509, 4.735966778795008381, 0.7998128361456341429 ) ) ;
#13425 = CARTESIAN_POINT ( 'NONE',  ( 3.421668107411596882, -1.366637645153226055, -1.840301194555084230 ) ) ;
#13426 = CARTESIAN_POINT ( 'NONE',  ( -0.6823417656250212460, 5.613541667008087543, 1.181850606188767472 ) ) ;
#13427 = CARTESIAN_POINT ( 'NONE',  ( 1.622747808203903963, -1.734053015003593101, 0.6191010992530541213 ) ) ;
#13428 = CARTESIAN_POINT ( 'NONE',  ( 5.055452015064900273, 6.750733944905253914, 1.449865234212225351 ) ) ;
#13429 = CARTESIAN_POINT ( 'NONE',  ( -10.62763048033980517, 4.753116220844278317, -5.576244429778776102 ) ) ;
#13430 = CARTESIAN_POINT ( 'NONE',  ( 1.817148636465517164, -0.2269042555285011864, 1.811363274943120771 ) ) ;
#13431 = CARTESIAN_POINT ( 'NONE',  ( 3.147111449167848019, 0.9091449406319618287, 1.799922684605055556 ) ) ;
#13432 = CARTESIAN_POINT ( 'NONE',  ( 1.675987266036529588, -1.170314894790158933, 1.852603040092118070 ) ) ;
#13433 = CARTESIAN_POINT ( 'NONE',  ( 9.483953901554681210, 14.00935217397140953, -8.399901643884886582 ) ) ;
#13434 = CARTESIAN_POINT ( 'NONE',  ( 4.225680580359360228, -2.015911352056736661, 0.6092541954213681610 ) ) ;
#13435 = CARTESIAN_POINT ( 'NONE',  ( -8.064402442030170093, 8.302891025323665630, 0.7998128361456602331 ) ) ;
#13436 = CARTESIAN_POINT ( 'NONE',  ( 6.744795205365000434, 13.99925803066161478, 9.538580854856197888 ) ) ;
#13437 = CARTESIAN_POINT ( 'NONE',  ( 1.064989848632340363, 1.568927673159369762, -1.351003706900590018 ) ) ;
#13438 = CARTESIAN_POINT ( 'NONE',  ( 4.157546660884947620, 8.002221537674429896, 1.040834085586084257E-14 ) ) ;
#13439 = CARTESIAN_POINT ( 'NONE',  ( -1.360316468750028651, -0.5781249996585913209, -4.510281037539698445E-14 ) ) ;
#13441 = B_SPLINE_CURVE_WITH_KNOTS ( 'NONE', 3,
 ( #76491, #176151, #111205, #106927 ),
 .UNSPECIFIED., .F., .F.,
 ( 4, 4 ),
 ( 0.001235641190896625326, 0.001582017824277171924 ),
 .UNSPECIFIED. ) ;
#13440 = CARTESIAN_POINT ( 'NONE',  ( 5.197945112634200449, 1.424400718755761908, 1.570990128125760554 ) ) ;
#13442 = CARTESIAN_POINT ( 'NONE',  ( 6.621730190220365131, -1.769489810573118049, 0.4491385735008179836 ) ) ;
#13443 = ORIENTED_EDGE ( 'NONE', *, *, #49082, .F. ) ;
#13444 = CARTESIAN_POINT ( 'NONE',  ( -4.633854640820660009, 8.628190524257904670, -0.7998128361456362523 ) ) ;
#13445 = CARTESIAN_POINT ( 'NONE',  ( 9.531545685607134999, 11.07889037375188401, 1.199719254218450271 ) ) ;
#13446 = CARTESIAN_POINT ( 'NONE',  ( 6.495764994278809823, 7.711385593814346073, 1.082531754730549967 ) ) ;
#13447 = CARTESIAN_POINT ( 'NONE',  ( 0.000000000000000000, -2.143749999044084031, -4.012584370867899430 ) ) ;
#13448 = AXIS2_PLACEMENT_3D ( 'NONE', #116369, #51314, #135772 ) ;
#13449 = CARTESIAN_POINT ( 'NONE',  ( -5.928993247877788697, 5.811580298812519807, 0.7998128361456341429 ) ) ;
#13450 = CARTESIAN_POINT ( 'NONE',  ( 6.222909436229170588, 1.570324008046734221, -1.425282903188800798 ) ) ;
#13451 = CARTESIAN_POINT ( 'NONE',  ( 1.342952632442768302, 0.4104956981533373628, 2.065382446648211801 ) ) ;
#13452 = CARTESIAN_POINT ( 'NONE',  ( -4.980641328173854632, 6.904110530993182948, 1.599625672291263179 ) ) ;
#13453 = CARTESIAN_POINT ( 'NONE',  ( 9.901532256681887745, 10.44620914241737530, 0.000000000000000000 ) ) ;
#13454 = CARTESIAN_POINT ( 'NONE',  ( 5.752756584690191133, -0.4505887142414471969, -1.805456089952769183 ) ) ;
#13455 = CARTESIAN_POINT ( 'NONE',  ( 8.483651433849084711, 10.92067931095586886, 1.599625672291281386 ) ) ;
#13456 = CARTESIAN_POINT ( 'NONE',  ( 4.081882008079450230, 3.980588341361369853, -0.7346435760097062007 ) ) ;
#13457 = CARTESIAN_POINT ( 'NONE',  ( -5.157951095356222204, 4.982307464195829816, 0.000000000000000000 ) ) ;
#13458 = CARTESIAN_POINT ( 'NONE',  ( -9.490344339885977476, 11.13478515369756217, -1.082531754730539753 ) ) ;
#13460 = CARTESIAN_POINT ( 'NONE',  ( 1.978885927095444863, 1.829411362569667743, 0.7090815385668995940 ) ) ;
#13459 = CARTESIAN_POINT ( 'NONE',  ( -6.449928391799210736, 8.548002428564306143, -1.599625672291263179 ) ) ;
#13461 = CARTESIAN_POINT ( 'NONE',  ( 0.8839147992780393981, 1.452536163361785260, 1.601146772000871188 ) ) ;
#13463 = CARTESIAN_POINT ( 'NONE',  ( -6.127725819454865608, 6.002332559294505820, -0.1884722350499398735 ) ) ;
#13462 = CARTESIAN_POINT ( 'NONE',  ( -6.608673532018475960, 6.674816973635147477, -0.7998128361456362523 ) ) ;
#13464 = CARTESIAN_POINT ( 'NONE',  ( -1.364683531250012516, 0.5302083336747518416, 0.7879004041258379498 ) ) ;
#13465 = CARTESIAN_POINT ( 'NONE',  ( 3.163173391212137808, -0.5009769021222918450, -1.659887746298273514 ) ) ;
#13466 = CARTESIAN_POINT ( 'NONE',  ( 2.185155941524752787, -0.7450687668543712894, 1.572906677108532936 ) ) ;
#13467 = CARTESIAN_POINT ( 'NONE',  ( 7.212574532790092974, 9.437756259720353924, -1.443375672974057666 ) ) ;
#13468 = CARTESIAN_POINT ( 'NONE',  ( -10.52284959769361805, 5.420271152154175986, 5.071911021504272199 ) ) ;
#13469 = CARTESIAN_POINT ( 'NONE',  ( 3.057942249777849675, 2.051182028257723999, -0.1983934154812707074 ) ) ;
#13470 = CARTESIAN_POINT ( 'NONE',  ( 1.177110994959302825, -0.9039684864705423983, -1.802142742073430171 ) ) ;
#13471 = CARTESIAN_POINT ( 'NONE',  ( 6.825078400183551608, 1.261667030487168439, 2.159888225955305163 ) ) ;
#13472 = CARTESIAN_POINT ( 'NONE',  ( -3.772911886352873445, 7.623757310712140800, 0.7998128361456352531 ) ) ;
#13473 = CARTESIAN_POINT ( 'NONE',  ( 1.041797052332312568, 0.8010751512182741063, -1.801556251716707413 ) ) ;
#13474 = EDGE_CURVE ( 'NONE', #153164, #85478, #13570, .T. ) ;
#13476 = CARTESIAN_POINT ( 'NONE',  ( -5.261973015879593873, 8.192700047617899273, 1.082531754730549967 ) ) ;
#13475 = CARTESIAN_POINT ( 'NONE',  ( 5.519756697582541172, -0.4584384640409416289, 1.856529252577573619 ) ) ;
#13477 = CARTESIAN_POINT ( 'NONE',  ( -6.251718229232856139, 8.387033582228697881, -1.443375672974066548 ) ) ;
#13478 = CARTESIAN_POINT ( 'NONE',  ( 6.984385409695311964, 8.177479728513226576, 1.199719254218452935 ) ) ;
#13479 = CARTESIAN_POINT ( 'NONE',  ( -5.271087860662956537, 9.371629280740593870, 0.000000000000000000 ) ) ;
#13480 = CARTESIAN_POINT ( 'NONE',  ( 0.7682301616282152246, 2.017272972751768645, -0.1012717401170943471 ) ) ;
#13481 = CARTESIAN_POINT ( 'NONE',  ( -1.250000000000001110, 8.500000000000000000, 3.469446951953614189E-15 ) ) ;
#13482 = CARTESIAN_POINT ( 'NONE',  ( 4.366487424706978260, 1.084006333436113634, 2.037121594781437839 ) ) ;
#13483 = CARTESIAN_POINT ( 'NONE',  ( 5.705508943770692731, -1.545575431542939970, -1.208212526538715137 ) ) ;
#13484 = CARTESIAN_POINT ( 'NONE',  ( 1.885527806591394961, -1.848987351811198998, 0.6559936482007987513 ) ) ;
#13485 = CARTESIAN_POINT ( 'NONE',  ( 9.585778300061798873, 11.14216175728232550, -1.199719254218440723 ) ) ;
#13486 = CARTESIAN_POINT ( 'NONE',  ( 0.0006249722829775038483, -1.976948959267275541, 0.3961041280396286890 ) ) ;
#13487 = ORIENTED_EDGE ( 'NONE', *, *, #16746, .T. ) ;
#13488 = CARTESIAN_POINT ( 'NONE',  ( 1.306030339497979531, -1.181222338749428280, -1.757047197724722620 ) ) ;
#13490 = CARTESIAN_POINT ( 'NONE',  ( -8.044065211609668253, 8.279164256499745633, 0.7998128361456602331 ) ) ;
#13489 = CARTESIAN_POINT ( 'NONE',  ( -3.262708522383007903, 6.958243709422141876, 1.040834085586084257E-14 ) ) ;
#13491 = CARTESIAN_POINT ( 'NONE',  ( 1.429379046243149931, 0.9088080074306194023, -1.601118750654044964 ) ) ;
#13492 = EDGE_LOOP ( 'NONE', ( #27564, #4625 ) ) ;
#13493 = CARTESIAN_POINT ( 'NONE',  ( 4.381792451580825976, -2.079388800107518698, 0.6243644347086656499 ) ) ;
#13494 = CARTESIAN_POINT ( 'NONE',  ( 11.34491280883428033, 8.770310257811074095, 3.915374332514163669 ) ) ;
#13496 = ADVANCED_FACE ( 'NONE', ( #24422 ), #171764, .T. ) ;
#13495 = CARTESIAN_POINT ( 'NONE',  ( 3.287459871768631636, 0.04819156399121089784, -2.120204644799832394 ) ) ;
#13497 = CARTESIAN_POINT ( 'NONE',  ( -0.7500000000000215383, 3.722916667349487785, 1.299038105676671107 ) ) ;
#13498 = CARTESIAN_POINT ( 'NONE',  ( 7.404724451357931336, 11.79059562655963056, 0.7998128361456462443 ) ) ;
#13500 = CARTESIAN_POINT ( 'NONE',  ( 0.000000000000000000, 4.000000000000003553, 0.000000000000000000 ) ) ;
#13499 = B_SPLINE_CURVE_WITH_KNOTS ( 'NONE', 3,
 ( #71285, #50795, #4147, #149365 ),
 .UNSPECIFIED., .F., .F.,
 ( 4, 4 ),
 ( 0.0004304244924211256284, 0.0006956056399114353287 ),
 .UNSPECIFIED. ) ;
#13501 = ORIENTED_EDGE ( 'NONE', *, *, #208272, .F. ) ;
#13502 = CARTESIAN_POINT ( 'NONE',  ( 3.304032624679804631, -2.058584765098357749, 0.09746896435120806779 ) ) ;
#13504 = CARTESIAN_POINT ( 'NONE',  ( 0.4152503475762688856, -0.9843521281015167324, -1.555853522519357934 ) ) ;
#13503 = CARTESIAN_POINT ( 'NONE',  ( -7.340850106795412167, 10.65174332698158643, 1.199719254218453823 ) ) ;
#13505 = CARTESIAN_POINT ( 'NONE',  ( 1.364683531249990311, 3.134375000341423245, 1.214306433183764966E-14 ) ) ;
#13506 = CARTESIAN_POINT ( 'NONE',  ( -1.347971487989957070E-14, -2.712500000000000355, 3.475000000000000089 ) ) ;
#13507 = CARTESIAN_POINT ( 'NONE',  ( 1.399654745096419406, 4.349328649162782057, 0.07090406488317976819 ) ) ;
#13508 = MECHANICAL_DESIGN_GEOMETRIC_PRESENTATION_REPRESENTATION (  '', ( #106962 ), #37630 ) ;
#13509 = CARTESIAN_POINT ( 'NONE',  ( 11.78331023100045627, 9.799999999999998934, -1.800000000000001155 ) ) ;
#13510 = CARTESIAN_POINT ( 'NONE',  ( 2.495744459589462227, 1.747532462024743882, 1.436835450399133407 ) ) ;
#13511 = CARTESIAN_POINT ( 'NONE',  ( -7.687109909268394325, 11.91211929421440097, 0.000000000000000000 ) ) ;
#13512 = CARTESIAN_POINT ( 'NONE',  ( 2.390610142633019741, -1.734584137932100312, -0.5226098844451251280 ) ) ;
#13513 = CARTESIAN_POINT ( 'NONE',  ( 1.991283197800724825, -0.4156388933829333610, 1.869923353789121556 ) ) ;
#13514 = CARTESIAN_POINT ( 'NONE',  ( 3.420434311836465291, 0.9283866757503267397, 1.850595421526677775 ) ) ;
#13515 = CARTESIAN_POINT ( 'NONE',  ( -1.201851678989727383E-14, 1.634375000341421025, 1.575800808251672791 ) ) ;
#13516 = CARTESIAN_POINT ( 'NONE',  ( 1.621884544099384096, -1.093522035911981050, -1.640203223306810232 ) ) ;
#13517 = CARTESIAN_POINT ( 'NONE',  ( 6.129514107576198967, -1.813157573415961066, 0.6514091821806231586 ) ) ;
#13518 = CARTESIAN_POINT ( 'NONE',  ( 2.957714569337116295, 1.861795396119047208, -0.1817069356538636715 ) ) ;
#13520 = CARTESIAN_POINT ( 'NONE',  ( 4.650542599771462449, 8.421518672640367242, 0.4769741307986720136 ) ) ;
#13519 = CARTESIAN_POINT ( 'NONE',  ( 1.471738413253330879, 0.1659702479998256264, -2.301786031945464828 ) ) ;
#13521 = CARTESIAN_POINT ( 'NONE',  ( 2.470971460243949203, 1.660895280785526618, 0.8397924955986632023 ) ) ;
#13522 = CARTESIAN_POINT ( 'NONE',  ( -1.201851678989727383E-14, 3.571875000341422357, 1.575800808251672791 ) ) ;
#13523 = CARTESIAN_POINT ( 'NONE',  ( 5.143062936040889710, -0.2492579690161021710, -2.047486851065055458 ) ) ;
#13524 = AXIS2_PLACEMENT_3D ( 'NONE', #106642, #173755, #25332 ) ;
#13525 = CARTESIAN_POINT ( 'NONE',  ( -6.261168011412601153, 6.199117522936475666, 1.040834085586084257E-14 ) ) ;
#13526 = CARTESIAN_POINT ( 'NONE',  ( 7.935599982700328958, 8.152621489438862667, 0.7998128361456481317 ) ) ;
#13527 = CARTESIAN_POINT ( 'NONE',  ( -1.273728293839776926, 3.987841871246060155, 0.4850152072975402739 ) ) ;
#13528 = EDGE_CURVE ( 'NONE', #102754, #127955, #202955, .T. ) ;
#13529 = B_SPLINE_CURVE_WITH_KNOTS ( 'NONE', 3,
 ( #100607, #34536, #121218, #84357, #20412, #136327, #51873 ),
 .UNSPECIFIED., .F., .F.,
 ( 4, 3, 4 ),
 ( 0.0001135037245265573214, 0.001517139415464327252, 0.002007692284160955340 ),
 .UNSPECIFIED. ) ;
#13530 = CARTESIAN_POINT ( 'NONE',  ( 5.860410395878546730, 0.8502751990519905601, 1.926866089339970056 ) ) ;
#13531 = CARTESIAN_POINT ( 'NONE',  ( 0.6823417656249899377, 2.655208333674753618, 1.181850606188767472 ) ) ;
#13532 = CARTESIAN_POINT ( 'NONE',  ( 5.659502677682959337, 0.4278135246765999988, -2.118672983663777654 ) ) ;
#13533 = CARTESIAN_POINT ( 'NONE',  ( 0.01783989211246589379, -0.5346760324982450241, 1.947684760809722304 ) ) ;
#13534 = CARTESIAN_POINT ( 'NONE',  ( -0.6823417656250246877, -0.9489583329919115684, 1.181850606188755259 ) ) ;
#13535 = CARTESIAN_POINT ( 'NONE',  ( -4.433153041988574294, 8.115836282387899558, 1.040834085586084257E-14 ) ) ;
#13538 = CARTESIAN_POINT ( 'NONE',  ( 5.531363484695522637, 5.555604941673978558, -0.7216878364870207285 ) ) ;
#13537 = CARTESIAN_POINT ( 'NONE',  ( 6.925078400183575233, 4.701279733332940580, 2.318349140213359583 ) ) ;
#13536 = CARTESIAN_POINT ( 'NONE',  ( 5.580062740476173566, 8.667767742934335828, 1.199719254218451159 ) ) ;
#13539 = CARTESIAN_POINT ( 'NONE',  ( -4.132202957115018727, 8.042930226601317401, 0.000000000000000000 ) ) ;
#13540 = CARTESIAN_POINT ( 'NONE',  ( 4.241422899474024177, 0.4370803545316758743, -1.968444674787086512 ) ) ;
#13541 = CARTESIAN_POINT ( 'NONE',  ( -6.530223543276495235, 10.77034456713125188, -0.7998128361456291469 ) ) ;
#13543 = CARTESIAN_POINT ( 'NONE',  ( -6.739811759324831897, 7.996106819701333634, -1.082531754730549967 ) ) ;
#13542 = CARTESIAN_POINT ( 'NONE',  ( -8.622622508611375025, 12.04318144581317895, 1.082531754730560403 ) ) ;
#13545 = CARTESIAN_POINT ( 'NONE',  ( -0.6823417656250003738, 9.901041667008065872, 1.181850606188754593 ) ) ;
#13544 = CARTESIAN_POINT ( 'NONE',  ( 5.963787895669664607, 2.130530397400759668, -0.3648857593604309391 ) ) ;
#13546 = CARTESIAN_POINT ( 'NONE',  ( -11.51196935752114392, 6.864815107568656316, 3.393625645527715395 ) ) ;
#13548 = CARTESIAN_POINT ( 'NONE',  ( 0.1928052069046156669, 1.667086954950956157, 0.9433992581227236274 ) ) ;
#13547 = CARTESIAN_POINT ( 'NONE',  ( -5.368665640887164692, 9.207267647769599606, 0.000000000000000000 ) ) ;
#13549 = CARTESIAN_POINT ( 'NONE',  ( -1.402160292154681736E-14, -0.7406249996585823059, -1.575800808251665908 ) ) ;
#13550 = CARTESIAN_POINT ( 'NONE',  ( 2.314726122855132129, 1.540323329518531903, 0.7764098835694576151 ) ) ;
#13551 = CARTESIAN_POINT ( 'NONE',  ( 6.073126464278658432, 6.050012061272033392, 0.000000000000000000 ) ) ;
#13553 = CARTESIAN_POINT ( 'NONE',  ( 4.830447868218803897, 8.857549289555754157, -0.7998128361456481317 ) ) ;
#13552 = CARTESIAN_POINT ( 'NONE',  ( 8.134528978519385944, 8.592631351135175066, -0.7216878364870267237 ) ) ;
#13554 = CIRCLE ( 'NONE', #6727, 12.00000000000000178 ) ;
#13555 = CARTESIAN_POINT ( 'NONE',  ( -10.81298704238391650, 6.434023936693727741, -5.221020569155840008 ) ) ;
#13556 = CARTESIAN_POINT ( 'NONE',  ( 6.555916519444559221, 1.865492442988415656, -0.1378669075578625169 ) ) ;
#13557 = CARTESIAN_POINT ( 'NONE',  ( 1.119790083981372142, -0.4868965817936173335, 1.953217858147300090 ) ) ;
#13558 = CARTESIAN_POINT ( 'NONE',  ( -4.791166081694341550, 4.882818525799564213, 0.4357780244859492669 ) ) ;
#13559 = CARTESIAN_POINT ( 'NONE',  ( 3.223846859376262142, -2.127229092858519799, 0.5869343725257711863 ) ) ;
#13560 = CARTESIAN_POINT ( 'NONE',  ( 5.313404054176891655, -1.830285002536722549, -1.167499077736388724 ) ) ;
#13561 = EDGE_LOOP ( 'NONE', ( #211456, #181237 ) ) ;
#13562 = CARTESIAN_POINT ( 'NONE',  ( 3.923105346307896202, 5.670318552149568703, -1.599625672291269396 ) ) ;
#13563 = CARTESIAN_POINT ( 'NONE',  ( 10.18181017373857600, 10.98112607889092907, 0.7216878364870438212 ) ) ;
#13565 = CARTESIAN_POINT ( 'NONE',  ( 2.109000121467627498, 0.002830143620808495131, 2.016598147190066914 ) ) ;
#13564 = CARTESIAN_POINT ( 'NONE',  ( 3.071057173463411338, -1.604308532545582366, 1.386676294644908713 ) ) ;
#13567 = ORIENTED_EDGE ( 'NONE', *, *, #109130, .T. ) ;
#13566 = CARTESIAN_POINT ( 'NONE',  ( 1.757782220650351723, 0.6909716962627761028, -1.674832866754811578 ) ) ;
#13568 = CARTESIAN_POINT ( 'NONE',  ( 7.361151057576892143, 7.552707420120024828, 0.7998128361456291469 ) ) ;
#13569 = ORIENTED_EDGE ( 'NONE', *, *, #183782, .F. ) ;
#13570 = CIRCLE ( 'NONE', #169119, 9.999999999999998224 ) ;
#13571 = CARTESIAN_POINT ( 'NONE',  ( 4.611744806942754238, 8.532119374741881757, -0.7998128361456231517 ) ) ;
#13573 = CARTESIAN_POINT ( 'NONE',  ( 0.8662487887013297083, -1.869732701101217476, -0.4164899194021577933 ) ) ;
#13572 = CARTESIAN_POINT ( 'NONE',  ( -3.391510981712833939, 7.108513245306943062, 0.7998128361456341429 ) ) ;
#13574 = CARTESIAN_POINT ( 'NONE',  ( -2.609770642201835855, 0.3830433331901555993, -0.1872689674646474400 ) ) ;
#13575 = CARTESIAN_POINT ( 'NONE',  ( 0.4499999999999747535, 3.949999999999988187, 0.4999999999999674705 ) ) ;
#13576 = CARTESIAN_POINT ( 'NONE',  ( 5.870317324592803310, 7.871789516823500144, -1.443375672974057666 ) ) ;
#13577 = CARTESIAN_POINT ( 'NONE',  ( -0.6823417656250246877, 0.6135416670080897639, 1.181850606188755259 ) ) ;
#13578 = CARTESIAN_POINT ( 'NONE',  ( -2.952042078427798533, 6.300591463180486684, -0.5728661040586968678 ) ) ;
#13579 = CARTESIAN_POINT ( 'NONE',  ( -10.13202086811422475, 10.71511252242175161, -0.7998128361456291469 ) ) ;
#13580 = CARTESIAN_POINT ( 'NONE',  ( 5.454052192070484750, 2.159419290912270029, -0.1019294599445344923 ) ) ;
#13581 = CARTESIAN_POINT ( 'NONE',  ( -4.001064729808656573, 7.682009594836471500, 1.214306433183764966E-14 ) ) ;
#13582 = CARTESIAN_POINT ( 'NONE',  ( 3.770576118376296471, 7.413106214832098750, 0.7216878364870257245 ) ) ;
#13583 = CARTESIAN_POINT ( 'NONE',  ( 3.533539421053990104, -0.1523460092780377639, 2.115156586662121363 ) ) ;
#13585 = CARTESIAN_POINT ( 'NONE',  ( -12.26673246283585961, 6.254089313302478637, -3.851195297204758727 ) ) ;
#13584 = CYLINDRICAL_SURFACE ( 'NONE', #200530, 9.499999999999992895 ) ;
#13586 = CARTESIAN_POINT ( 'NONE',  ( 3.075414692445295195, 1.873101151500027317, -0.6148835396118810248 ) ) ;
#13587 = EDGE_LOOP ( 'NONE', ( #51154, #55833, #99286, #12803 ) ) ;
#13588 = PLANE ( 'NONE',  #42477 ) ;
#13589 = CARTESIAN_POINT ( 'NONE',  ( 0.3618904354094238385, -0.5536326762660361833, 1.994880328902041589 ) ) ;
#13590 = CARTESIAN_POINT ( 'NONE',  ( 2.624863168539525393, -1.811862388431908721, 0.6992392096202125762 ) ) ;
#13591 = EDGE_LOOP ( 'NONE', ( #18635, #112933, #190831, #148500, #160653, #41297, #114528 ) ) ;
#13592 = FACE_OUTER_BOUND ( 'NONE', #80481, .T. ) ;
#13594 = CARTESIAN_POINT ( 'NONE',  ( 5.989670002187236442, 10.20997511251894529, -0.7998128361456481317 ) ) ;
#13593 = CARTESIAN_POINT ( 'NONE',  ( -6.211043768836215229, 8.339580045099285854, 1.443375672974064550 ) ) ;
#13596 = CARTESIAN_POINT ( 'NONE',  ( 4.957477724091233995, 8.935474444748447098, -0.7998128361456281477 ) ) ;
#13595 = CARTESIAN_POINT ( 'NONE',  ( 2.765665077289869433, 1.118955468730401526, 1.765788254259098800 ) ) ;
#13597 = CARTESIAN_POINT ( 'NONE',  ( 5.370438244344566847, 5.438135171256338829, 0.000000000000000000 ) ) ;
#13599 = VERTEX_POINT ( 'NONE', #72105 ) ;
#13598 = CARTESIAN_POINT ( 'NONE',  ( 6.235011639695052565, 1.786057601157979180, 0.6837302122261402770 ) ) ;
#13600 = CARTESIAN_POINT ( 'NONE',  ( 3.914836437932368796, 1.561248537261412883, -1.560010120355350693 ) ) ;
#13601 = COLOUR_RGB ( '', 0.09019608, 0.27058824, 0.51372549) ;
#13602 = CARTESIAN_POINT ( 'NONE',  ( 3.048105859194950362, 0.7956334958073747465, -2.058523145315640956 ) ) ;
#13603 = CARTESIAN_POINT ( 'NONE',  ( -11.91292854676714974, 12.48518470326975205, 1.446370920797324100 ) ) ;
#13604 = CARTESIAN_POINT ( 'NONE',  ( 2.227084300891319035, 1.708885092217244051, 0.8583199515034345417 ) ) ;
#13605 = CARTESIAN_POINT ( 'NONE',  ( 10.55910270694468345, 11.21337466772398095, 0.7998128361456462443 ) ) ;
#13606 = CARTESIAN_POINT ( 'NONE',  ( 3.895033709675084221, 0.3008086390649654662, 2.048262060622765279 ) ) ;
#13608 = CARTESIAN_POINT ( 'NONE',  ( 3.186554565756247737, -2.129457467500107004, -0.3711038070777841202 ) ) ;
#13607 = CARTESIAN_POINT ( 'NONE',  ( -3.789667630219657912, 4.380032642466370696, 1.199719254218462483 ) ) ;
#13609 = CARTESIAN_POINT ( 'NONE',  ( 5.144143540903125533, 0.6357783856077160456, 2.097287126430439130 ) ) ;
#13610 =( GEOMETRIC_REPRESENTATION_CONTEXT ( 3 ) GLOBAL_UNCERTAINTY_ASSIGNED_CONTEXT ( ( #36331 ) ) GLOBAL_UNIT_ASSIGNED_CONTEXT ( ( #9616, #189440, #72474 ) ) REPRESENTATION_CONTEXT ( 'NONE', 'WORKASPACE' ) );
#13611 = FACE_OUTER_BOUND ( 'NONE', #35884, .T. ) ;
#13612 = CARTESIAN_POINT ( 'NONE',  ( -0.4659925305415743568, -6.893137084989842123, -10.91005274787796786 ) ) ;
#13613 = CARTESIAN_POINT ( 'NONE',  ( -0.1598595594940371567, 7.033953395470809333, 1.994736385849470883 ) ) ;
#13614 = EDGE_CURVE ( 'NONE', #72492, #401, #96438, .T. ) ;
#13615 = CARTESIAN_POINT ( 'NONE',  ( 4.213551878797002992, 8.137837301896977849, 0.000000000000000000 ) ) ;
#13616 = CARTESIAN_POINT ( 'NONE',  ( -1.402160292154681736E-14, 15.23437500034140157, 1.575800808251682339 ) ) ;
#13617 = CARTESIAN_POINT ( 'NONE',  ( -3.142457743317409680, 6.888227477170756785, 0.7998128361456352531 ) ) ;
#13618 = CARTESIAN_POINT ( 'NONE',  ( -0.05211191391743182078, -1.802403943428915412, -0.9041556775107384425 ) ) ;
#13619 = CARTESIAN_POINT ( 'NONE',  ( -9.056483424248693126, 10.62861408545402675, 1.082531754730558626 ) ) ;
#13620 = CARTESIAN_POINT ( 'NONE',  ( 5.190316231837919680, 1.068962568377257671, -1.772817291931286787 ) ) ;
#13621 = CARTESIAN_POINT ( 'NONE',  ( 2.789578772358902281, 1.362584191422511415, 1.362147869459982230 ) ) ;
#13622 = CARTESIAN_POINT ( 'NONE',  ( 5.431313658478175377, -1.669672585088026517, -1.301796502452344129 ) ) ;
#13623 = CARTESIAN_POINT ( 'NONE',  ( 4.449046963578762615, 8.342305224150557308, -0.7998128361456231517 ) ) ;
#13624 = FACE_OUTER_BOUND ( 'NONE', #48632, .T. ) ;
#13625 = CARTESIAN_POINT ( 'NONE',  ( 4.241030189111538284, -0.1885853823969813603, -1.960358720193545068 ) ) ;
#13626 = CARTESIAN_POINT ( 'NONE',  ( 6.316396932256916230, 2.136508426756661638, 0.8310160958180726753 ) ) ;
#13627 = CARTESIAN_POINT ( 'NONE',  ( 3.721172816245840842, -0.1328194893376876962, 1.820914920514608459 ) ) ;
#13628 = CARTESIAN_POINT ( 'NONE',  ( 7.187230829020129441, 8.518095734345896730, 1.082531754730549967 ) ) ;
#13629 = CARTESIAN_POINT ( 'NONE',  ( 4.975479186090852046, 6.827811688571220117, 1.443375672974062551 ) ) ;
#13630 = CARTESIAN_POINT ( 'NONE',  ( -6.257970421159510188, 9.458660037064859694, 1.199719254218452047 ) ) ;
#13631 = CARTESIAN_POINT ( 'NONE',  ( 6.852720297064418986, 6.959538199522133262, 0.7998128361456331437 ) ) ;
#13632 = EDGE_LOOP ( 'NONE', ( #203770, #51156, #134911, #86054 ) ) ;
#13634 = CARTESIAN_POINT ( 'NONE',  ( 5.080342566386993219, 0.9961330521413218619, 1.749448578721881198 ) ) ;
#13633 = CARTESIAN_POINT ( 'NONE',  ( 1.171164436615620863, 1.096940724416964885, 1.478650282607060662 ) ) ;
#13635 = CARTESIAN_POINT ( 'NONE',  ( 5.836663081169705336, 0.6703748249779170054, -2.198801845021758350 ) ) ;
#13636 = CARTESIAN_POINT ( 'NONE',  ( 5.735196368693616265, -0.04450293679344322767, -1.961403813732150780 ) ) ;
#13637 = CARTESIAN_POINT ( 'NONE',  ( -5.520141099058386125, 9.591915048876776595, 0.000000000000000000 ) ) ;
#13638 = CARTESIAN_POINT ( 'NONE',  ( -3.262708522383007903, 6.958243709422141876, 1.040834085586084257E-14 ) ) ;
#13639 = LINE ( 'NONE', #130678, #154252 ) ;
#13640 = CARTESIAN_POINT ( 'NONE',  ( -6.283277845290492714, 6.295188672452495915, -0.7998128361456362523 ) ) ;
#13642 = CARTESIAN_POINT ( 'NONE',  ( 6.754783849477350444, -1.364574176550734208, 1.126888093558385817 ) ) ;
#13641 = CARTESIAN_POINT ( 'NONE',  ( 1.786781105396139102, 1.817558579408204089, -1.033184933219722934 ) ) ;
#13643 = CARTESIAN_POINT ( 'NONE',  ( -7.836475020641954004, -5.360178282914185743, 7.719547554928810840 ) ) ;
#13644 = CARTESIAN_POINT ( 'NONE',  ( -0.1106727585415837045, 2.018984206239351042, -2.418200238751634146 ) ) ;
#13645 = CARTESIAN_POINT ( 'NONE',  ( 0.4854153416827499679, -1.726952712381021326, -0.2154422717644439433 ) ) ;
#13646 = CARTESIAN_POINT ( 'NONE',  ( 6.419949431270806528, 7.448694743692793274, 1.199719254218462483 ) ) ;
#13648 = CARTESIAN_POINT ( 'NONE',  ( 1.530509776559449753, 8.694755902745800569, 2.517145264428167106 ) ) ;
#13647 = CARTESIAN_POINT ( 'NONE',  ( 0.002914018882855369096, 14.55305236535103397, 11.95586205439599681 ) ) ;
#13649 = CARTESIAN_POINT ( 'NONE',  ( 1.576317393346495344, -1.636983117988626946, -0.5438251031371076349 ) ) ;
#13650 = CARTESIAN_POINT ( 'NONE',  ( 1.874823134854076923, -0.1115055541827478930, -2.188858692977871279 ) ) ;
#13651 = CARTESIAN_POINT ( 'NONE',  ( 4.600333186373093852, -2.206333364838486411, -0.05604163552313382035 ) ) ;
#13652 = CARTESIAN_POINT ( 'NONE',  ( 6.116136693540529912, 10.14959355252369910, 1.530808498934192557E-16 ) ) ;
#13653 =( GEOMETRIC_REPRESENTATION_CONTEXT ( 3 ) GLOBAL_UNCERTAINTY_ASSIGNED_CONTEXT ( ( #115795 ) ) GLOBAL_UNIT_ASSIGNED_CONTEXT ( ( #164460, #179652, #78927 ) ) REPRESENTATION_CONTEXT ( 'NONE', 'WORKASPACE' ) );
#13654 = CARTESIAN_POINT ( 'NONE',  ( 1.024573611315128252, 1.068414711107899429, 1.889872971959544401 ) ) ;
#13655 = LINE ( 'NONE', #80805, #79084 ) ;
#13656 = CARTESIAN_POINT ( 'NONE',  ( 2.167340134605561630, 1.933669477944195636, -0.8630234182349978411 ) ) ;
#13657 = CARTESIAN_POINT ( 'NONE',  ( 6.539320575229251808, 2.472926584938171413, 2.181659282373017650 ) ) ;
#13658 = ADVANCED_FACE ( 'NONE', ( #26575 ), #54818, .F. ) ;
#13660 = CARTESIAN_POINT ( 'NONE',  ( 0.6823417656249882723, -0.2614583329919109578, -1.181850606188749264 ) ) ;
#13659 = CARTESIAN_POINT ( 'NONE',  ( 2.876852093609012950, -0.1713799144957695864, -2.286037302510893099 ) ) ;
#13661 = SURFACE_STYLE_USAGE ( .BOTH. , #213963 ) ;
#13662 = CARTESIAN_POINT ( 'NONE',  ( 5.867981556616276073, 5.740399992340775803, -0.7998128361456281477 ) ) ;
#13663 = CARTESIAN_POINT ( 'NONE',  ( 6.041669411999269990, -2.092492953876758044, 0.7457244993839227121 ) ) ;
#13664 = CARTESIAN_POINT ( 'NONE',  ( -5.734735788900501952, 9.634349487118505806, 0.000000000000000000 ) ) ;
#13665 = CARTESIAN_POINT ( 'NONE',  ( 5.504247177468186258, 6.484338464210099851, 1.082531754730558626 ) ) ;
#13666 = CARTESIAN_POINT ( 'NONE',  ( -6.358410854684783509, 9.401601182898824405, -1.082531754730537976 ) ) ;
#13667 = CARTESIAN_POINT ( 'NONE',  ( 3.933273961740296087, 6.642551151122080277, 1.082531754730549078 ) ) ;
#13668 = ORIENTED_EDGE ( 'NONE', *, *, #212293, .T. ) ;
#13669 = CARTESIAN_POINT ( 'NONE',  ( 3.568982563115063567, -0.9913999084223242830, 1.755768870528086056 ) ) ;
#13671 = CARTESIAN_POINT ( 'NONE',  ( 2.553648762129530958, 1.591643574212991297, 1.311770128662164137 ) ) ;
#13670 = CARTESIAN_POINT ( 'NONE',  ( 6.582647274634798151, 7.638508894284114170, 1.199719254218462483 ) ) ;
#13672 = DIRECTION ( 'NONE',  ( 0.000000000000000000, 0.000000000000000000, -1.000000000000000000 ) ) ;
#13673 = EDGE_CURVE ( 'NONE', #78850, #130236, #86084, .T. ) ;
#13674 = CARTESIAN_POINT ( 'NONE',  ( 5.573810548549551491, 6.635772073796838200, -1.082531754730548412 ) ) ;
#13675 = ORIENTED_EDGE ( 'NONE', *, *, #156704, .F. ) ;
#13676 = DIRECTION ( 'NONE',  ( 0.000000000000000000, 0.000000000000000000, 1.000000000000000000 ) ) ;
#13677 = CARTESIAN_POINT ( 'NONE',  ( 1.364683531249988535, 4.363541667008090208, 0.7879004041258500513 ) ) ;
#13678 = CARTESIAN_POINT ( 'NONE',  ( 5.455090197064776270, 0.4301712223657681022, -2.148646160378755443 ) ) ;
#13679 = CARTESIAN_POINT ( 'NONE',  ( 2.742814741689561853, 2.006446121045248887, -0.2004354718553730264 ) ) ;
#13680 = CARTESIAN_POINT ( 'NONE',  ( 2.419273308677453826, -1.061688697878185206, -1.504126257600538974 ) ) ;
#13681 = CARTESIAN_POINT ( 'NONE',  ( 7.609150525767641504, 9.900428251527500834, -1.599625672291262513 ) ) ;
#13682 = SHAPE_REPRESENTATION_RELATIONSHIP ( 'NONE' , 'NONE' ,  #137092, #176823 ) ;
#13683 = CARTESIAN_POINT ( 'NONE',  ( 5.561492448144861989, 0.3540975402388062965, -1.790731494587729067 ) ) ;
#13684 = CARTESIAN_POINT ( 'NONE',  ( 6.604150280000163242, -0.1430408514614608939, 1.983920101186954721 ) ) ;
#13685 = CARTESIAN_POINT ( 'NONE',  ( -8.148614017013223076, 9.465470093725620870, -1.199719254218446718 ) ) ;
#13687 = CARTESIAN_POINT ( 'NONE',  ( -5.010620288702242853, 8.003418215864698482, -1.199719254218453823 ) ) ;
#13686 = CARTESIAN_POINT ( 'NONE',  ( 5.682586732044571320, -2.206005490488979426, -0.5019008842952320526 ) ) ;
#13688 = CARTESIAN_POINT ( 'NONE',  ( 1.155059408868217119, -1.659095468083382041, 1.297160957089478206 ) ) ;
#13689 = CARTESIAN_POINT ( 'NONE',  ( -5.912237504011027767, 9.055304967058290799, 1.199719254218454489 ) ) ;
#13690 = CARTESIAN_POINT ( 'NONE',  ( 7.703003830858588863, 12.13858823597705872, -0.7998128361456291469 ) ) ;
#13691 = FACE_OUTER_BOUND ( 'NONE', #188013, .T. ) ;
#13692 = CARTESIAN_POINT ( 'NONE',  ( 8.378074386687000441, 31.50815134976859255, 15.76159487570644124 ) ) ;
#13693 = CARTESIAN_POINT ( 'NONE',  ( -7.121056995675673740, 9.330985799753529264, -1.599625672291263179 ) ) ;
#13694 = CARTESIAN_POINT ( 'NONE',  ( 0.4082588578520087719, 6.973322098160817717, 3.931096130881035489 ) ) ;
#13695 = CARTESIAN_POINT ( 'NONE',  ( 7.364013710877980401, 8.620379413226322285, -1.199719254218452047 ) ) ;
#13696 = CARTESIAN_POINT ( 'NONE',  ( 5.611280047485872835, 6.151892252731265387, -0.8436193503846599606 ) ) ;
#13697 = CARTESIAN_POINT ( 'NONE',  ( -8.337901282724359930, 12.67137589657970409, 1.040834085586084257E-14 ) ) ;
#13698 = CARTESIAN_POINT ( 'NONE',  ( 2.426306324659221136, -2.196553987802750907, 0.3307981192552343352 ) ) ;
#13699 = CARTESIAN_POINT ( 'NONE',  ( 3.284841267552055299, 6.405332120898776793, -0.9495590844852130896 ) ) ;
#13700 = CARTESIAN_POINT ( 'NONE',  ( -5.529746549527323474, 7.544733289238903851, -1.599625672291271394 ) ) ;
#13701 = PRODUCT_RELATED_PRODUCT_CATEGORY ( 'part', '', ( #93852 ) ) ;
#13702 = CARTESIAN_POINT ( 'NONE',  ( 6.311484202361478779, 7.322151976631905868, -1.199719254218446718 ) ) ;
#13703 = CARTESIAN_POINT ( 'NONE',  ( 3.508209890309890167, 1.962046631884439174, 0.002529298861464468473 ) ) ;
#13704 = CARTESIAN_POINT ( 'NONE',  ( 6.311484202361478779, 7.322151976631905868, -1.199719254218446718 ) ) ;
#13705 = CARTESIAN_POINT ( 'NONE',  ( -4.305726085941478765, 7.254707473775878768, 0.9719050602644065950 ) ) ;
#13706 = CARTESIAN_POINT ( 'NONE',  ( 4.359110081993588182, 5.044382169536003602, -1.199719254218452047 ) ) ;
#13707 = CARTESIAN_POINT ( 'NONE',  ( -3.987506576194992824, 7.666191748953863794, 0.7216878364870338292 ) ) ;
#13708 = CARTESIAN_POINT ( 'NONE',  ( -6.968527767744110868, 9.153035033833367251, 1.443375672974078761 ) ) ;
#13709 = CARTESIAN_POINT ( 'NONE',  ( 1.933984528066152953, -2.055706711753771287, 0.5200354980386610038 ) ) ;
#13710 = CARTESIAN_POINT ( 'NONE',  ( -5.795184315198522285, 5.725746220678519904, -0.7998128361456362523 ) ) ;
#13711 = CARTESIAN_POINT ( 'NONE',  ( 4.733375416736937069, -1.977748744329570263, 0.8730265686548792647 ) ) ;
#13712 = CARTESIAN_POINT ( 'NONE',  ( 2.770863647982471534, 1.747605724785822767, -0.5798694457997202178 ) ) ;
#13713 = CARTESIAN_POINT ( 'NONE',  ( -4.235850332497944848, 7.335353122692886529, 0.8760575672057471230 ) ) ;
#13714 = CARTESIAN_POINT ( 'NONE',  ( -1.364683531250012516, 0.5927083336747520637, 0.7879004041258379498 ) ) ;
#13715 = CARTESIAN_POINT ( 'NONE',  ( 5.437372246358883388, 0.6999822053482355200, -1.593550356025658976 ) ) ;
#13716 = CARTESIAN_POINT ( 'NONE',  ( 6.727182134110195832, 0.008744176509076214548, 1.710970312420513784 ) ) ;
#13717 = CARTESIAN_POINT ( 'NONE',  ( 3.212919216758630014, 6.692230152952963529, 0.000000000000000000 ) ) ;
#13718 = CARTESIAN_POINT ( 'NONE',  ( 6.720655732516645386, 0.002698097948191865297, 1.926293798961113080 ) ) ;
#13719 = CARTESIAN_POINT ( 'NONE',  ( 2.782270202741622178, -1.112240752214749273, 1.853481441253836071 ) ) ;
#13720 = COLOUR_RGB ( '', 0.09019608, 0.27058824, 0.51372549) ;
#13721 = CARTESIAN_POINT ( 'NONE',  ( 4.710314442360476583, -1.556670644073439913, -1.281164596596932936 ) ) ;
#13722 = CARTESIAN_POINT ( 'NONE',  ( -9.788623718942277563, 10.52240854829523187, 1.040834085586084257E-14 ) ) ;
#13723 = CARTESIAN_POINT ( 'NONE',  ( 2.465889518630470789, 2.120156730345585938, -0.4209195040108040797 ) ) ;
#13724 =( BOUNDED_SURFACE ( )  B_SPLINE_SURFACE ( 3, 3, ( 
 ( #107605, #126002, #141153, #138990, #191963, #171467, #27345, #92389, #190902, #6806, #173636 ),
 ( #25208, #157369, #56658, #207162, #43628, #42566, #40418, #39334, #159486, #8963, #142203 ),
 ( #75038, #23056, #93448, #122821, #109743, #72883, #58785, #143283, #187706, #156300, #10025 ),
 ( #124940, #174698, #175754, #77161, #209274, #172547, #105431, #140066, #60920, #90234, #7883 ),
 ( #73971, #48950, #147517, #63053, #15346, #161637, #213538, #81439, #65161, #194111, #176806 ),
 ( #112943, #177883, #64127, #111879, #29496, #13232, #95588, #28422, #128151, #129219, #145 ),
 ( #79305, #82489, #145421, #45761, #131317, #115068, #193040, #162704, #61995, #14276, #197309 ) ),
 .UNSPECIFIED., .T., .F., .T. ) 
 B_SPLINE_SURFACE_WITH_KNOTS ( ( 4, 3, 4 ),
 ( 4, 1, 1, 1, 1, 1, 1, 1, 4 ),
 ( 0.000000000000000000, 0.5000000000000000000, 1.000000000000000000 ),
 ( 0.000000000000000000, 0.2254704865597413344, 0.3973194950497592193, 0.5246576192285303808, 0.6166070239209043846, 0.6823180413592140336, 0.7309932997181896042, 0.7717238569598857678, 1.000000000000000000 ),
 .UNSPECIFIED. ) 
 GEOMETRIC_REPRESENTATION_ITEM ( )  RATIONAL_B_SPLINE_SURFACE ( (
 ( 1.000000000000000000, 1.000000000000000000, 1.000000000000000222, 0.9999999999999997780, 1.000000000000000444, 0.9999999999999996669, 1.000000000000000222, 1.000000000000000222, 1.000000000000000222, 1.000000000000000222, 1.000000000000000222),
 ( 0.3333333333333333703, 0.3333333333333334259, 0.3333333333333333703, 0.3333333333333333703, 0.3333333333333334814, 0.3333333333333332038, 0.3333333333333334814, 0.3333333333333334259, 0.3333333333333334259, 0.3333333333333334259, 0.3333333333333334259),
 ( 0.3333333333333333703, 0.3333333333333334259, 0.3333333333333333703, 0.3333333333333333703, 0.3333333333333334814, 0.3333333333333332038, 0.3333333333333334814, 0.3333333333333334259, 0.3333333333333334259, 0.3333333333333334259, 0.3333333333333334259),
 ( 1.000000000000000000, 1.000000000000000000, 1.000000000000000222, 0.9999999999999997780, 1.000000000000000444, 0.9999999999999996669, 1.000000000000000222, 1.000000000000000222, 1.000000000000000222, 1.000000000000000222, 1.000000000000000222),
 ( 0.3333333333333333703, 0.3333333333333334259, 0.3333333333333333703, 0.3333333333333333703, 0.3333333333333334814, 0.3333333333333332038, 0.3333333333333334814, 0.3333333333333334259, 0.3333333333333334259, 0.3333333333333334259, 0.3333333333333334259),
 ( 0.3333333333333333703, 0.3333333333333334259, 0.3333333333333333703, 0.3333333333333333703, 0.3333333333333334814, 0.3333333333333332038, 0.3333333333333334814, 0.3333333333333334259, 0.3333333333333334259, 0.3333333333333334259, 0.3333333333333334259),
 ( 1.000000000000000000, 1.000000000000000000, 1.000000000000000222, 0.9999999999999997780, 1.000000000000000444, 0.9999999999999996669, 1.000000000000000222, 1.000000000000000222, 1.000000000000000222, 1.000000000000000222, 1.000000000000000222) ) ) 
 REPRESENTATION_ITEM ( '' )  SURFACE ( )  );
#13725 = CARTESIAN_POINT ( 'NONE',  ( 2.512907010818050679, 1.759183109745281692, 0.8898679072262619671 ) ) ;
#13726 = CARTESIAN_POINT ( 'NONE',  ( -3.475000000000000533, -2.785416665710751527, -2.006292185433948827 ) ) ;
#13727 = CARTESIAN_POINT ( 'NONE',  ( 4.423342042002774477, -1.197376356234590933, -1.528922412636232631 ) ) ;
#13730 = ORIENTED_EDGE ( 'NONE', *, *, #88854, .F. ) ;
#13729 = CARTESIAN_POINT ( 'NONE',  ( 8.016215341155765728, -5.223177556212426964, -7.499070966595000165 ) ) ;
#13728 = CARTESIAN_POINT ( 'NONE',  ( -9.625925875578284163, 10.33259439770390564, 1.040834085586084257E-14 ) ) ;
#13731 = CARTESIAN_POINT ( 'NONE',  ( -7.930593509350902792, 8.217056947189661287, -0.7998128361456362523 ) ) ;
#13732 = CARTESIAN_POINT ( 'NONE',  ( 4.435452530326143616, 5.203724702582467998, -1.199719254218452047 ) ) ;
#13734 = ORIENTED_EDGE ( 'NONE', *, *, #174269, .T. ) ;
#13733 = CARTESIAN_POINT ( 'NONE',  ( -5.061990249855848667, 6.999017606288844284, -1.599625672291271394 ) ) ;
#13735 = CARTESIAN_POINT ( 'NONE',  ( -7.307481607641392429, 11.46921960898288972, 0.7216878364870458196 ) ) ;
#13736 = CARTESIAN_POINT ( 'NONE',  ( 0.7278961316968115547, -2.094849050945537972, 0.6941159686642893734 ) ) ;
#13737 = CARTESIAN_POINT ( 'NONE',  ( -1.642778471875000035, -1.917708332855375897, -2.845375778867859751 ) ) ;
#13738 = CARTESIAN_POINT ( 'NONE',  ( 4.785966450049039089, -1.203721183051874810, -1.548998264137561254 ) ) ;
#13739 = CARTESIAN_POINT ( 'NONE',  ( -0.4019237886466871523, 8.948664549684629321, -1.499999999999998668 ) ) ;
#13740 = CARTESIAN_POINT ( 'NONE',  ( 0.7499999999999902300, 4.347916667349481123, -1.299038105676658228 ) ) ;
#13741 = CARTESIAN_POINT ( 'NONE',  ( 5.389300372041062381, 6.501875383066589187, -1.316743393031569509 ) ) ;
#13742 = CARTESIAN_POINT ( 'NONE',  ( 0.07479286986305369589, 4.095183424177953668, -2.410510762676120411 ) ) ;
#13743 = CARTESIAN_POINT ( 'NONE',  ( 4.329911453333429527, 1.806054511993939515, 0.3568155486674411958 ) ) ;
#13744 = VERTEX_POINT ( 'NONE', #123124 ) ;
#13745 = CARTESIAN_POINT ( 'NONE',  ( -1.225000000000005640, 2.812500000682796486, -1.734723475976807094E-15 ) ) ;
#13746 = CARTESIAN_POINT ( 'NONE',  ( -8.453672473320708036, 9.821371626084353323, -1.199719254218446718 ) ) ;
#13747 = CARTESIAN_POINT ( 'NONE',  ( -0.5236421425768283955, -3.124072594479749216E-14, 1.213415396354516673 ) ) ;
#13749 = EDGE_CURVE ( 'NONE', #193462, #180190, #138050, .T. ) ;
#13748 = DIRECTION ( 'NONE',  ( -5.578564026256490882E-16, -1.000000000000000000, -9.066213480720158442E-32 ) ) ;
#13750 = CARTESIAN_POINT ( 'NONE',  ( 11.65646892497034592, 7.079448886673395336, -2.644575417635384618 ) ) ;
#13751 = CARTESIAN_POINT ( 'NONE',  ( 4.313465427442102929, 8.184126765324453601, 0.7998128361456462443 ) ) ;
#13752 = CARTESIAN_POINT ( 'NONE',  ( 6.643830136542335119, 0.7930364421293911725, -1.902288772117090687 ) ) ;
#13755 = CARTESIAN_POINT ( 'NONE',  ( 3.210337823311388394, 1.665856106666419034, 0.7845605768846477535 ) ) ;
#13754 = CARTESIAN_POINT ( 'NONE',  ( 1.451354471725987860, 1.406072211568440755, 1.219298000798328507 ) ) ;
#13753 = CARTESIAN_POINT ( 'NONE',  ( 0.000000000000000000, 0.000000000000000000, -5.732590180780448463 ) ) ;
#13756 = CARTESIAN_POINT ( 'NONE',  ( 8.444030743212801227, 8.745790710036752458, 0.7998128361456462443 ) ) ;
#13757 = CARTESIAN_POINT ( 'NONE',  ( -5.582925393777276035, 9.735439736040634173, 0.7998128361456291469 ) ) ;
#13758 = CARTESIAN_POINT ( 'NONE',  ( -5.810221930991193690E-16, 2.125000000682803147, 1.224999999999976774 ) ) ;
#13759 = CARTESIAN_POINT ( 'NONE',  ( 3.194164748978207680, -0.8942147705085048415, 2.017778291555922809 ) ) ;
#13760 = CARTESIAN_POINT ( 'NONE',  ( 5.677129043647218154, -0.04737763303009440846, -2.262073803551585272 ) ) ;
#13761 = CARTESIAN_POINT ( 'NONE',  ( -6.616015773788831211, 7.781401826584148473, 1.082531754730549967 ) ) ;
#13762 = CARTESIAN_POINT ( 'NONE',  ( 6.064714483498689468, 0.5772776769059180246, 1.717211531030158556 ) ) ;
#13763 = CARTESIAN_POINT ( 'NONE',  ( 4.962082351039136086, -1.058791762104252632, 1.596325305674146433 ) ) ;
#13764 = CARTESIAN_POINT ( 'NONE',  ( 1.806654366501771136, 0.000000000000000000, 2.499999999999998668 ) ) ;
#13765 = CIRCLE ( 'NONE', #172896, 9.999999999999996447 ) ;
#13766 = CARTESIAN_POINT ( 'NONE',  ( 6.578970801323708706, -0.09418725797194843485, -1.868394071727994543 ) ) ;
#13767 = CARTESIAN_POINT ( 'NONE',  ( 6.514093505496237668, 1.855963486094978965, -0.1381079127797563977 ) ) ;
#13768 = CARTESIAN_POINT ( 'NONE',  ( 3.551873057100290776, 7.087676300018209474, 0.7216878364870409346 ) ) ;
#13769 = CARTESIAN_POINT ( 'NONE',  ( 6.807488043635657959, -0.3792581958518992935, 1.734866861734218446 ) ) ;
#13770 = CARTESIAN_POINT ( 'NONE',  ( 0.9015777671340443611, -1.966303774932298021, 0.4465067697373495403 ) ) ;
#13772 = CARTESIAN_POINT ( 'NONE',  ( 3.123755640277770418, -2.029568314945415786, 0.5621985482912382759 ) ) ;
#13771 = CARTESIAN_POINT ( 'NONE',  ( -10.15235809853472126, 10.73883929124566983, -0.7998128361456291469 ) ) ;
#13773 = B_SPLINE_CURVE_WITH_KNOTS ( 'NONE', 3,
 ( #52355, #101086, #54487, #18762, #17687, #103239 ),
 .UNSPECIFIED., .F., .F.,
 ( 4, 2, 4 ),
 ( 0.000000000000000000, 0.0004994260320849895846, 0.0009988520641699791692 ),
 .UNSPECIFIED. ) ;
#13774 = CARTESIAN_POINT ( 'NONE',  ( 9.121938423896107651, 9.536683004167278099, -0.7998128361456221525 ) ) ;
#13776 = CARTESIAN_POINT ( 'NONE',  ( -9.515124878692420296, 9.995400534762978850, 1.040834085586084257E-14 ) ) ;
#13775 = CARTESIAN_POINT ( 'NONE',  ( -0.7500000000000006661, -0.1416666666666441254, -1.299038105676652011 ) ) ;
#13777 = LINE ( 'NONE', #171770, #34015 ) ;
#13778 = CARTESIAN_POINT ( 'NONE',  ( 3.340107562988120726, -1.206563586372558561, -1.619613960689977761 ) ) ;
#13779 = CARTESIAN_POINT ( 'NONE',  ( 0.6823417656249917140, 4.092708333674755394, 1.181850606188765695 ) ) ;
#13780 = CARTESIAN_POINT ( 'NONE',  ( 4.518945272056516416, 4.166524327021037699, 0.7998128361456341429 ) ) ;
#13781 = CARTESIAN_POINT ( 'NONE',  ( 3.479894426560462328, 1.368377867093536482, 1.673357603396708360 ) ) ;
#13782 = DIRECTION ( 'NONE',  ( -5.578564026256490882E-16, -1.000000000000000000, -9.066213480720158442E-32 ) ) ;
#13784 = FACE_OUTER_BOUND ( 'NONE', #171293, .T. ) ;
#13783 = CARTESIAN_POINT ( 'NONE',  ( 6.855582950365507244, 8.027210192628430718, -1.199719254218452047 ) ) ;
#13785 = CARTESIAN_POINT ( 'NONE',  ( 10.19536832735223975, 10.99694392477354477, 0.000000000000000000 ) ) ;
#13787 = DIRECTION ( 'NONE',  ( 0.000000000000000000, 1.000000000000000000, 0.000000000000000000 ) ) ;
#13786 = CARTESIAN_POINT ( 'NONE',  ( 1.047617182619766885, 1.914800503461089543, -1.023450759211230521 ) ) ;
#13788 = CARTESIAN_POINT ( 'NONE',  ( -7.212574532790110737, 7.517017831117667193, -0.7216878364870278340 ) ) ;
#13789 = CARTESIAN_POINT ( 'NONE',  ( 0.6823417656249882723, 0.9260416670080831025, -1.181850606188749264 ) ) ;
#13790 = CARTESIAN_POINT ( 'NONE',  ( 2.138457411672203712, 0.4836887423533155483, 2.137355272389021899 ) ) ;
#13791 = CARTESIAN_POINT ( 'NONE',  ( -1.782949938078045138, -1.600000000000000755, 2.093702347113242102 ) ) ;
#13792 = CARTESIAN_POINT ( 'NONE',  ( 2.800010096142038218, -0.7105090101824761417, 2.148112714708799942 ) ) ;
#13793 = CARTESIAN_POINT ( 'NONE',  ( -8.843996274815957293, 9.212417163573759282, 1.040834085586084257E-14 ) ) ;
#13794 = CARTESIAN_POINT ( 'NONE',  ( -3.429849674132942727, 5.984946472254969230, -1.082531754730549078 ) ) ;
#13795 = CARTESIAN_POINT ( 'NONE',  ( -0.6823417656249969321, 4.030208333674754506, -1.181850606188749264 ) ) ;
#13796 = CARTESIAN_POINT ( 'NONE',  ( 4.954704567260191261, 7.963257648925383236, 1.029694947009308859 ) ) ;
#13797 = CARTESIAN_POINT ( 'NONE',  ( -1.500000000000001110, 11.27083333333333393, 0.8660254037844419273 ) ) ;
#13798 = CARTESIAN_POINT ( 'NONE',  ( 7.675324359112103423, 8.127168971818530707, 0.7216878364870267237 ) ) ;
#13799 = CARTESIAN_POINT ( 'NONE',  ( 3.233429047156919811, -1.186097956103189910, -1.313638963288694228 ) ) ;
#13800 =( BOUNDED_CURVE ( )  B_SPLINE_CURVE ( 2, ( #79094, #57528, #191770, #159282, #76956, #140946, #60712, #126876, #44492 ),
 .UNSPECIFIED., .F., .T. ) 
 B_SPLINE_CURVE_WITH_KNOTS ( ( 3, 2, 2, 2, 3 ),
 ( 0.5267857142857143016, 0.5297619047619047672, 0.5357142857142856984, 0.5416666666666666297, 0.5446428571428572063 ),
 .UNSPECIFIED. ) 
 CURVE ( )  GEOMETRIC_REPRESENTATION_ITEM ( )  RATIONAL_B_SPLINE_CURVE ( ( 0.9330127018922194093, 0.9330127018922194093, 1.000000000000000000, 0.8660254037844387076, 1.000000000000000000, 0.8660254037844387076, 1.000000000000000000, 0.9330127018922180770, 0.9330127018922194093 ) ) 
 REPRESENTATION_ITEM ( '' )  );
#13801 =( GEOMETRIC_REPRESENTATION_CONTEXT ( 3 ) GLOBAL_UNCERTAINTY_ASSIGNED_CONTEXT ( ( #7300 ) ) GLOBAL_UNIT_ASSIGNED_CONTEXT ( ( #207618, #191359, #92839 ) ) REPRESENTATION_CONTEXT ( 'NONE', 'WORKASPACE' ) );
#13802 = CARTESIAN_POINT ( 'NONE',  ( 9.935427640716063991, 10.48575375712389679, -0.7998128361456281477 ) ) ;
#13803 = CARTESIAN_POINT ( 'NONE',  ( 0.07735805125222078305, -0.0005418671161615954465, -2.088975025666544472 ) ) ;
#13804 = CARTESIAN_POINT ( 'NONE',  ( 1.364683531249997417, 8.984375000341396245, 2.602085213965210642E-15 ) ) ;
#13805 = EDGE_CURVE ( 'NONE', #54853, #69998, #61985, .T. ) ;
#13806 = CARTESIAN_POINT ( 'NONE',  ( -4.014095998097799267, 6.840806543492835345, -1.199719254218450271 ) ) ;
#13807 = CARTESIAN_POINT ( 'NONE',  ( 5.765249964824501028, 1.862012222821707308, -0.7743297468396084238 ) ) ;
#13808 = VERTEX_POINT ( 'NONE', #154457 ) ;
#13809 = EDGE_CURVE ( 'NONE', #101924, #127020, #210704, .T. ) ;
#13810 = CARTESIAN_POINT ( 'NONE',  ( 3.942156681999692491, 1.861596489644477437, 0.1839347620080991064 ) ) ;
#13811 = CARTESIAN_POINT ( 'NONE',  ( 3.397389602098393802, -1.828008730618407629, 0.9717071122367710867 ) ) ;
#13812 = CARTESIAN_POINT ( 'NONE',  ( -5.600926855776877211, 9.548515408466085930, -0.7216878364870338292 ) ) ;
#13813 = CARTESIAN_POINT ( 'NONE',  ( 5.301814855701348250, 3.000000000000002665, 1.561251128379126385E-14 ) ) ;
#13814 = CARTESIAN_POINT ( 'NONE',  ( -10.44369633504468631, 5.112959841837462882, -5.232137017608346596 ) ) ;
#13815 = CARTESIAN_POINT ( 'NONE',  ( -4.864214080903581205, 4.879786425613829692, -0.6392378712632116322 ) ) ;
#13816 = CARTESIAN_POINT ( 'NONE',  ( 0.6823417656249917140, 3.905208333674754950, 1.181850606188765695 ) ) ;
#13817 = CARTESIAN_POINT ( 'NONE',  ( 3.033595934319989418, 1.863777508880835487, -0.6128360024686765328 ) ) ;
#13818 = CARTESIAN_POINT ( 'NONE',  ( 1.247422469434919412, -1.966343046301596509, -0.4444367004674750210 ) ) ;
#13819 = CARTESIAN_POINT ( 'NONE',  ( 1.123270288250309834, 2.971052654332832610, -0.7749999999993620881 ) ) ;
#13820 = CARTESIAN_POINT ( 'NONE',  ( 9.447334110624092673, 9.916311305349925220, -0.7998128361456281477 ) ) ;
#13821 = CARTESIAN_POINT ( 'NONE',  ( 0.5087955169046609605, 1.624258005607306599, 0.9276666955444978768 ) ) ;
#13822 = CARTESIAN_POINT ( 'NONE',  ( 1.364683531249988535, 3.655208333674750509, -0.7879004041258239610 ) ) ;
#13823 = CARTESIAN_POINT ( 'NONE',  ( 1.863541034856039502, -1.619513613076409397, -1.195741390080407918 ) ) ;
#13825 = CARTESIAN_POINT ( 'NONE',  ( 2.548581339128490608, -1.457745987184940306, 1.535692819318078550 ) ) ;
#13824 = CARTESIAN_POINT ( 'NONE',  ( -7.104109303880803417, 8.350844278358124484, 1.082531754730549967 ) ) ;
#13826 = CARTESIAN_POINT ( 'NONE',  ( 1.485618637124549890, 7.335443175656853221, 4.255655007286210711 ) ) ;
#13827 = CARTESIAN_POINT ( 'NONE',  ( 3.455589482447298355, 1.630370400113918095, 1.275915752658786095 ) ) ;
#13828 = CARTESIAN_POINT ( 'NONE',  ( 6.481679955784983349, 9.719654494127929922, -1.199719254218452047 ) ) ;
#13830 = CARTESIAN_POINT ( 'NONE',  ( 2.191614386903386613, 5.708633884695917260, -0.7998128361456281477 ) ) ;
#13829 = CARTESIAN_POINT ( 'NONE',  ( 6.123005977957785007, -1.968908147963293942, 0.7033269742807277680 ) ) ;
#13832 = EDGE_LOOP ( 'NONE', ( #176733, #106427, #67677, #90976, #85784, #12418 ) ) ;
#13831 = CARTESIAN_POINT ( 'NONE',  ( 4.155160913615768337, -1.517764731708035386, -1.014145119915064841 ) ) ;
#13833 = CARTESIAN_POINT ( 'NONE',  ( 10.37606763316019531, 10.99983374830873650, 0.7998128361456462443 ) ) ;
#13834 = DIRECTION ( 'NONE',  ( 0.000000000000000000, 1.000000000000000000, 0.000000000000000000 ) ) ;
#13835 = CARTESIAN_POINT ( 'NONE',  ( 11.15656239214823664, 9.703780284206802165, -5.826040129427457970 ) ) ;
#13836 = CARTESIAN_POINT ( 'NONE',  ( 6.299877592275240801, -0.7493655176046759570, 2.075778730795534877 ) ) ;
#13837 = CARTESIAN_POINT ( 'NONE',  ( 0.6823417656249934904, 10.75520833367472839, 1.181850606188764807 ) ) ;
#13838 = CARTESIAN_POINT ( 'NONE',  ( 4.863870654145381778, 0.5962773724161560818, -1.817021391602848812 ) ) ;
#13839 = CARTESIAN_POINT ( 'NONE',  ( -8.839026081105473054, 12.39961529701003684, -1.199719254218446718 ) ) ;
#13840 = CARTESIAN_POINT ( 'NONE',  ( 7.308008492965924141, 8.484763649003774333, -1.199719254218451159 ) ) ;
#13841 = CARTESIAN_POINT ( 'NONE',  ( 1.360316468749955598, 1.526041667008097402, 0.7853790794158861388 ) ) ;
#13842 = CARTESIAN_POINT ( 'NONE',  ( 4.826339496340538382, 4.733076955259818419, 1.040834085586084257E-14 ) ) ;
#13843 = CARTESIAN_POINT ( 'NONE',  ( 9.520891725235928860, -8.148349307653536044, -0.3199376857464704682 ) ) ;
#13844 = ADVANCED_FACE ( 'NONE', ( #75335 ), #127777, .T. ) ;
#13845 = CARTESIAN_POINT ( 'NONE',  ( 0.6086344939593493208, -0.2706599535906920040, 1.821105742621460744 ) ) ;
#13846 = ORIENTED_EDGE ( 'NONE', *, *, #144073, .F. ) ;
#13847 = CARTESIAN_POINT ( 'NONE',  ( -0.2108831679770946654, 7.629137130509072939, -2.497154329497498715 ) ) ;
#13848 = VECTOR ( 'NONE', #89131, 1000.000000000000000 ) ;
#13849 = CARTESIAN_POINT ( 'NONE',  ( 4.253091631423633778, -1.553859266942819284, -1.041061106808522929 ) ) ;
#13850 = CARTESIAN_POINT ( 'NONE',  ( -3.644109427023046521, 7.473487774827342278, 0.000000000000000000 ) ) ;
#13851 = CARTESIAN_POINT ( 'NONE',  ( 5.494797395288433250, 9.632623737803665875, 0.000000000000000000 ) ) ;
#13852 = CARTESIAN_POINT ( 'NONE',  ( 0.06005724485651787320, 14.50193764430533250, 11.99783616005606035 ) ) ;
#13853 = CARTESIAN_POINT ( 'NONE',  ( -6.108552962726611746, 7.019250575032890183, 0.9758408306729206005 ) ) ;
#13854 = CARTESIAN_POINT ( 'NONE',  ( -6.575341312947811545, 6.773579074634973551, 1.040834085586084257E-14 ) ) ;
#13855 = CARTESIAN_POINT ( 'NONE',  ( 4.467575310902914154, 5.170924936596891008, 1.199719254218464037 ) ) ;
#13856 = CARTESIAN_POINT ( 'NONE',  ( 0.7429342955292950190, -0.2353911671746557188, -1.955230025236649682 ) ) ;
#13857 = CARTESIAN_POINT ( 'NONE',  ( 2.337517745082304810, 0.5350678814987767096, -1.944078148028173914 ) ) ;
#13858 = CARTESIAN_POINT ( 'NONE',  ( -9.155833807930273238, 9.576227618873799585, -0.7998128361456291469 ) ) ;
#13859 = CARTESIAN_POINT ( 'NONE',  ( 6.066347387471824781, 6.042103138330730872, -0.7998128361456481317 ) ) ;
#13860 = DIRECTION ( 'NONE',  ( 0.05872483221476459958, 0.000000000000000000, -0.9982742078614211811 ) ) ;
#13861 = CARTESIAN_POINT ( 'NONE',  ( 2.291216553123593958, 1.694975396412688351, 1.389067552005143424 ) ) ;
#13862 = CARTESIAN_POINT ( 'NONE',  ( -9.134442807305063639, 11.67993591332117376, 1.599625672291281386 ) ) ;
#13863 = FACE_OUTER_BOUND ( 'NONE', #6100, .T. ) ;
#13864 = DIRECTION ( 'NONE',  ( 0.000000000000000000, 0.000000000000000000, 1.000000000000000000 ) ) ;
#13865 = EDGE_CURVE ( 'NONE', #89267, #15203, #135168, .T. ) ;
#13866 = CARTESIAN_POINT ( 'NONE',  ( -9.348561386899502779, 3.999985931113709814, -7.001914024221965960 ) ) ;
#13867 = CARTESIAN_POINT ( 'NONE',  ( 8.121497709785879593, 9.433834401960398353, -1.199719254218445830 ) ) ;
#13868 = CARTESIAN_POINT ( 'NONE',  ( 6.094553744542824170, 7.069066442510145265, 1.199719254218462483 ) ) ;
#13869 = CARTESIAN_POINT ( 'NONE',  ( -4.569915857295916872, 8.517381272593750552, -0.02673743978307913799 ) ) ;
#13870 = CARTESIAN_POINT ( 'NONE',  ( 5.221298555038576872, 9.105615724271411082, 0.000000000000000000 ) ) ;
#13871 = ORIENTED_EDGE ( 'NONE', *, *, #45298, .F. ) ;
#13873 = CARTESIAN_POINT ( 'NONE',  ( 2.104154084628720334, -0.8588668247239000797, 1.820802598171267439 ) ) ;
#13872 = CARTESIAN_POINT ( 'NONE',  ( 5.231922985772964552, 1.814955821992572993, 0.3091130605668013231 ) ) ;
#13874 = CARTESIAN_POINT ( 'NONE',  ( 3.708664688178139102, -1.738024148615105569, -1.504010254680566483 ) ) ;
#13876 = CARTESIAN_POINT ( 'NONE',  ( 2.113880859634624354, 1.856391821545114951, -0.1307286092924550835 ) ) ;
#13875 = CARTESIAN_POINT ( 'NONE',  ( -0.1290005225502676156, 1.324981729379502537, -2.425680704180297464 ) ) ;
#13877 = CARTESIAN_POINT ( 'NONE',  ( 3.285556943750000070, -1.684374999522043836, 0.000000000000000000 ) ) ;
#13878 = CARTESIAN_POINT ( 'NONE',  ( 5.642805672956042962, 1.844803604357934779, 0.5037821151940986564 ) ) ;
#13879 = CARTESIAN_POINT ( 'NONE',  ( -6.984421689334302741, 11.30024240419870374, 0.000000000000000000 ) ) ;
#13880 = CARTESIAN_POINT ( 'NONE',  ( -4.828112100242279325, 8.646898193675708555, -0.7216878364870338292 ) ) ;
#13882 = CARTESIAN_POINT ( 'NONE',  ( 3.731198135974967300, -1.728734619261709904, 0.7151963084984153118 ) ) ;
#13881 = CARTESIAN_POINT ( 'NONE',  ( 5.144118995967028596, 0.6083014027435985627, 2.000272865920887266 ) ) ;
#13883 = CARTESIAN_POINT ( 'NONE',  ( 5.666945020832160118, 9.555260257705446847, 0.7216878364870438212 ) ) ;
#13884 = CARTESIAN_POINT ( 'NONE',  ( 5.354971380013192395, 0.3533838956982695567, -1.806849549699687696 ) ) ;
#13885 = CARTESIAN_POINT ( 'NONE',  ( 4.695201269034174452, 4.372156323494968966, 1.214306433183764966E-14 ) ) ;
#13886 = CARTESIAN_POINT ( 'NONE',  ( -5.737959331755660019E-16, -8.256136661604607241, -10.93205753685918680 ) ) ;
#13887 = CARTESIAN_POINT ( 'NONE',  ( 5.584504578548418863, -1.684151958202559252, -0.3718293602123431962 ) ) ;
#13888 = CARTESIAN_POINT ( 'NONE',  ( -6.911959384868566758, 6.958374125301778790, 1.040834085586084257E-14 ) ) ;
#13889 = CARTESIAN_POINT ( 'NONE',  ( 0.7032560681843272876, 1.601581415593232860, 0.6654971025301190668 ) ) ;
#13890 = SURFACE_STYLE_USAGE ( .BOTH. , #17085 ) ;
#13891 = FACE_OUTER_BOUND ( 'NONE', #80347, .T. ) ;
#13892 = CARTESIAN_POINT ( 'NONE',  ( 4.539989016966003099, 1.413352768409949389, 1.648148102320112329 ) ) ;
#13893 = CARTESIAN_POINT ( 'NONE',  ( 3.422296110638740174, 1.157362003623555236, -1.411967061744797691 ) ) ;
#13894 = CARTESIAN_POINT ( 'NONE',  ( 1.024179675629211861, 0.9620134025654383247, 1.709582039726687430 ) ) ;
#13895 = CARTESIAN_POINT ( 'NONE',  ( 0.2107725088618967457, 2.027540257690120029, 0.6097772466436711669 ) ) ;
#13897 = CARTESIAN_POINT ( 'NONE',  ( -1.001543065824772872E-14, 4.384375000341417916, 1.575800808251672791 ) ) ;
#13896 = CARTESIAN_POINT ( 'NONE',  ( 0.3227791477718846558, 2.195406398872503217, 0.6593016323864949735 ) ) ;
#13898 = CARTESIAN_POINT ( 'NONE',  ( 5.738979324004444216, 5.917037536917005625, 2.440165351819284290 ) ) ;
#13899 = CARTESIAN_POINT ( 'NONE',  ( 8.809047120577066181, 11.30030761213851953, 1.599625672291281386 ) ) ;
#13900 = CIRCLE ( 'NONE', #93578, 0.07999999999999998779 ) ;
#13901 = CARTESIAN_POINT ( 'NONE',  ( 2.983181628360128013, -1.960071735995170927, -0.8095406527153580223 ) ) ;
#13902 = CARTESIAN_POINT ( 'NONE',  ( -4.609409038966253647, 4.479991421656468908, -0.7216878364870207285 ) ) ;
#13903 = CARTESIAN_POINT ( 'NONE',  ( -6.385527162356468445, 10.39360608948380538, 1.040834085586084257E-14 ) ) ;
#13904 = CARTESIAN_POINT ( 'NONE',  ( -3.565431210269599749, 7.103494145382415859, 0.7216878364870317197 ) ) ;
#13905 = CARTESIAN_POINT ( 'NONE',  ( 0.9540663221972445207, -0.7486024665571254788, 1.930331157511067097 ) ) ;
#13906 = CARTESIAN_POINT ( 'NONE',  ( -1.402160292154681736E-14, 13.59375000068279604, 1.732050807568881190 ) ) ;
#13908 = EDGE_LOOP ( 'NONE', ( #58646, #54612, #102300 ) ) ;
#13907 = CARTESIAN_POINT ( 'NONE',  ( 2.332966905468473406, 1.448476307009987307, -1.684171307209429314 ) ) ;
#13909 = CARTESIAN_POINT ( 'NONE',  ( 0.1944798361989338309, 2.004116887782161349, 1.125739740898183294 ) ) ;
#13911 = CARTESIAN_POINT ( 'NONE',  ( 6.016483441405136467, 0.8307744727026479259, 1.888021813390627246 ) ) ;
#13910 = CARTESIAN_POINT ( 'NONE',  ( 8.581948047770334043, 12.95609712246668899, 0.000000000000000000 ) ) ;
#13913 = CARTESIAN_POINT ( 'NONE',  ( 0.000000000000000000, -1.837499999999999911, -4.012584370867899430 ) ) ;
#13912 = CARTESIAN_POINT ( 'NONE',  ( 6.703580607314123085, 6.785541894813420072, 0.000000000000000000 ) ) ;
#13914 = ADVANCED_FACE ( 'NONE', ( #161936 ), #71375, .T. ) ;
#13915 = CARTESIAN_POINT ( 'NONE',  ( 4.362691568547328202, 8.311833606605697256, -0.7998128361456381397 ) ) ;
#13916 = CARTESIAN_POINT ( 'NONE',  ( 0.2331563151865486683, 7.629137130509099585, -2.545728013813946422 ) ) ;
#13917 = CARTESIAN_POINT ( 'NONE',  ( 5.091278345985558396, -0.6575378499774006125, 1.720029930423284448 ) ) ;
#13918 = EDGE_CURVE ( 'NONE', #11196, #202127, #26572, .T. ) ;
#13919 = CARTESIAN_POINT ( 'NONE',  ( 4.680589345215795838, 6.483773540883647435, -1.599625672291256295 ) ) ;
#13920 = CARTESIAN_POINT ( 'NONE',  ( 1.729112849636908367, -1.625594568690587050, 0.5768372424696955880 ) ) ;
#13921 = CARTESIAN_POINT ( 'NONE',  ( 0.8840003597419334724, -2.016708404047353742, 0.004841148455551891328 ) ) ;
#13922 = CARTESIAN_POINT ( 'NONE',  ( 1.916985526034093335, -1.504927692415005014, -1.737642283433957768 ) ) ;
#13923 = CARTESIAN_POINT ( 'NONE',  ( 0.6823417656249899377, 3.738541667008085767, -1.181850606188754593 ) ) ;
#13924 = CARTESIAN_POINT ( 'NONE',  ( 2.021152898351881166, 2.110506920502265960, 0.8154138738461161884 ) ) ;
#13925 = CARTESIAN_POINT ( 'NONE',  ( 4.512399653719460169, -0.8998888299811370617, -1.904278430835882885 ) ) ;
#13926 = CARTESIAN_POINT ( 'NONE',  ( -3.688700311369816909, 6.461178242310183784, -1.199719254218450271 ) ) ;
#13927 = CARTESIAN_POINT ( 'NONE',  ( 2.530210103492841256, 1.715365446638704494, 0.4347029418121580169 ) ) ;
#13928 = CARTESIAN_POINT ( 'NONE',  ( 5.148345644887269756, 7.029489223833707001, -1.599625672291256295 ) ) ;
#13930 = CARTESIAN_POINT ( 'NONE',  ( 4.827800031893906052, 1.179792396777184615, -1.965320743881134646 ) ) ;
#13929 = CARTESIAN_POINT ( 'NONE',  ( 5.519577934094861860, 6.572500690266394940, 1.082531754730549078 ) ) ;
#13931 = CARTESIAN_POINT ( 'NONE',  ( -5.434120640978981065, 5.234228924097238611, -0.7998128361456221525 ) ) ;
#13932 = CARTESIAN_POINT ( 'NONE',  ( -1.201851678989727383E-14, 1.962500000000020783, 1.732050807568877637 ) ) ;
#13933 = CARTESIAN_POINT ( 'NONE',  ( 4.048915112334880106, -1.821525731582713359, -1.218098874207810933 ) ) ;
#13934 = CARTESIAN_POINT ( 'NONE',  ( -4.599240423533815125, 6.388866465587984322, 1.599625672291267398 ) ) ;
#13935 = CARTESIAN_POINT ( 'NONE',  ( 0.2718889520039936558, 8.158259021453691417, -2.022062967018519064 ) ) ;
#13936 = CARTESIAN_POINT ( 'NONE',  ( 6.639320575229281651, -0.0007625845807879281287, 2.103388539994067497 ) ) ;
#13937 = CARTESIAN_POINT ( 'NONE',  ( 0.6823417656249899377, 2.842708333674753618, 1.181850606188765695 ) ) ;
#13938 = CARTESIAN_POINT ( 'NONE',  ( 2.648949911425259263, -1.601578617359520340, 1.070393023584510050 ) ) ;
#13939 = CARTESIAN_POINT ( 'NONE',  ( 0.6823417656249969321, 9.526041667008065872, -1.181850606188757036 ) ) ;
#13940 = CARTESIAN_POINT ( 'NONE',  ( -4.365362273920257330, 6.116008624372160973, 1.443375672974064550 ) ) ;
#13941 = CARTESIAN_POINT ( 'NONE',  ( 5.765915565743810589, 0.6138260544302427402, -2.029845472315944921 ) ) ;
#13942 = CARTESIAN_POINT ( 'NONE',  ( -5.478903473698255588, 7.485416367438324059, -1.443375672974066548 ) ) ;
#13943 = ORIENTED_EDGE ( 'NONE', *, *, #136186, .T. ) ;
#13945 = CARTESIAN_POINT ( 'NONE',  ( 4.343210567687194157, 7.059472288894379055, 1.256205200019292256 ) ) ;
#13944 = CARTESIAN_POINT ( 'NONE',  ( -3.960390268967665328, 6.674186842887300131, 1.082531754730549967 ) ) ;
#13946 = CARTESIAN_POINT ( 'NONE',  ( 5.054492339796319733, 4.791329239384148231, -0.7998128361456211532 ) ) ;
#13947 = CARTESIAN_POINT ( 'NONE',  ( 6.005383971424570255, -1.826508537601937432, 0.2321369796495567073 ) ) ;
#13948 = CARTESIAN_POINT ( 'NONE',  ( 0.000000000000000000, 8.499999999999996447, 0.000000000000000000 ) ) ;
#13949 = CARTESIAN_POINT ( 'NONE',  ( 0.5451294565930948632, 6.857673063737054875, -3.776897418316011557 ) ) ;
#13950 = CARTESIAN_POINT ( 'NONE',  ( -1.364683531250012516, 4.301041667008089320, -0.7879004041258300672 ) ) ;
#13951 = CARTESIAN_POINT ( 'NONE',  ( 1.891783327304029205, -0.4647161096258972668, -1.677148923195219243 ) ) ;
#13952 = CARTESIAN_POINT ( 'NONE',  ( 5.205967797967502975, 5.175976640491358083, -0.7216878364870503715 ) ) ;
#13953 = CARTESIAN_POINT ( 'NONE',  ( 0.4319881149899909567, 1.126445828788334991, 1.606065282034954578 ) ) ;
#13954 = CARTESIAN_POINT ( 'NONE',  ( -1.364683531250000748, 0.5718750003414208027, 0.000000000000000000 ) ) ;
#13955 = DIRECTION ( 'NONE',  ( 0.6507913734559641616, 0.7592566023653004592, 0.000000000000000000 ) ) ;
#13956 = CARTESIAN_POINT ( 'NONE',  ( -10.63367255181986160, 11.30037282007833532, 1.040834085586084257E-14 ) ) ;
#13957 = CARTESIAN_POINT ( 'NONE',  ( -4.894130264408858899, 8.653643041878236630, -0.7216878364870207285 ) ) ;
#13958 = CARTESIAN_POINT ( 'NONE',  ( 5.647404790089923132, -1.701416311724871067, -1.333359258283283166 ) ) ;
#13960 = ORIENTED_EDGE ( 'NONE', *, *, #149988, .T. ) ;
#13959 = DIRECTION ( 'NONE',  ( -0.000000000000000000, -1.000000000000000000, -0.000000000000000000 ) ) ;
#13961 = CARTESIAN_POINT ( 'NONE',  ( -1.001543065824772872E-14, 4.321875000341417916, 1.575800808251672791 ) ) ;
#13962 = CARTESIAN_POINT ( 'NONE',  ( 6.274684828636788225, -1.871173557121402542, -0.6205748305461754599 ) ) ;
#13963 = CARTESIAN_POINT ( 'NONE',  ( 5.079290571759123019, 1.194821443462086963, -1.256652284620445759 ) ) ;
#13965 = CARTESIAN_POINT ( 'NONE',  ( 1.470551405592795957, -2.082434148983134392, -0.6831980896230758216 ) ) ;
#13964 = CARTESIAN_POINT ( 'NONE',  ( -1.360316468750002894, 0.4114583336747319464, 0.7853790794158961308 ) ) ;
#13966 = CARTESIAN_POINT ( 'NONE',  ( 3.223938161889360110, -2.224449554215703895, 0.6136290147475926826 ) ) ;
#13967 = CARTESIAN_POINT ( 'NONE',  ( 6.257116178607133428, -1.765205416791076010, -1.063208849337776485 ) ) ;
#13968 = CARTESIAN_POINT ( 'NONE',  ( 1.693202460532976295, -0.6543010362765960819, 1.828533997230662234 ) ) ;
#13969 = CARTESIAN_POINT ( 'NONE',  ( -5.368665640887164692, 9.207267647769599606, 0.000000000000000000 ) ) ;
#13970 = CARTESIAN_POINT ( 'NONE',  ( -5.354544322754380303, 5.211666229493680191, 0.7998128361456281477 ) ) ;
#13971 = CARTESIAN_POINT ( 'NONE',  ( -9.586151930903435314, 14.76609868405410886, 7.218760141420751175 ) ) ;
#13972 = CARTESIAN_POINT ( 'NONE',  ( 3.902672080109194752, -2.098000727953463151, -0.3078000538283761078 ) ) ;
#13973 = CARTESIAN_POINT ( 'NONE',  ( 2.514296259408643319, -1.880434619097739013, 0.7283795345095490648 ) ) ;
#13974 = CARTESIAN_POINT ( 'NONE',  ( -6.697364695026446491, 6.915939687060050467, 1.040834085586084257E-14 ) ) ;
#13975 = CARTESIAN_POINT ( 'NONE',  ( 4.876106637443972325, 1.267215935518750669, 1.806476597341267087 ) ) ;
#13976 = CARTESIAN_POINT ( 'NONE',  ( 3.285556943749998737, -0.3427083328553764408, -1.896917185911906500 ) ) ;
#13978 =( BOUNDED_SURFACE ( )  B_SPLINE_SURFACE ( 3, 3, ( 
 ( #57975, #7062, #41753, #107865, #138175, #5994, #173891, #108931, #121997, #87276, #154415, #89428, #157626, #155479, #139239, #9223, #75295, #141411, #153345, #207418, #59037, #125195, #191158, #42825, #70993, #96907, #161896, #64379, #143541, #208471, #44952, #12409, #160817, #95840, #30831, #194374, #114270, #195454, #27604, #144606, #94769, #26534, #78489, #111060, #93705, #193307, #146726, #159745, #77424, #28683, #61177, #79558, #210621, #62247, #179207, #129472, #130524, #128407, #158683, #162959, #46018, #142463, #43886, #60107, #112137, #126266, #178141, #196515, #13483, #176012, #127337, #177067, #29755, #92641, #212745, #192223, #145677, #211674, #63310, #47083, #113201, #209535, #14537, #80634, #48158, #10282, #76356, #110000, #11343, #168272, #198616, #83810, #183449, #81689, #49206, #84884, #149903, #1470, #133679, #199684, #213789, #51327, #16667, #397, #68611, #115326, #147773, #82751, #97968, #116381, #148824, #19873, #18800, #52392, #67537, #165076, #167212, #180267, #100073, #200743, #184504, #31891, #131561, #65412, #36123, #197562, #182369, #33999, #117455, #166135, #66468, #150971, #132609, #2536, #35053, #181316, #164026, #32945, #15601, #99018, #50262, #101124, #85957, #17722, #134735, #118520, #102207, #152032, #3602, #69680, #135784, #201808, #53450, #153091, #138996, #170394, #154166, #7888, #54524, #20923, #21983, #37202, #55589, #88092, #173640, #172552, #206093, #23062, #104350, #106526, #119589, #39339, #140070, #123885, #185572, #70739, #4666, #189851, #136852, #121744, #187711, #56663, #105437, #5731, #24137, #71810, #156305, #72889, #120669, #103276, #202876, #169338, #186647, #137921, #203941, #171472, #89178, #87018, #205017, #38273, #122826, #90239, #155230, #6811, #40423, #73975, #41496, #57728, #157374, #188788, #107609, #25213, #91317, #8969, #75042, #141159, #207166, #146473, #13239, #59855, #176813, #127083, #58790, #193046, #143288, #126007, #11090, #178962, #191968, #109749, #60926, #93454, #111886, #44700, #110807, #211429, #161644, #162711, #28428, #190907, #63059, #94521, #174702, #76105, #92393, #160559, #26277, #12167, #96658, #194118, #208223, #159491, #209279, #78239, #124945, #30577, #158429, #62002, #77167, #144361, #210362, #128158, #175759, #45769, #195200, #177890, #27351, #29503, #95596, #43634, #79312, #145428, #129227, #46837, #112951, #14283, #80378, #42571, #108674, #10031, #142209, #2285, #116132, #114023, #15353, #31640, #50008, #180019, #152, #35880, #133427, #147524, #32689, #148583, #182120, #64134, #118269, #97717, #1226, #98769, #33750, #66218, #82496, #48957, #83562, #134494, #132366, #115075, #99827, #164826, #149644, #200498, #16416, #165893, #67288, #163775, #81447, #117202, #17478, #199434, #51076, #183199, #213545, #34805, #181071, #198368, #100880, #65168, #131323, #166967, #130278, #18557, #84634, #52141, #150725, #68361, #184253, #197316, #101955, #212493, #168022, #19626, #85697, #196266, #47913, #36945, #156041, #103026, #153913, #5483, #88923, #71564, #136603, #204756, #120414, #188531, #105178, #152842, #69429, #169081, #3358, #185322, #38026, #202627, #104097, #54277, #53204, #22808, #135534, #154976, #56407, #201558, #186389, #72641, #106275, #7630, #138738, #189597, #170146, #119335, #21733, #137671, #203692, #6561, #73715, #171214, #24956 ),
 ( #139813, #87842, #20680, #55339, #122568, #173372, #151785, #121491, #40161, #187463, #4416, #172296, #205841, #107350, #23884, #89990, #57475, #41243, #123634, #86770, #70487, #39091, #13767, #163244, #131841, #164299, #178432, #79843, #15888, #158185, #30039, #124690, #145952, #195740, #157119, #81972, #96125, #196797, #207969, #197849, #43372, #48438, #112418, #108423, #114553, #180545, #59595, #147008, #63601, #125752, #92131, #191714, #190648, #181596, #49481, #115601, #162181, #213026, #140894, #211962, #91058, #8708, #47377, #129755, #113488, #26021, #58535, #179496, #42308, #74792, #97192, #31118, #14827, #206904, #174445, #148059, #214067, #9778, #64660, #75850, #141957, #80918, #32167, #130805, #98245, #65693, #185857, #182663, #51623, #199974, #102493, #151256, #86243, #165355, #2826, #101424, #132893, #36414, #168557, #167496, #68897, #135016, #84106, #166427, #201030, #54815, #150193, #120964, #149106, #35346, #52672, #33224, #99308, #20156, #19092, #152313, #53745, #1762, #198896, #136072, #118803, #3890, #119879, #184788, #203170, #34284, #133967, #83032, #66752, #21209, #153380, #116665, #69960, #16951, #50543, #685, #37489, #202087, #100357, #103567, #169626, #18017, #117747, #183738, #87311, #4951, #71029, #67820, #137143, #85172, #72102, #190137, #41791, #106817, #90531, #8187, #23356, #105730, #156593, #208506, #89465, #60141, #88385, #189079, #74272, #186935, #38567, #107904, #40712, #91611, #207455, #155519, #138213, #75331, #140364, #173930, #59074, #206383, #142500, #188000, #73172, #141448, #108966, #205310, #55877, #139278, #25503, #104642, #170689, #58009, #157662, #123119, #39625, #124173, #174986, #22276, #9260, #125234, #191192, #10317, #42859, #26570, #92675, #158719, #172847, #76391, #154455, #6033, #56947, #24418, #204225, #171760, #122034, #7100, #144640, #46051, #192257, #179242, #12444, #63347, #193342, #80670, #177102, #129506, #28717, #11379, #195487, #47121, #44987, #79594, #128443, #111096, #143576, #94804, #93740, #64414, #146761, #212779, #78523, #145713, #110035, #160852, #126298, #176047, #178176, #210655, #29791, #209568, #159779, #62283, #77458, #27640, #13521, #161931, #112172, #211711, #113238, #95876, #61214, #127371, #14575, #43920, #30866, #194409, #162994, #96944, #126998, #43547, #9947, #60837, #42482, #109669, #40339, #123804, #57644, #174619, #8880, #158354, #22976, #74959, #173554, #204930, #108591, #26195, #25127, #141069, #207076, #156225, #24056, #58707, #192957, #7802, #105348, #6730, #107523, #124857, #171385, #89094, #92311, #91230, #76023, #125928, #73894, #56581, #208139, #190821, #142126, #191886, #59769, #155148, #106445, #206009, #175671, #27259, #189764, #188703, #41416, #93367, #72809, #138910, #159403, #11002, #157290, #172468, #77079, #143207, #122740, #209197, #90159, #139988, #38494, #134950, #169556, #5958, #86175, #200957, #136002, #36342, #21138, #72029, #102420, #202015, #87241, #199906, #167430, #203095, #53674, #119806, #37419, #103495, #117677, #153306, #52605, #118734, #186864, #19022, #51552, #184718, #1695, #20087, #168488, #138141, #137070, #170617, #185785, #68828, #70960, #84033, #3818, #104572, #88317, #150122, #35273, #183670, #154381, #101351, #152245, #69889, #4881, #54740, #120890, #22204, #85102, #204150, #55806, #121960, #187927 ),
 ( #67749, #151187, #105658, #39557, #171686, #133899, #2759, #175981, #172776, #41722, #190070, #92610, #141378, #76327, #155443, #205235, #107832, #9193, #157598, #158653, #27574, #191125, #111030, #192192, #24350, #207389, #91539, #23283, #75264, #173857, #90460, #25433, #143507, #156526, #74205, #59010, #57942, #142433, #125166, #42791, #93672, #126231, #127306, #108900, #7028, #159715, #174923, #139205, #40646, #56876, #26503, #123052, #10251, #61144, #208441, #8117, #124107, #60075, #43856, #89395, #209504, #189003, #109970, #73104, #140299, #11313, #77391, #206318, #193277, #44922, #106749, #13454, #14508, #129441, #48127, #165041, #195424, #80599, #180237, #78458, #45986, #81656, #146695, #212711, #130498, #196485, #210590, #114239, #79530, #211644, #65382, #112107, #144576, #145648, #94739, #113170, #63279, #16634, #15569, #49176, #64352, #161864, #163994, #177035, #96877, #197531, #181284, #28652, #128377, #62220, #32911, #30798, #194345, #31861, #97936, #162927, #147743, #213759, #47054, #95808, #131528, #198583, #179174, #50229, #178110, #115293, #98988, #160785, #12378, #82718, #148795, #365, #66438, #132580, #29726, #4633, #19840, #103246, #202845, #152000, #71778, #117422, #2506, #70705, #38242, #134705, #199651, #68579, #37168, #137894, #116349, #85926, #86987, #52361, #183419, #135754, #104316, #203913, #69645, #154131, #20891, #200710, #54494, #53417, #153058, #201777, #36090, #185540, #5701, #186616, #118490, #102174, #170366, #35022, #184473, #149872, #168241, #3572, #182339, #21949, #119554, #136818, #18769, #33967, #169306, #120638, #88059, #133651, #100044, #166107, #84853, #17693, #83780, #150943, #101094, #1440, #67504, #51297, #167180, #159455, #57696, #174670, #105402, #156273, #55560, #187679, #8932, #7857, #75012, #204984, #23030, #189817, #89145, #39307, #58758, #207133, #157343, #171440, #155199, #43597, #175721, #138962, #26243, #121715, #6780, #77134, #208190, #92362, #11053, #124910, #59823, #56629, #73942, #140037, #190873, #72855, #206061, #158399, #123853, #107576, #122794, #41467, #93418, #42539, #188752, #90209, #173610, #25183, #40391, #27313, #106495, #108642, #172521, #24106, #9997, #76074, #91284, #141122, #191933, #142174, #125976, #109716, #143255, #80337, #200194, #13198, #112913, #917, #110775, #78201, #116894, #178924, #30539, #162673, #14243, #28390, #149337, #45731, #29466, #100583, #144326, #176775, #111850, #127048, #145392, #177854, #51847, #50765, #84331, #96619, #194079, #199121, #209244, #129187, #18247, #1984, #60888, #160524, #94486, #68048, #12129, #211390, #63018, #66984, #195165, #95557, #182893, #161608, #34510, #133122, #210325, #193008, #61962, #44661, #128119, #79274, #46800, #166657, #150417, #134185, #117966, #183960, #35571, #101651, #167718, #19321, #85397, #105973, #38789, #102724, #73407, #151483, #119031, #169848, #137372, #71259, #6260, #155745, #104870, #24653, #171995, #152534, #55042, #5183, #3053, #203389, #21435, #4120, #103798, #57174, #70189, #202323, #153612, #186089, #204455, #121191, #187160, #89694, #39864, #40940, #170915, #69122, #7330, #22510, #52897, #168781, #185013, #88620, #139510, #23587, #107045, #154675, #135243, #205537, #72331, #36640, #20386, #86470, #138437, #136301, #56109, #189300, #122266, #53973, #37720, #87543, #188224 ),
 ( #123336, #120110, #173072, #201257, #176267, #78741, #109198, #208734, #93965, #206609, #174151, #209799, #60361, #126524, #44137, #110258, #124395, #27869, #141667, #125456, #193567, #25724, #58239, #207678, #8408, #26792, #59297, #144865, #143802, #177328, #192485, #75557, #77681, #90760, #10538, #111325, #95026, #156821, #42015, #190353, #161076, #108124, #92897, #158943, #160006, #76611, #191418, #61434, #43085, #127601, #11607, #91833, #74493, #157892, #140599, #9484, #175210, #142725, #45210, #28942, #12667, #210872, #62497, #128662, #194630, #46271, #112388, #178400, #198867, #131812, #195710, #166393, #30012, #211935, #48411, #15860, #164271, #99279, #34254, #197821, #117715, #50514, #31088, #148029, #98219, #96096, #81946, #114523, #97161, #196768, #150162, #163216, #80890, #32139, #64634, #83000, #214039, #49453, #65664, #165327, #67787, #100326, #180518, #115571, #17984, #14799, #181567, #63570, #33196, #16920, #162151, #84074, #149076, #132863, #146980, #133937, #653, #116637, #66720, #47345, #182632, #1730, #212997, #199943, #51591, #130773, #13738, #79811, #129726, #145923, #113459, #179464, #185823, #88352, #19061, #69928, #183705, #101391, #137107, #136040, #203136, #118771, #151226, #103533, #2795, #167465, #186898, #120925, #70994, #85139, #68866, #171722, #89429, #52641, #154416, #35313, #134986, #205272, #121998, #5995, #139240, #38530, #187964, #184754, #202052, #53712, #104608, #200996, #119845, #72066, #37454, #169592, #36382, #170655, #22242, #21175, #87278, #4917, #20124, #102460, #153347, #56912, #86210, #168526, #152282, #54778, #138176, #3855, #204186, #55842, #39592, #105695, #23321, #155480, #7063, #73136, #26535, #110001, #209536, #158685, #78490, #124139, #9225, #77425, #44954, #141412, #206349, #75297, #43887, #144607, #123085, #92643, #93706, #59038, #190101, #142464, #111062, #210622, #76357, #160818, #27606, #207419, #61178, #60108, #159746, #11344, #125196, #41754, #208472, #177068, #189042, #126267, #12410, #143542, #191159, #127338, #192224, #193308, #176014, #42826, #28684, #40679, #94770, #108932, #174953, #106782, #107866, #10283, #156558, #172810, #24382, #90495, #8153, #74237, #140330, #25467, #57976, #173892, #91575, #157627, #79559, #16668, #165077, #179208, #115327, #31892, #30832, #63312, #96908, #161897, #149904, #166136, #17723, #64380, #181318, #112138, #162960, #62248, #194376, #15603, #14539, #81690, #211676, #29756, #196516, #95841, #46019, #65413, #213790, #164028, #178142, #13484, #50264, #182371, #145678, #32946, #128409, #129473, #83811, #398, #99020, #195455, #131562, #66469, #47084, #80636, #146728, #197563, #113202, #212746, #82752, #130525, #48159, #114271, #49207, #148825, #180268, #97969, #147774, #132610, #198617, #116382, #34000, #100074, #89180, #117456, #3604, #37204, #1471, #67538, #4668, #69681, #120671, #21985, #118521, #101125, #104352, #119591, #202878, #88094, #103278, #171474, #2537, #102208, #170397, #137922, #19874, #84885, #168273, #136854, #23064, #133680, #185574, #5733, #199685, #167213, #18801, #71812, #150972, #135785, #201809, #153093, #53452, #200744, #54526, #184505, #38275, #169340, #68612, #51329, #134737, #183450, #35054, #85958, #52393, #152033, #36124, #20925, #87021, #70741, #186649, #154167, #203943, #55590, #121745, #187713, #39342 ),
 ( #105438, #156306, #58792, #8971, #155232, #75045, #25215, #7890, #107611, #60928, #73978, #206096, #157377, #189853, #208225, #141160, #207168, #93456, #43636, #44702, #124947, #72891, #159493, #190909, #56665, #172554, #188790, #42573, #122829, #108676, #193048, #76107, #90240, #41498, #91319, #174704, #6813, #127085, #40425, #158432, #138997, #140072, #142211, #109751, #57730, #26280, #77169, #92394, #123887, #10033, #173642, #59857, #143290, #126009, #191970, #175761, #106528, #24138, #27354, #11092, #209281, #110810, #176815, #28430, #205019, #145430, #129228, #197317, #29505, #210364, #211430, #12169, #30578, #63061, #148584, #147525, #181072, #212494, #79314, #81448, #94523, #14284, #115076, #160561, #64135, #65169, #96659, #161646, #114024, #16417, #50009, #47914, #132367, #213546, #112952, #32690, #31641, #131324, #180020, #80379, #163776, #198369, #164827, #178963, #146475, #82497, #13241, #162712, #128160, #130279, #196267, #78241, #153, #97718, #48958, #195201, #116133, #46838, #98771, #15355, #111888, #66219, #182122, #144363, #62004, #194121, #45771, #95598, #177892, #133428, #121492, #137672, #203694, #35881, #152843, #83563, #134496, #33751, #165894, #201559, #200499, #53205, #183200, #1227, #168023, #67289, #17479, #36947, #185323, #135535, #149645, #199435, #21734, #153914, #117203, #4417, #99828, #51078, #55340, #186390, #70488, #34806, #103027, #38027, #100881, #52142, #118270, #169082, #166968, #184254, #136604, #101956, #19627, #18558, #20681, #86772, #85698, #151786, #69430, #84635, #150726, #3360, #2286, #68362, #119336, #202628, #54278, #120416, #104098, #170148, #87843, #5484, #71565, #207970, #89991, #72643, #75851, #91059, #174446, #59596, #8709, #143028, #188532, #73716, #141958, #109494, #205843, #56408, #139814, #108425, #209024, #107351, #42309, #191716, #140895, #60660, #125753, #40162, #157120, #41244, #187464, #173373, #57476, #106276, #123635, #93198, #172297, #23885, #189598, #7631, #26022, #24958, #74794, #43373, #175501, #76904, #206905, #105179, #27091, #58536, #88924, #204757, #6562, #124691, #154977, #190649, #10830, #92132, #122570, #158187, #9779, #159229, #39093, #171215, #138739, #22809, #156043, #127904, #113756, #81183, #177633, #212230, #48695, #128951, #29242, #178696, #79043, #63864, #114809, #145159, #30310, #130019, #28167, #210097, #31377, #96396, #162446, #80108, #146213, #160302, #196010, #95333, #161382, #15093, #61737, #94263, #12967, #44438, #62789, #211164, #180808, #179761, #213293, #14022, #111621, #97453, #126823, #46567, #147261, #131068, #192780, #77979, #11906, #197056, #144103, #194929, #112686, #47645, #163508, #64919, #32434, #98502, #164564, #16149, #193856, #110556, #45505, #176557, #82234, #148325, #214324, #166698, #182936, #181857, #151524, #132106, #3093, #185055, #115872, #34552, #201297, #20427, #167762, #17218, #202364, #65956, #33493, #84376, #51887, #54013, #186129, #149379, #36681, #198114, #99566, #87583, #4161, #102768, #21474, #69163, #70231, #962, #150463, #18289, #135283, #83294, #2024, #168823, #68093, #134228, #165630, #52938, #119074, #200237, #183999, #101691, #116936, #199164, #35613, #153655, #100623, #49745, #67027, #118010, #19359, #133164, #50810, #86510, #85439, #152574, #136343, #120153, #37764, #103836, #169885, #209571, #94806 ),
 ( #154721, #39909, #155789, #60143, #71298, #128445, #187203, #11381, #5224, #6303, #61216, #177104, #56149, #93742, #144642, #7373, #122311, #126300, #172039, #159781, #210657, #23632, #192260, #77460, #121233, #88661, #127373, #43922, #110037, #176049, #27642, #38832, #143578, #188268, #106018, #111098, #72378, #104915, #89739, #137410, #73452, #139554, #62285, #193344, #160855, #44989, #204499, #28719, #203430, #205581, #12447, #78525, #55084, #170956, #22556, #194411, #138477, #46053, #112174, #178178, #29794, #95878, #435, #130561, #198651, #115362, #162996, #79596, #47124, #180304, #65448, #165111, #63349, #30868, #66506, #131598, #197600, #181354, #32980, #195489, #99056, #212781, #196551, #50300, #96946, #129508, #64417, #145715, #98005, #48194, #1507, #132645, #34038, #49243, #146763, #148862, #161933, #81729, #182409, #166172, #13523, #113240, #179244, #17761, #14577, #164062, #15641, #16703, #147811, #114306, #116418, #31926, #100111, #82789, #80672, #211713, #213830, #83849, #149938, #67573, #133718, #199723, #51369, #117492, #183483, #35092, #186682, #5771, #151009, #3638, #22021, #55625, #202917, #52431, #23100, #101163, #68648, #119626, #87057, #20959, #170434, #105474, #54561, #188827, #121782, #102240, #4700, #169375, #167248, #153129, #185611, #168312, #53489, #6849, #19909, #152068, #103313, #135820, #154202, #70776, #136890, #39377, #203978, #205057, #120707, #18836, #171507, #38310, #2578, #118557, #134771, #104387, #200779, #88131, #139033, #71850, #36161, #201844, #37242, #137958, #84920, #72927, #184539, #187749, #85994, #69717, #89216, #155268, #56699, #122866, #176849, #42606, #91352, #92427, #207204, #126041, #28462, #143321, #157414, #93487, #10067, #9005, #41534, #75080, #140106, #128194, #144397, #210398, #108713, #159526, #90274, #141193, #40462, #172593, #208259, #58828, #59892, #189892, #7928, #174741, #74014, #24171, #43669, #192004, #142246, #156343, #206133, #94556, #160595, #123924, #11125, #106565, #57763, #62041, #193086, #77203, #107645, #109786, #44737, #173677, #124982, #190942, #175795, #25252, #26314, #209315, #158467, #76143, #27387, #60962, #127119, #110843, #12201, #78271, #30611, #112986, #97752, #1262, #96700, #67320, #95630, #196300, #15387, #194155, #45803, #197350, #47946, #98805, #186, #162747, #79348, #82532, #163811, #181107, #66254, #81481, #149681, #195234, #80413, #148618, #116169, #212528, #63095, #146511, #115110, #111924, #177924, #147558, #164858, #130312, #46872, #213580, #182155, #29539, #65203, #17512, #16451, #64169, #132402, #131355, #198404, #48992, #114061, #32723, #83599, #50046, #180053, #31675, #33785, #178996, #99864, #13274, #165927, #161680, #145465, #211460, #129264, #14320, #35915, #171247, #85736, #21767, #151821, #150760, #87875, #101990, #22843, #3395, #153947, #69464, #2322, #5516, #71596, #168059, #186424, #103063, #19661, #134526, #135569, #18593, #6596, #88958, #155011, #201593, #38063, #183235, #53241, #133464, #51110, #86807, #119370, #152873, #68398, #100914, #185358, #167002, #117235, #136637, #70521, #20714, #34839, #84671, #121527, #39127, #200532, #104133, #199468, #52178, #118303, #137705, #170179, #184290, #202662, #203725, #36980, #169117, #4451, #54312, #120450, #55373, #187497, #105210, #24994, #40198, #108462, #174482, #91097 ),
 ( #72677, #138773, #26058, #157157, #75887, #125791, #123670, #23920, #208009, #206944, #158223, #191753, #124729, #143065, #73753, #107391, #59633, #27127, #173413, #156082, #8749, #9812, #204791, #56444, #190688, #43408, #74831, #57512, #92172, #93233, #122603, #141995, #188566, #109532, #140930, #159266, #175537, #10866, #76940, #42347, #106309, #172332, #90026, #7668, #139848, #205877, #189633, #41282, #58573, #37683, #153573, #117929, #122228, #53936, #154640, #52862, #4081, #171955, #118995, #102686, #120072, #86433, #104834, #186048, #103760, #204416, #6221, #155707, #169809, #183923, #56072, #21399, #167679, #69084, #85361, #87509, #19279, #5143, #89654, #187120, #201221, #152498, #202283, #71218, #35535, #23544, #151443, #55005, #51811, #184974, #38753, #72291, #168744, #137335, #188188, #203352, #20348, #121155, #70152, #170879, #39823, #136263, #22471, #88582, #3015, #135204, #138398, #105931, #7288, #73366, #139471, #36599, #101611, #41973, #25686, #93928, #140558, #107008, #108084, #123300, #141628, #174113, #45175, #44102, #77644, #109158, #190315, #192447, #205500, #125413, #11574, #209760, #57133, #156785, #90723, #61401, #8371, #207637, #59255, #142686, #191379, #91794, #110222, #157851, #27832, #158905, #206572, #189263, #74454, #40902, #24614, #9445, #75516, #43045, #175170, #173032, #76574, #58199, #208696, #176230, #124358, #26757, #126483, #159969, #92858, #10501, #127564, #60323, #143766, #193533, #111287, #177293, #28907, #94992, #161038, #78704, #12633, #145888, #48373, #212960, #144830, #64598, #14764, #130739, #112354, #128626, #147995, #81907, #32101, #194593, #178367, #132829, #50478, #13703, #49417, #210838, #29975, #166356, #82966, #115537, #100289, #214005, #149039, #79776, #163179, #97127, #65627, #162113, #80854, #181532, #146945, #196732, #96060, #131776, #197779, #114485, #180482, #98186, #195674, #63536, #164234, #17946, #47310, #62464, #46237, #15822, #33160, #211899, #129691, #99241, #165290, #16884, #614, #113424, #179430, #66682, #198833, #116599, #182593, #34216, #31051, #123935, #56708, #172602, #188836, #207215, #122875, #157425, #196040, #79072, #90284, #189903, #91365, #58839, #6858, #63892, #40472, #158479, #155278, #156353, #145190, #112715, #206143, #26326, #80139, #9016, #57774, #124994, #107659, #92440, #146242, #173688, #190953, #10079, #106575, #24181, #62822, #42617, #108727, #174753, #211196, #7937, #128982, #41545, #25264, #46597, #74027, #140117, #75092, #72937, #141204, #194961, #212258, #178727, #30342, #96427, #162478, #14050, #139041, #130047, #47674, #113785, #205066, #179787, #31407, #101723, #48724, #99594, #165660, #34582, #214355, #135314, #49774, #200267, #115901, #114838, #51919, #118042, #65985, #150494, #67057, #132135, #98532, #198142, #197086, #185086, #201328, #52966, #17247, #2053, #147291, #181886, #97481, #15123, #50843, #33522, #116970, #32463, #64945, #83324, #131097, #81211, #100654, #166732, #199195, #213323, #180836, #85468, #3124, #164593, #68126, #163538, #16179, #119104, #35644, #134261, #82263, #18323, #167794, #148356, #149411, #993, #84406, #133193, #182967, #184028, #19389, #151556, #69193, #39937, #106045, #170985, #154750, #72406, #87612, #169917, #6334, #58313, #153683, #124468, #152605, #38862, #138506, #36710, #102796, #172068, #104945 ) ),
 .UNSPECIFIED., .T., .F., .F. ) 
 B_SPLINE_SURFACE_WITH_KNOTS ( ( 4, 3, 4 ),
 ( 4, 1, 1, 1, 1, 1, 1, 1, 1, 1, 1, 1, 1, 1, 1, 1, 1, 1, 1, 1, 1, 1, 1, 1, 1, 1, 1, 1, 1, 1, 1, 1, 1, 1, 1, 1, 1, 1, 1, 1, 1, 1, 1, 1, 1, 1, 1, 1, 1, 1, 1, 1, 1, 1, 1, 1, 1, 1, 1, 1, 1, 1, 1, 1, 1, 1, 1, 1, 1, 1, 1, 1, 1, 1, 1, 1, 1, 1, 1, 1, 1, 1, 1, 1, 1, 1, 1, 1, 1, 1, 1, 1, 1, 1, 1, 1, 1, 1, 1, 1, 1, 1, 1, 1, 1, 1, 1, 1, 1, 1, 1, 1, 1, 1, 1, 1, 1, 1, 1, 1, 1, 1, 1, 1, 1, 1, 1, 1, 1, 1, 1, 1, 1, 1, 1, 1, 1, 1, 1, 1, 1, 1, 1, 1, 1, 1, 1, 1, 1, 1, 1, 1, 1, 1, 1, 1, 1, 1, 1, 1, 1, 1, 1, 1, 1, 1, 1, 1, 1, 1, 1, 1, 1, 1, 1, 1, 1, 1, 1, 1, 1, 1, 1, 1, 1, 1, 1, 1, 1, 1, 1, 1, 1, 1, 1, 1, 1, 1, 1, 1, 1, 1, 1, 1, 1, 1, 1, 1, 1, 1, 1, 1, 1, 1, 1, 1, 1, 1, 1, 1, 1, 1, 1, 1, 1, 1, 1, 1, 1, 1, 1, 1, 1, 1, 1, 1, 1, 1, 1, 1, 1, 1, 1, 1, 1, 1, 1, 1, 1, 1, 1, 1, 1, 1, 1, 1, 1, 1, 1, 1, 1, 1, 1, 1, 1, 1, 1, 1, 1, 1, 1, 1, 1, 1, 1, 1, 1, 1, 1, 1, 1, 1, 1, 1, 1, 1, 1, 1, 1, 1, 1, 1, 1, 1, 1, 1, 1, 1, 1, 1, 1, 1, 1, 1, 1, 1, 1, 1, 1, 1, 1, 1, 1, 1, 1, 1, 1, 1, 1, 1, 1, 1, 1, 1, 1, 1, 1, 1, 1, 1, 1, 1, 1, 1, 1, 1, 1, 1, 1, 1, 1, 1, 1, 1, 1, 1, 1, 1, 1, 1, 1, 1, 1, 1, 1, 1, 1, 1, 1, 1, 1, 1, 1, 1, 1, 1, 1, 1, 1, 1, 1, 1, 1, 1, 1, 1, 1, 1, 1, 1, 1, 1, 1, 1, 4 ),
 ( 0.000000000000000000, 0.5000000000000000000, 1.000000000000000000 ),
 ( 0.000000000000000000, 0.002600063085273907840, 0.005208809393482579861, 0.007813201938950280895, 0.01041611862257568050, 0.01302098276518856741, 0.01562474632808895890, 0.01822919105953027183, 0.02083324087635668453, 0.02343728507989274734, 0.02604173773626635227, 0.02864548761524753420, 0.03125016255115702773, 0.03385383280295282959, 0.03645844125268089125, 0.03906229690237970897, 0.04166656525949016115, 0.04427081591349327910, 0.04687468903198145631, 0.04947928942627017462, 0.05208296534865054783, 0.05468764290212216328, 0.05729137561078536528, 0.05989584521530456201, 0.06249987723257615507, 0.06510392926424246607, 0.06770838613806146045, 0.07031213076997053224, 0.07291680575263978503, 0.07552047744215656389, 0.07812508546332513903, 0.08072894086165181837, 0.08333320924388483431, 0.08593745993457323207, 0.08854133291633270453, 0.09114593330519306369, 0.09374960916840779923, 0.09635428668231969807, 0.09895801939011879267, 0.1015624889210437753, 0.1041665209728785957, 0.1067705729027476208, 0.1093750297965602747, 0.1119787743537518920, 0.1145834493281674554, 0.1171871210017138010, 0.1197917289818775377, 0.1223955844170728779, 0.1249998527215379351, 0.1276041034591044177, 0.1302079763611066199, 0.1328125767709825433, 0.1354162526020633861, 0.1380209301064295735, 0.1406246628425296130, 0.1432291323291436380, 0.1458331644451768827, 0.1484372163025670099, 0.1510416732455448496, 0.1536454177576472568, 0.1562500927529001105, 0.1588537644400710158, 0.1614583724083656635, 0.1640622279099430147, 0.1666664961659596600, 0.1692707469797122277, 0.1718746198314790308, 0.1744792202914958457, 0.1770828961200470730, 0.1796875736439581817, 0.1822913064379278192, 0.1848957759094348730, 0.1874998081190861754, 0.1901038599334289314, 0.1927083169547665342, 0.1953120614513534081, 0.1979167364965291054, 0.2005204082269216870, 0.2031250162124720871, 0.2057288718099357372, 0.2083331400468157457, 0.2109373909660553770, 0.2135412637971000893, 0.2161458643363758370, 0.2187495401919937743, 0.2213542177645327069, 0.2239579506459335456, 0.2265624201315297737, 0.2291664524642116896, 0.2317705042649303715, 0.2343749613938155840, 0.2369787059044528299, 0.2395833810286300269, 0.2421870528318344207, 0.2447916608637582536, 0.2473955165866061623, 0.2499997848336539263, 0.2526040358876752157, 0.2552079087275039293, 0.2578125093751503782, 0.2604161852874245509, 0.2630208629376679097, 0.2656245959360551967, 0.2682290654649299166, 0.2708330979500496172, 0.2734371497665608608, 0.2760416070321756732, 0.2786453515864226738, 0.2812500268186742258, 0.2838536987242743503, 0.2864583068316831627, 0.2890621627094078216, 0.2916664309959213219, 0.2942706822140139789, 0.2968745550921262355, 0.2994791558772498252, 0.3020828318757637354, 0.3046875096327826826, 0.3072912427777066413, 0.3098957123790437307, 0.3124997450460035853, 0.3151037969077182255, 0.3177082543392401592, 0.3203119989666507461, 0.3229166743360447622, 0.3255203463736199843, 0.3281249545856204097, 0.3307288106477103140, 0.3333330790029824242, 0.3359373304144318562, 0.3385412033603223403, 0.3411458043120255135, 0.3437494804263583337, 0.3463541583192197293, 0.3489578916402267250, 0.3515623613432052874, 0.3541663942214042238, 0.3567704461577280162, 0.3593749037843310123, 0.3619786485144548260, 0.3645833240500557237, 0.3671869962491814965, 0.3697916045948764219, 0.3723954608708167080, 0.3749997293241361662, 0.3776039809582251716, 0.3802078540013843488, 0.3828124551487663840, 0.3854161314084936785, 0.3880208094662612184, 0.3906245429928945634, 0.3932290128266905938, 0.3958330459455252637, 0.3984370979858605777, 0.4010415558367163569, 0.4036453006990994852, 0.4062499764299690730, 0.4088536488202184072, 0.4114582573287078326, 0.4140621138479816388, 0.4166663824286341855, 0.4192706343146435644, 0.4218745074845589027, 0.4244791088567174686, 0.4270827852914125256, 0.4296874635431477407, 0.4322911973049493040, 0.4348956672987361882, 0.4374997006876018557, 0.4401037528613486738, 0.4427082109656274023, 0.4453119559898139901, 0.4479166319450127998, 0.4505203045559570407, 0.4531249132563394122, 0.4557287700484292658, 0.4583330387856985322, 0.4609372909529084184, 0.4635411642790657205, 0.4661457659050973201, 0.4687494425443319290, 0.4713541210190953512, 0.4739578550456061690, 0.4765623252285562383, 0.4791663589168480009, 0.4817704112534048067, 0.4843748696402766507, 0.4869786148558097882, 0.4895832910643978519, 0.4921869639256079565, 0.4947915728469811647, 0.4973954299413693159, 0.4999996988645384333, 0.5026039513422294602, 0.5052078248541136407, 0.5078124267631153321, 0.5104161036364611714, 0.5130207823633133879, 0.5156245166840751626, 0.5182289870853604707, 0.5208330211024742029, 0.5234370736312391470, 0.5260415323298749390, 0.5286452777662975500, 0.5312499542573357880, 0.5338536273983837122, 0.5364582365698458144, 0.5390620939960163449, 0.5416663631343685559, 0.5442706159518226894, 0.5468744896789192733, 0.5494790918999890028, 0.5520827690370186946, 0.5546874480450217915, 0.5572911826895774468, 0.5598956533383712131, 0.5624996877137050655, 0.5651037404640770756, 0.5677081995036498130, 0.5703119451905063197, 0.5729166219930570403, 0.5755202954435161278, 0.5781249048941674573, 0.5807287626816063364, 0.5833330320644263267, 0.5859372852509285856, 0.5885411592227242084, 0.5911457617849628088, 0.5937494392152512512, 0.5963541185334689798, 0.5989578535313645480, 0.6015623244568418793, 0.6041663592197970001, 0.6067704122211770024, 0.6093748716308627911, 0.6119786175976995590, 0.6145832947408284008, 0.6171869685302752151, 0.6197915782892181591, 0.6223954364674153528, 0.6249997061239902507, 0.6276039597088286515, 0.6302078339548128350, 0.6328124368873246919, 0.6354161146404495586, 0.6380207942979494451, 0.6406245296787346222, 0.6432290009100736228, 0.6458330360900554901, 0.6484370893718474083, 0.6510415491808263511, 0.6536452954571934093, 0.6562499729699700080, 0.6588536471279848872, 0.6614582572243260516, 0.6640621158227759668, 0.6666663857823964534, 0.6692706397948642305, 0.6718745143445301604, 0.6744791176764239893, 0.6770827957819672838, 0.6796874758078212952, 0.6822912116010506622, 0.6848956831674339885, 0.6874997187938534093, 0.6901037723854651640, 0.6927082326229228038, 0.6953119792383747333, 0.6979166571498732763, 0.7005203317060422208, 0.7031249421688929857, 0.7057288012170955804, 0.7083330715090569996, 0.7109373259784533827, 0.7135412008612989077, 0.7161458046216893081, 0.7187494831092385850, 0.7213541635325240176, 0.7239578997677582617, 0.7265623716983737879, 0.7291664078006476757, 0.7317704617314926274, 0.7343749224266207243, 0.7369786694107173242, 0.7395833477500189934, 0.7421870227339337767, 0.7447916335924112952, 0.7473954931198736329, 0.7499997637734774347, 0.7526040187291080930, 0.7552078939746372788, 0.7578124981926457338, 0.7604161770917949870, 0.7630208579415957981, 0.7656245946484027121, 0.7682290669724446408, 0.7708331035799980135, 0.7734371578794957403, 0.7760416190614934928, 0.7786453664438016675, 0.7812500452399944173, 0.7838537206812543623, 0.7864583319644831150, 0.7890621920007202528, 0.7916664630452742157, 0.7942707185164536998, 0.7968745941541772737, 0.7994791988589329268, 0.8020828781992835887, 0.8046875595046918406, 0.8072912967126475436, 0.8098957694593176271, 0.8124998066015838294, 0.8151038612991610144, 0.8177083229972362810, 0.8203120708073305956, 0.8229167500895105958, 0.8255204260177235742, 0.8281250377548363684, 0.8307288983293719120, 0.8333331697941922522, 0.8359374258102438837, 0.8385413018696807885, 0.8411459070903221091, 0.8437495869014844940, 0.8463542686916004643, 0.8489580064302900686, 0.8515624796287988296, 0.8541665173352209761, 0.8567705724603134065, 0.8593750347036837045, 0.8619787829711476057, 0.8645834627684209073, 0.8671871392132045608, 0.8697917514333429745, 0.8723956125757112989, 0.8749998844901232253, 0.8776041410803804288, 0.8802080175910590443, 0.8828126233567346048, 0.8854163036683286858, 0.8880209859722626442, 0.8906247242712825862, 0.8932291979508502067, 0.8958332362508822921, 0.8984372918329353030, 0.9010417546508288078, 0.9036455034052560675, 0.9062501837467389354, 0.9088538607377212308, 0.9114584734700372781, 0.9140623352097841936, 0.9166666076031229071, 0.9192708647969299873, 0.9218747417883903505, 0.9244793481282622682, 0.9270830289699085736, 0.9296877118167798937, 0.9322914507057830091, 0.9348959248956096868, 0.9374999638185942397, 0.9401040198872741005, 0.9427084833090058069, 0.9453122325795346725, 0.9479169134952544207, 0.9505205910598265584, 0.9531252043308329203, 0.9557290667238423909, 0.9583333396063040688, 0.9609375973010293448, 0.9635414750455153499, 0.9661460823481272664, 0.9687497623469286667, 0.9713544456720903941, 0.9739581901020435417, 0.9765626606554614897, 0.9791666924408860551, 0.9817707657828746992, 0.9843752055175947202, 0.9869789906880002128, 0.9895838567146432174, 0.9921867690109741345, 0.9947911791560083428, 0.9973999138825643263, 0.9999999999999998890 ),
 .UNSPECIFIED. ) 
 GEOMETRIC_REPRESENTATION_ITEM ( )  RATIONAL_B_SPLINE_SURFACE ( (
 ( 1.000000000000000222, 1.000000000000000222, 1.000000000000000222, 1.000000000000000222, 1.000000000000000444, 1.000000000000000444, 1.000000000000000222, 1.000000000000000444, 1.000000000000000222, 1.000000000000000444, 1.000000000000000444, 1.000000000000000000, 1.000000000000000222, 1.000000000000000000, 1.000000000000000222, 1.000000000000000222, 1.000000000000000444, 1.000000000000000000, 1.000000000000000444, 1.000000000000000444, 1.000000000000000222, 1.000000000000000222, 1.000000000000000000, 1.000000000000000222, 1.000000000000000000, 1.000000000000000444, 1.000000000000000000, 1.000000000000000444, 1.000000000000000222, 1.000000000000000000, 1.000000000000000666, 1.000000000000000000, 1.000000000000000222, 1.000000000000000666, 1.000000000000000222, 1.000000000000000444, 1.000000000000000222, 1.000000000000000444, 1.000000000000000000, 1.000000000000000444, 1.000000000000000000, 1.000000000000000444, 1.000000000000000000, 1.000000000000000444, 1.000000000000000000, 1.000000000000000222, 1.000000000000000444, 1.000000000000000000, 1.000000000000000444, 1.000000000000000222, 1.000000000000000222, 1.000000000000000444, 1.000000000000000222, 1.000000000000000444, 1.000000000000000222, 1.000000000000000222, 1.000000000000000444, 1.000000000000000444, 1.000000000000000222, 1.000000000000000222, 1.000000000000000444, 1.000000000000000222, 1.000000000000000444, 1.000000000000000000, 1.000000000000000222, 1.000000000000000222, 1.000000000000000222, 1.000000000000000222, 1.000000000000000444, 1.000000000000000000, 0.9999999999999997780, 1.000000000000000444, 1.000000000000000444, 1.000000000000000222, 1.000000000000000222, 1.000000000000000444, 0.9999999999999997780, 1.000000000000000666, 1.000000000000000000, 1.000000000000000000, 1.000000000000000444, 1.000000000000000222, 1.000000000000000222, 0.9999999999999997780, 1.000000000000000222, 1.000000000000000444, 0.9999999999999997780, 1.000000000000000444, 1.000000000000000000, 1.000000000000000000, 1.000000000000000444, 1.000000000000000000, 1.000000000000000444, 1.000000000000000444, 0.9999999999999997780, 1.000000000000000444, 1.000000000000000444, 1.000000000000000444, 1.000000000000000444, 1.000000000000000000, 1.000000000000000444, 1.000000000000000222, 1.000000000000000000, 1.000000000000000444, 1.000000000000000444, 1.000000000000000222, 1.000000000000000000, 1.000000000000000444, 1.000000000000000444, 1.000000000000000000, 1.000000000000000222, 1.000000000000000000, 1.000000000000000444, 1.000000000000000222, 1.000000000000000444, 1.000000000000000222, 1.000000000000000444, 1.000000000000000444, 1.000000000000000000, 1.000000000000000666, 1.000000000000000222, 1.000000000000000222, 1.000000000000000000, 1.000000000000000222, 1.000000000000000222, 1.000000000000000222, 1.000000000000000444, 1.000000000000000222, 1.000000000000000222, 1.000000000000000444, 0.9999999999999997780, 1.000000000000000666, 0.9999999999999997780, 1.000000000000000222, 1.000000000000000000, 1.000000000000000444, 1.000000000000000000, 1.000000000000000444, 1.000000000000000000, 1.000000000000000222, 1.000000000000000222, 1.000000000000000444, 1.000000000000000444, 1.000000000000000222, 1.000000000000000444, 1.000000000000000444, 1.000000000000000000, 1.000000000000000666, 1.000000000000000222, 1.000000000000000222, 1.000000000000000444, 1.000000000000000000, 1.000000000000000222, 1.000000000000000444, 1.000000000000000000, 1.000000000000000222, 1.000000000000000222, 1.000000000000000444, 1.000000000000000222, 1.000000000000000222, 1.000000000000000444, 1.000000000000000000, 1.000000000000000222, 1.000000000000000000, 1.000000000000000444, 1.000000000000000222, 1.000000000000000444, 1.000000000000000222, 1.000000000000000222, 1.000000000000000444, 1.000000000000000000, 1.000000000000000222, 1.000000000000000444, 1.000000000000000000, 1.000000000000000444, 1.000000000000000222, 1.000000000000000444, 1.000000000000000444, 1.000000000000000222, 1.000000000000000222, 1.000000000000000000, 1.000000000000000444, 1.000000000000000444, 1.000000000000000000, 1.000000000000000444, 1.000000000000000222, 1.000000000000000444, 1.000000000000000444, 1.000000000000000222, 1.000000000000000000, 1.000000000000000444, 1.000000000000000222, 1.000000000000000444, 1.000000000000000000, 1.000000000000000444, 1.000000000000000222, 1.000000000000000222, 1.000000000000000444, 1.000000000000000222, 1.000000000000000222, 1.000000000000000222, 1.000000000000000222, 1.000000000000000444, 1.000000000000000000, 1.000000000000000666, 1.000000000000000000, 1.000000000000000222, 1.000000000000000444, 1.000000000000000000, 1.000000000000000222, 1.000000000000000444, 1.000000000000000000, 1.000000000000000666, 0.9999999999999997780, 1.000000000000000222, 1.000000000000000444, 1.000000000000000000, 1.000000000000000444, 1.000000000000000222, 1.000000000000000444, 1.000000000000000000, 1.000000000000000444, 1.000000000000000222, 1.000000000000000222, 1.000000000000000000, 1.000000000000000444, 1.000000000000000222, 1.000000000000000000, 1.000000000000000222, 1.000000000000000222, 1.000000000000000222, 1.000000000000000444, 1.000000000000000000, 1.000000000000000444, 1.000000000000000222, 1.000000000000000222, 1.000000000000000222, 1.000000000000000000, 1.000000000000000666, 1.000000000000000000, 1.000000000000000000, 1.000000000000000222, 1.000000000000000444, 1.000000000000000222, 1.000000000000000444, 0.9999999999999997780, 1.000000000000000444, 1.000000000000000444, 0.9999999999999997780, 1.000000000000000444, 1.000000000000000444, 1.000000000000000444, 1.000000000000000222, 1.000000000000000444, 1.000000000000000444, 1.000000000000000000, 1.000000000000000444, 0.9999999999999997780, 1.000000000000000444, 0.9999999999999997780, 1.000000000000000444, 1.000000000000000000, 1.000000000000000444, 1.000000000000000444, 1.000000000000000444, 1.000000000000000222, 1.000000000000000444, 1.000000000000000444, 1.000000000000000222, 1.000000000000000222, 1.000000000000000000, 1.000000000000000222, 1.000000000000000444, 0.9999999999999997780, 1.000000000000000666, 0.9999999999999997780, 1.000000000000000444, 1.000000000000000222, 1.000000000000000222, 1.000000000000000000, 1.000000000000000222, 1.000000000000000222, 1.000000000000000000, 1.000000000000000000, 1.000000000000000444, 1.000000000000000222, 1.000000000000000444, 0.9999999999999997780, 1.000000000000000444, 1.000000000000000444, 1.000000000000000222, 1.000000000000000444, 1.000000000000000000, 1.000000000000000444, 1.000000000000000444, 0.9999999999999997780, 1.000000000000000444, 1.000000000000000222, 1.000000000000000444, 1.000000000000000222, 1.000000000000000222, 1.000000000000000444, 1.000000000000000000, 1.000000000000000000, 1.000000000000000444, 1.000000000000000444, 1.000000000000000444, 0.9999999999999997780, 1.000000000000000444, 1.000000000000000222, 1.000000000000000222, 1.000000000000000444, 1.000000000000000000, 1.000000000000000444, 1.000000000000000222, 1.000000000000000444, 1.000000000000000000, 1.000000000000000444, 1.000000000000000444, 1.000000000000000444, 1.000000000000000000, 1.000000000000000444, 1.000000000000000000, 1.000000000000000222, 1.000000000000000444, 1.000000000000000444, 1.000000000000000000, 1.000000000000000444, 1.000000000000000444, 1.000000000000000000, 1.000000000000000444, 1.000000000000000222, 1.000000000000000000, 1.000000000000000444, 1.000000000000000222, 1.000000000000000222, 1.000000000000000444, 1.000000000000000444, 1.000000000000000000, 1.000000000000000000, 1.000000000000000444, 1.000000000000000000, 1.000000000000000222, 1.000000000000000444, 1.000000000000000000, 1.000000000000000222, 1.000000000000000444, 0.9999999999999997780, 1.000000000000000444, 1.000000000000000222, 1.000000000000000000, 1.000000000000000444, 1.000000000000000000, 1.000000000000000444, 1.000000000000000444, 1.000000000000000000, 1.000000000000000222, 1.000000000000000222, 1.000000000000000222, 1.000000000000000444, 1.000000000000000222, 1.000000000000000000, 1.000000000000000222, 1.000000000000000444, 1.000000000000000444, 1.000000000000000222, 1.000000000000000444, 1.000000000000000444, 1.000000000000000000, 1.000000000000000000, 1.000000000000000666, 0.9999999999999997780, 1.000000000000000444, 0.9999999999999997780, 1.000000000000000222, 0.9999999999999997780, 1.000000000000000444, 1.000000000000000000, 1.000000000000000222, 1.000000000000000222, 1.000000000000000444, 1.000000000000000000, 1.000000000000000000, 1.000000000000000444, 1.000000000000000000, 1.000000000000000222, 1.000000000000000222),
 ( 0.3333333333333334259, 0.3333333333333334259, 0.3333333333333334814, 0.3333333333333333703, 0.3333333333333335369, 0.3333333333333335369, 0.3333333333333334259, 0.3333333333333334259, 0.3333333333333334259, 0.3333333333333334814, 0.3333333333333334259, 0.3333333333333334259, 0.3333333333333334259, 0.3333333333333334259, 0.3333333333333333148, 0.3333333333333334259, 0.3333333333333334814, 0.3333333333333333703, 0.3333333333333335369, 0.3333333333333335924, 0.3333333333333334259, 0.3333333333333334814, 0.3333333333333333703, 0.3333333333333334259, 0.3333333333333333703, 0.3333333333333334814, 0.3333333333333333703, 0.3333333333333334259, 0.3333333333333333703, 0.3333333333333333703, 0.3333333333333335369, 0.3333333333333334259, 0.3333333333333333703, 0.3333333333333335924, 0.3333333333333334259, 0.3333333333333334259, 0.3333333333333333703, 0.3333333333333334814, 0.3333333333333333703, 0.3333333333333334814, 0.3333333333333333703, 0.3333333333333335369, 0.3333333333333333148, 0.3333333333333334814, 0.3333333333333333703, 0.3333333333333334814, 0.3333333333333334259, 0.3333333333333333703, 0.3333333333333334259, 0.3333333333333334259, 0.3333333333333334814, 0.3333333333333333703, 0.3333333333333335369, 0.3333333333333334259, 0.3333333333333334259, 0.3333333333333334814, 0.3333333333333334259, 0.3333333333333334259, 0.3333333333333333703, 0.3333333333333333703, 0.3333333333333335924, 0.3333333333333334259, 0.3333333333333335369, 0.3333333333333333703, 0.3333333333333333703, 0.3333333333333333703, 0.3333333333333334814, 0.3333333333333333703, 0.3333333333333335369, 0.3333333333333332593, 0.3333333333333333703, 0.3333333333333334259, 0.3333333333333335369, 0.3333333333333334259, 0.3333333333333333703, 0.3333333333333334814, 0.3333333333333333703, 0.3333333333333335369, 0.3333333333333334259, 0.3333333333333333148, 0.3333333333333334814, 0.3333333333333334814, 0.3333333333333334259, 0.3333333333333333148, 0.3333333333333333703, 0.3333333333333334814, 0.3333333333333333703, 0.3333333333333334814, 0.3333333333333333148, 0.3333333333333334259, 0.3333333333333334814, 0.3333333333333333703, 0.3333333333333335369, 0.3333333333333334814, 0.3333333333333333148, 0.3333333333333335369, 0.3333333333333334814, 0.3333333333333334259, 0.3333333333333334814, 0.3333333333333333703, 0.3333333333333334814, 0.3333333333333334259, 0.3333333333333333703, 0.3333333333333334259, 0.3333333333333335369, 0.3333333333333334259, 0.3333333333333334259, 0.3333333333333334814, 0.3333333333333335369, 0.3333333333333333148, 0.3333333333333334259, 0.3333333333333333148, 0.3333333333333335924, 0.3333333333333334259, 0.3333333333333334814, 0.3333333333333333703, 0.3333333333333334814, 0.3333333333333334259, 0.3333333333333333703, 0.3333333333333335924, 0.3333333333333334259, 0.3333333333333334259, 0.3333333333333333703, 0.3333333333333334259, 0.3333333333333333703, 0.3333333333333333703, 0.3333333333333335369, 0.3333333333333334259, 0.3333333333333333703, 0.3333333333333334814, 0.3333333333333333148, 0.3333333333333335924, 0.3333333333333333148, 0.3333333333333334259, 0.3333333333333333148, 0.3333333333333335924, 0.3333333333333333703, 0.3333333333333335369, 0.3333333333333333148, 0.3333333333333334259, 0.3333333333333334814, 0.3333333333333334259, 0.3333333333333334259, 0.3333333333333334259, 0.3333333333333334259, 0.3333333333333334259, 0.3333333333333334259, 0.3333333333333334814, 0.3333333333333334259, 0.3333333333333333703, 0.3333333333333334814, 0.3333333333333333148, 0.3333333333333334259, 0.3333333333333334814, 0.3333333333333334259, 0.3333333333333333703, 0.3333333333333334259, 0.3333333333333334814, 0.3333333333333333703, 0.3333333333333334259, 0.3333333333333334814, 0.3333333333333333703, 0.3333333333333333703, 0.3333333333333333703, 0.3333333333333335369, 0.3333333333333333703, 0.3333333333333334814, 0.3333333333333334259, 0.3333333333333333703, 0.3333333333333334814, 0.3333333333333333703, 0.3333333333333334259, 0.3333333333333335369, 0.3333333333333333703, 0.3333333333333334259, 0.3333333333333334814, 0.3333333333333334259, 0.3333333333333335924, 0.3333333333333333703, 0.3333333333333334259, 0.3333333333333333148, 0.3333333333333335369, 0.3333333333333334259, 0.3333333333333334259, 0.3333333333333334259, 0.3333333333333333703, 0.3333333333333335369, 0.3333333333333334259, 0.3333333333333333703, 0.3333333333333334259, 0.3333333333333334259, 0.3333333333333333703, 0.3333333333333335369, 0.3333333333333333703, 0.3333333333333335369, 0.3333333333333333703, 0.3333333333333334814, 0.3333333333333334259, 0.3333333333333333703, 0.3333333333333334259, 0.3333333333333333703, 0.3333333333333334814, 0.3333333333333334259, 0.3333333333333333703, 0.3333333333333335369, 0.3333333333333333703, 0.3333333333333333703, 0.3333333333333334814, 0.3333333333333333703, 0.3333333333333333148, 0.3333333333333335924, 0.3333333333333333148, 0.3333333333333335924, 0.3333333333333332593, 0.3333333333333334814, 0.3333333333333334814, 0.3333333333333334259, 0.3333333333333334259, 0.3333333333333334814, 0.3333333333333334259, 0.3333333333333333703, 0.3333333333333335369, 0.3333333333333334259, 0.3333333333333334814, 0.3333333333333333703, 0.3333333333333334259, 0.3333333333333333703, 0.3333333333333334814, 0.3333333333333333703, 0.3333333333333335369, 0.3333333333333333148, 0.3333333333333335924, 0.3333333333333333703, 0.3333333333333334259, 0.3333333333333333703, 0.3333333333333334259, 0.3333333333333333703, 0.3333333333333333703, 0.3333333333333335924, 0.3333333333333334259, 0.3333333333333333148, 0.3333333333333334814, 0.3333333333333335369, 0.3333333333333333703, 0.3333333333333334814, 0.3333333333333333703, 0.3333333333333334259, 0.3333333333333335369, 0.3333333333333333148, 0.3333333333333334814, 0.3333333333333334814, 0.3333333333333333703, 0.3333333333333334259, 0.3333333333333334259, 0.3333333333333335369, 0.3333333333333333148, 0.3333333333333335369, 0.3333333333333333148, 0.3333333333333335369, 0.3333333333333332593, 0.3333333333333335924, 0.3333333333333333148, 0.3333333333333335369, 0.3333333333333335369, 0.3333333333333334814, 0.3333333333333334259, 0.3333333333333334814, 0.3333333333333334814, 0.3333333333333334259, 0.3333333333333334259, 0.3333333333333334259, 0.3333333333333334814, 0.3333333333333334259, 0.3333333333333333703, 0.3333333333333334814, 0.3333333333333333703, 0.3333333333333335369, 0.3333333333333333703, 0.3333333333333334259, 0.3333333333333333148, 0.3333333333333334259, 0.3333333333333334259, 0.3333333333333333703, 0.3333333333333333703, 0.3333333333333335924, 0.3333333333333334259, 0.3333333333333335369, 0.3333333333333333148, 0.3333333333333335369, 0.3333333333333334814, 0.3333333333333334259, 0.3333333333333334814, 0.3333333333333334259, 0.3333333333333333703, 0.3333333333333335369, 0.3333333333333333148, 0.3333333333333335369, 0.3333333333333333703, 0.3333333333333335369, 0.3333333333333333703, 0.3333333333333334814, 0.3333333333333334259, 0.3333333333333333703, 0.3333333333333334259, 0.3333333333333333703, 0.3333333333333335924, 0.3333333333333334259, 0.3333333333333333148, 0.3333333333333334259, 0.3333333333333334259, 0.3333333333333334259, 0.3333333333333335924, 0.3333333333333333703, 0.3333333333333334259, 0.3333333333333334259, 0.3333333333333335369, 0.3333333333333333703, 0.3333333333333334814, 0.3333333333333334814, 0.3333333333333334814, 0.3333333333333333703, 0.3333333333333334814, 0.3333333333333333148, 0.3333333333333335369, 0.3333333333333334259, 0.3333333333333334814, 0.3333333333333333703, 0.3333333333333334259, 0.3333333333333334259, 0.3333333333333334259, 0.3333333333333334259, 0.3333333333333333703, 0.3333333333333333703, 0.3333333333333334814, 0.3333333333333333703, 0.3333333333333334259, 0.3333333333333334814, 0.3333333333333334259, 0.3333333333333334259, 0.3333333333333333703, 0.3333333333333334814, 0.3333333333333333703, 0.3333333333333334259, 0.3333333333333335369, 0.3333333333333333148, 0.3333333333333333703, 0.3333333333333334814, 0.3333333333333333148, 0.3333333333333334259, 0.3333333333333333703, 0.3333333333333333703, 0.3333333333333334814, 0.3333333333333333703, 0.3333333333333334259, 0.3333333333333334814, 0.3333333333333333703, 0.3333333333333334259, 0.3333333333333334259, 0.3333333333333334259, 0.3333333333333335369, 0.3333333333333334259, 0.3333333333333334259, 0.3333333333333333703, 0.3333333333333334259, 0.3333333333333334259, 0.3333333333333334259, 0.3333333333333334814, 0.3333333333333335369, 0.3333333333333333148, 0.3333333333333333703, 0.3333333333333335924, 0.3333333333333333148, 0.3333333333333334259, 0.3333333333333334259, 0.3333333333333333703, 0.3333333333333333148, 0.3333333333333335369, 0.3333333333333334259, 0.3333333333333333703, 0.3333333333333334814, 0.3333333333333334259, 0.3333333333333334259, 0.3333333333333333148, 0.3333333333333335369, 0.3333333333333333703, 0.3333333333333334259, 0.3333333333333334259),
 ( 0.3333333333333334259, 0.3333333333333334259, 0.3333333333333334814, 0.3333333333333333703, 0.3333333333333335369, 0.3333333333333335369, 0.3333333333333334259, 0.3333333333333334259, 0.3333333333333334259, 0.3333333333333334814, 0.3333333333333334259, 0.3333333333333334259, 0.3333333333333334259, 0.3333333333333334259, 0.3333333333333333148, 0.3333333333333334259, 0.3333333333333334814, 0.3333333333333333703, 0.3333333333333335369, 0.3333333333333335924, 0.3333333333333334259, 0.3333333333333334814, 0.3333333333333333703, 0.3333333333333334259, 0.3333333333333333703, 0.3333333333333334814, 0.3333333333333333703, 0.3333333333333334259, 0.3333333333333333703, 0.3333333333333333703, 0.3333333333333335369, 0.3333333333333334259, 0.3333333333333333703, 0.3333333333333335924, 0.3333333333333334259, 0.3333333333333334259, 0.3333333333333333703, 0.3333333333333334814, 0.3333333333333333703, 0.3333333333333334814, 0.3333333333333333703, 0.3333333333333335369, 0.3333333333333333148, 0.3333333333333334814, 0.3333333333333333703, 0.3333333333333334814, 0.3333333333333334259, 0.3333333333333333703, 0.3333333333333334259, 0.3333333333333334259, 0.3333333333333334814, 0.3333333333333333703, 0.3333333333333335369, 0.3333333333333334259, 0.3333333333333334259, 0.3333333333333334814, 0.3333333333333334259, 0.3333333333333334259, 0.3333333333333333703, 0.3333333333333333703, 0.3333333333333335924, 0.3333333333333334259, 0.3333333333333335369, 0.3333333333333333703, 0.3333333333333333703, 0.3333333333333333703, 0.3333333333333334814, 0.3333333333333333703, 0.3333333333333335369, 0.3333333333333332593, 0.3333333333333333703, 0.3333333333333334259, 0.3333333333333335369, 0.3333333333333334259, 0.3333333333333333703, 0.3333333333333334814, 0.3333333333333333703, 0.3333333333333335369, 0.3333333333333334259, 0.3333333333333333148, 0.3333333333333334814, 0.3333333333333334814, 0.3333333333333334259, 0.3333333333333333148, 0.3333333333333333703, 0.3333333333333334814, 0.3333333333333333703, 0.3333333333333334814, 0.3333333333333333148, 0.3333333333333334259, 0.3333333333333334814, 0.3333333333333333703, 0.3333333333333335369, 0.3333333333333334814, 0.3333333333333333148, 0.3333333333333335369, 0.3333333333333334814, 0.3333333333333334259, 0.3333333333333334814, 0.3333333333333333703, 0.3333333333333334814, 0.3333333333333334259, 0.3333333333333333703, 0.3333333333333334259, 0.3333333333333335369, 0.3333333333333334259, 0.3333333333333334259, 0.3333333333333334814, 0.3333333333333335369, 0.3333333333333333148, 0.3333333333333334259, 0.3333333333333333148, 0.3333333333333335924, 0.3333333333333334259, 0.3333333333333334814, 0.3333333333333333703, 0.3333333333333334814, 0.3333333333333334259, 0.3333333333333333703, 0.3333333333333335924, 0.3333333333333334259, 0.3333333333333334259, 0.3333333333333333703, 0.3333333333333334259, 0.3333333333333333703, 0.3333333333333333703, 0.3333333333333335369, 0.3333333333333334259, 0.3333333333333333703, 0.3333333333333334814, 0.3333333333333333148, 0.3333333333333335924, 0.3333333333333333148, 0.3333333333333334259, 0.3333333333333333148, 0.3333333333333335924, 0.3333333333333333703, 0.3333333333333335369, 0.3333333333333333148, 0.3333333333333334259, 0.3333333333333334814, 0.3333333333333334259, 0.3333333333333334259, 0.3333333333333334259, 0.3333333333333334259, 0.3333333333333334259, 0.3333333333333334259, 0.3333333333333334814, 0.3333333333333334259, 0.3333333333333333703, 0.3333333333333334814, 0.3333333333333333148, 0.3333333333333334259, 0.3333333333333334814, 0.3333333333333334259, 0.3333333333333333703, 0.3333333333333334259, 0.3333333333333334814, 0.3333333333333333703, 0.3333333333333334259, 0.3333333333333334814, 0.3333333333333333703, 0.3333333333333333703, 0.3333333333333333703, 0.3333333333333335369, 0.3333333333333333703, 0.3333333333333334814, 0.3333333333333334259, 0.3333333333333333703, 0.3333333333333334814, 0.3333333333333333703, 0.3333333333333334259, 0.3333333333333335369, 0.3333333333333333703, 0.3333333333333334259, 0.3333333333333334814, 0.3333333333333334259, 0.3333333333333335924, 0.3333333333333333703, 0.3333333333333334259, 0.3333333333333333148, 0.3333333333333335369, 0.3333333333333334259, 0.3333333333333334259, 0.3333333333333334259, 0.3333333333333333703, 0.3333333333333335369, 0.3333333333333334259, 0.3333333333333333703, 0.3333333333333334259, 0.3333333333333334259, 0.3333333333333333703, 0.3333333333333335369, 0.3333333333333333703, 0.3333333333333335369, 0.3333333333333333703, 0.3333333333333334814, 0.3333333333333334259, 0.3333333333333333703, 0.3333333333333334259, 0.3333333333333333703, 0.3333333333333334814, 0.3333333333333334259, 0.3333333333333333703, 0.3333333333333335369, 0.3333333333333333703, 0.3333333333333333703, 0.3333333333333334814, 0.3333333333333333703, 0.3333333333333333148, 0.3333333333333335924, 0.3333333333333333148, 0.3333333333333335924, 0.3333333333333332593, 0.3333333333333334814, 0.3333333333333334814, 0.3333333333333334259, 0.3333333333333334259, 0.3333333333333334814, 0.3333333333333334259, 0.3333333333333333703, 0.3333333333333335369, 0.3333333333333334259, 0.3333333333333334814, 0.3333333333333333703, 0.3333333333333334259, 0.3333333333333333703, 0.3333333333333334814, 0.3333333333333333703, 0.3333333333333335369, 0.3333333333333333148, 0.3333333333333335924, 0.3333333333333333703, 0.3333333333333334259, 0.3333333333333333703, 0.3333333333333334259, 0.3333333333333333703, 0.3333333333333333703, 0.3333333333333335924, 0.3333333333333334259, 0.3333333333333333148, 0.3333333333333334814, 0.3333333333333335369, 0.3333333333333333703, 0.3333333333333334814, 0.3333333333333333703, 0.3333333333333334259, 0.3333333333333335369, 0.3333333333333333148, 0.3333333333333334814, 0.3333333333333334814, 0.3333333333333333703, 0.3333333333333334259, 0.3333333333333334259, 0.3333333333333335369, 0.3333333333333333148, 0.3333333333333335369, 0.3333333333333333148, 0.3333333333333335369, 0.3333333333333332593, 0.3333333333333335924, 0.3333333333333333148, 0.3333333333333335369, 0.3333333333333335369, 0.3333333333333334814, 0.3333333333333334259, 0.3333333333333334814, 0.3333333333333334814, 0.3333333333333334259, 0.3333333333333334259, 0.3333333333333334259, 0.3333333333333334814, 0.3333333333333334259, 0.3333333333333333703, 0.3333333333333334814, 0.3333333333333333703, 0.3333333333333335369, 0.3333333333333333703, 0.3333333333333334259, 0.3333333333333333148, 0.3333333333333334259, 0.3333333333333334259, 0.3333333333333333703, 0.3333333333333333703, 0.3333333333333335924, 0.3333333333333334259, 0.3333333333333335369, 0.3333333333333333148, 0.3333333333333335369, 0.3333333333333334814, 0.3333333333333334259, 0.3333333333333334814, 0.3333333333333334259, 0.3333333333333333703, 0.3333333333333335369, 0.3333333333333333148, 0.3333333333333335369, 0.3333333333333333703, 0.3333333333333335369, 0.3333333333333333703, 0.3333333333333334814, 0.3333333333333334259, 0.3333333333333333703, 0.3333333333333334259, 0.3333333333333333703, 0.3333333333333335924, 0.3333333333333334259, 0.3333333333333333148, 0.3333333333333334259, 0.3333333333333334259, 0.3333333333333334259, 0.3333333333333335924, 0.3333333333333333703, 0.3333333333333334259, 0.3333333333333334259, 0.3333333333333335369, 0.3333333333333333703, 0.3333333333333334814, 0.3333333333333334814, 0.3333333333333334814, 0.3333333333333333703, 0.3333333333333334814, 0.3333333333333333148, 0.3333333333333335369, 0.3333333333333334259, 0.3333333333333334814, 0.3333333333333333703, 0.3333333333333334259, 0.3333333333333334259, 0.3333333333333334259, 0.3333333333333334259, 0.3333333333333333703, 0.3333333333333333703, 0.3333333333333334814, 0.3333333333333333703, 0.3333333333333334259, 0.3333333333333334814, 0.3333333333333334259, 0.3333333333333334259, 0.3333333333333333703, 0.3333333333333334814, 0.3333333333333333703, 0.3333333333333334259, 0.3333333333333335369, 0.3333333333333333148, 0.3333333333333333703, 0.3333333333333334814, 0.3333333333333333148, 0.3333333333333334259, 0.3333333333333333703, 0.3333333333333333703, 0.3333333333333334814, 0.3333333333333333703, 0.3333333333333334259, 0.3333333333333334814, 0.3333333333333333703, 0.3333333333333334259, 0.3333333333333334259, 0.3333333333333334259, 0.3333333333333335369, 0.3333333333333334259, 0.3333333333333334259, 0.3333333333333333703, 0.3333333333333334259, 0.3333333333333334259, 0.3333333333333334259, 0.3333333333333334814, 0.3333333333333335369, 0.3333333333333333148, 0.3333333333333333703, 0.3333333333333335924, 0.3333333333333333148, 0.3333333333333334259, 0.3333333333333334259, 0.3333333333333333703, 0.3333333333333333148, 0.3333333333333335369, 0.3333333333333334259, 0.3333333333333333703, 0.3333333333333334814, 0.3333333333333334259, 0.3333333333333334259, 0.3333333333333333148, 0.3333333333333335369, 0.3333333333333333703, 0.3333333333333334259, 0.3333333333333334259),
 ( 1.000000000000000222, 1.000000000000000222, 1.000000000000000222, 1.000000000000000222, 1.000000000000000444, 1.000000000000000444, 1.000000000000000222, 1.000000000000000444, 1.000000000000000222, 1.000000000000000444, 1.000000000000000444, 1.000000000000000000, 1.000000000000000222, 1.000000000000000000, 1.000000000000000222, 1.000000000000000222, 1.000000000000000444, 1.000000000000000000, 1.000000000000000444, 1.000000000000000444, 1.000000000000000222, 1.000000000000000222, 1.000000000000000000, 1.000000000000000222, 1.000000000000000000, 1.000000000000000444, 1.000000000000000000, 1.000000000000000444, 1.000000000000000222, 1.000000000000000000, 1.000000000000000666, 1.000000000000000000, 1.000000000000000222, 1.000000000000000666, 1.000000000000000222, 1.000000000000000444, 1.000000000000000222, 1.000000000000000444, 1.000000000000000000, 1.000000000000000444, 1.000000000000000000, 1.000000000000000444, 1.000000000000000000, 1.000000000000000444, 1.000000000000000000, 1.000000000000000222, 1.000000000000000444, 1.000000000000000000, 1.000000000000000444, 1.000000000000000222, 1.000000000000000222, 1.000000000000000444, 1.000000000000000222, 1.000000000000000444, 1.000000000000000222, 1.000000000000000222, 1.000000000000000444, 1.000000000000000444, 1.000000000000000222, 1.000000000000000222, 1.000000000000000444, 1.000000000000000222, 1.000000000000000444, 1.000000000000000000, 1.000000000000000222, 1.000000000000000222, 1.000000000000000222, 1.000000000000000222, 1.000000000000000444, 1.000000000000000000, 0.9999999999999997780, 1.000000000000000444, 1.000000000000000444, 1.000000000000000222, 1.000000000000000222, 1.000000000000000444, 0.9999999999999997780, 1.000000000000000666, 1.000000000000000000, 1.000000000000000000, 1.000000000000000444, 1.000000000000000222, 1.000000000000000222, 0.9999999999999997780, 1.000000000000000222, 1.000000000000000444, 0.9999999999999997780, 1.000000000000000444, 1.000000000000000000, 1.000000000000000000, 1.000000000000000444, 1.000000000000000000, 1.000000000000000444, 1.000000000000000444, 0.9999999999999997780, 1.000000000000000444, 1.000000000000000444, 1.000000000000000444, 1.000000000000000444, 1.000000000000000000, 1.000000000000000444, 1.000000000000000222, 1.000000000000000000, 1.000000000000000444, 1.000000000000000444, 1.000000000000000222, 1.000000000000000000, 1.000000000000000444, 1.000000000000000444, 1.000000000000000000, 1.000000000000000222, 1.000000000000000000, 1.000000000000000444, 1.000000000000000222, 1.000000000000000444, 1.000000000000000222, 1.000000000000000444, 1.000000000000000444, 1.000000000000000000, 1.000000000000000666, 1.000000000000000222, 1.000000000000000222, 1.000000000000000000, 1.000000000000000222, 1.000000000000000222, 1.000000000000000222, 1.000000000000000444, 1.000000000000000222, 1.000000000000000222, 1.000000000000000444, 0.9999999999999997780, 1.000000000000000666, 0.9999999999999997780, 1.000000000000000222, 1.000000000000000000, 1.000000000000000444, 1.000000000000000000, 1.000000000000000444, 1.000000000000000000, 1.000000000000000222, 1.000000000000000222, 1.000000000000000444, 1.000000000000000444, 1.000000000000000222, 1.000000000000000444, 1.000000000000000444, 1.000000000000000000, 1.000000000000000666, 1.000000000000000222, 1.000000000000000222, 1.000000000000000444, 1.000000000000000000, 1.000000000000000222, 1.000000000000000444, 1.000000000000000000, 1.000000000000000222, 1.000000000000000222, 1.000000000000000444, 1.000000000000000222, 1.000000000000000222, 1.000000000000000444, 1.000000000000000000, 1.000000000000000222, 1.000000000000000000, 1.000000000000000444, 1.000000000000000222, 1.000000000000000444, 1.000000000000000222, 1.000000000000000222, 1.000000000000000444, 1.000000000000000000, 1.000000000000000222, 1.000000000000000444, 1.000000000000000000, 1.000000000000000444, 1.000000000000000222, 1.000000000000000444, 1.000000000000000444, 1.000000000000000222, 1.000000000000000222, 1.000000000000000000, 1.000000000000000444, 1.000000000000000444, 1.000000000000000000, 1.000000000000000444, 1.000000000000000222, 1.000000000000000444, 1.000000000000000444, 1.000000000000000222, 1.000000000000000000, 1.000000000000000444, 1.000000000000000222, 1.000000000000000444, 1.000000000000000000, 1.000000000000000444, 1.000000000000000222, 1.000000000000000222, 1.000000000000000444, 1.000000000000000222, 1.000000000000000222, 1.000000000000000222, 1.000000000000000222, 1.000000000000000444, 1.000000000000000000, 1.000000000000000666, 1.000000000000000000, 1.000000000000000222, 1.000000000000000444, 1.000000000000000000, 1.000000000000000222, 1.000000000000000444, 1.000000000000000000, 1.000000000000000666, 0.9999999999999997780, 1.000000000000000222, 1.000000000000000444, 1.000000000000000000, 1.000000000000000444, 1.000000000000000222, 1.000000000000000444, 1.000000000000000000, 1.000000000000000444, 1.000000000000000222, 1.000000000000000222, 1.000000000000000000, 1.000000000000000444, 1.000000000000000222, 1.000000000000000000, 1.000000000000000222, 1.000000000000000222, 1.000000000000000222, 1.000000000000000444, 1.000000000000000000, 1.000000000000000444, 1.000000000000000222, 1.000000000000000222, 1.000000000000000222, 1.000000000000000000, 1.000000000000000666, 1.000000000000000000, 1.000000000000000000, 1.000000000000000222, 1.000000000000000444, 1.000000000000000222, 1.000000000000000444, 0.9999999999999997780, 1.000000000000000444, 1.000000000000000444, 0.9999999999999997780, 1.000000000000000444, 1.000000000000000444, 1.000000000000000444, 1.000000000000000222, 1.000000000000000444, 1.000000000000000444, 1.000000000000000000, 1.000000000000000444, 0.9999999999999997780, 1.000000000000000444, 0.9999999999999997780, 1.000000000000000444, 1.000000000000000000, 1.000000000000000444, 1.000000000000000444, 1.000000000000000444, 1.000000000000000222, 1.000000000000000444, 1.000000000000000444, 1.000000000000000222, 1.000000000000000222, 1.000000000000000000, 1.000000000000000222, 1.000000000000000444, 0.9999999999999997780, 1.000000000000000666, 0.9999999999999997780, 1.000000000000000444, 1.000000000000000222, 1.000000000000000222, 1.000000000000000000, 1.000000000000000222, 1.000000000000000222, 1.000000000000000000, 1.000000000000000000, 1.000000000000000444, 1.000000000000000222, 1.000000000000000444, 0.9999999999999997780, 1.000000000000000444, 1.000000000000000444, 1.000000000000000222, 1.000000000000000444, 1.000000000000000000, 1.000000000000000444, 1.000000000000000444, 0.9999999999999997780, 1.000000000000000444, 1.000000000000000222, 1.000000000000000444, 1.000000000000000222, 1.000000000000000222, 1.000000000000000444, 1.000000000000000000, 1.000000000000000000, 1.000000000000000444, 1.000000000000000444, 1.000000000000000444, 0.9999999999999997780, 1.000000000000000444, 1.000000000000000222, 1.000000000000000222, 1.000000000000000444, 1.000000000000000000, 1.000000000000000444, 1.000000000000000222, 1.000000000000000444, 1.000000000000000000, 1.000000000000000444, 1.000000000000000444, 1.000000000000000444, 1.000000000000000000, 1.000000000000000444, 1.000000000000000000, 1.000000000000000222, 1.000000000000000444, 1.000000000000000444, 1.000000000000000000, 1.000000000000000444, 1.000000000000000444, 1.000000000000000000, 1.000000000000000444, 1.000000000000000222, 1.000000000000000000, 1.000000000000000444, 1.000000000000000222, 1.000000000000000222, 1.000000000000000444, 1.000000000000000444, 1.000000000000000000, 1.000000000000000000, 1.000000000000000444, 1.000000000000000000, 1.000000000000000222, 1.000000000000000444, 1.000000000000000000, 1.000000000000000222, 1.000000000000000444, 0.9999999999999997780, 1.000000000000000444, 1.000000000000000222, 1.000000000000000000, 1.000000000000000444, 1.000000000000000000, 1.000000000000000444, 1.000000000000000444, 1.000000000000000000, 1.000000000000000222, 1.000000000000000222, 1.000000000000000222, 1.000000000000000444, 1.000000000000000222, 1.000000000000000000, 1.000000000000000222, 1.000000000000000444, 1.000000000000000444, 1.000000000000000222, 1.000000000000000444, 1.000000000000000444, 1.000000000000000000, 1.000000000000000000, 1.000000000000000666, 0.9999999999999997780, 1.000000000000000444, 0.9999999999999997780, 1.000000000000000222, 0.9999999999999997780, 1.000000000000000444, 1.000000000000000000, 1.000000000000000222, 1.000000000000000222, 1.000000000000000444, 1.000000000000000000, 1.000000000000000000, 1.000000000000000444, 1.000000000000000000, 1.000000000000000222, 1.000000000000000222),
 ( 0.3333333333333334259, 0.3333333333333334259, 0.3333333333333334814, 0.3333333333333333703, 0.3333333333333335369, 0.3333333333333335369, 0.3333333333333334259, 0.3333333333333334259, 0.3333333333333334259, 0.3333333333333334814, 0.3333333333333334259, 0.3333333333333334259, 0.3333333333333334259, 0.3333333333333334259, 0.3333333333333333148, 0.3333333333333334259, 0.3333333333333334814, 0.3333333333333333703, 0.3333333333333335369, 0.3333333333333335924, 0.3333333333333334259, 0.3333333333333334814, 0.3333333333333333703, 0.3333333333333334259, 0.3333333333333333703, 0.3333333333333334814, 0.3333333333333333703, 0.3333333333333334259, 0.3333333333333333703, 0.3333333333333333703, 0.3333333333333335369, 0.3333333333333334259, 0.3333333333333333703, 0.3333333333333335924, 0.3333333333333334259, 0.3333333333333334259, 0.3333333333333333703, 0.3333333333333334814, 0.3333333333333333703, 0.3333333333333334814, 0.3333333333333333703, 0.3333333333333335369, 0.3333333333333333148, 0.3333333333333334814, 0.3333333333333333703, 0.3333333333333334814, 0.3333333333333334259, 0.3333333333333333703, 0.3333333333333334259, 0.3333333333333334259, 0.3333333333333334814, 0.3333333333333333703, 0.3333333333333335369, 0.3333333333333334259, 0.3333333333333334259, 0.3333333333333334814, 0.3333333333333334259, 0.3333333333333334259, 0.3333333333333333703, 0.3333333333333333703, 0.3333333333333335924, 0.3333333333333334259, 0.3333333333333335369, 0.3333333333333333703, 0.3333333333333333703, 0.3333333333333333703, 0.3333333333333334814, 0.3333333333333333703, 0.3333333333333335369, 0.3333333333333332593, 0.3333333333333333703, 0.3333333333333334259, 0.3333333333333335369, 0.3333333333333334259, 0.3333333333333333703, 0.3333333333333334814, 0.3333333333333333703, 0.3333333333333335369, 0.3333333333333334259, 0.3333333333333333148, 0.3333333333333334814, 0.3333333333333334814, 0.3333333333333334259, 0.3333333333333333148, 0.3333333333333333703, 0.3333333333333334814, 0.3333333333333333703, 0.3333333333333334814, 0.3333333333333333148, 0.3333333333333334259, 0.3333333333333334814, 0.3333333333333333703, 0.3333333333333335369, 0.3333333333333334814, 0.3333333333333333148, 0.3333333333333335369, 0.3333333333333334814, 0.3333333333333334259, 0.3333333333333334814, 0.3333333333333333703, 0.3333333333333334814, 0.3333333333333334259, 0.3333333333333333703, 0.3333333333333334259, 0.3333333333333335369, 0.3333333333333334259, 0.3333333333333334259, 0.3333333333333334814, 0.3333333333333335369, 0.3333333333333333148, 0.3333333333333334259, 0.3333333333333333148, 0.3333333333333335924, 0.3333333333333334259, 0.3333333333333334814, 0.3333333333333333703, 0.3333333333333334814, 0.3333333333333334259, 0.3333333333333333703, 0.3333333333333335924, 0.3333333333333334259, 0.3333333333333334259, 0.3333333333333333703, 0.3333333333333334259, 0.3333333333333333703, 0.3333333333333333703, 0.3333333333333335369, 0.3333333333333334259, 0.3333333333333333703, 0.3333333333333334814, 0.3333333333333333148, 0.3333333333333335924, 0.3333333333333333148, 0.3333333333333334259, 0.3333333333333333148, 0.3333333333333335924, 0.3333333333333333703, 0.3333333333333335369, 0.3333333333333333148, 0.3333333333333334259, 0.3333333333333334814, 0.3333333333333334259, 0.3333333333333334259, 0.3333333333333334259, 0.3333333333333334259, 0.3333333333333334259, 0.3333333333333334259, 0.3333333333333334814, 0.3333333333333334259, 0.3333333333333333703, 0.3333333333333334814, 0.3333333333333333148, 0.3333333333333334259, 0.3333333333333334814, 0.3333333333333334259, 0.3333333333333333703, 0.3333333333333334259, 0.3333333333333334814, 0.3333333333333333703, 0.3333333333333334259, 0.3333333333333334814, 0.3333333333333333703, 0.3333333333333333703, 0.3333333333333333703, 0.3333333333333335369, 0.3333333333333333703, 0.3333333333333334814, 0.3333333333333334259, 0.3333333333333333703, 0.3333333333333334814, 0.3333333333333333703, 0.3333333333333334259, 0.3333333333333335369, 0.3333333333333333703, 0.3333333333333334259, 0.3333333333333334814, 0.3333333333333334259, 0.3333333333333335924, 0.3333333333333333703, 0.3333333333333334259, 0.3333333333333333148, 0.3333333333333335369, 0.3333333333333334259, 0.3333333333333334259, 0.3333333333333334259, 0.3333333333333333703, 0.3333333333333335369, 0.3333333333333334259, 0.3333333333333333703, 0.3333333333333334259, 0.3333333333333334259, 0.3333333333333333703, 0.3333333333333335369, 0.3333333333333333703, 0.3333333333333335369, 0.3333333333333333703, 0.3333333333333334814, 0.3333333333333334259, 0.3333333333333333703, 0.3333333333333334259, 0.3333333333333333703, 0.3333333333333334814, 0.3333333333333334259, 0.3333333333333333703, 0.3333333333333335369, 0.3333333333333333703, 0.3333333333333333703, 0.3333333333333334814, 0.3333333333333333703, 0.3333333333333333148, 0.3333333333333335924, 0.3333333333333333148, 0.3333333333333335924, 0.3333333333333332593, 0.3333333333333334814, 0.3333333333333334814, 0.3333333333333334259, 0.3333333333333334259, 0.3333333333333334814, 0.3333333333333334259, 0.3333333333333333703, 0.3333333333333335369, 0.3333333333333334259, 0.3333333333333334814, 0.3333333333333333703, 0.3333333333333334259, 0.3333333333333333703, 0.3333333333333334814, 0.3333333333333333703, 0.3333333333333335369, 0.3333333333333333148, 0.3333333333333335924, 0.3333333333333333703, 0.3333333333333334259, 0.3333333333333333703, 0.3333333333333334259, 0.3333333333333333703, 0.3333333333333333703, 0.3333333333333335924, 0.3333333333333334259, 0.3333333333333333148, 0.3333333333333334814, 0.3333333333333335369, 0.3333333333333333703, 0.3333333333333334814, 0.3333333333333333703, 0.3333333333333334259, 0.3333333333333335369, 0.3333333333333333148, 0.3333333333333334814, 0.3333333333333334814, 0.3333333333333333703, 0.3333333333333334259, 0.3333333333333334259, 0.3333333333333335369, 0.3333333333333333148, 0.3333333333333335369, 0.3333333333333333148, 0.3333333333333335369, 0.3333333333333332593, 0.3333333333333335924, 0.3333333333333333148, 0.3333333333333335369, 0.3333333333333335369, 0.3333333333333334814, 0.3333333333333334259, 0.3333333333333334814, 0.3333333333333334814, 0.3333333333333334259, 0.3333333333333334259, 0.3333333333333334259, 0.3333333333333334814, 0.3333333333333334259, 0.3333333333333333703, 0.3333333333333334814, 0.3333333333333333703, 0.3333333333333335369, 0.3333333333333333703, 0.3333333333333334259, 0.3333333333333333148, 0.3333333333333334259, 0.3333333333333334259, 0.3333333333333333703, 0.3333333333333333703, 0.3333333333333335924, 0.3333333333333334259, 0.3333333333333335369, 0.3333333333333333148, 0.3333333333333335369, 0.3333333333333334814, 0.3333333333333334259, 0.3333333333333334814, 0.3333333333333334259, 0.3333333333333333703, 0.3333333333333335369, 0.3333333333333333148, 0.3333333333333335369, 0.3333333333333333703, 0.3333333333333335369, 0.3333333333333333703, 0.3333333333333334814, 0.3333333333333334259, 0.3333333333333333703, 0.3333333333333334259, 0.3333333333333333703, 0.3333333333333335924, 0.3333333333333334259, 0.3333333333333333148, 0.3333333333333334259, 0.3333333333333334259, 0.3333333333333334259, 0.3333333333333335924, 0.3333333333333333703, 0.3333333333333334259, 0.3333333333333334259, 0.3333333333333335369, 0.3333333333333333703, 0.3333333333333334814, 0.3333333333333334814, 0.3333333333333334814, 0.3333333333333333703, 0.3333333333333334814, 0.3333333333333333148, 0.3333333333333335369, 0.3333333333333334259, 0.3333333333333334814, 0.3333333333333333703, 0.3333333333333334259, 0.3333333333333334259, 0.3333333333333334259, 0.3333333333333334259, 0.3333333333333333703, 0.3333333333333333703, 0.3333333333333334814, 0.3333333333333333703, 0.3333333333333334259, 0.3333333333333334814, 0.3333333333333334259, 0.3333333333333334259, 0.3333333333333333703, 0.3333333333333334814, 0.3333333333333333703, 0.3333333333333334259, 0.3333333333333335369, 0.3333333333333333148, 0.3333333333333333703, 0.3333333333333334814, 0.3333333333333333148, 0.3333333333333334259, 0.3333333333333333703, 0.3333333333333333703, 0.3333333333333334814, 0.3333333333333333703, 0.3333333333333334259, 0.3333333333333334814, 0.3333333333333333703, 0.3333333333333334259, 0.3333333333333334259, 0.3333333333333334259, 0.3333333333333335369, 0.3333333333333334259, 0.3333333333333334259, 0.3333333333333333703, 0.3333333333333334259, 0.3333333333333334259, 0.3333333333333334259, 0.3333333333333334814, 0.3333333333333335369, 0.3333333333333333148, 0.3333333333333333703, 0.3333333333333335924, 0.3333333333333333148, 0.3333333333333334259, 0.3333333333333334259, 0.3333333333333333703, 0.3333333333333333148, 0.3333333333333335369, 0.3333333333333334259, 0.3333333333333333703, 0.3333333333333334814, 0.3333333333333334259, 0.3333333333333334259, 0.3333333333333333148, 0.3333333333333335369, 0.3333333333333333703, 0.3333333333333334259, 0.3333333333333334259),
 ( 0.3333333333333334259, 0.3333333333333334259, 0.3333333333333334814, 0.3333333333333333703, 0.3333333333333335369, 0.3333333333333335369, 0.3333333333333334259, 0.3333333333333334259, 0.3333333333333334259, 0.3333333333333334814, 0.3333333333333334259, 0.3333333333333334259, 0.3333333333333334259, 0.3333333333333334259, 0.3333333333333333148, 0.3333333333333334259, 0.3333333333333334814, 0.3333333333333333703, 0.3333333333333335369, 0.3333333333333335924, 0.3333333333333334259, 0.3333333333333334814, 0.3333333333333333703, 0.3333333333333334259, 0.3333333333333333703, 0.3333333333333334814, 0.3333333333333333703, 0.3333333333333334259, 0.3333333333333333703, 0.3333333333333333703, 0.3333333333333335369, 0.3333333333333334259, 0.3333333333333333703, 0.3333333333333335924, 0.3333333333333334259, 0.3333333333333334259, 0.3333333333333333703, 0.3333333333333334814, 0.3333333333333333703, 0.3333333333333334814, 0.3333333333333333703, 0.3333333333333335369, 0.3333333333333333148, 0.3333333333333334814, 0.3333333333333333703, 0.3333333333333334814, 0.3333333333333334259, 0.3333333333333333703, 0.3333333333333334259, 0.3333333333333334259, 0.3333333333333334814, 0.3333333333333333703, 0.3333333333333335369, 0.3333333333333334259, 0.3333333333333334259, 0.3333333333333334814, 0.3333333333333334259, 0.3333333333333334259, 0.3333333333333333703, 0.3333333333333333703, 0.3333333333333335924, 0.3333333333333334259, 0.3333333333333335369, 0.3333333333333333703, 0.3333333333333333703, 0.3333333333333333703, 0.3333333333333334814, 0.3333333333333333703, 0.3333333333333335369, 0.3333333333333332593, 0.3333333333333333703, 0.3333333333333334259, 0.3333333333333335369, 0.3333333333333334259, 0.3333333333333333703, 0.3333333333333334814, 0.3333333333333333703, 0.3333333333333335369, 0.3333333333333334259, 0.3333333333333333148, 0.3333333333333334814, 0.3333333333333334814, 0.3333333333333334259, 0.3333333333333333148, 0.3333333333333333703, 0.3333333333333334814, 0.3333333333333333703, 0.3333333333333334814, 0.3333333333333333148, 0.3333333333333334259, 0.3333333333333334814, 0.3333333333333333703, 0.3333333333333335369, 0.3333333333333334814, 0.3333333333333333148, 0.3333333333333335369, 0.3333333333333334814, 0.3333333333333334259, 0.3333333333333334814, 0.3333333333333333703, 0.3333333333333334814, 0.3333333333333334259, 0.3333333333333333703, 0.3333333333333334259, 0.3333333333333335369, 0.3333333333333334259, 0.3333333333333334259, 0.3333333333333334814, 0.3333333333333335369, 0.3333333333333333148, 0.3333333333333334259, 0.3333333333333333148, 0.3333333333333335924, 0.3333333333333334259, 0.3333333333333334814, 0.3333333333333333703, 0.3333333333333334814, 0.3333333333333334259, 0.3333333333333333703, 0.3333333333333335924, 0.3333333333333334259, 0.3333333333333334259, 0.3333333333333333703, 0.3333333333333334259, 0.3333333333333333703, 0.3333333333333333703, 0.3333333333333335369, 0.3333333333333334259, 0.3333333333333333703, 0.3333333333333334814, 0.3333333333333333148, 0.3333333333333335924, 0.3333333333333333148, 0.3333333333333334259, 0.3333333333333333148, 0.3333333333333335924, 0.3333333333333333703, 0.3333333333333335369, 0.3333333333333333148, 0.3333333333333334259, 0.3333333333333334814, 0.3333333333333334259, 0.3333333333333334259, 0.3333333333333334259, 0.3333333333333334259, 0.3333333333333334259, 0.3333333333333334259, 0.3333333333333334814, 0.3333333333333334259, 0.3333333333333333703, 0.3333333333333334814, 0.3333333333333333148, 0.3333333333333334259, 0.3333333333333334814, 0.3333333333333334259, 0.3333333333333333703, 0.3333333333333334259, 0.3333333333333334814, 0.3333333333333333703, 0.3333333333333334259, 0.3333333333333334814, 0.3333333333333333703, 0.3333333333333333703, 0.3333333333333333703, 0.3333333333333335369, 0.3333333333333333703, 0.3333333333333334814, 0.3333333333333334259, 0.3333333333333333703, 0.3333333333333334814, 0.3333333333333333703, 0.3333333333333334259, 0.3333333333333335369, 0.3333333333333333703, 0.3333333333333334259, 0.3333333333333334814, 0.3333333333333334259, 0.3333333333333335924, 0.3333333333333333703, 0.3333333333333334259, 0.3333333333333333148, 0.3333333333333335369, 0.3333333333333334259, 0.3333333333333334259, 0.3333333333333334259, 0.3333333333333333703, 0.3333333333333335369, 0.3333333333333334259, 0.3333333333333333703, 0.3333333333333334259, 0.3333333333333334259, 0.3333333333333333703, 0.3333333333333335369, 0.3333333333333333703, 0.3333333333333335369, 0.3333333333333333703, 0.3333333333333334814, 0.3333333333333334259, 0.3333333333333333703, 0.3333333333333334259, 0.3333333333333333703, 0.3333333333333334814, 0.3333333333333334259, 0.3333333333333333703, 0.3333333333333335369, 0.3333333333333333703, 0.3333333333333333703, 0.3333333333333334814, 0.3333333333333333703, 0.3333333333333333148, 0.3333333333333335924, 0.3333333333333333148, 0.3333333333333335924, 0.3333333333333332593, 0.3333333333333334814, 0.3333333333333334814, 0.3333333333333334259, 0.3333333333333334259, 0.3333333333333334814, 0.3333333333333334259, 0.3333333333333333703, 0.3333333333333335369, 0.3333333333333334259, 0.3333333333333334814, 0.3333333333333333703, 0.3333333333333334259, 0.3333333333333333703, 0.3333333333333334814, 0.3333333333333333703, 0.3333333333333335369, 0.3333333333333333148, 0.3333333333333335924, 0.3333333333333333703, 0.3333333333333334259, 0.3333333333333333703, 0.3333333333333334259, 0.3333333333333333703, 0.3333333333333333703, 0.3333333333333335924, 0.3333333333333334259, 0.3333333333333333148, 0.3333333333333334814, 0.3333333333333335369, 0.3333333333333333703, 0.3333333333333334814, 0.3333333333333333703, 0.3333333333333334259, 0.3333333333333335369, 0.3333333333333333148, 0.3333333333333334814, 0.3333333333333334814, 0.3333333333333333703, 0.3333333333333334259, 0.3333333333333334259, 0.3333333333333335369, 0.3333333333333333148, 0.3333333333333335369, 0.3333333333333333148, 0.3333333333333335369, 0.3333333333333332593, 0.3333333333333335924, 0.3333333333333333148, 0.3333333333333335369, 0.3333333333333335369, 0.3333333333333334814, 0.3333333333333334259, 0.3333333333333334814, 0.3333333333333334814, 0.3333333333333334259, 0.3333333333333334259, 0.3333333333333334259, 0.3333333333333334814, 0.3333333333333334259, 0.3333333333333333703, 0.3333333333333334814, 0.3333333333333333703, 0.3333333333333335369, 0.3333333333333333703, 0.3333333333333334259, 0.3333333333333333148, 0.3333333333333334259, 0.3333333333333334259, 0.3333333333333333703, 0.3333333333333333703, 0.3333333333333335924, 0.3333333333333334259, 0.3333333333333335369, 0.3333333333333333148, 0.3333333333333335369, 0.3333333333333334814, 0.3333333333333334259, 0.3333333333333334814, 0.3333333333333334259, 0.3333333333333333703, 0.3333333333333335369, 0.3333333333333333148, 0.3333333333333335369, 0.3333333333333333703, 0.3333333333333335369, 0.3333333333333333703, 0.3333333333333334814, 0.3333333333333334259, 0.3333333333333333703, 0.3333333333333334259, 0.3333333333333333703, 0.3333333333333335924, 0.3333333333333334259, 0.3333333333333333148, 0.3333333333333334259, 0.3333333333333334259, 0.3333333333333334259, 0.3333333333333335924, 0.3333333333333333703, 0.3333333333333334259, 0.3333333333333334259, 0.3333333333333335369, 0.3333333333333333703, 0.3333333333333334814, 0.3333333333333334814, 0.3333333333333334814, 0.3333333333333333703, 0.3333333333333334814, 0.3333333333333333148, 0.3333333333333335369, 0.3333333333333334259, 0.3333333333333334814, 0.3333333333333333703, 0.3333333333333334259, 0.3333333333333334259, 0.3333333333333334259, 0.3333333333333334259, 0.3333333333333333703, 0.3333333333333333703, 0.3333333333333334814, 0.3333333333333333703, 0.3333333333333334259, 0.3333333333333334814, 0.3333333333333334259, 0.3333333333333334259, 0.3333333333333333703, 0.3333333333333334814, 0.3333333333333333703, 0.3333333333333334259, 0.3333333333333335369, 0.3333333333333333148, 0.3333333333333333703, 0.3333333333333334814, 0.3333333333333333148, 0.3333333333333334259, 0.3333333333333333703, 0.3333333333333333703, 0.3333333333333334814, 0.3333333333333333703, 0.3333333333333334259, 0.3333333333333334814, 0.3333333333333333703, 0.3333333333333334259, 0.3333333333333334259, 0.3333333333333334259, 0.3333333333333335369, 0.3333333333333334259, 0.3333333333333334259, 0.3333333333333333703, 0.3333333333333334259, 0.3333333333333334259, 0.3333333333333334259, 0.3333333333333334814, 0.3333333333333335369, 0.3333333333333333148, 0.3333333333333333703, 0.3333333333333335924, 0.3333333333333333148, 0.3333333333333334259, 0.3333333333333334259, 0.3333333333333333703, 0.3333333333333333148, 0.3333333333333335369, 0.3333333333333334259, 0.3333333333333333703, 0.3333333333333334814, 0.3333333333333334259, 0.3333333333333334259, 0.3333333333333333148, 0.3333333333333335369, 0.3333333333333333703, 0.3333333333333334259, 0.3333333333333334259),
 ( 1.000000000000000222, 1.000000000000000222, 1.000000000000000222, 1.000000000000000222, 1.000000000000000444, 1.000000000000000444, 1.000000000000000222, 1.000000000000000444, 1.000000000000000222, 1.000000000000000444, 1.000000000000000444, 1.000000000000000000, 1.000000000000000222, 1.000000000000000000, 1.000000000000000222, 1.000000000000000222, 1.000000000000000444, 1.000000000000000000, 1.000000000000000444, 1.000000000000000444, 1.000000000000000222, 1.000000000000000222, 1.000000000000000000, 1.000000000000000222, 1.000000000000000000, 1.000000000000000444, 1.000000000000000000, 1.000000000000000444, 1.000000000000000222, 1.000000000000000000, 1.000000000000000666, 1.000000000000000000, 1.000000000000000222, 1.000000000000000666, 1.000000000000000222, 1.000000000000000444, 1.000000000000000222, 1.000000000000000444, 1.000000000000000000, 1.000000000000000444, 1.000000000000000000, 1.000000000000000444, 1.000000000000000000, 1.000000000000000444, 1.000000000000000000, 1.000000000000000222, 1.000000000000000444, 1.000000000000000000, 1.000000000000000444, 1.000000000000000222, 1.000000000000000222, 1.000000000000000444, 1.000000000000000222, 1.000000000000000444, 1.000000000000000222, 1.000000000000000222, 1.000000000000000444, 1.000000000000000444, 1.000000000000000222, 1.000000000000000222, 1.000000000000000444, 1.000000000000000222, 1.000000000000000444, 1.000000000000000000, 1.000000000000000222, 1.000000000000000222, 1.000000000000000222, 1.000000000000000222, 1.000000000000000444, 1.000000000000000000, 0.9999999999999997780, 1.000000000000000444, 1.000000000000000444, 1.000000000000000222, 1.000000000000000222, 1.000000000000000444, 0.9999999999999997780, 1.000000000000000666, 1.000000000000000000, 1.000000000000000000, 1.000000000000000444, 1.000000000000000222, 1.000000000000000222, 0.9999999999999997780, 1.000000000000000222, 1.000000000000000444, 0.9999999999999997780, 1.000000000000000444, 1.000000000000000000, 1.000000000000000000, 1.000000000000000444, 1.000000000000000000, 1.000000000000000444, 1.000000000000000444, 0.9999999999999997780, 1.000000000000000444, 1.000000000000000444, 1.000000000000000444, 1.000000000000000444, 1.000000000000000000, 1.000000000000000444, 1.000000000000000222, 1.000000000000000000, 1.000000000000000444, 1.000000000000000444, 1.000000000000000222, 1.000000000000000000, 1.000000000000000444, 1.000000000000000444, 1.000000000000000000, 1.000000000000000222, 1.000000000000000000, 1.000000000000000444, 1.000000000000000222, 1.000000000000000444, 1.000000000000000222, 1.000000000000000444, 1.000000000000000444, 1.000000000000000000, 1.000000000000000666, 1.000000000000000222, 1.000000000000000222, 1.000000000000000000, 1.000000000000000222, 1.000000000000000222, 1.000000000000000222, 1.000000000000000444, 1.000000000000000222, 1.000000000000000222, 1.000000000000000444, 0.9999999999999997780, 1.000000000000000666, 0.9999999999999997780, 1.000000000000000222, 1.000000000000000000, 1.000000000000000444, 1.000000000000000000, 1.000000000000000444, 1.000000000000000000, 1.000000000000000222, 1.000000000000000222, 1.000000000000000444, 1.000000000000000444, 1.000000000000000222, 1.000000000000000444, 1.000000000000000444, 1.000000000000000000, 1.000000000000000666, 1.000000000000000222, 1.000000000000000222, 1.000000000000000444, 1.000000000000000000, 1.000000000000000222, 1.000000000000000444, 1.000000000000000000, 1.000000000000000222, 1.000000000000000222, 1.000000000000000444, 1.000000000000000222, 1.000000000000000222, 1.000000000000000444, 1.000000000000000000, 1.000000000000000222, 1.000000000000000000, 1.000000000000000444, 1.000000000000000222, 1.000000000000000444, 1.000000000000000222, 1.000000000000000222, 1.000000000000000444, 1.000000000000000000, 1.000000000000000222, 1.000000000000000444, 1.000000000000000000, 1.000000000000000444, 1.000000000000000222, 1.000000000000000444, 1.000000000000000444, 1.000000000000000222, 1.000000000000000222, 1.000000000000000000, 1.000000000000000444, 1.000000000000000444, 1.000000000000000000, 1.000000000000000444, 1.000000000000000222, 1.000000000000000444, 1.000000000000000444, 1.000000000000000222, 1.000000000000000000, 1.000000000000000444, 1.000000000000000222, 1.000000000000000444, 1.000000000000000000, 1.000000000000000444, 1.000000000000000222, 1.000000000000000222, 1.000000000000000444, 1.000000000000000222, 1.000000000000000222, 1.000000000000000222, 1.000000000000000222, 1.000000000000000444, 1.000000000000000000, 1.000000000000000666, 1.000000000000000000, 1.000000000000000222, 1.000000000000000444, 1.000000000000000000, 1.000000000000000222, 1.000000000000000444, 1.000000000000000000, 1.000000000000000666, 0.9999999999999997780, 1.000000000000000222, 1.000000000000000444, 1.000000000000000000, 1.000000000000000444, 1.000000000000000222, 1.000000000000000444, 1.000000000000000000, 1.000000000000000444, 1.000000000000000222, 1.000000000000000222, 1.000000000000000000, 1.000000000000000444, 1.000000000000000222, 1.000000000000000000, 1.000000000000000222, 1.000000000000000222, 1.000000000000000222, 1.000000000000000444, 1.000000000000000000, 1.000000000000000444, 1.000000000000000222, 1.000000000000000222, 1.000000000000000222, 1.000000000000000000, 1.000000000000000666, 1.000000000000000000, 1.000000000000000000, 1.000000000000000222, 1.000000000000000444, 1.000000000000000222, 1.000000000000000444, 0.9999999999999997780, 1.000000000000000444, 1.000000000000000444, 0.9999999999999997780, 1.000000000000000444, 1.000000000000000444, 1.000000000000000444, 1.000000000000000222, 1.000000000000000444, 1.000000000000000444, 1.000000000000000000, 1.000000000000000444, 0.9999999999999997780, 1.000000000000000444, 0.9999999999999997780, 1.000000000000000444, 1.000000000000000000, 1.000000000000000444, 1.000000000000000444, 1.000000000000000444, 1.000000000000000222, 1.000000000000000444, 1.000000000000000444, 1.000000000000000222, 1.000000000000000222, 1.000000000000000000, 1.000000000000000222, 1.000000000000000444, 0.9999999999999997780, 1.000000000000000666, 0.9999999999999997780, 1.000000000000000444, 1.000000000000000222, 1.000000000000000222, 1.000000000000000000, 1.000000000000000222, 1.000000000000000222, 1.000000000000000000, 1.000000000000000000, 1.000000000000000444, 1.000000000000000222, 1.000000000000000444, 0.9999999999999997780, 1.000000000000000444, 1.000000000000000444, 1.000000000000000222, 1.000000000000000444, 1.000000000000000000, 1.000000000000000444, 1.000000000000000444, 0.9999999999999997780, 1.000000000000000444, 1.000000000000000222, 1.000000000000000444, 1.000000000000000222, 1.000000000000000222, 1.000000000000000444, 1.000000000000000000, 1.000000000000000000, 1.000000000000000444, 1.000000000000000444, 1.000000000000000444, 0.9999999999999997780, 1.000000000000000444, 1.000000000000000222, 1.000000000000000222, 1.000000000000000444, 1.000000000000000000, 1.000000000000000444, 1.000000000000000222, 1.000000000000000444, 1.000000000000000000, 1.000000000000000444, 1.000000000000000444, 1.000000000000000444, 1.000000000000000000, 1.000000000000000444, 1.000000000000000000, 1.000000000000000222, 1.000000000000000444, 1.000000000000000444, 1.000000000000000000, 1.000000000000000444, 1.000000000000000444, 1.000000000000000000, 1.000000000000000444, 1.000000000000000222, 1.000000000000000000, 1.000000000000000444, 1.000000000000000222, 1.000000000000000222, 1.000000000000000444, 1.000000000000000444, 1.000000000000000000, 1.000000000000000000, 1.000000000000000444, 1.000000000000000000, 1.000000000000000222, 1.000000000000000444, 1.000000000000000000, 1.000000000000000222, 1.000000000000000444, 0.9999999999999997780, 1.000000000000000444, 1.000000000000000222, 1.000000000000000000, 1.000000000000000444, 1.000000000000000000, 1.000000000000000444, 1.000000000000000444, 1.000000000000000000, 1.000000000000000222, 1.000000000000000222, 1.000000000000000222, 1.000000000000000444, 1.000000000000000222, 1.000000000000000000, 1.000000000000000222, 1.000000000000000444, 1.000000000000000444, 1.000000000000000222, 1.000000000000000444, 1.000000000000000444, 1.000000000000000000, 1.000000000000000000, 1.000000000000000666, 0.9999999999999997780, 1.000000000000000444, 0.9999999999999997780, 1.000000000000000222, 0.9999999999999997780, 1.000000000000000444, 1.000000000000000000, 1.000000000000000222, 1.000000000000000222, 1.000000000000000444, 1.000000000000000000, 1.000000000000000000, 1.000000000000000444, 1.000000000000000000, 1.000000000000000222, 1.000000000000000222) ) ) 
 REPRESENTATION_ITEM ( '' )  SURFACE ( )  );
#13977 = CARTESIAN_POINT ( 'NONE',  ( -10.14031698345510080, 3.934660213246443661, 5.561808457406734796 ) ) ;
#13979 = CARTESIAN_POINT ( 'NONE',  ( -1.250000000000039302, 8.500000000000000000, -10.85702537530423228 ) ) ;
#13980 = EDGE_CURVE ( 'NONE', #73877, #17090, #13411, .T. ) ;
#13981 = CARTESIAN_POINT ( 'NONE',  ( -6.505933609711270549, 8.683618192786854095, -1.599625672291271394 ) ) ;
#13983 = DIRECTION ( 'NONE',  ( 0.000000000000000000, 0.000000000000000000, 1.000000000000000000 ) ) ;
#13982 = CARTESIAN_POINT ( 'NONE',  ( -4.607972389651186162, 8.469779238289159906, 0.3137405545926199579 ) ) ;
#13984 = CARTESIAN_POINT ( 'NONE',  ( 1.458514304043815102, 8.731595392684152301, -2.560210433951503273 ) ) ;
#13985 = ORIENTED_EDGE ( 'NONE', *, *, #66840, .T. ) ;
#13986 = CARTESIAN_POINT ( 'NONE',  ( 4.873930702218094879, 1.184903577025652188, 1.686001177547257424 ) ) ;
#13987 = CARTESIAN_POINT ( 'NONE',  ( -6.224601922005509991, 10.27613631906616476, 0.7216878364870267237 ) ) ;
#13988 = CARTESIAN_POINT ( 'NONE',  ( -4.205000198532790279, 8.057583998263570635, 0.7998128361456341429 ) ) ;
#13989 = CARTESIAN_POINT ( 'NONE',  ( -3.630551273409382329, 7.457669928944732796, 0.7998128361456352531 ) ) ;
#13990 = CARTESIAN_POINT ( 'NONE',  ( 3.985024733980116363, -1.885273983189727831, -0.7249480779877092163 ) ) ;
#13991 = CARTESIAN_POINT ( 'NONE',  ( -1.500000000000001332, 0.4000000000000253353, 0.000000000000000000 ) ) ;
#13993 = CARTESIAN_POINT ( 'NONE',  ( 4.369805582306193870, 3.992528022312320957, 1.214306433183764966E-14 ) ) ;
#13992 = CARTESIAN_POINT ( 'NONE',  ( -4.655245641445871385, 6.524482229810530498, 1.599625672291263179 ) ) ;
#13994 = CARTESIAN_POINT ( 'NONE',  ( 8.118635056484817980, 8.366162408854107113, 0.7998128361456481317 ) ) ;
#13995 = CARTESIAN_POINT ( 'NONE',  ( 3.098563410164618226, -0.5969507786072983935, -1.972546241584592241 ) ) ;
#13996 = CARTESIAN_POINT ( 'NONE',  ( 3.322888845334175389, 0.9041102021897020613, -1.802417075407992897 ) ) ;
#13997 = CARTESIAN_POINT ( 'NONE',  ( -2.428612866367529932E-14, 2.800000000000024691, 0.7750000000000117906 ) ) ;
#13998 = CARTESIAN_POINT ( 'NONE',  ( 5.464099601507359516, 6.333536608968757697, 1.199719254218462483 ) ) ;
#13999 = CARTESIAN_POINT ( 'NONE',  ( -0.4680205011783908353, 8.035366863023629236, -1.945178226287664902 ) ) ;
#14000 = CARTESIAN_POINT ( 'NONE',  ( 1.306327274835542784, 1.622920506532832929, 0.8694138843568788300 ) ) ;
#14001 = CARTESIAN_POINT ( 'NONE',  ( 0.3293365701910222487, 2.210228212078951149, 0.6636047247109229108 ) ) ;
#14002 = CARTESIAN_POINT ( 'NONE',  ( 4.227110032410640095, 8.153655147779589996, 0.7998128361456271485 ) ) ;
#14003 = CARTESIAN_POINT ( 'NONE',  ( 2.108864864398530159, 1.603267699958549342, -1.450045708023157687 ) ) ;
#14004 = CARTESIAN_POINT ( 'NONE',  ( -4.121315508874269007, 5.831287398485176077, -1.443375672974053447 ) ) ;
#14005 = CARTESIAN_POINT ( 'NONE',  ( 4.346934998023818331, -1.892857631927163498, -0.9488708475321022684 ) ) ;
#14006 = CARTESIAN_POINT ( 'NONE',  ( 3.642672431166743330, 3.097590952613315185, -2.447572309175019889 ) ) ;
#14007 = CARTESIAN_POINT ( 'NONE',  ( 1.727212824277712944, -1.762453432929488528, 0.6273722324065673650 ) ) ;
#14008 = CARTESIAN_POINT ( 'NONE',  ( 4.698096894549816049, -1.971010956759836397, -0.04940921540304286930 ) ) ;
#14009 = CARTESIAN_POINT ( 'NONE',  ( 5.190638768449240992, 1.523797776992100284, -1.320824044268428255 ) ) ;
#14011 = CARTESIAN_POINT ( 'NONE',  ( 0.000000000000000000, 7.999999999999992895, 0.000000000000000000 ) ) ;
#14010 = CARTESIAN_POINT ( 'NONE',  ( 1.364683531249988535, 3.155208333674756283, -0.7879004041258239610 ) ) ;
#14013 = CARTESIAN_POINT ( 'NONE',  ( 6.604139054488365801, -2.105657007711879469, 0.04960021190137350877 ) ) ;
#14012 = CARTESIAN_POINT ( 'NONE',  ( -5.605406444246153974, 8.627059054007450101, -1.199719254218440723 ) ) ;
#14014 = CARTESIAN_POINT ( 'NONE',  ( 5.076602173674213070, 4.887400388900169368, 0.000000000000000000 ) ) ;
#14015 = CARTESIAN_POINT ( 'NONE',  ( 6.169123589417988995, 7.156064594864501416, -1.199719254218445830 ) ) ;
#14016 = CARTESIAN_POINT ( 'NONE',  ( -6.039267359883488950, 9.133230122250985517, 1.199719254218452047 ) ) ;
#14017 = CARTESIAN_POINT ( 'NONE',  ( 5.524284814141814159, 1.174771371627521876, -1.583071389104006244 ) ) ;
#14018 = CARTESIAN_POINT ( 'NONE',  ( 5.924083597509600452, -2.004057273996622701, 0.2512124657789679971 ) ) ;
#14019 = CARTESIAN_POINT ( 'NONE',  ( 1.499999999999989120, -0.1937499993171845625, 0.000000000000000000 ) ) ;
#14020 = CARTESIAN_POINT ( 'NONE',  ( 4.547712581667567200, -1.782031661950409962, -1.466240793230636275 ) ) ;
#14021 = EDGE_CURVE ( 'NONE', #7711, #43590, #84924, .T. ) ;
#14022 = CARTESIAN_POINT ( 'NONE',  ( 1.850508050571671559, -2.052242141108654661, -0.2064673365099172486 ) ) ;
#14023 = CARTESIAN_POINT ( 'NONE',  ( 7.293923454472080792, 9.532663335016016148, 1.443375672974076540 ) ) ;
#14024 = CARTESIAN_POINT ( 'NONE',  ( 5.180097208873055692, 8.201141289397330780, -1.199719254218450271 ) ) ;
#14025 = CARTESIAN_POINT ( 'NONE',  ( 4.248501033035879004, 6.049946853332221153, -1.599625672291273171 ) ) ;
#14026 = CARTESIAN_POINT ( 'NONE',  ( 1.364683531249988535, 1.676041667008085101, 0.7879004041258500513 ) ) ;
#14027 = CARTESIAN_POINT ( 'NONE',  ( 5.252858170651868441, 5.093032385374103299, -0.7998128361456481317 ) ) ;
#14028 = CARTESIAN_POINT ( 'NONE',  ( 5.761852095683461350, 9.665985178365305686, -0.7216878364870267237 ) ) ;
#14029 = CARTESIAN_POINT ( 'NONE',  ( 4.738842072872849087, -2.104903140973454434, -0.5318641579697135358 ) ) ;
#14030 = CARTESIAN_POINT ( 'NONE',  ( -6.265276382846530545, 6.482112999508623297, 0.000000000000000000 ) ) ;
#14032 = CARTESIAN_POINT ( 'NONE',  ( 3.016969003575611818, -1.773741936391802332, 0.4936923545346691977 ) ) ;
#14031 = CARTESIAN_POINT ( 'NONE',  ( -3.850152436600983386, 4.554561266531622188, 1.082531754730560403 ) ) ;
#14034 = CARTESIAN_POINT ( 'NONE',  ( 6.620655732516644854, 4.701125524277991907, 2.388986273831222640 ) ) ;
#14033 = CARTESIAN_POINT ( 'NONE',  ( -0.6823417656249969321, 4.217708333674755394, -1.181850606188749264 ) ) ;
#14035 = CARTESIAN_POINT ( 'NONE',  ( 5.460537066722415567, -1.980877156148381335, -0.9378266216248376530 ) ) ;
#14036 = CARTESIAN_POINT ( 'NONE',  ( 8.717236016799597920, 13.50218641590694979, 8.247095274259196529 ) ) ;
#14037 = CARTESIAN_POINT ( 'NONE',  ( 5.471622919743277969, 2.182126815565027300, -0.5975609995224858695 ) ) ;
#14038 = CARTESIAN_POINT ( 'NONE',  ( -4.613696345000219523, 7.131516869168907924, -1.371494837298018243 ) ) ;
#14039 = CARTESIAN_POINT ( 'NONE',  ( 4.596911992430688265, 8.487755744900498556, -0.08351877912710949092 ) ) ;
#14040 = CARTESIAN_POINT ( 'NONE',  ( -5.600926855776888758, 7.627776979863398310, -1.443375672974066548 ) ) ;
#14041 = CARTESIAN_POINT ( 'NONE',  ( -6.764898216727353919, -7.628386336122861877, -6.764898216730279579 ) ) ;
#14042 = CARTESIAN_POINT ( 'NONE',  ( 0.1448901830083254016, -1.363511527656173339, -1.128195317737596293 ) ) ;
#14043 = CARTESIAN_POINT ( 'NONE',  ( 4.406893533441514244, -0.4431801161997659944, -1.963548474556547685 ) ) ;
#14044 = CARTESIAN_POINT ( 'NONE',  ( 5.296431564432884542, 9.330920591813708143, 1.040834085586084257E-14 ) ) ;
#14045 = CARTESIAN_POINT ( 'NONE',  ( 2.590967463960031303, -0.3587740299011917267, -2.075001757462133778 ) ) ;
#14046 = CARTESIAN_POINT ( 'NONE',  ( 2.460426067449926535, -1.833815074015308300, -0.5538200352182551800 ) ) ;
#14047 = CARTESIAN_POINT ( 'NONE',  ( 3.171717870593107058, 5.787755718078879674, -1.199719254218446718 ) ) ;
#14048 = CARTESIAN_POINT ( 'NONE',  ( 2.998452255303164726, 1.954363348466476857, 0.2436675063324095225 ) ) ;
#14049 = CARTESIAN_POINT ( 'NONE',  ( 1.674454752297813265, -1.775319108138155633, -0.5897529795871117031 ) ) ;
#14050 = CARTESIAN_POINT ( 'NONE',  ( 1.680054527999317759, -1.087118939145682583, -1.632918184844594611 ) ) ;
#14053 = VERTEX_POINT ( 'NONE', #98010 ) ;
#14052 = CARTESIAN_POINT ( 'NONE',  ( 1.283307755816986528, 0.1377011610334301639, -1.907463248872851569 ) ) ;
#14051 = CARTESIAN_POINT ( 'NONE',  ( 4.353923116202039978, 1.724447095217627401, -0.04574849716902986557 ) ) ;
#14055 = CARTESIAN_POINT ( 'NONE',  ( 3.850152436600926542, 7.435668909435648288, -0.7216878364870197293 ) ) ;
#14054 = CARTESIAN_POINT ( 'NONE',  ( 1.524350002934187653, -1.228176919886795782, -1.833354347511229498 ) ) ;
#14056 = TOROIDAL_SURFACE ( 'NONE', #114504, 0.8299999999999998490, 0.08000000000000000167 ) ;
#14057 = CARTESIAN_POINT ( 'NONE',  ( -0.6823417656250003738, 1.530208333674752730, -1.181850606188749264 ) ) ;
#14059 = EDGE_CURVE ( 'NONE', #157630, #130351, #165718, .T. ) ;
#14058 = CARTESIAN_POINT ( 'NONE',  ( 9.576136569953906275, 10.06658084123472641, 0.000000000000000000 ) ) ;
#14060 = CARTESIAN_POINT ( 'NONE',  ( 6.754772315933175619, -1.444328698515121800, 1.188528157999017454 ) ) ;
#14061 = CARTESIAN_POINT ( 'NONE',  ( -0.6823417656249969321, 3.217708333674754062, -1.181850606188749264 ) ) ;
#14062 = CYLINDRICAL_SURFACE ( 'NONE', #23922, 2.000000000000000000 ) ;
#14063 = CARTESIAN_POINT ( 'NONE',  ( 6.526242037438201749, 1.059062773735760521, 1.778703558766213000 ) ) ;
#14064 = CARTESIAN_POINT ( 'NONE',  ( 1.170471352854907776, -0.9292243337341490328, -1.850172451097586990 ) ) ;
#14065 = CARTESIAN_POINT ( 'NONE',  ( -0.7500000000000215383, 2.441666666666689078, 1.299038105676671107 ) ) ;
#14066 = CARTESIAN_POINT ( 'NONE',  ( 6.449928391799196525, 8.548002428564306143, -1.599625672291262513 ) ) ;
#14067 = CARTESIAN_POINT ( 'NONE',  ( -8.040148788103921973, 9.338927326664741457, 1.199719254218462483 ) ) ;
#14068 = CARTESIAN_POINT ( 'NONE',  ( 4.258142763143749399, 7.125527769379820242, 1.199719254218451159 ) ) ;
#14069 = CARTESIAN_POINT ( 'NONE',  ( 5.813165546740090228, 1.733599321496303691, -1.220823391460408303 ) ) ;
#14070 = CARTESIAN_POINT ( 'NONE',  ( 1.364683531249986537, 2.655208333674754062, -0.7879004041258239610 ) ) ;
#14071 = CARTESIAN_POINT ( 'NONE',  ( -1.402160292154681736E-14, 2.587500000000023892, -1.732050807568863648 ) ) ;
#14073 = CARTESIAN_POINT ( 'NONE',  ( 3.765413976293345844, 5.416068943807445635, 1.599625672291267398 ) ) ;
#14072 = CARTESIAN_POINT ( 'NONE',  ( 6.109812101310618360, 0.5708666350849945781, -1.876949146916474298 ) ) ;
#14074 = CARTESIAN_POINT ( 'NONE',  ( 4.745470142856022200, -1.954873481938533608, -0.4925652823710227612 ) ) ;
#14075 = CARTESIAN_POINT ( 'NONE',  ( 4.100734417499996454, 1.753908128398029787, 0.7709784123341425488 ) ) ;
#14076 = CARTESIAN_POINT ( 'NONE',  ( -15.75000000000000000, 11.29999999999998117, 3.199999999999997957 ) ) ;
#14077 = CARTESIAN_POINT ( 'NONE',  ( 1.874823134854076923, -0.1115055541827478930, -2.188858692977871279 ) ) ;
#14078 = FACE_OUTER_BOUND ( 'NONE', #25305, .T. ) ;
#14079 = CARTESIAN_POINT ( 'NONE',  ( 0.7499999999999902300, 1.264583334016147642, 1.299038105676657340 ) ) ;
#14080 = CARTESIAN_POINT ( 'NONE',  ( 4.763936024516410406, 0.6273381447981136727, -1.913061789696899995 ) ) ;
#14081 = CARTESIAN_POINT ( 'NONE',  ( -5.856232286098998152, 8.919689202835742847, 1.199719254218452047 ) ) ;
#14083 = CARTESIAN_POINT ( 'NONE',  ( 5.905892042933183816, -1.176582040423958642, -1.760015123184681007 ) ) ;
#14082 = CARTESIAN_POINT ( 'NONE',  ( -4.934804725694236893, 4.859619722839116918, -0.7216878364870207285 ) ) ;
#14084 = B_SPLINE_CURVE_WITH_KNOTS ( 'NONE', 3,
 ( #133244, #34634, #166781, #203507, #185133, #188344, #87659, #35697 ),
 .UNSPECIFIED., .F., .F.,
 ( 4, 2, 2, 4 ),
 ( 1.064888869118067945E-15, 0.0004636157603174408007, 0.0006954236404756272043, 0.0009272315206338136622 ),
 .UNSPECIFIED. ) ;
#14086 = CARTESIAN_POINT ( 'NONE',  ( -5.433785704026946384, 9.561443431331920095, 0.000000000000000000 ) ) ;
#14085 = CARTESIAN_POINT ( 'NONE',  ( 2.068024735862358021, -1.283949768261948288, 1.649988806608338798 ) ) ;
#14088 = VERTEX_POINT ( 'NONE', #134774 ) ;
#14087 = CARTESIAN_POINT ( 'NONE',  ( 0.4106395295978342297, 1.496939291644447279, 0.8566152473860905170 ) ) ;
#14089 = CARTESIAN_POINT ( 'NONE',  ( 5.113396490648394632, 9.117379672398465473, 1.040834085586084257E-14 ) ) ;
#14090 = DIRECTION ( 'NONE',  ( 1.000000000000000000, -0.000000000000000000, -0.000000000000000000 ) ) ;
#14091 = EDGE_CURVE ( 'NONE', #80549, #69931, #47329, .T. ) ;
#14092 = CARTESIAN_POINT ( 'NONE',  ( 7.503460210123510166, -6.893136966056697901, 8.043985462411230358 ) ) ;
#14093 = CARTESIAN_POINT ( 'NONE',  ( 6.779954559072996823, -7.792646766724983465, -6.731761806397363657 ) ) ;
#14095 = CARTESIAN_POINT ( 'NONE',  ( 8.500599125643985232, 11.90082083235127008, -1.082531754730543083 ) ) ;
#14094 = CARTESIAN_POINT ( 'NONE',  ( 7.142447996300871793, 7.227277505306155092, 0.7998128361456341429 ) ) ;
#14096 = ORIENTED_EDGE ( 'NONE', *, *, #76230, .T. ) ;
#14097 = PRESENTATION_LAYER_ASSIGNMENT (  '', '', ( #180038 ) ) ;
#14099 = CARTESIAN_POINT ( 'NONE',  ( 2.226969132303910470, 1.618658205268191930, 0.8133494039403755815 ) ) ;
#14098 = CARTESIAN_POINT ( 'NONE',  ( 5.285699784481295183, 7.260012063351913625, 1.599625672291268286 ) ) ;
#14100 = CARTESIAN_POINT ( 'NONE',  ( -6.989391883044787868, 8.113044270762433285, -1.199719254218446718 ) ) ;
#14101 = CARTESIAN_POINT ( 'NONE',  ( 4.701980345841006326, 4.380065246436280368, 0.7998128361456341429 ) ) ;
#14102 = CARTESIAN_POINT ( 'NONE',  ( 5.845500506147374153, 6.848780674373954547, 1.199719254218453823 ) ) ;
#14103 = CARTESIAN_POINT ( 'NONE',  ( 3.211360534488953977, 1.429591190403207035, 1.112411576641762379 ) ) ;
#14104 = CARTESIAN_POINT ( 'NONE',  ( 6.539320575229256249, 2.979067782826943844, 2.350490835693248126 ) ) ;
#14105 = CIRCLE ( 'NONE', #3724, 2.500000000000007994 ) ;
#14106 = CARTESIAN_POINT ( 'NONE',  ( 0.000000000000000000, 0.2000000000000057288, 0.000000000000000000 ) ) ;
#14107 = CARTESIAN_POINT ( 'NONE',  ( 4.863282293121215183, 6.691362709583676072, 1.250037515303052738 ) ) ;
#14108 = CARTESIAN_POINT ( 'NONE',  ( 10.08690309888728187, 10.87040115823107911, -0.7216878364870257245 ) ) ;
#14109 = CARTESIAN_POINT ( 'NONE',  ( 2.963170385688845609, 1.570644928931948181, 0.9979875196418576122 ) ) ;
#14110 = CARTESIAN_POINT ( 'NONE',  ( 0.9135317552573400945, -1.216341065326152160, -1.479849217926126004 ) ) ;
#14111 = CARTESIAN_POINT ( 'NONE',  ( 0.1119280604304096899, -0.7754228321929098611, -1.651232954423286436 ) ) ;
#14112 = FACE_OUTER_BOUND ( 'NONE', #195776, .T. ) ;
#14113 = CARTESIAN_POINT ( 'NONE',  ( 5.048048446811987944, 4.783811364235761587, -0.4196793407983526181 ) ) ;
#14114 = CARTESIAN_POINT ( 'NONE',  ( 4.763071791759735163, 8.170823326046956936, 0.7639991172946744014 ) ) ;
#14115 = CARTESIAN_POINT ( 'NONE',  ( -3.714570900464290393, 5.356752022006865843, 1.443375672974064550 ) ) ;
#14116 = CARTESIAN_POINT ( 'NONE',  ( 7.104109303880752790, 11.23195192126214970, -0.7216878364870267237 ) ) ;
#14117 = CARTESIAN_POINT ( 'NONE',  ( 4.241030189111538284, -0.1885853823969813603, -1.960358720193545068 ) ) ;
#14118 = CARTESIAN_POINT ( 'NONE',  ( -3.744022975668147790, 7.519777238254810925, -0.7998128361456281477 ) ) ;
#14119 = CARTESIAN_POINT ( 'NONE',  ( -9.500350659417458488, -7.217450603046464686, 0.002323312720852115966 ) ) ;
#14120 = DIRECTION ( 'NONE',  ( 0.000000000000000000, 1.000000000000000000, 0.000000000000000000 ) ) ;
#14121 = CARTESIAN_POINT ( 'NONE',  ( 6.562441972333600937, -2.001882313047067985, -0.8919867065708479981 ) ) ;
#14122 = FILL_AREA_STYLE_COLOUR ( '', #105569 ) ;
#14123 = CARTESIAN_POINT ( 'NONE',  ( 5.614262457756467484, -0.8664596825185383322, -1.720589126903127264 ) ) ;
#14124 = CARTESIAN_POINT ( 'NONE',  ( -7.881367368245678406, 8.089350105908421185, 0.7998128361456602331 ) ) ;
#14125 = CARTESIAN_POINT ( 'NONE',  ( 0.3404811318320750679, 0.3065618842239410946, 1.799498403862239693 ) ) ;
#14126 = CARTESIAN_POINT ( 'NONE',  ( 2.403190426070573871, 1.771669130372434564, -1.315670724662293178 ) ) ;
#14127 = EDGE_CURVE ( 'NONE', #29424, #162756, #75728, .T. ) ;
#14128 = CARTESIAN_POINT ( 'NONE',  ( 0.000000000000000000, 0.000000000000000000, 0.000000000000000000 ) ) ;
#14129 = LINE ( 'NONE', #130129, #116313 ) ;
#14130 = EDGE_LOOP ( 'NONE', ( #27426, #159998, #185496, #114749 ) ) ;
#14131 = ORIENTED_EDGE ( 'NONE', *, *, #47472, .F. ) ;
#14132 = CARTESIAN_POINT ( 'NONE',  ( 6.977413706903823787, -0.1529601955215283693, 1.936277946061695898 ) ) ;
#14133 = CARTESIAN_POINT ( 'NONE',  ( 1.382261328670054246, -0.2867773604850975544, -1.920668630092968732 ) ) ;
#14134 = CARTESIAN_POINT ( 'NONE',  ( 0.7200771085676247463, -1.701685607325746252, -1.080902626906909747 ) ) ;
#14136 = CARTESIAN_POINT ( 'NONE',  ( 5.594539833219323022, 1.833072992967394788, 0.3199324213378691439 ) ) ;
#14135 = CARTESIAN_POINT ( 'NONE',  ( -6.089547271193396227, 7.133501900260939443, -1.199719254218453823 ) ) ;
#14137 = CARTESIAN_POINT ( 'NONE',  ( 5.712781623311797397, 7.758274208654143855, -1.599625672291283607 ) ) ;
#14138 = FACE_BOUND ( 'NONE', #86725, .T. ) ;
#14139 = CARTESIAN_POINT ( 'NONE',  ( 1.485661138090796918, 7.335467742080692410, -4.255596723435695949 ) ) ;
#14140 = CARTESIAN_POINT ( 'NONE',  ( -6.555530967407501741, 7.606873202518897870, 1.199719254218450271 ) ) ;
#14141 = CARTESIAN_POINT ( 'NONE',  ( -7.598418745816086783, 7.829519723065708092, 0.000000000000000000 ) ) ;
#14142 = CARTESIAN_POINT ( 'NONE',  ( 1.294752383181968503, 1.788903229852260246, -1.265732775075766092 ) ) ;
#14143 = CARTESIAN_POINT ( 'NONE',  ( 4.555176424511575561, 4.416720038126027426, -0.7216878364870188411 ) ) ;
#14144 = ORIENTED_EDGE ( 'NONE', *, *, #16612, .T. ) ;
#14145 = CARTESIAN_POINT ( 'NONE',  ( 0.3999999999999922506, 3.949999999999971756, -0.8338124244296082344 ) ) ;
#14146 = DIRECTION ( 'NONE',  ( -0.6507913734559640506, -0.7592566023653004592, 0.000000000000000000 ) ) ;
#14148 = ADVANCED_FACE ( 'NONE', ( #165114 ), #10644, .T. ) ;
#14147 = CARTESIAN_POINT ( 'NONE',  ( 1.998415063578623085, -0.4859047700337820741, -1.759764234465097221 ) ) ;
#14149 = DIRECTION ( 'NONE',  ( 0.9446243521954068578, -4.336808689942003852E-14, 0.3281536732072456997 ) ) ;
#14150 = CARTESIAN_POINT ( 'NONE',  ( -6.453559683527718249, 6.864596255245277057, -0.6992757447422948136 ) ) ;
#14151 = CARTESIAN_POINT ( 'NONE',  ( 6.509000000000037645, 2.054060622569788386, 2.307050226316338382 ) ) ;
#14152 = CARTESIAN_POINT ( 'NONE',  ( 7.879259827836241570, 12.34422023245099176, 1.040834085586084257E-14 ) ) ;
#14153 = CARTESIAN_POINT ( 'NONE',  ( 0.2055245034400269288, -0.5150763003200479195, 1.856310442892949553 ) ) ;
#14154 = CARTESIAN_POINT ( 'NONE',  ( 4.838696733575553743, -1.901848327180942766, -0.4805237247276354928 ) ) ;
#14155 = CARTESIAN_POINT ( 'NONE',  ( -7.015454420067433361, 10.27211502579893754, 1.199719254218453823 ) ) ;
#14156 = CARTESIAN_POINT ( 'NONE',  ( 4.462605117192430804, 8.358123070033169455, 1.040834085586084257E-14 ) ) ;
#14157 = CARTESIAN_POINT ( 'NONE',  ( 4.511385190476093321, -2.149204750630455241, 0.4279282578087198474 ) ) ;
#14158 = AXIS2_PLACEMENT_3D ( 'NONE', #210268, #64036, #209194 ) ;
#14159 = CARTESIAN_POINT ( 'NONE',  ( 3.662674053986138656, 7.424870162959149589, 0.7998128361456321445 ) ) ;
#14160 = CARTESIAN_POINT ( 'NONE',  ( 4.504778988403771223, 0.5471568804141565545, 1.996604337080605474 ) ) ;
#14161 = CARTESIAN_POINT ( 'NONE',  ( 0.6823417656249899377, 1.655208333674752730, 1.181850606188755259 ) ) ;
#14162 = ORIENTED_EDGE ( 'NONE', *, *, #124080, .T. ) ;
#14163 = CARTESIAN_POINT ( 'NONE',  ( 3.745041490520171212, 2.281215052333289250, -0.2826575254791847680 ) ) ;
#14164 = CARTESIAN_POINT ( 'NONE',  ( 8.120970824905713314, 8.576813505252564696, 1.040834085586084257E-14 ) ) ;
#14166 = CARTESIAN_POINT ( 'NONE',  ( 3.285556943750000514, -0.6635416661887083567, 1.896917185911906500 ) ) ;
#14165 = CARTESIAN_POINT ( 'NONE',  ( 5.560252395380206103, 8.540692657035327429, 1.082531754730547524 ) ) ;
#14168 = EDGE_CURVE ( 'NONE', #23324, #85368, #93570, .T. ) ;
#14167 = FACE_OUTER_BOUND ( 'NONE', #190762, .T. ) ;
#14169 = DIRECTION ( 'NONE',  ( 1.000000000000000000, 0.000000000000000000, 0.000000000000000000 ) ) ;
#14170 = CARTESIAN_POINT ( 'NONE',  ( 3.574105527548767647, -1.871835235816914578, -0.5168888941823551741 ) ) ;
#14171 = ORIENTED_EDGE ( 'NONE', *, *, #111938, .F. ) ;
#14172 = CARTESIAN_POINT ( 'NONE',  ( 10.68346185744421462, 11.56638637654751989, 0.000000000000000000 ) ) ;
#14173 = EDGE_CURVE ( 'NONE', #29350, #88820, #120799, .T. ) ;
#14174 = CARTESIAN_POINT ( 'NONE',  ( 5.379139070037473935, -1.731557697741787916, -0.8120211572784155063 ) ) ;
#14175 = SURFACE_SIDE_STYLE ('',( #49903 ) ) ;
#14176 = CARTESIAN_POINT ( 'NONE',  ( 4.717633463169556229, -1.691034389814783712, 0.3384810450017295969 ) ) ;
#14177 = CARTESIAN_POINT ( 'NONE',  ( 4.100796195634116792, 1.845626398921360822, 0.8128187495666516771 ) ) ;
#14178 = CARTESIAN_POINT ( 'NONE',  ( 4.975319123388493914, -2.281077821084981583, -0.2834334243917625562 ) ) ;
#14179 = CARTESIAN_POINT ( 'NONE',  ( -2.060660350337629509, 8.500464906089689521, 2.499999999999999556 ) ) ;
#14180 = CARTESIAN_POINT ( 'NONE',  ( 0.4521680116954321371, 0.6883007682146925488, -2.096869779678663281 ) ) ;
#14182 = CARTESIAN_POINT ( 'NONE',  ( -3.824808732831001201, 7.476377598362539345, 0.7216878364870338292 ) ) ;
#14181 = CARTESIAN_POINT ( 'NONE',  ( -3.841022230581641050, 7.492630022202825479, -0.07115184559442505607 ) ) ;
#14183 = CARTESIAN_POINT ( 'NONE',  ( 5.641803817319237524, 0.7161603046910887116, -1.618556768665664114 ) ) ;
#14184 = CARTESIAN_POINT ( 'NONE',  ( 5.115861365725078436, 0.1511377038382749338, 2.010826595755777824 ) ) ;
#14186 = CARTESIAN_POINT ( 'NONE',  ( 2.221020806870691366, 0.002245647979397680065, 2.292435215953308791 ) ) ;
#14185 = CARTESIAN_POINT ( 'NONE',  ( 4.715203562502613188, 8.723097599553565118, 0.7998128361456341429 ) ) ;
#14187 = CARTESIAN_POINT ( 'NONE',  ( 1.060061488152568510, -1.571881217706198042, -0.7472303940359821262 ) ) ;
#14188 = CIRCLE ( 'NONE', #135302, 0.4000000000000001887 ) ;
#14189 = CARTESIAN_POINT ( 'NONE',  ( -2.624193383061824036, -0.3882907696143628185, -0.1722368472184268029 ) ) ;
#14190 = CARTESIAN_POINT ( 'NONE',  ( 1.088703816646944267, 1.038853075768126910, -1.387971508864824788 ) ) ;
#14191 = CARTESIAN_POINT ( 'NONE',  ( -1.360316468750042862, 0.9010416670080622081, -0.7853790794159041244 ) ) ;
#14192 = DIRECTION ( 'NONE',  ( 1.000000000000000000, -0.000000000000000000, 1.224646799147353207E-16 ) ) ;
#14193 = CARTESIAN_POINT ( 'NONE',  ( 1.117902646172004522, 0.4237721370383492059, -2.129260471988907000 ) ) ;
#14194 = CARTESIAN_POINT ( 'NONE',  ( 2.448454179885679149, -1.387098808145654560, 1.463928423225707931 ) ) ;
#14195 = CARTESIAN_POINT ( 'NONE',  ( -1.500000000000015099, 0.9104166673494835660, -0.8660254037844313801 ) ) ;
#14196 = CARTESIAN_POINT ( 'NONE',  ( 6.721331456258776704, -0.1291123375851965516, 1.896827325797964869 ) ) ;
#14197 = CARTESIAN_POINT ( 'NONE',  ( -8.012344526598182026E-15, 13.29687500034140157, -1.575800808251669460 ) ) ;
#14198 = CARTESIAN_POINT ( 'NONE',  ( 2.848112528106065078, -1.494902295879830589, -1.643281164644925907 ) ) ;
#14199 = ORIENTED_EDGE ( 'NONE', *, *, #74843, .F. ) ;
#14200 = CARTESIAN_POINT ( 'NONE',  ( 6.649736275991402934, -8.039737506397919731, 6.784764760059098343 ) ) ;
#14201 = CARTESIAN_POINT ( 'NONE',  ( 1.499999999999987121, -0.9958333333333134751, 0.8660254037844524744 ) ) ;
#14202 = CARTESIAN_POINT ( 'NONE',  ( 7.079328764629950754, 11.41096732537697633, 0.7998128361456462443 ) ) ;
#14203 = CARTESIAN_POINT ( 'NONE',  ( 5.899919523139840472, -0.6348737135929006792, -1.620717943835482844 ) ) ;
#14205 = CARTESIAN_POINT ( 'NONE',  ( 3.402741375674179114, 0.4741672551989496998, 1.903589013717405853 ) ) ;
#14204 = MECHANICAL_DESIGN_GEOMETRIC_PRESENTATION_REPRESENTATION (  '', ( #52270 ), #169921 ) ;
#14207 = CARTESIAN_POINT ( 'NONE',  ( -6.073689629242151611, 10.02979563418376685, -0.7216878364870278340 ) ) ;
#14206 = CARTESIAN_POINT ( 'NONE',  ( 2.347533153460546806, 5.890539112345938300, 0.000000000000000000 ) ) ;
#14208 = CARTESIAN_POINT ( 'NONE',  ( 11.84668730067608600, 10.89999999999998259, 1.399999999999998579 ) ) ;
#14209 = CARTESIAN_POINT ( 'NONE',  ( 4.253392140805613231, -1.877938019876054243, -1.261413133637336204 ) ) ;
#14210 = CARTESIAN_POINT ( 'NONE',  ( 0.7661727470247855498, -2.052889565338772204, 0.2005107248105562623 ) ) ;
#14211 = CARTESIAN_POINT ( 'NONE',  ( -5.194745412330402878, 9.212286747694129474, 0.000000000000000000 ) ) ;
#14212 = CARTESIAN_POINT ( 'NONE',  ( 2.342968712349004168, 0.4955985968413346709, 2.207426715909040826 ) ) ;
#14213 = VERTEX_POINT ( 'NONE', #25255 ) ;
#14214 = CARTESIAN_POINT ( 'NONE',  ( -1.499999999999997780, 1.681250000682817047, 0.000000000000000000 ) ) ;
#14215 = CARTESIAN_POINT ( 'NONE',  ( 3.444469828353763141, 0.4513171681363346566, 1.815172769691273835 ) ) ;
#14216 = CARTESIAN_POINT ( 'NONE',  ( 2.689770611714628945, 1.466270380367465043, 0.9255270069659697896 ) ) ;
#14217 = CARTESIAN_POINT ( 'NONE',  ( 6.620655732516649294, -0.002413161512292843602, 2.173887093218459743 ) ) ;
#14218 = CARTESIAN_POINT ( 'NONE',  ( 0.2005908178989434243, -2.206344910233990486, -0.05143828380192031619 ) ) ;
#14219 = CARTESIAN_POINT ( 'NONE',  ( 4.329101982860062314, 0.1031891237209987822, 2.159356164053369387 ) ) ;
#14220 = CARTESIAN_POINT ( 'NONE',  ( 4.505766059781188382, -0.8317635995198893184, -1.754939027834252485 ) ) ;
#14221 = CARTESIAN_POINT ( 'NONE',  ( -9.642873567817536795, 12.27310513391906532, 1.599625672291281386 ) ) ;
#14222 = CARTESIAN_POINT ( 'NONE',  ( 6.274654046616443992, -1.776150972019393093, -0.5868208112121617859 ) ) ;
#14223 = CARTESIAN_POINT ( 'NONE',  ( 4.244147651705390878, 7.284590634535035747, 0.9143829328417275581 ) ) ;
#14224 = LINE ( 'NONE', #11035, #58873 ) ;
#14225 = CARTESIAN_POINT ( 'NONE',  ( 11.86687934130374522, 12.49048050383441755, 1.056332641424306606 ) ) ;
#14226 = CARTESIAN_POINT ( 'NONE',  ( 0.000000000000000000, -9.919999999999998153, 0.000000000000000000 ) ) ;
#14227 = CARTESIAN_POINT ( 'NONE',  ( 5.942029771888944545, -1.730864577151491890, -1.034168155301495862 ) ) ;
#14228 = CARTESIAN_POINT ( 'NONE',  ( -8.292783513053063160, 12.82666453187061073, 0.7998128361456481317 ) ) ;
#14229 = CARTESIAN_POINT ( 'NONE',  ( 6.923409998072794558, 11.22906209772695618, 1.040834085586084257E-14 ) ) ;
#14230 = CARTESIAN_POINT ( 'NONE',  ( 3.444653546323793947, 6.176457016423196222, 1.199719254218451159 ) ) ;
#14232 = CARTESIAN_POINT ( 'NONE',  ( -6.725445687907764203, -7.162053774861991684, 6.710127771514628137 ) ) ;
#14231 = CARTESIAN_POINT ( 'NONE',  ( 3.105874302609371362, -1.823586186413633126, 0.09019715141062728536 ) ) ;
#14233 = DIRECTION ( 'NONE',  ( 1.000000000000000000, -4.985516615831701596E-16, 0.000000000000000000 ) ) ;
#14234 = ORIENTED_EDGE ( 'NONE', *, *, #173298, .F. ) ;
#14235 = CARTESIAN_POINT ( 'NONE',  ( -4.299344108864953995, 7.069632989434141201, -1.082531754730551743 ) ) ;
#14236 = UNCERTAINTY_MEASURE_WITH_UNIT (LENGTH_MEASURE( 1.000000000000000082E-05 ), #133148, 'distance_accuracy_value', 'NONE');
#14237 = FACE_OUTER_BOUND ( 'NONE', #7245, .T. ) ;
#14238 = CARTESIAN_POINT ( 'NONE',  ( -8.483651433849100698, 10.92067931095586886, 1.599625672291269396 ) ) ;
#14239 = CARTESIAN_POINT ( 'NONE',  ( -0.01731643392406666954, -1.316173432332496507, 1.532187831819804780 ) ) ;
#14240 = CARTESIAN_POINT ( 'NONE',  ( 1.524255003590764046, -2.104078925693805502, 0.2628582283784736684 ) ) ;
#14241 = ORIENTED_EDGE ( 'NONE', *, *, #65049, .T. ) ;
#14242 = CARTESIAN_POINT ( 'NONE',  ( -4.762657100150483380, 8.778460060142702304, 0.000000000000000000 ) ) ;
#14243 = CARTESIAN_POINT ( 'NONE',  ( 2.184208379282841950, 1.076359544750982389, -1.517863362848305808 ) ) ;
#14244 = CARTESIAN_POINT ( 'NONE',  ( 4.436542580169809291, 6.199052314996659874, 1.599625672291267398 ) ) ;
#14245 = CARTESIAN_POINT ( 'NONE',  ( 6.508673417949426110, 1.528841652884159963, -1.382195874861185336 ) ) ;
#14246 = CARTESIAN_POINT ( 'NONE',  ( 5.924453975591452703, -1.462443569488897754, -1.388487997949397368 ) ) ;
#14247 = VERTEX_POINT ( 'NONE', #87060 ) ;
#14248 = ORIENTED_EDGE ( 'NONE', *, *, #40321, .F. ) ;
#14249 = AXIS2_PLACEMENT_3D ( 'NONE', #112344, #97115, #31040 ) ;
#14250 = CARTESIAN_POINT ( 'NONE',  ( 0.000000000000000000, -4.000000000000003553, 0.000000000000000000 ) ) ;
#14252 = ADVANCED_FACE ( 'NONE', ( #103316 ), #157417, .T. ) ;
#14251 = CARTESIAN_POINT ( 'NONE',  ( -0.2108831679771167866, 1.375689764684871808, -2.152500126786048185 ) ) ;
#14253 = AXIS2_PLACEMENT_3D ( 'NONE', #57190, #58255, #123350 ) ;
#14256 = VERTEX_POINT ( 'NONE', #6852 ) ;
#14255 = DIRECTION ( 'NONE',  ( 0.7592566023653003482, 0.6507913734559641616, 0.000000000000000000 ) ) ;
#14254 = CARTESIAN_POINT ( 'NONE',  ( -4.685224601974262271, 7.623789914682047808, -1.199719254218453823 ) ) ;
#14257 = CARTESIAN_POINT ( 'NONE',  ( 5.869365784521903606, 7.282179437329668659, 1.264975801879052453 ) ) ;
#14258 = CARTESIAN_POINT ( 'NONE',  ( 5.835314490094169138, -1.281163661392352493, 1.556671411349755285 ) ) ;
#14259 = CARTESIAN_POINT ( 'NONE',  ( 4.171694865975253741, -1.058263924308279424, 1.506412014522513720 ) ) ;
#14260 = AXIS2_PLACEMENT_3D ( 'NONE', #175846, #56744, #24217 ) ;
#14261 = CARTESIAN_POINT ( 'NONE',  ( -0.02299388927988389730, 0.001624902753813092359, -1.910968047046639251 ) ) ;
#14262 = CARTESIAN_POINT ( 'NONE',  ( 3.545847025713305012, -1.747029255069532550, -1.507864240153370172 ) ) ;
#14263 = CARTESIAN_POINT ( 'NONE',  ( 5.936491157937257235, 8.019268665717216749, 1.599625672291268286 ) ) ;
#14264 = CARTESIAN_POINT ( 'NONE',  ( 6.520800673124607982, 2.014292100380775885, 0.7847517145297827623 ) ) ;
#14265 = CARTESIAN_POINT ( 'NONE',  ( 0.7318534483069280006, 1.913536139905326339, 0.3307262847246707493 ) ) ;
#14266 = CARTESIAN_POINT ( 'NONE',  ( -5.623934791570306402, 5.455678766453782913, 0.7998128361456341429 ) ) ;
#14267 = ORIENTED_EDGE ( 'NONE', *, *, #72253, .T. ) ;
#14268 = CARTESIAN_POINT ( 'NONE',  ( 4.534687899768989006, 2.230887184458398398, -0.5525863250545393068 ) ) ;
#14269 = CARTESIAN_POINT ( 'NONE',  ( -10.99970480893081870, -5.907420853759282053, -0.08058608058607828750 ) ) ;
#14270 = CARTESIAN_POINT ( 'NONE',  ( -4.118644803501354978, 8.027112380718707030, 0.7998128361456352531 ) ) ;
#14271 = CARTESIAN_POINT ( 'NONE',  ( 5.049604242677837362, 0.5861553263475408615, -1.776501995420045832 ) ) ;
#14274 = CARTESIAN_POINT ( 'NONE',  ( -3.786470039966538970, 7.639575156594750283, 0.000000000000000000 ) ) ;
#14273 = CARTESIAN_POINT ( 'NONE',  ( -0.7500000000000249800, -0.2770833326505156569, 1.299038105676659116 ) ) ;
#14272 = CARTESIAN_POINT ( 'NONE',  ( 1.019614524654769872, -0.4619345408787678964, 1.855657206939323789 ) ) ;
#14275 = CARTESIAN_POINT ( 'NONE',  ( 2.455956380646412196, 0.5873987694336445520, -2.127207350628975924 ) ) ;
#14276 = CARTESIAN_POINT ( 'NONE',  ( 6.883263157960367806, 0.5819222519044697783, 1.998722019247618276 ) ) ;
#14277 = CARTESIAN_POINT ( 'NONE',  ( 2.367870383881045981, 5.914265881169853856, 0.000000000000000000 ) ) ;
#14278 = CARTESIAN_POINT ( 'NONE',  ( 5.953438849732186178, 8.999410187112612647, -1.082531754730548412 ) ) ;
#14279 = CARTESIAN_POINT ( 'NONE',  ( -2.300079615812729905, 5.835176651756807331, -0.7998128361456281477 ) ) ;
#14280 = CARTESIAN_POINT ( 'NONE',  ( -6.468648687051513413, 7.679749902049126220, 1.082531754730549078 ) ) ;
#14281 = CARTESIAN_POINT ( 'NONE',  ( 1.282427153303007605, -1.922404290768309432, -0.4359020612285709473 ) ) ;
#14282 = CARTESIAN_POINT ( 'NONE',  ( 1.132322824279883955, -1.466084937595305560, -1.782028031347275832 ) ) ;
#14283 = CARTESIAN_POINT ( 'NONE',  ( 2.066782613880484565, 1.455849762852476248, -1.315278764014264912 ) ) ;
#14284 = CARTESIAN_POINT ( 'NONE',  ( 5.577030875653865571, 1.903616248300431746, 0.7944661687919268855 ) ) ;
#14285 = CARTESIAN_POINT ( 'NONE',  ( 3.714570900464274850, 6.317121236308204324, 1.082531754730558626 ) ) ;
#14286 = CARTESIAN_POINT ( 'NONE',  ( 6.042093733545556233, 7.078139439671806699, -1.199719254218452047 ) ) ;
#14287 = VERTEX_POINT ( 'NONE', #202920 ) ;
#14288 = CARTESIAN_POINT ( 'NONE',  ( 0.6823417656249899377, 5.488541667008087543, -1.181850606188754593 ) ) ;
#14289 = FACE_OUTER_BOUND ( 'NONE', #11192, .T. ) ;
#14290 = CARTESIAN_POINT ( 'NONE',  ( 8.886479618753304166, 12.45497775759917758, -1.199719254218446718 ) ) ;
#14291 = CARTESIAN_POINT ( 'NONE',  ( 0.4972420419220639487, 0.3698279840313797862, 2.139175918340649574 ) ) ;
#14293 = CARTESIAN_POINT ( 'NONE',  ( 4.296393142825893463, 0.4330127018922214077, -4.470011852588159584 ) ) ;
#14292 = CARTESIAN_POINT ( 'NONE',  ( -0.08058962652509195357, -9.910877166163972518, -10.99970478295253606 ) ) ;
#14294 = CARTESIAN_POINT ( 'NONE',  ( 11.33772463945043718, 10.90000000000000924, -3.600000000000078693 ) ) ;
#14295 = CARTESIAN_POINT ( 'NONE',  ( -3.475000000000000533, -1.750000000000001554, 0.000000000000000000 ) ) ;
#14296 = CARTESIAN_POINT ( 'NONE',  ( 2.284254421533092216, -1.833544361078912388, -0.3693468884775340522 ) ) ;
#14297 = CARTESIAN_POINT ( 'NONE',  ( 6.749309733681256418, -1.731629633356733589, -1.293610171197785652 ) ) ;
#14299 = ADVANCED_FACE ( 'NONE', ( #72930 ), #32815, .T. ) ;
#14298 = CARTESIAN_POINT ( 'NONE',  ( -5.679923764332232672, 6.292470487948599533, 1.134535232271353999 ) ) ;
#14301 = CARTESIAN_POINT ( 'NONE',  ( 6.827182134110164391, 0.5838490905608649806, 1.963161153048794905 ) ) ;
#14300 = CARTESIAN_POINT ( 'NONE',  ( -0.02244404828160087226, 4.081832076214893412, -2.743766916979750281 ) ) ;
#14302 = CARTESIAN_POINT ( 'NONE',  ( 1.364683531249986537, -0.8864583329919110133, 0.7879004041258500513 ) ) ;
#14303 = CARTESIAN_POINT ( 'NONE',  ( 2.104032245951466429, -0.8162354410432022256, 1.729450509904674416 ) ) ;
#14304 = CARTESIAN_POINT ( 'NONE',  ( 3.625649997064513297, -1.053871202854910871, -1.421704988934450409 ) ) ;
#14305 = CARTESIAN_POINT ( 'NONE',  ( 2.367698891403247519, 0.5082884949165042965, -1.843433491391050838 ) ) ;
#14306 = CARTESIAN_POINT ( 'NONE',  ( -6.403528624356093601, 6.365204904703887223, 1.040834085586084257E-14 ) ) ;
#14308 = CARTESIAN_POINT ( 'NONE',  ( 5.536718839138406345, -1.507006759595967305, 1.182436279247323085 ) ) ;
#14307 = CARTESIAN_POINT ( 'NONE',  ( 1.258396710555287346, -3.152325552749383863, -3.126779214646796756 ) ) ;
#14309 = CARTESIAN_POINT ( 'NONE',  ( 0.2036857628631080219, -1.599406074100502506, -1.314310892166506095 ) ) ;
#14310 = CARTESIAN_POINT ( 'NONE',  ( 1.499999999999990896, 4.775000000000022560, 1.214306433183764966E-14 ) ) ;
#14312 = EDGE_CURVE ( 'NONE', #144299, #39263, #113849, .T. ) ;
#14311 = CARTESIAN_POINT ( 'NONE',  ( 1.793382672576701919, -0.1090974814243403090, -2.117938670719583527 ) ) ;
#14313 = DIRECTION ( 'NONE',  ( 0.000000000000000000, 0.000000000000000000, 1.000000000000000000 ) ) ;
#14314 = CARTESIAN_POINT ( 'NONE',  ( 4.785944050937030347, -0.8815013282119155136, 1.649949660215948688 ) ) ;
#14316 = EDGE_LOOP ( 'NONE', ( #108492, #41932, #194808, #161749 ) ) ;
#14315 = CARTESIAN_POINT ( 'NONE',  ( 0.5744775230259161480, -1.718042477583326066, -0.6180270036199516648 ) ) ;
#14318 = CARTESIAN_POINT ( 'NONE',  ( 4.735857411151594754, 8.202189375375613878, -0.7076125000919450958 ) ) ;
#14317 = CARTESIAN_POINT ( 'NONE',  ( 4.512475528931441104, -0.9420208833846724916, -1.995868093903986118 ) ) ;
#14319 = CARTESIAN_POINT ( 'NONE',  ( 1.364683531249986981, -1.115624999658580752, 0.000000000000000000 ) ) ;
#14320 = CARTESIAN_POINT ( 'NONE',  ( 1.328664801108740523, -1.309985447229580213, 1.593267124675311841 ) ) ;
#14322 = ADVANCED_FACE ( 'NONE', ( #46875 ), #115733, .T. ) ;
#14321 = CARTESIAN_POINT ( 'NONE',  ( 5.829115978871627135, 8.888053511070525659, 1.199719254218462483 ) ) ;
#14323 = CARTESIAN_POINT ( 'NONE',  ( -7.069687034522070590, 10.33538640932937724, -1.199719254218440723 ) ) ;
#14324 = CARTESIAN_POINT ( 'NONE',  ( 10.21336978979620191, 10.81001959771741205, 0.7998128361456462443 ) ) ;
#14325 = CARTESIAN_POINT ( 'NONE',  ( 1.424698021954186711, 3.742711217035210147, -0.4926413923218386781 ) ) ;
#14326 = AXIS2_PLACEMENT_3D ( 'NONE', #208233, #59865, #126017 ) ;
#14327 = CARTESIAN_POINT ( 'NONE',  ( 0.9999999999999833467, 8.600000000000013856, 0.4000000000000014655 ) ) ;
#14328 = DIRECTION ( 'NONE',  ( -0.9486832980505139901, -0.3162277660168373861, 3.312310031615527941E-15 ) ) ;
#14329 = EDGE_LOOP ( 'NONE', ( #102177, #100842, #104147, #211135, #136774 ) ) ;
#14330 = B_SPLINE_CURVE_WITH_KNOTS ( 'NONE', 3,
 ( #146958, #126499, #209776, #62478, #212973, #145903, #46250 ),
 .UNSPECIFIED., .F., .F.,
 ( 4, 3, 4 ),
 ( 0.000000000000000000, 0.0008000000000005097218, 0.002977368225425562533 ),
 .UNSPECIFIED. ) ;
#14331 = CARTESIAN_POINT ( 'NONE',  ( 3.771986465066007099, -2.040223509676724500, 0.3510349978646867264 ) ) ;
#14332 = CARTESIAN_POINT ( 'NONE',  ( -0.7499999999999972244, 5.358333333333353821, -1.299038105676652011 ) ) ;
#14333 = CARTESIAN_POINT ( 'NONE',  ( 2.056162960589353883, 2.155939639820044107, -0.1567802445739118478 ) ) ;
#14334 = CARTESIAN_POINT ( 'NONE',  ( -6.165548087794384458, 6.979908488848794335, -0.9162763116292941268 ) ) ;
#14335 = CARTESIAN_POINT ( 'NONE',  ( 2.016276777042900203, -2.019190368190917795, 0.05175015523710930349 ) ) ;
#14336 = CARTESIAN_POINT ( 'NONE',  ( -5.204170427930421283E-15, 4.000000000000003553, -11.99999999999998224 ) ) ;
#14337 = PRODUCT ( 'positive pin', 'positive pin', '', ( #198820 ) ) ;
#14338 = ORIENTED_EDGE ( 'NONE', *, *, #36355, .F. ) ;
#14339 = ORIENTED_EDGE ( 'NONE', *, *, #130004, .F. ) ;
#14341 = CARTESIAN_POINT ( 'NONE',  ( 6.616015773788773480, 10.66250946948817813, -0.7216878364870267237 ) ) ;
#14340 = CARTESIAN_POINT ( 'NONE',  ( 1.737500000000001155, -3.383333333333331971, 3.009438278150922130 ) ) ;
#14342 = FACE_OUTER_BOUND ( 'NONE', #161977, .T. ) ;
#14343 = CARTESIAN_POINT ( 'NONE',  ( -3.973948422136981407, 5.729635473950147606, -1.443375672974066548 ) ) ;
#14344 = CARTESIAN_POINT ( 'NONE',  ( -0.1706859984542466180, -1.561801110730935971, -1.275320528755889526 ) ) ;
#14345 = CARTESIAN_POINT ( 'NONE',  ( 4.968408144156592599, -2.063508908063705238, -0.7385586828293492223 ) ) ;
#14346 = CARTESIAN_POINT ( 'NONE',  ( 1.499999999999990896, 5.056250000682820378, 1.214306433183764966E-14 ) ) ;
#14347 = CARTESIAN_POINT ( 'NONE',  ( 4.131050151015442928, 1.750605847248308145, 0.7702136748066327199 ) ) ;
#14348 = CARTESIAN_POINT ( 'NONE',  ( -4.603156847039612920, 5.329103395422994716, 1.199719254218462483 ) ) ;
#14349 = CARTESIAN_POINT ( 'NONE',  ( 5.300874872818828187, 8.167809204055208383, 1.082531754730558626 ) ) ;
#14351 = CARTESIAN_POINT ( 'NONE',  ( 2.302361438560030393, 1.314982760645909465, -1.528754769246756018 ) ) ;
#14350 = CARTESIAN_POINT ( 'NONE',  ( -7.795575137733361970, 12.03866206075687018, 0.7216878364870458196 ) ) ;
#14352 = CARTESIAN_POINT ( 'NONE',  ( 0.6823417656249934904, 12.75520833367473017, 1.181850606188764807 ) ) ;
#14353 = CARTESIAN_POINT ( 'NONE',  ( -4.573896719763875574, 6.429575154514868274, -1.599625672291271394 ) ) ;
#14354 = CARTESIAN_POINT ( 'NONE',  ( 5.086778385480665854, -0.2138867007538784171, -1.711364050844576434 ) ) ;
#14355 = CARTESIAN_POINT ( 'NONE',  ( 0.1405533004714279999, 2.862415582289945526, -2.767767315042678700 ) ) ;
#14356 = CARTESIAN_POINT ( 'NONE',  ( 10.39874063200158893, 11.23421161353111586, 0.000000000000000000 ) ) ;
#14357 = AXIS2_PLACEMENT_3D ( 'NONE', #75561, #209803, #77685 ) ;
#14358 = LINE ( 'NONE', #111955, #147339 ) ;
#14359 = CARTESIAN_POINT ( 'NONE',  ( 0.000000000000000000, 12.21999999999998288, 0.000000000000000000 ) ) ;
#14360 = ORIENTED_EDGE ( 'NONE', *, *, #154706, .T. ) ;
#14361 = DIRECTION ( 'NONE',  ( -3.451266460341926649E-31, -5.200009205990155575E-32, 1.000000000000000000 ) ) ;
#14362 = ORIENTED_EDGE ( 'NONE', *, *, #14825, .F. ) ;
#14363 = CARTESIAN_POINT ( 'NONE',  ( 4.512255818007496977, -1.811207030272870000, -0.03965706671436861758 ) ) ;
#14364 = CARTESIAN_POINT ( 'NONE',  ( 4.583538449871731757, 7.505156070562471804, 1.199719254218451159 ) ) ;
#14365 = DIRECTION ( 'NONE',  ( 0.000000000000000000, 1.804652791718263484E-16, -1.000000000000000000 ) ) ;
#14366 = CARTESIAN_POINT ( 'NONE',  ( 6.586573151046549945, -1.108064789702201569, 1.433474704228101748 ) ) ;
#14367 = CARTESIAN_POINT ( 'NONE',  ( 5.872089928050205465, 6.023395468912922546, -0.7216878364870458196 ) ) ;
#14368 = CARTESIAN_POINT ( 'NONE',  ( -11.91826849282518452, 10.19999999999999929, -1.400000000000001465 ) ) ;
#14369 = CARTESIAN_POINT ( 'NONE',  ( 3.064592470464472473, -2.024993410009158890, -0.8382372354380845936 ) ) ;
#14370 = AXIS2_PLACEMENT_3D ( 'NONE', #176347, #74579, #43169 ) ;
#14372 = CARTESIAN_POINT ( 'NONE',  ( 9.725276259704228821, 10.24057714594344048, 0.7998128361456462443 ) ) ;
#14371 = CARTESIAN_POINT ( 'NONE',  ( 6.848144937404742727, -0.7948834574948275833, 1.681425573653466676 ) ) ;
#14373 = CARTESIAN_POINT ( 'NONE',  ( 5.360912872498101223, -0.05169663686300975808, -1.915091480415902048 ) ) ;
#14374 = CARTESIAN_POINT ( 'NONE',  ( -1.364683531249997417, 5.821875000341418804, 1.214306433183764966E-14 ) ) ;
#14375 = DIRECTION ( 'NONE',  ( -1.000000000000000000, 0.000000000000000000, 0.000000000000000000 ) ) ;
#14376 = CARTESIAN_POINT ( 'NONE',  ( 0.6823417656249882723, -0.6572916663252492686, 1.181850606188755259 ) ) ;
#14377 = CARTESIAN_POINT ( 'NONE',  ( 5.422898255786183341, 7.349800603215774331, -1.443375672974051449 ) ) ;
#14378 = CARTESIAN_POINT ( 'NONE',  ( -8.134528978519403708, 11.47373899403920205, 1.082531754730549967 ) ) ;
#14379 = CARTESIAN_POINT ( 'NONE',  ( 1.762795743007524063, -1.528684080660724920, 1.528680807790387286 ) ) ;
#14380 = CARTESIAN_POINT ( 'NONE',  ( -4.664887371553763096, 7.600063145858131364, -1.199719254218453823 ) ) ;
#14381 = CARTESIAN_POINT ( 'NONE',  ( 3.217027588192558074, 6.975225629525113824, -1.734723475976807094E-15 ) ) ;
#14382 = CARTESIAN_POINT ( 'NONE',  ( 1.412830140145465263, 1.608106816955911178, 0.8641515426408912237 ) ) ;
#14383 = CARTESIAN_POINT ( 'NONE',  ( -4.790108344329849110, 4.482881244673243337, 0.7998128361456341429 ) ) ;
#14384 = CARTESIAN_POINT ( 'NONE',  ( 4.471595891589618788, 1.770651423122941548, -0.4439726157009425411 ) ) ;
#14385 = ADVANCED_FACE ( 'NONE', ( #190 ), #3034, .T. ) ;
#14386 = CARTESIAN_POINT ( 'NONE',  ( 10.16691492120896712, 10.85832867828739090, -8.127724911529011109 ) ) ;
#14387 = CARTESIAN_POINT ( 'NONE',  ( 2.988426722125224977, -1.135634098421594240, 1.538566774472991616 ) ) ;
#14388 = ORIENTED_EDGE ( 'NONE', *, *, #212165, .T. ) ;
#14389 = CARTESIAN_POINT ( 'NONE',  ( 3.930098287398839041, 1.092129198686382141, 1.638800773490353802 ) ) ;
#14390 = VERTEX_POINT ( 'NONE', #1266 ) ;
#14391 = CARTESIAN_POINT ( 'NONE',  ( 4.950698622930713277, -1.642605121802564350, -1.035792469189389386 ) ) ;
#14392 = EDGE_LOOP ( 'NONE', ( #110334, #150269, #110375, #15961 ) ) ;
#14393 = CARTESIAN_POINT ( 'NONE',  ( -6.936931872047518155, 8.122117267924091166, 1.199719254218452047 ) ) ;
#14395 = CARTESIAN_POINT ( 'NONE',  ( 5.449516625918088053, -1.916229881892789866, 0.9086369058012438993 ) ) ;
#14394 = CARTESIAN_POINT ( 'NONE',  ( 4.857564175446106525, 8.889184981320973122, 0.7998128361456331437 ) ) ;
#14396 = CARTESIAN_POINT ( 'NONE',  ( -4.450244736158147418, 7.987476157872628768, -2.500000000000000444 ) ) ;
#14397 = ORIENTED_EDGE ( 'NONE', *, *, #185383, .T. ) ;
#14398 = CARTESIAN_POINT ( 'NONE',  ( 4.983022828693913553, 6.814620138096638691, -1.425645453754071257 ) ) ;
#14399 = DIRECTION ( 'NONE',  ( 0.000000000000000000, 0.000000000000000000, 1.000000000000000000 ) ) ;
#14400 = CARTESIAN_POINT ( 'NONE',  ( 4.634908411025333130, 6.500755460986618495, 1.599625672291268286 ) ) ;
#14401 = CARTESIAN_POINT ( 'NONE',  ( 5.671388329218120639, 5.511041227042920099, 1.040834085586084257E-14 ) ) ;
#14402 = CARTESIAN_POINT ( 'NONE',  ( 4.986981296356192139, -1.896340117422308236, -0.6759883393069978652 ) ) ;
#14404 =( BOUNDED_SURFACE ( )  B_SPLINE_SURFACE ( 3, 1, ( 
 ( #189815, #93415 ),
 ( #41465, #209242 ),
 ( #158396, #60886 ),
 ( #125974, #54755 ),
 ( #76072, #44658 ),
 ( #27311, #110773 ),
 ( #142171, #59821 ) ),
 .UNSPECIFIED., .T., .F., .T. ) 
 B_SPLINE_SURFACE_WITH_KNOTS ( ( 4, 3, 4 ),
 ( 2, 2 ),
 ( 0.000000000000000000, 0.5000000000000000000, 1.000000000000000000 ),
 ( 0.000000000000000000, 1.000000000000000000 ),
 .UNSPECIFIED. ) 
 GEOMETRIC_REPRESENTATION_ITEM ( )  RATIONAL_B_SPLINE_SURFACE ( (
 ( 1.000000000000000000, 1.000000000000000000),
 ( 0.3333333333333333703, 0.3333333333333333703),
 ( 0.3333333333333333703, 0.3333333333333333703),
 ( 1.000000000000000000, 1.000000000000000000),
 ( 0.3333333333333333703, 0.3333333333333333703),
 ( 0.3333333333333333703, 0.3333333333333333703),
 ( 1.000000000000000000, 1.000000000000000000) ) ) 
 REPRESENTATION_ITEM ( '' )  SURFACE ( )  );
#14403 = DIRECTION ( 'NONE',  ( 1.000000000000000000, -0.000000000000000000, -0.000000000000000000 ) ) ;
#14405 = CARTESIAN_POINT ( 'NONE',  ( 4.688025921862073453, -0.8580590012943272171, 1.611482198803436905 ) ) ;
#14406 = CARTESIAN_POINT ( 'NONE',  ( 0.4673438449808891559, 1.800595422158430825, 1.021790579661910003 ) ) ;
#14407 = CARTESIAN_POINT ( 'NONE',  ( -7.537970219518083326, 9.817384560903001045, -1.443375672974059665 ) ) ;
#14408 = STYLED_ITEM ( 'NONE', ( #71261 ), #60652 ) ;
#14409 = CARTESIAN_POINT ( 'NONE',  ( -6.111218785694742195, 7.101581614182197022, 1.130138924470771800 ) ) ;
#14410 = CARTESIAN_POINT ( 'NONE',  ( 3.475000000000000533, -2.931249999044084120, 0.000000000000000000 ) ) ;
#14411 = CARTESIAN_POINT ( 'NONE',  ( 5.418772907935071714, 1.728844841293469159, 0.7149302089985640762 ) ) ;
#14412 = CARTESIAN_POINT ( 'NONE',  ( 6.799577732453452761, 7.891594428405881878, -1.199719254218446718 ) ) ;
#14413 = AXIS2_PLACEMENT_3D ( 'NONE', #198487, #3477, #136723 ) ;
#14414 = CARTESIAN_POINT ( 'NONE',  ( -5.759516327706960759, 5.613857225279885732, -0.7998128361456221525 ) ) ;
#14415 = CARTESIAN_POINT ( 'NONE',  ( 1.364683531249997417, 11.04687500034139802, 2.602085213965210642E-15 ) ) ;
#14416 = CARTESIAN_POINT ( 'NONE',  ( -6.410307701162927252, 6.373113827645189744, -0.7998128361456291469 ) ) ;
#14418 = CARTESIAN_POINT ( 'NONE',  ( -3.648552735408990166, 6.310376387068841630, -1.082531754730546636 ) ) ;
#14417 = CARTESIAN_POINT ( 'NONE',  ( -11.94105721237523099, 10.90000000000000036, -1.187919463087248939 ) ) ;
#14419 = CARTESIAN_POINT ( 'NONE',  ( -6.389970470742427189, 6.349387058821269747, -0.7998128361456291469 ) ) ;
#14420 = CARTESIAN_POINT ( 'NONE',  ( 1.692325190600419305, 1.023896122633965566, -1.799289093316607469 ) ) ;
#14421 = CARTESIAN_POINT ( 'NONE',  ( 2.126704408204147967, 0.4671447874508818932, 2.064898165909804906 ) ) ;
#14422 = CARTESIAN_POINT ( 'NONE',  ( 7.239163954692881653, 10.53310948286200599, -1.199719254218441611 ) ) ;
#14423 = CARTESIAN_POINT ( 'NONE',  ( -0.7500000000000215383, 3.472916667349487785, 1.299038105676671107 ) ) ;
#14424 = CARTESIAN_POINT ( 'NONE',  ( 0.8132587859420150611, -1.660809389245621492, -1.058212622827129357 ) ) ;
#14425 = CARTESIAN_POINT ( 'NONE',  ( 4.954777096267108050, 6.838018505022927407, 1.425084580847448379 ) ) ;
#14426 = CARTESIAN_POINT ( 'NONE',  ( 3.701012746850603996, 7.261672604726938651, 1.040834085586084257E-14 ) ) ;
#14428 = FACE_OUTER_BOUND ( 'NONE', #102166, .T. ) ;
#14427 = CARTESIAN_POINT ( 'NONE',  ( -1.737500000000000266, -3.908333333333333215, -3.009438278150923907 ) ) ;
#14429 = CARTESIAN_POINT ( 'NONE',  ( 3.082263327019618249, -2.258438545724365643, -0.3914850642001906356 ) ) ;
#14431 = ADVANCED_FACE ( 'NONE', ( #97757 ), #196305, .T. ) ;
#14430 = CARTESIAN_POINT ( 'NONE',  ( 0.6447967512687136082, -1.567379569643694515, 0.9359695128687425258 ) ) ;
#14432 = CARTESIAN_POINT ( 'NONE',  ( 2.109489925670060551, 1.480643174185194200, 1.210387159491378650 ) ) ;
#14433 = EDGE_LOOP ( 'NONE', ( #135450, #17726, #27003, #177400 ) ) ;
#14434 = CARTESIAN_POINT ( 'NONE',  ( 6.114364089638775646, 10.07724917131317355, 0.7216878364870438212 ) ) ;
#14435 = CARTESIAN_POINT ( 'NONE',  ( 2.232683648988046610, 1.311727534961094177, -1.527327462066043084 ) ) ;
#14436 = CARTESIAN_POINT ( 'NONE',  ( 1.410910527293834260, -1.549868713165471590, 1.202602906592651788 ) ) ;
#14437 = CARTESIAN_POINT ( 'NONE',  ( -9.267161690140662600, 10.77044237904097734, -1.199719254218441611 ) ) ;
#14438 = CARTESIAN_POINT ( 'NONE',  ( -7.739006755302186846, 7.923262724141010516, 0.7998128361456462443 ) ) ;
#14440 = EDGE_CURVE ( 'NONE', #124, #4829, #2327, .T. ) ;
#14439 = CARTESIAN_POINT ( 'NONE',  ( -11.26783843162779775, 6.407685724923858572, -3.998516562640498151 ) ) ;
#14442 = CARTESIAN_POINT ( 'NONE',  ( 3.168565732603556562, -1.634766719728536266, -0.6786406015907071598 ) ) ;
#14441 = CARTESIAN_POINT ( 'NONE',  ( 3.433613042289254569, 0.9395709039844526433, -1.867677030932006765 ) ) ;
#14443 = CARTESIAN_POINT ( 'NONE',  ( -11.41176686791169281, 13.75950803486851903, 3.404018756831824533 ) ) ;
#14445 = CARTESIAN_POINT ( 'NONE',  ( 6.175753646036172384, -1.231511006544892206, 1.933186584637256678 ) ) ;
#14444 = CARTESIAN_POINT ( 'NONE',  ( 1.579999999999990523, 8.674529973577531194, -2.499999999999989342 ) ) ;
#14446 = CARTESIAN_POINT ( 'NONE',  ( 4.365022556061240344, 1.687170946148343953, -0.4262992432423305389 ) ) ;
#14447 = CARTESIAN_POINT ( 'NONE',  ( 9.077347539549325717, 10.54899253668443393, -1.199719254218446718 ) ) ;
#14448 = CARTESIAN_POINT ( 'NONE',  ( 0.000000000000000000, 19.00000000000000000, 11.18000000000000149 ) ) ;
#14449 = CARTESIAN_POINT ( 'NONE',  ( 4.674945122873967129, -0.7415060156777570910, -1.567401138452922060 ) ) ;
#14450 = CARTESIAN_POINT ( 'NONE',  ( 5.055217142685058285, 1.807878865648751221, -1.202052933306910765 ) ) ;
#14451 = CARTESIAN_POINT ( 'NONE',  ( 4.521807925357579805, 5.234196320127330715, -1.199719254218452047 ) ) ;
#14452 = CARTESIAN_POINT ( 'NONE',  ( 6.227749967195368441, 0.7672974224810541477, -1.865044430435198741 ) ) ;
#14453 = CARTESIAN_POINT ( 'NONE',  ( 4.968750000000002665, 0.7852924748297213098, -1.895863743164188042 ) ) ;
#14454 = CARTESIAN_POINT ( 'NONE',  ( -1.500000000000011324, 4.910416667349486453, -0.8660254037844313801 ) ) ;
#14455 = CARTESIAN_POINT ( 'NONE',  ( 2.836843495735667187, 0.2342426253194809793, 1.912026175940540140 ) ) ;
#14456 = CARTESIAN_POINT ( 'NONE',  ( 1.499999999999997113, 10.17708333401613174, -0.8660254037844378194 ) ) ;
#14457 = CARTESIAN_POINT ( 'NONE',  ( 6.310783679736120533, -0.5911123833974815112, -2.141223572898354188 ) ) ;
#14458 = ORIENTED_EDGE ( 'NONE', *, *, #26377, .T. ) ;
#14459 = CARTESIAN_POINT ( 'NONE',  ( 6.883263157960399781, 2.038134514454426505, 2.350812138539408735 ) ) ;
#14460 = CARTESIAN_POINT ( 'NONE',  ( -1.500000000000013101, 3.629166666666692187, -0.8660254037844313801 ) ) ;
#14461 = CARTESIAN_POINT ( 'NONE',  ( 6.148786358997489820, 7.132337826040578754, -1.199719254218446718 ) ) ;
#14462 = CARTESIAN_POINT ( 'NONE',  ( 1.331071098547026654, 1.488246241617418697, -1.649206797639357180 ) ) ;
#14463 = CARTESIAN_POINT ( 'NONE',  ( -0.7499999999999972244, 4.858333333333353821, -1.299038105676652011 ) ) ;
#14464 = CARTESIAN_POINT ( 'NONE',  ( 6.968527767744093993, 10.11340424813470662, 1.082531754730558626 ) ) ;
#14465 = CARTESIAN_POINT ( 'NONE',  ( -9.070041577417988776, 12.56517035942090388, 1.082531754730558626 ) ) ;
#14467 = EDGE_CURVE ( 'NONE', #14213, #19175, #37703, .T. ) ;
#14466 = CIRCLE ( 'NONE', #176995, 1.852123800559096534 ) ;
#14468 = CARTESIAN_POINT ( 'NONE',  ( 5.011674058906918638, 5.875983152593414971, 1.199719254218452047 ) ) ;
#14469 = CARTESIAN_POINT ( 'NONE',  ( -4.828112100242294424, 5.765790550771681566, -1.082531754730549967 ) ) ;
#14471 = CARTESIAN_POINT ( 'NONE',  ( 5.494603814743470593, 2.031562770168824361, 0.3561260095714424700 ) ) ;
#14470 = CARTESIAN_POINT ( 'NONE',  ( 9.673906298550626559, 11.24497775551929557, 1.199719254218452047 ) ) ;
#14472 = DIRECTION ( 'NONE',  ( 1.000000000000000000, 0.000000000000000000, -0.000000000000000000 ) ) ;
#14473 = CARTESIAN_POINT ( 'NONE',  ( -3.795392936821753604, 6.515376628678959392, -1.199719254218452047 ) ) ;
#14474 = CARTESIAN_POINT ( 'NONE',  ( -1.001543065824772872E-14, 5.243750000682815937, 1.732050807568877637 ) ) ;
#14475 = CARTESIAN_POINT ( 'NONE',  ( -1.364683531250000748, -0.2406249996585799189, 0.000000000000000000 ) ) ;
#14476 = CARTESIAN_POINT ( 'NONE',  ( 6.555916519444559221, 1.865492442988415656, -0.1378669075578625169 ) ) ;
#14477 = CARTESIAN_POINT ( 'NONE',  ( 5.906827578720975858, -0.9711093913858243054, -1.436504219383877290 ) ) ;
#14478 = CARTESIAN_POINT ( 'NONE',  ( 4.141972075035261547, 0.4693275899197508760, 1.675879475284934195 ) ) ;
#14479 = CARTESIAN_POINT ( 'NONE',  ( 3.659811400685081040, 6.357198169852855685, -1.199719254218446718 ) ) ;
#14480 = CARTESIAN_POINT ( 'NONE',  ( 3.509589594912354116, -2.258262956851801118, 0.3931918642409871212 ) ) ;
#14481 = CARTESIAN_POINT ( 'NONE',  ( 0.6823417656249899377, 5.238541667008086655, -1.181850606188754593 ) ) ;
#14482 = CARTESIAN_POINT ( 'NONE',  ( 1.446930991382020748, 0.5358794165791405106, -1.761430032344503349 ) ) ;
#14483 = CARTESIAN_POINT ( 'NONE',  ( -0.3544712801349463871, 3.975028838742713511, 0.9637995819943760978 ) ) ;
#14484 = CARTESIAN_POINT ( 'NONE',  ( -10.08983450696851669, 4.085200418580138049, 6.506611369081194418 ) ) ;
#14485 = CARTESIAN_POINT ( 'NONE',  ( 2.028078973712159172, 1.053637016394028292, -1.490636434207486261 ) ) ;
#14486 = CARTESIAN_POINT ( 'NONE',  ( 2.637342451166882373, 0.6819965276749391236, 1.897697610567940174 ) ) ;
#14487 = CARTESIAN_POINT ( 'NONE',  ( 1.131117939106265791, -1.979831898266545487, 0.9398196729281658168 ) ) ;
#14488 = CARTESIAN_POINT ( 'NONE',  ( 8.498552245539556793, 15.83935224703753875, -9.434290412321708175 ) ) ;
#14489 = CARTESIAN_POINT ( 'NONE',  ( 3.944438254296574797, 2.095630017474863660, 0.2083849179023259668 ) ) ;
#14490 = CARTESIAN_POINT ( 'NONE',  ( -7.202405917357668663, 9.425892875049191488, 1.599625672291295375 ) ) ;
#14491 = CARTESIAN_POINT ( 'NONE',  ( 6.861935260488042587, 14.99925532292382790, 9.452900204311735166 ) ) ;
#14492 = CARTESIAN_POINT ( 'NONE',  ( 1.311079954825690619, -1.633285661836245906, 1.272233187909928454 ) ) ;
#14493 = CARTESIAN_POINT ( 'NONE',  ( 5.005985031943777308, 6.863401842066294556, -1.599625672291256295 ) ) ;
#14494 = CARTESIAN_POINT ( 'NONE',  ( 0.6801582343749987825, 2.723958333674732391, 1.178068619123836314 ) ) ;
#14495 = CARTESIAN_POINT ( 'NONE',  ( 3.387459763963754700, 0.05019612904376415108, -2.120051327867578550 ) ) ;
#14496 = CARTESIAN_POINT ( 'NONE',  ( 6.094357461763901362, -1.817385979143220309, -0.1739998769475574192 ) ) ;
#14497 = EDGE_LOOP ( 'NONE', ( #167537, #79639, #140741, #60778 ) ) ;
#14498 = CARTESIAN_POINT ( 'NONE',  ( -5.655686355556086120, 6.627330832017406692, 1.199719254218452935 ) ) ;
#14499 = CARTESIAN_POINT ( 'NONE',  ( 8.778014389843965759, 12.32843499053828928, 1.199719254218450271 ) ) ;
#14500 = CARTESIAN_POINT ( 'NONE',  ( 5.790741006368192778, 8.809596036521288198, -1.082531754730548412 ) ) ;
#14501 = CARTESIAN_POINT ( 'NONE',  ( 1.001543065824772753E-15, -3.368749999044086341, 4.012584370867899430 ) ) ;
#14502 = CARTESIAN_POINT ( 'NONE',  ( -4.904298879841297421, 6.744767997946721216, 1.599625672291267398 ) ) ;
#14503 = CARTESIAN_POINT ( 'NONE',  ( 3.181903496825384092, 1.969597418195143446, -0.4466673548119536319 ) ) ;
#14504 = CARTESIAN_POINT ( 'NONE',  ( 0.6222711621935803628, -1.126682295963852276, -1.779026129514348353 ) ) ;
#14506 = CARTESIAN_POINT ( 'NONE',  ( -4.471156797456668386, 8.438376373666578445, -0.7998128361456362523 ) ) ;
#14505 = VECTOR ( 'NONE', #91247, 1000.000000000000000 ) ;
#14507 = CARTESIAN_POINT ( 'NONE',  ( 9.752392566931574081, 10.27221283770866300, -0.7998128361456281477 ) ) ;
#14508 = CARTESIAN_POINT ( 'NONE',  ( 5.735155330654303718, -0.04388460642621531960, -1.860581820771879835 ) ) ;
#14509 = CARTESIAN_POINT ( 'NONE',  ( 7.052212457402625922, 11.37933163361175382, -0.7998128361456291469 ) ) ;
#14510 = DIRECTION ( 'NONE',  ( 3.330669073875478989E-16, -3.540251991789410786E-16, -1.000000000000000000 ) ) ;
#14511 = CARTESIAN_POINT ( 'NONE',  ( -5.309953438407606363, 6.223975762010839574, 1.199719254218452935 ) ) ;
#14512 = CARTESIAN_POINT ( 'NONE',  ( -8.948018195339354719, 12.42280974699582607, 1.082531754730560403 ) ) ;
#14514 = CARTESIAN_POINT ( 'NONE',  ( 2.435929278166943490, 1.204617592564939166, 1.548422000036096202 ) ) ;
#14513 = CARTESIAN_POINT ( 'NONE',  ( -6.398558430645608475, 9.552403038140164782, -1.199719254218440723 ) ) ;
#14515 = CARTESIAN_POINT ( 'NONE',  ( 0.2687375195599971400, -1.410744835756465365, 1.637978619736128127 ) ) ;
#14517 = CARTESIAN_POINT ( 'NONE',  ( -5.364460139690476304, 6.514416944181776081, 1.355983593732257741 ) ) ;
#14516 = CARTESIAN_POINT ( 'NONE',  ( -5.611095471209320174, 7.639640364534566075, 1.599625672291263179 ) ) ;
#14518 = CARTESIAN_POINT ( 'NONE',  ( -0.6823417656250003738, 0.4677083336747517306, -1.181850606188749264 ) ) ;
#14519 = CARTESIAN_POINT ( 'NONE',  ( 2.899396954618923772, 0.2085115220819243054, 1.721149687620449953 ) ) ;
#14520 = CARTESIAN_POINT ( 'NONE',  ( 2.536699030922508591, -1.289252169270055370, -1.169197435003018315 ) ) ;
#14522 = CARTESIAN_POINT ( 'NONE',  ( 6.751597309925441159, 9.860318714012938912, -1.082531754730537088 ) ) ;
#14521 = CARTESIAN_POINT ( 'NONE',  ( 0.3414292828918061296, 0.3991051782518301727, 2.272663865251875581 ) ) ;
#14523 = CARTESIAN_POINT ( 'NONE',  ( -11.14389002924298566, 7.220603907090449525, 3.549113525960188031 ) ) ;
#14524 = CARTESIAN_POINT ( 'NONE',  ( 2.319669497725483254, -1.999663683883694532, 0.4976976026799494468 ) ) ;
#14525 = CARTESIAN_POINT ( 'NONE',  ( 1.651720012567552853, -0.2930234437087535504, -1.994564656426714988 ) ) ;
#14526 = CARTESIAN_POINT ( 'NONE',  ( 6.925078400183519278, 1.259550266093687920, 2.159391284976417857 ) ) ;
#14527 = CARTESIAN_POINT ( 'NONE',  ( -4.878955176071358757, 6.785476686873604280, -1.599625672291271394 ) ) ;
#14528 = CARTESIAN_POINT ( 'NONE',  ( 1.112115884188523918, -0.8845927946041342027, -1.761928416731074476 ) ) ;
#14530 = CARTESIAN_POINT ( 'NONE',  ( -5.587368702607575344, 8.572328348800551723, 1.082531754730550855 ) ) ;
#14529 = CARTESIAN_POINT ( 'NONE',  ( 4.183787391381143195, 1.853651273288700718, -0.4697857328580385960 ) ) ;
#14531 = CARTESIAN_POINT ( 'NONE',  ( -6.034787771414192648, 9.094317262408276648, 1.082531754730549967 ) ) ;
#14532 = CARTESIAN_POINT ( 'NONE',  ( 7.550965208168244125, 7.774157262476569130, -0.7998128361456341429 ) ) ;
#14533 = CARTESIAN_POINT ( 'NONE',  ( -7.618755976236585958, 7.853246491889623648, 0.000000000000000000 ) ) ;
#14534 = CARTESIAN_POINT ( 'NONE',  ( 0.8033855960881201019, 1.780198652630104794, -0.9539489498650125521 ) ) ;
#14535 = FACE_OUTER_BOUND ( 'NONE', #29609, .T. ) ;
#14536 = CARTESIAN_POINT ( 'NONE',  ( 5.069473898719869531, 0.2322026582469650102, -2.295885384840197663 ) ) ;
#14537 = CARTESIAN_POINT ( 'NONE',  ( 5.459412808053472510, 1.602871733476991079, 1.130958114227413436 ) ) ;
#14538 = EDGE_CURVE ( 'NONE', #108029, #12234, #23454, .T. ) ;
#14539 = CARTESIAN_POINT ( 'NONE',  ( 2.078885752709497492, 1.828579749420868872, 0.7109141669488158177 ) ) ;
#14540 = CARTESIAN_POINT ( 'NONE',  ( 9.561524646135536543, 12.17819805862340310, -1.599625672291262513 ) ) ;
#14541 = FACE_OUTER_BOUND ( 'NONE', #49899, .T. ) ;
#14542 = VERTEX_POINT ( 'NONE', #88962 ) ;
#14543 = CARTESIAN_POINT ( 'NONE',  ( 1.692723046232265105, 1.565162839624185898, -1.426121385913220019 ) ) ;
#14545 = CARTESIAN_POINT ( 'NONE',  ( -6.157374318900681764, 10.33535380535947290, 0.7998128361456481317 ) ) ;
#14544 = CARTESIAN_POINT ( 'NONE',  ( -5.005985031943793295, 6.863401842066301661, -1.599625672291256295 ) ) ;
#14546 = CARTESIAN_POINT ( 'NONE',  ( 1.323879276782027770, 1.773944146221797746, 0.4926282247687193139 ) ) ;
#14547 = EDGE_LOOP ( 'NONE', ( #51688, #164098, #18057, #7513 ) ) ;
#14548 = CARTESIAN_POINT ( 'NONE',  ( 4.627881963378519536, 2.107464937132212501, -0.5213077441503320975 ) ) ;
#14549 = B_SPLINE_CURVE_WITH_KNOTS ( 'NONE', 3,
 ( #147638, #45883, #95706, #65282, #112004, #82613, #13351, #63176, #129341, #195319, #46950, #213656 ),
 .UNSPECIFIED., .F., .F.,
 ( 4, 2, 2, 2, 2, 4 ),
 ( 0.0001305756608390105640, 0.1066250804225375576, 0.2131195851842360989, 0.2663668375650854458, 0.3196140899459348206, 0.4261085947076337366 ),
 .UNSPECIFIED. ) ;
#14550 = CARTESIAN_POINT ( 'NONE',  ( 11.63317533773959589, 8.260435399328212469, -2.973782887496474459 ) ) ;
#14551 = CARTESIAN_POINT ( 'NONE',  ( 2.162495577681341707, 2.120227376586072854, 0.04728746717985036346 ) ) ;
#14552 = CARTESIAN_POINT ( 'NONE',  ( 1.499999999999989120, 3.285416667349486897, 0.8660254037844524744 ) ) ;
#14553 = CARTESIAN_POINT ( 'NONE',  ( 8.320953590485093088, 10.73086516036454618, 1.599625672291281386 ) ) ;
#14554 = CARTESIAN_POINT ( 'NONE',  ( 2.847006562934909280, -1.715207642559450685, 1.141990792043580338 ) ) ;
#14556 = CARTESIAN_POINT ( 'NONE',  ( 0.2218712608162629052, 1.761692264604281633, 0.5354471447000588302 ) ) ;
#14555 = CARTESIAN_POINT ( 'NONE',  ( -7.831806290188425557, 12.28885777186185990, -0.7998128361456281477 ) ) ;
#14557 = CARTESIAN_POINT ( 'NONE',  ( 0.6823417656249917140, 3.842708333674754506, 1.181850606188765695 ) ) ;
#14558 = CARTESIAN_POINT ( 'NONE',  ( -0.02264175331119500090, 1.349762599094967763, -2.344447671987642146 ) ) ;
#14559 = DIRECTION ( 'NONE',  ( 0.000000000000000000, 1.000000000000000000, 0.000000000000000000 ) ) ;
#14560 = CIRCLE ( 'NONE', #190976, 4.583333333333340143 ) ;
#14561 = CARTESIAN_POINT ( 'NONE',  ( 0.5048604690408053930, -0.7474223562033958101, -2.076596198196341003 ) ) ;
#14562 = CARTESIAN_POINT ( 'NONE',  ( 1.001694622806301060, 1.849986872810194694, 1.302049432249830607 ) ) ;
#14563 = VECTOR ( 'NONE', #191994, 1000.000000000000000 ) ;
#14564 = CARTESIAN_POINT ( 'NONE',  ( -10.16825202056928390, 10.96530823352674133, 0.7216878364870438212 ) ) ;
#14565 = CARTESIAN_POINT ( 'NONE',  ( 2.812559491778331200, -0.5300286150072616165, -1.732275345909091380 ) ) ;
#14566 = CARTESIAN_POINT ( 'NONE',  ( 1.692462117551472911, 1.416773270106906235, -1.289619884002331407 ) ) ;
#14567 = CARTESIAN_POINT ( 'NONE',  ( 3.033707436314789785, 1.966763487489433970, -0.6469820378900912328 ) ) ;
#14568 = CARTESIAN_POINT ( 'NONE',  ( 0.6823417656249882723, 0.9885416670080832136, -1.181850606188749264 ) ) ;
#14569 = EDGE_CURVE ( 'NONE', #126082, #26543, #127168, .T. ) ;
#14570 = CARTESIAN_POINT ( 'NONE',  ( 1.709780583834107803, -1.956794704801574358, 0.2394988650771395777 ) ) ;
#14571 = CARTESIAN_POINT ( 'NONE',  ( 0.1297406284284522426, -1.182532350666727128, -1.521449160436913584 ) ) ;
#14572 = CARTESIAN_POINT ( 'NONE',  ( 3.168673215318769110, -1.727878594304608217, -0.7172629358194044791 ) ) ;
#14574 = CARTESIAN_POINT ( 'NONE',  ( 6.485343392949857844, 6.752073445700102816, -0.1478272009810890908 ) ) ;
#14573 = CARTESIAN_POINT ( 'NONE',  ( 1.524504908422112726, -1.285150704446396341, -1.916548379014111791 ) ) ;
#14575 = CARTESIAN_POINT ( 'NONE',  ( 2.330303589177587398, -1.147911989558418222, 1.464751052146954224 ) ) ;
#14576 = CARTESIAN_POINT ( 'NONE',  ( -1.364683531249997417, 3.259375000341423245, 1.214306433183764966E-14 ) ) ;
#14577 = CARTESIAN_POINT ( 'NONE',  ( 5.072745416573516408, 1.424789591659934684, -1.491725785151225336 ) ) ;
#14578 = CARTESIAN_POINT ( 'NONE',  ( -5.708146366553361162, 6.618257834855742594, -1.199719254218446718 ) ) ;
#14579 = CARTESIAN_POINT ( 'NONE',  ( -1.369767765231834300, 3.411414233851330025, -0.2488260012212513972 ) ) ;
#14580 = CARTESIAN_POINT ( 'NONE',  ( 6.124072230051534227, -1.166888049220366597, -1.752910934067633875 ) ) ;
#14581 = CARTESIAN_POINT ( 'NONE',  ( 0.6823417656249899377, 2.905208333674754062, 1.181850606188765695 ) ) ;
#14582 = CARTESIAN_POINT ( 'NONE',  ( 6.011032505573889573, 1.903242638633116712, 1.024824547371510075 ) ) ;
#14583 = CARTESIAN_POINT ( 'NONE',  ( 0.5910386730991653570, -0.6632029860377097741, 1.717849102829023922 ) ) ;
#14584 = CARTESIAN_POINT ( 'NONE',  ( 5.391273274344085209, -0.05166147132495273880, -2.019192591660509351 ) ) ;
#14585 = DIRECTION ( 'NONE',  ( -0.6507913734559642727, -0.7592566023653003482, -2.775557561562895049E-17 ) ) ;
#14586 = CARTESIAN_POINT ( 'NONE',  ( -4.717874267875590277, 7.487641831621378863, 1.082531754730560403 ) ) ;
#14587 = EDGE_CURVE ( 'NONE', #57016, #37648, #11930, .T. ) ;
#14590 = CARTESIAN_POINT ( 'NONE',  ( 5.233084105194869551, 6.167981546557892436, -1.082531754730548412 ) ) ;
#14589 = CARTESIAN_POINT ( 'NONE',  ( 1.001543065824772753E-15, -0.7218749995220414828, 3.793834371823811669 ) ) ;
#14588 = CARTESIAN_POINT ( 'NONE',  ( 0.000000000000000000, 14.55305236562704252, -11.95586206896551928 ) ) ;
#14591 =( BOUNDED_SURFACE ( )  B_SPLINE_SURFACE ( 3, 2, ( 
 ( #85259, #38656, #204316 ),
 ( #6124, #200064, #138301 ),
 ( #76216, #51716, #19184 ),
 ( #151348, #68989, #146589 ),
 ( #64245, #212606, #209394 ),
 ( #161757, #96772, #180128 ),
 ( #160676, #130388, #195315 ),
 ( #62114, #13347, #208336 ) ),
 .UNSPECIFIED., .F., .F., .T. ) 
 B_SPLINE_SURFACE_WITH_KNOTS ( ( 4, 2, 2, 4 ),
 ( 3, 3 ),
 ( 0.000000000000000000, 0.0002204160392919248554, 0.0004408320785838497108, 0.0008816641571676994216 ),
 ( 0.000000000000000000, 1.000000000000000000 ),
 .UNSPECIFIED. ) 
 GEOMETRIC_REPRESENTATION_ITEM ( )  RATIONAL_B_SPLINE_SURFACE ( (
 ( 1.000000000000000000, 0.4127341956165088144, 1.000000000000000000),
 ( 1.000000000000000000, 0.4103180386330694818, 1.000000000000000000),
 ( 1.000000000000000000, 0.4223234233959186623, 1.000000000000000000),
 ( 1.000000000000000000, 0.4613847219397944066, 1.000000000000000000),
 ( 1.000000000000000000, 0.4878744032655861762, 1.000000000000000000),
 ( 1.000000000000000000, 0.5702658980234645014, 1.000000000000000000),
 ( 1.000000000000000000, 0.6280001242509920534, 1.000000000000000000),
 ( 1.000000000000000000, 0.6787756258918242747, 1.000000000000000000) ) ) 
 REPRESENTATION_ITEM ( '' )  SURFACE ( )  );
#14592 = CARTESIAN_POINT ( 'NONE',  ( -3.657667580636712934, 7.489305620709952649, -0.7998128361456481317 ) ) ;
#14593 = CARTESIAN_POINT ( 'NONE',  ( 3.380092458137720968, -2.014432998692190058, -0.09411721906785883163 ) ) ;
#14594 = CARTESIAN_POINT ( 'NONE',  ( -6.353967546298838087, 10.56471257065732416, 0.000000000000000000 ) ) ;
#14595 = CARTESIAN_POINT ( 'NONE',  ( -4.302014814237876017, 3.913438792899272212, 0.7998128361456341429 ) ) ;
#14596 = CARTESIAN_POINT ( 'NONE',  ( 0.6823417656249899377, 5.426041667008087543, -1.181850606188754593 ) ) ;
#14598 = CARTESIAN_POINT ( 'NONE',  ( -0.6823417656250039265, 9.067708333674733723, -1.181850606188755259 ) ) ;
#14597 = CARTESIAN_POINT ( 'NONE',  ( 5.471600609837615536, 2.084441204114939161, -0.5725544205837928002 ) ) ;
#14599 = LINE ( 'NONE', #80696, #162376 ) ;
#14600 = CARTESIAN_POINT ( 'NONE',  ( -12.00016184804641206, 8.029277273509505264, -0.2582136249091951385 ) ) ;
#14602 = CARTESIAN_POINT ( 'NONE',  ( 5.185172808627552143, 1.650094130669476522, 1.158673036085342112 ) ) ;
#14601 = CARTESIAN_POINT ( 'NONE',  ( -7.036318535368094373, 7.311385834125318617, 0.7216878364870317197 ) ) ;
#14603 = CARTESIAN_POINT ( 'NONE',  ( 1.364683531249984538, -1.032291666325247714, -0.7879004041258309554 ) ) ;
#14604 = CARTESIAN_POINT ( 'NONE',  ( 2.068594797844982125, -1.576417056545238893, -0.7005022305992656406 ) ) ;
#14605 = CARTESIAN_POINT ( 'NONE',  ( 5.761288931164342486, 5.686201605971993978, -0.7998128361456481317 ) ) ;
#14606 = VECTOR ( 'NONE', #21533, 1000.000000000000000 ) ;
#14608 = CARTESIAN_POINT ( 'NONE',  ( 6.668631453075247073, 8.873432343378178544, -1.599625672291281386 ) ) ;
#14607 = CARTESIAN_POINT ( 'NONE',  ( 6.141480397310468575, 10.10888486359680982, 1.040834085586084257E-14 ) ) ;
#14609 = CARTESIAN_POINT ( 'NONE',  ( 0.3255492091119998599, 2.641190174458327711, -1.974278555462047668 ) ) ;
#14610 = CARTESIAN_POINT ( 'NONE',  ( 0.2976568962721929390, -1.769157359987379996, -0.05240849467303894393 ) ) ;
#14611 = CARTESIAN_POINT ( 'NONE',  ( 0.2760392706695756759, 1.990868297383071139, -0.2976099395228733457 ) ) ;
#14612 = CARTESIAN_POINT ( 'NONE',  ( 0.000000000000000000, -4.500000000000003553, 0.000000000000000000 ) ) ;
#14613 = CARTESIAN_POINT ( 'NONE',  ( 2.925073249431627165, 2.077443920948469192, 0.7446974470129495982 ) ) ;
#14614 = CARTESIAN_POINT ( 'NONE',  ( 5.664936021742177807, 1.649023742746661192, -1.412335049966114253 ) ) ;
#14615 = VERTEX_POINT ( 'NONE', #29280 ) ;
#14616 = CARTESIAN_POINT ( 'NONE',  ( 3.061108821635398769, 6.793320401875094561, -0.7998128361456362523 ) ) ;
#14617 = CARTESIAN_POINT ( 'NONE',  ( 8.825994812371966702, 12.28044913353391898, -1.082531754730543083 ) ) ;
#14619 = CARTESIAN_POINT ( 'NONE',  ( 1.441030037510174777, -1.730879250949714843, -1.034145807338890277 ) ) ;
#14618 = CARTESIAN_POINT ( 'NONE',  ( 3.088655771522513582, -1.261447869382603004, 1.704333039148818507 ) ) ;
#14621 = ORIENTED_EDGE ( 'NONE', *, *, #185057, .F. ) ;
#14620 = CARTESIAN_POINT ( 'NONE',  ( 2.408236768384981019, -1.806978867004911171, -0.1295660047265032311 ) ) ;
#14622 = CARTESIAN_POINT ( 'NONE',  ( 6.547661840756936691, 6.603636667163397256, 0.7998128361456352531 ) ) ;
#14623 = VERTEX_POINT ( 'NONE', #8753 ) ;
#14624 = CARTESIAN_POINT ( 'NONE',  ( 6.043183783389218355, 8.073467052085995022, 1.599625672291267398 ) ) ;
#14626 = CARTESIAN_POINT ( 'NONE',  ( 1.586979130512996772, 1.594871783843774260, 1.060967117046989427 ) ) ;
#14625 = CARTESIAN_POINT ( 'NONE',  ( -5.101945877444165944, 4.846691699973280976, 0.000000000000000000 ) ) ;
#14627 = VECTOR ( 'NONE', #139931, 1000.000000000000000 ) ;
#14628 = CARTESIAN_POINT ( 'NONE',  ( -2.680963273416246295, 0.4787157238462547704, -0.1016320821874245467 ) ) ;
#14629 = CARTESIAN_POINT ( 'NONE',  ( 1.484505139761094883, 7.334797934598051405, 4.257182005875050024 ) ) ;
#14630 = CARTESIAN_POINT ( 'NONE',  ( 4.460269348771534581, 8.147471973634706544, -0.7216878364870207285 ) ) ;
#14631 = CARTESIAN_POINT ( 'NONE',  ( -0.6823417656250003738, 0.5302083336747518416, -1.181850606188749264 ) ) ;
#14632 = LINE ( 'NONE', #62339, #18849 ) ;
#14633 = CARTESIAN_POINT ( 'NONE',  ( -9.053093885623068715, 11.58502883802551153, -1.599625672291263179 ) ) ;
#14634 = CARTESIAN_POINT ( 'NONE',  ( 4.751185534883737738, 0.1928377863454934504, -2.007255887737584121 ) ) ;
#14635 = CARTESIAN_POINT ( 'NONE',  ( 5.629794960336353071, -1.368038101806166029, -1.673757646710342550 ) ) ;
#14636 = CARTESIAN_POINT ( 'NONE',  ( -4.340018570150306232, 8.077455741901736985, -0.7216878364870338292 ) ) ;
#14637 = CARTESIAN_POINT ( 'NONE',  ( 5.072158865288233009, 7.010880990960010273, 1.443375672974065660 ) ) ;
#14638 = CARTESIAN_POINT ( 'NONE',  ( 1.916421503514931679, -2.120014230100770725, 0.05699577502370903326 ) ) ;
#14640 = CARTESIAN_POINT ( 'NONE',  ( -11.77619280525687451, 4.711391180887883223, -4.977117663154129623 ) ) ;
#14639 = CARTESIAN_POINT ( 'NONE',  ( -0.1298852118743840378, 0.7651466308506644776, -1.811855282322960781 ) ) ;
#14641 = ADVANCED_FACE ( 'NONE', ( #93238 ), #75892, .T. ) ;
#14642 = CARTESIAN_POINT ( 'NONE',  ( 3.690661264905565009, -0.3812834177611671982, -1.933973196684968920 ) ) ;
#14643 = CARTESIAN_POINT ( 'NONE',  ( 5.185773951807310489, 1.841398108398510480, -0.5159224025059682139 ) ) ;
#14644 = ORIENTED_EDGE ( 'NONE', *, *, #190890, .T. ) ;
#14645 = FILL_AREA_STYLE ('',( #93809 ) ) ;
#14646 = CARTESIAN_POINT ( 'NONE',  ( 0.5728211633247158874, 1.428863753495920763, -1.498466819491943269 ) ) ;
#14647 = CARTESIAN_POINT ( 'NONE',  ( 2.062350447250702157, -1.775486198902403778, -0.7870378659600388849 ) ) ;
#14648 = ORIENTED_EDGE ( 'NONE', *, *, #139829, .T. ) ;
#14649 = CARTESIAN_POINT ( 'NONE',  ( -4.981695098378565945, 4.776675467721892332, -0.7998128361456362523 ) ) ;
#14651 = CARTESIAN_POINT ( 'NONE',  ( 7.526711554241970248, 8.810193563817646734, -1.199719254218452047 ) ) ;
#14650 = CARTESIAN_POINT ( 'NONE',  ( -7.783789588021474692, 8.253711738879413673, 0.7216878364870317197 ) ) ;
#14653 = CARTESIAN_POINT ( 'NONE',  ( 7.644099680006512187, 7.812537802962739697, 1.040834085586084257E-14 ) ) ;
#14652 = CARTESIAN_POINT ( 'NONE',  ( 2.537156728381038118, -1.549654062961543177, -1.403521045075975415 ) ) ;
#14654 = CARTESIAN_POINT ( 'NONE',  ( 5.682275777458851707, 6.762314840857718501, 1.082531754730549078 ) ) ;
#14656 = EDGE_LOOP ( 'NONE', ( #210394, #166395, #203395, #156257, #149531, #1371, #5109, #8407 ) ) ;
#14655 = CARTESIAN_POINT ( 'NONE',  ( 6.604189988765333474, -0.8127675640051763573, 1.729262449380222222 ) ) ;
#14657 = CARTESIAN_POINT ( 'NONE',  ( 4.688207069967821106, -1.042061291317699423, 1.945354640606362873 ) ) ;
#14658 = AXIS2_PLACEMENT_3D ( 'NONE', #188451, #101875, #19543 ) ;
#14659 = CARTESIAN_POINT ( 'NONE',  ( 2.626236979526615389, -1.269917727785064843, -1.804575601930514139 ) ) ;
#14660 = CARTESIAN_POINT ( 'NONE',  ( 9.121938423896107651, 9.536683004167278099, -0.7998128361456221525 ) ) ;
#14661 = CARTESIAN_POINT ( 'NONE',  ( -11.92050416151433012, 12.44794624720363174, 1.381922468431395767 ) ) ;
#14662 = CARTESIAN_POINT ( 'NONE',  ( 1.400873256076972329, -0.2815782128867699852, -1.891321520182134286 ) ) ;
#14663 = CARTESIAN_POINT ( 'NONE',  ( 0.4294425147611402038, -9.199999999999990408, -9.490288674561773163 ) ) ;
#14664 = CARTESIAN_POINT ( 'NONE',  ( 8.224992744984721327, 12.74757530245756243, 1.040834085586084257E-14 ) ) ;
#14665 = CARTESIAN_POINT ( 'NONE',  ( 4.299325596424930396, -1.802881993240162961, 1.017688063649782482 ) ) ;
#14667 = CARTESIAN_POINT ( 'NONE',  ( 1.305796196612364124, -0.5247483525172502716, 2.096912610238470975 ) ) ;
#14666 = CARTESIAN_POINT ( 'NONE',  ( -2.266184231778562541, 5.795632037050281404, 1.040834085586084257E-14 ) ) ;
#14668 = CARTESIAN_POINT ( 'NONE',  ( 4.071962858106247474, -1.261020321617589479, 1.792237525612811355 ) ) ;
#14669 = CARTESIAN_POINT ( 'NONE',  ( -0.07968760456310633455, 7.629137130509075604, -2.426417496045676803 ) ) ;
#14670 = CARTESIAN_POINT ( 'NONE',  ( -0.4829820140311024135, 7.516281308464804134, 1.942130999994731377 ) ) ;
#14671 = CARTESIAN_POINT ( 'NONE',  ( 5.061990249855835344, 6.999017606288844284, -1.599625672291273171 ) ) ;
#14672 = CARTESIAN_POINT ( 'NONE',  ( -1.402160292154681736E-14, 13.73437500034139624, 1.575800808251682339 ) ) ;
#14673 = CARTESIAN_POINT ( 'NONE',  ( -3.871735385154307263, 6.674719161725423788, -1.199719254218450271 ) ) ;
#14674 = CARTESIAN_POINT ( 'NONE',  ( 0.3346115673153668424, 0.6298721381652396811, -1.915601020889952322 ) ) ;
#14675 = CARTESIAN_POINT ( 'NONE',  ( -8.514157279702020631, 11.91663867875229776, -1.082531754730543971 ) ) ;
#14676 = CARTESIAN_POINT ( 'NONE',  ( 4.944224162298806569, -0.9806570695735459253, 1.823293813017504039 ) ) ;
#14677 = CARTESIAN_POINT ( 'NONE',  ( 2.842313889931574522, 1.911971217405187495, 0.2356370756458354143 ) ) ;
#14678 = CARTESIAN_POINT ( 'NONE',  ( 5.993796379919574591, -2.101200072677239739, 0.2596931833054038630 ) ) ;
#14679 = CARTESIAN_POINT ( 'NONE',  ( 5.986088515633498197, 6.942523675449257858, -1.199719254218446718 ) ) ;
#14680 = CARTESIAN_POINT ( 'NONE',  ( 9.333041836227126353, 3.553052365627043852, 7.472413793103449997 ) ) ;
#14681 = CARTESIAN_POINT ( 'NONE',  ( 3.907052821786443975, -1.612583007836394966, 1.130340192709837766 ) ) ;
#14682 = CARTESIAN_POINT ( 'NONE',  ( 5.490252784120214002, -0.5523235152877626897, -2.224609438220140234 ) ) ;
#14684 = ADVANCED_FACE ( 'NONE', ( #193899 ), #192822, .T. ) ;
#14683 = CARTESIAN_POINT ( 'NONE',  ( 4.617693566336190436, -1.789886777702164089, 0.3589094947460610974 ) ) ;
#14685 = CARTESIAN_POINT ( 'NONE',  ( 5.533136088152891929, 9.469426179571447832, -0.7216878364870458196 ) ) ;
#14686 = CARTESIAN_POINT ( 'NONE',  ( 4.270455198180219902, 6.965652916976816655, -1.082531754730548412 ) ) ;
#14687 = CARTESIAN_POINT ( 'NONE',  ( -5.121948170912633991, 9.197632976031879792, -0.7998128361456362523 ) ) ;
#14688 = CARTESIAN_POINT ( 'NONE',  ( 5.285699784481295183, 7.260012063351913625, 1.599625672291268286 ) ) ;
#14689 = B_SPLINE_CURVE_WITH_KNOTS ( 'NONE', 3,
 ( #154462, #56957, #9268, #89474, #123129, #137151, #88395, #104650, #189088, #25512 ),
 .UNSPECIFIED., .F., .F.,
 ( 4, 2, 2, 2, 4 ),
 ( 0.0002061898317416346730, 0.0005587239135660432461, 0.0009112579953904516566, 0.001263792077214860067, 0.001616326159039268694 ),
 .UNSPECIFIED. ) ;
#14690 = ORIENTED_EDGE ( 'NONE', *, *, #149161, .F. ) ;
#14691 = CARTESIAN_POINT ( 'NONE',  ( 5.414319639144633101, -2.013376227731620283, 0.004290823026709827959 ) ) ;
#14692 = CARTESIAN_POINT ( 'NONE',  ( 5.731119460814408484, 2.295830932937119595, 0.1164615576392889484 ) ) ;
#14693 = CARTESIAN_POINT ( 'NONE',  ( 5.875826477234550538, -1.914729252524836056, 0.4262945716600323731 ) ) ;
#14694 = CARTESIAN_POINT ( 'NONE',  ( -5.696397096036042385, 9.797547045350714967, -0.7998128361456231517 ) ) ;
#14695 = CARTESIAN_POINT ( 'NONE',  ( -4.731959306369413198, 5.479372931307791461, -1.199719254218446718 ) ) ;
#14697 = EDGE_CURVE ( 'NONE', #36899, #132416, #45546, .T. ) ;
#14696 = CARTESIAN_POINT ( 'NONE',  ( -7.876942567271134621, -5.350481869465722795, 7.629869294364564070 ) ) ;
#14698 = CARTESIAN_POINT ( 'NONE',  ( -5.936491157937300756, 8.019268665717216749, 1.599625672291263179 ) ) ;
#14700 = CARTESIAN_POINT ( 'NONE',  ( 0.5670072068131201126, 0.1877032549213939472, -1.861219751863735672 ) ) ;
#14699 = CARTESIAN_POINT ( 'NONE',  ( 1.487951815845720338, -2.081006265264739419, -0.2013860056617396421 ) ) ;
#14701 = CARTESIAN_POINT ( 'NONE',  ( -0.4000000000000113465, 3.017365524286432787, 2.023857702507793288 ) ) ;
#14702 = CARTESIAN_POINT ( 'NONE',  ( 5.736261908918430130, 0.3809393362203088440, 1.904059320497718089 ) ) ;
#14703 = CARTESIAN_POINT ( 'NONE',  ( -0.2104748580754183807, 2.005809028216706924, -2.517884123765606663 ) ) ;
#14704 = CARTESIAN_POINT ( 'NONE',  ( 1.206182128890446403, 1.534490571913693868, 0.8211921505957423539 ) ) ;
#14705 = CARTESIAN_POINT ( 'NONE',  ( 6.474182045725470402, 7.511966127223233869, -1.199719254218446718 ) ) ;
#14706 = DIRECTION ( 'NONE',  ( 0.000000000000000000, 0.000000000000000000, -1.000000000000000000 ) ) ;
#14707 = CARTESIAN_POINT ( 'NONE',  ( 1.312684994149786455, 1.519677550804766852, 0.8159285863849721210 ) ) ;
#14708 = CARTESIAN_POINT ( 'NONE',  ( 1.470551405592795957, -2.082434148983134392, -0.6831980896230758216 ) ) ;
#14709 = CARTESIAN_POINT ( 'NONE',  ( 6.854911444608583260, -0.7389736882487309977, 1.567799899397160912 ) ) ;
#14710 = CARTESIAN_POINT ( 'NONE',  ( 3.633602750639616019, -2.039237483250630589, 0.8441791899983088765 ) ) ;
#14711 = AXIS2_PLACEMENT_3D ( 'NONE', #177849, #198326, #63011 ) ;
#14712 = CARTESIAN_POINT ( 'NONE',  ( 1.305810364819631753, -1.710103357748852027, -1.337415221091219353 ) ) ;
#14713 = CARTESIAN_POINT ( 'NONE',  ( 0.3108172448005979138, 1.586703044182024458, 0.9029097728878652251 ) ) ;
#14714 = CARTESIAN_POINT ( 'NONE',  ( 2.413409855213846544, -1.973772631060242144, 0.7668006401621522139 ) ) ;
#14715 = AXIS2_PLACEMENT_3D ( 'NONE', #15651, #134783, #83860 ) ;
#14716 = CARTESIAN_POINT ( 'NONE',  ( 6.639320575229231025, 3.706874577532508486, 2.311316081152973823 ) ) ;
#14717 = EDGE_LOOP ( 'NONE', ( #163470, #70457, #115751, #36232, #7329 ) ) ;
#14719 = CARTESIAN_POINT ( 'NONE',  ( 0.6823417656249882723, -0.09479166632524876901, 1.181850606188755259 ) ) ;
#14718 = CARTESIAN_POINT ( 'NONE',  ( 2.156203017566417302, 0.9840264443441574249, 2.070573632387271434 ) ) ;
#14720 = CARTESIAN_POINT ( 'NONE',  ( 0.000000000000000000, -1.000000000000000888, -10.91999999999999105 ) ) ;
#14721 = CARTESIAN_POINT ( 'NONE',  ( 4.168242161197552420, 6.950367390450747251, -1.199719254218452047 ) ) ;
#14722 = CARTESIAN_POINT ( 'NONE',  ( 5.145291483242067088, 0.1622298597842904699, 2.215448774714718461 ) ) ;
#14723 = CARTESIAN_POINT ( 'NONE',  ( -6.724481002698130538, 7.907944593645035880, -1.082531754730544860 ) ) ;
#14724 = CARTESIAN_POINT ( 'NONE',  ( 4.189106276942576201, 7.831115056500907556, 1.040834085586084257E-14 ) ) ;
#14725 = CARTESIAN_POINT ( 'NONE',  ( -7.334597914868735025, 9.580116872145431728, -1.443375672974058777 ) ) ;
#14726 = EDGE_CURVE ( 'NONE', #169159, #113990, #436, .T. ) ;
#14727 = CARTESIAN_POINT ( 'NONE',  ( 5.560252395380215873, 6.619954228432645138, 1.082531754730549078 ) ) ;
#14728 = ORIENTED_EDGE ( 'NONE', *, *, #31789, .F. ) ;
#14729 = CARTESIAN_POINT ( 'NONE',  ( 2.426407915648312930, -1.496052118593782065, -1.352154011671408362 ) ) ;
#14731 = CARTESIAN_POINT ( 'NONE',  ( 2.114201203919101157, 2.057314814202032771, -0.1476098556340669499 ) ) ;
#14730 = CARTESIAN_POINT ( 'NONE',  ( 5.777746017718023097, 9.892454120646377191, 0.7998128361456462443 ) ) ;
#14732 = FACE_OUTER_BOUND ( 'NONE', #188611, .T. ) ;
#14733 = CARTESIAN_POINT ( 'NONE',  ( 6.007671464186837618, 6.181573927739029806, 0.7216878364870328300 ) ) ;
#14734 = B_SPLINE_CURVE_WITH_KNOTS ( 'NONE', 3,
 ( #17284, #70295, #67092, #4225, #164631, #54082, #150528, #165695, #53003, #16215 ),
 .UNSPECIFIED., .F., .F.,
 ( 4, 2, 2, 2, 4 ),
 ( 0.03215845547981503738, 0.04524000524079174745, 0.05832155500176845753, 0.08448465452372194706, 0.1368108535676289816 ),
 .UNSPECIFIED. ) ;
#14735 = CARTESIAN_POINT ( 'NONE',  ( -5.097502569058221411, 6.009803087731781623, -1.082531754730544860 ) ) ;
#14736 = CARTESIAN_POINT ( 'NONE',  ( 1.364683531249992088, 5.634375000341417916, 1.214306433183764966E-14 ) ) ;
#14737 = CARTESIAN_POINT ( 'NONE',  ( 5.367185978643659539, 2.112682091867735146, -0.5819856738719306755 ) ) ;
#14738 = CARTESIAN_POINT ( 'NONE',  ( 2.057267738415057057, -1.238319999287675888, 1.591319116112683618 ) ) ;
#14739 = CARTESIAN_POINT ( 'NONE',  ( 0.6261898170028465938, 0.1349980957352381883, 1.836376839866371569 ) ) ;
#14740 = CARTESIAN_POINT ( 'NONE',  ( 8.281332899848809603, 8.555976559445431562, 0.7998128361456481317 ) ) ;
#14741 =( NAMED_UNIT ( * ) SI_UNIT ( $, .STERADIAN. ) SOLID_ANGLE_UNIT ( ) );
#14742 = CARTESIAN_POINT ( 'NONE',  ( 5.772426501671443333, -1.156275361458743545, 1.412693073426966262 ) ) ;
#14743 = CARTESIAN_POINT ( 'NONE',  ( 6.276017556857773627, 1.753032240926259311, -0.9962986157117934560 ) ) ;
#14744 = CARTESIAN_POINT ( 'NONE',  ( -7.446452682403657874, 9.710614100936176385, -1.599625672291263179 ) ) ;
#14746 = CARTESIAN_POINT ( 'NONE',  ( -4.620296487206990932, 8.612372678375294299, 0.000000000000000000 ) ) ;
#14745 = CARTESIAN_POINT ( 'NONE',  ( 4.768612610038791111, -1.481304060603398032, 1.710260256980479898 ) ) ;
#14747 = CARTESIAN_POINT ( 'NONE',  ( 0.4695305163736606668, 0.2040741594158005934, -2.096154701512464413 ) ) ;
#14748 = CARTESIAN_POINT ( 'NONE',  ( -5.237192476628793614, 9.332084666034067055, 0.7998128361456291469 ) ) ;
#14749 = CARTESIAN_POINT ( 'NONE',  ( 4.527825515032589898, 2.008996319933327612, -0.4998958796476050681 ) ) ;
#14750 = CARTESIAN_POINT ( 'NONE',  ( 8.106885785967500979, 11.54545161934907682, 1.199719254218460707 ) ) ;
#14751 = CYLINDRICAL_SURFACE ( 'NONE', #162988, 0.07999999999999998779 ) ;
#14752 = DIRECTION ( 'NONE',  ( 1.000000000000000000, 3.122502256758251537E-17, 2.220446049250313081E-16 ) ) ;
#14753 = CARTESIAN_POINT ( 'NONE',  ( -7.340850106795412167, 10.65174332698158643, 1.199719254218453823 ) ) ;
#14754 = UNCERTAINTY_MEASURE_WITH_UNIT (LENGTH_MEASURE( 1.000000000000000082E-05 ), #46865, 'distance_accuracy_value', 'NONE');
#14755 = CARTESIAN_POINT ( 'NONE',  ( 11.04536101718726293, 11.00581808788928306, 1.099999999999996980 ) ) ;
#14756 = CARTESIAN_POINT ( 'NONE',  ( 4.055297343818933697, 5.824542549245813383, 1.443375672974058777 ) ) ;
#14757 = CARTESIAN_POINT ( 'NONE',  ( 5.815065281910236195, 6.023992952839542170, -0.4647386070683479642 ) ) ;
#14758 = CARTESIAN_POINT ( 'NONE',  ( -10.30383355670593737, 11.12348669235284504, -0.7216878364870267237 ) ) ;
#14759 = CARTESIAN_POINT ( 'NONE',  ( 2.566880079249767022, 0.7526719050801253807, 2.090118821510750458 ) ) ;
#14760 = PRESENTATION_LAYER_ASSIGNMENT (  '', '', ( #208338 ) ) ;
#14761 = DIRECTION ( 'NONE',  ( 0.000000000000000000, 0.000000000000000000, -1.000000000000000000 ) ) ;
#14762 = CARTESIAN_POINT ( 'NONE',  ( -4.450819567036169211, 8.414649604842665553, -0.7998128361456362523 ) ) ;
#14763 = CARTESIAN_POINT ( 'NONE',  ( 6.257251587906815793, 7.258880593101466161, 1.199719254218462483 ) ) ;
#14764 = CARTESIAN_POINT ( 'NONE',  ( 3.701569118832209515, -1.483977648892897960, -1.283320388228793130 ) ) ;
#14765 = CARTESIAN_POINT ( 'NONE',  ( 5.066996723205273057, 6.934582148538044777, 1.599625672291267398 ) ) ;
#14766 = CARTESIAN_POINT ( 'NONE',  ( -4.014213326890253342, 7.626914324717730231, 0.01912188359321290165 ) ) ;
#14767 = CARTESIAN_POINT ( 'NONE',  ( 3.602716132929354664, 5.226254793216122074, 1.599625672291267398 ) ) ;
#14768 = CARTESIAN_POINT ( 'NONE',  ( -4.177320726786315497, 7.887641591310407208, -0.7216878364870458196 ) ) ;
#14769 = CARTESIAN_POINT ( 'NONE',  ( -7.049876689426113785, 8.287572894827684777, -1.082531754730544860 ) ) ;
#14770 = CARTESIAN_POINT ( 'NONE',  ( 2.689816194747224110, 2.012238202079220439, -0.6693303307304664385 ) ) ;
#14771 = CARTESIAN_POINT ( 'NONE',  ( -6.286140498591554326, 7.362860665558790707, 1.199719254218452047 ) ) ;
#14772 = CARTESIAN_POINT ( 'NONE',  ( 4.258765444007106105, -1.603684720688375975, 1.449730421305382544 ) ) ;
#14773 = CARTESIAN_POINT ( 'NONE',  ( 3.069684041021227827, -1.094477399149307306, 1.480508570315848482 ) ) ;
#14774 = CARTESIAN_POINT ( 'NONE',  ( -4.159863475130535448, 7.428450666093093346, 0.7365534166655554049 ) ) ;
#14775 = CARTESIAN_POINT ( 'NONE',  ( 0.6823417656249882723, -0.09479166632524876901, 1.181850606188755259 ) ) ;
#14776 = CARTESIAN_POINT ( 'NONE',  ( 6.087833319296645840, -1.732659258567319505, -0.1633284621618599775 ) ) ;
#14777 = CARTESIAN_POINT ( 'NONE',  ( -4.407809337774280856, 7.196175756495025055, 1.082531754730549967 ) ) ;
#14778 = CARTESIAN_POINT ( 'NONE',  ( 4.284013352238246419, 6.021101549076499637, -1.443375672974051449 ) ) ;
#14779 = CARTESIAN_POINT ( 'NONE',  ( 1.499999999999987121, 3.577083334016152971, -0.8660254037844263841 ) ) ;
#14780 = CARTESIAN_POINT ( 'NONE',  ( 2.729541802387557059, -2.017400560480298033, 0.7770373237434913261 ) ) ;
#14781 = CARTESIAN_POINT ( 'NONE',  ( 4.007185349139028574, 2.006139037694018690, 0.2004037502189442987 ) ) ;
#14782 = CARTESIAN_POINT ( 'NONE',  ( -8.310784975052669665, 12.63974020429606249, -0.7216878364870267237 ) ) ;
#14784 = AXIS2_PLACEMENT_3D ( 'NONE', #48429, #132885, #183726 ) ;
#14783 = CARTESIAN_POINT ( 'NONE',  ( 2.483474991488154870, 1.976725341044349271, -0.8753317036461552014 ) ) ;
#14785 = CARTESIAN_POINT ( 'NONE',  ( 3.128153591792836252, 1.098079186366843985, -1.637025598404780791 ) ) ;
#14786 = CARTESIAN_POINT ( 'NONE',  ( 6.509000000000039421, 4.695815278351551214, 2.562658139094181386 ) ) ;
#14787 = CARTESIAN_POINT ( 'NONE',  ( 4.353030786369998850, 0.4220677823760305980, -1.895499586301018224 ) ) ;
#14790 = ORIENTED_EDGE ( 'NONE', *, *, #64546, .T. ) ;
#14789 = PRESENTATION_STYLE_ASSIGNMENT (( #126514 ) ) ;
#14788 = CARTESIAN_POINT ( 'NONE',  ( -8.880227426826648340, 11.38335130276301754, 1.443375672974064550 ) ) ;
#14791 = CARTESIAN_POINT ( 'NONE',  ( -3.323157048681004699, 6.891117300187535655, -0.7216878364870458196 ) ) ;
#14792 = CARTESIAN_POINT ( 'NONE',  ( 5.408776937209000657, 5.274937613024121674, 0.7998128361456352531 ) ) ;
#14794 = ORIENTED_EDGE ( 'NONE', *, *, #95866, .F. ) ;
#14793 = CARTESIAN_POINT ( 'NONE',  ( -4.956387674247580755, 7.940146832334256111, 1.199719254218452935 ) ) ;
#14795 = CARTESIAN_POINT ( 'NONE',  ( -6.982085920913410071, 11.08959130780024260, 0.7216878364870458196 ) ) ;
#14796 = CARTESIAN_POINT ( 'NONE',  ( 1.413402608508182556, 1.946665536341249503, 1.039416302365432587 ) ) ;
#14797 = CARTESIAN_POINT ( 'NONE',  ( 1.642778471875000035, -2.326041666188709112, -2.845375778867859751 ) ) ;
#14798 = CIRCLE ( 'NONE', #87489, 0.08000000000000015432 ) ;
#14799 = CARTESIAN_POINT ( 'NONE',  ( 5.155110299917927463, 1.633153276354940342, -1.086568599608192409 ) ) ;
#14800 = CARTESIAN_POINT ( 'NONE',  ( -0.6823417656249969321, 4.780208333674755394, -1.181850606188749264 ) ) ;
#14801 = CARTESIAN_POINT ( 'NONE',  ( -1.499999999999997780, 2.681250000682818158, 1.214306433183764966E-14 ) ) ;
#14802 = CARTESIAN_POINT ( 'NONE',  ( 0.1745949693968797123, 1.415412180343596837, -2.016327490378281073 ) ) ;
#14803 = CARTESIAN_POINT ( 'NONE',  ( 4.435397664686764330, 0.7849604969769330420, -1.665558179074405620 ) ) ;
#14804 = ORIENTED_EDGE ( 'NONE', *, *, #199216, .F. ) ;
#14805 = CARTESIAN_POINT ( 'NONE',  ( 1.360316468749994012, -0.9843749996586090845, -5.204170427930421283E-15 ) ) ;
#14806 = CARTESIAN_POINT ( 'NONE',  ( -6.157374318900681764, 10.33535380535947290, 0.7998128361456481317 ) ) ;
#14807 = CARTESIAN_POINT ( 'NONE',  ( 3.796405077356793438E-16, -0.5000000000000005551, -3.099999999999999201 ) ) ;
#14808 = CARTESIAN_POINT ( 'NONE',  ( 5.133110336712339183, 1.960249873928998410, 0.8093987030339530042 ) ) ;
#14809 = CARTESIAN_POINT ( 'NONE',  ( 4.611744806942754238, 8.532119374741881757, -0.7998128361456231517 ) ) ;
#14810 = VECTOR ( 'NONE', #46946, 1000.000000000000000 ) ;
#14811 = CARTESIAN_POINT ( 'NONE',  ( 6.925078400183531713, -0.004750840071900476122, 2.044148492825672569 ) ) ;
#14814 = CARTESIAN_POINT ( 'NONE',  ( 3.737712173649463399, 1.832726675769575486, 0.1767833568970395008 ) ) ;
#14813 = CARTESIAN_POINT ( 'NONE',  ( 0.9591554131188588794, 1.518337787816389284, 1.075887112759424280 ) ) ;
#14812 = CARTESIAN_POINT ( 'NONE',  ( 10.59765138761703085, 12.29999999999998472, 3.303242380465396533 ) ) ;
#14815 = CARTESIAN_POINT ( 'NONE',  ( 8.392660782059197189, 9.750191319612612872, 1.199719254218462483 ) ) ;
#14816 = CARTESIAN_POINT ( 'NONE',  ( 8.879134602966002987, 3.426985321572576293, 7.474367077670482473 ) ) ;
#14817 = CARTESIAN_POINT ( 'NONE',  ( -5.745623237141265882, 9.925253886631958622, 0.7998128361456291469 ) ) ;
#14818 = CYLINDRICAL_SURFACE ( 'NONE', #208509, 0.08000000000000020983 ) ;
#14819 = CARTESIAN_POINT ( 'NONE',  ( 3.668774463136436736, -1.482526648764719734, 1.634931011441637771 ) ) ;
#14820 = CARTESIAN_POINT ( 'NONE',  ( 6.169232171785941965, 0.1756554044750150145, -2.255672955852848993 ) ) ;
#14821 = CARTESIAN_POINT ( 'NONE',  ( -7.388830529767770550, 7.722649827591604677, 1.040834085586084257E-14 ) ) ;
#14822 = CARTESIAN_POINT ( 'NONE',  ( 5.888875516108613262, -1.723027129771546484, -0.5597982944235294633 ) ) ;
#14823 = CARTESIAN_POINT ( 'NONE',  ( 5.700375016119385130, 1.281441245451527600, -1.424251128553160273 ) ) ;
#14824 = CARTESIAN_POINT ( 'NONE',  ( -1.364683531250010295, 5.551041667008087543, -0.7879004041258300672 ) ) ;
#14825 = EDGE_CURVE ( 'NONE', #58688, #185939, #54952, .T. ) ;
#14826 = CARTESIAN_POINT ( 'NONE',  ( 6.368025811218641863, 0.9635043244729593059, 1.603280169136585220 ) ) ;
#14827 = CARTESIAN_POINT ( 'NONE',  ( 5.635155393647417910, -0.04589315835645593061, -1.860648885492953486 ) ) ;
#14828 = CARTESIAN_POINT ( 'NONE',  ( 0.000000000000000000, -9.999999999999994671, 10.99999999999999112 ) ) ;
#14829 = CARTESIAN_POINT ( 'NONE',  ( 6.420749384593221087, 1.653102913324438816, 0.6326092773807339142 ) ) ;
#14830 = CARTESIAN_POINT ( 'NONE',  ( 1.358611653602972646, -1.916354379050893009, -0.6279873632355145174 ) ) ;
#14832 = CARTESIAN_POINT ( 'NONE',  ( 2.367922061077184726, 2.065251240347278472, -0.4117205849265455075 ) ) ;
#14831 = CARTESIAN_POINT ( 'NONE',  ( -10.47775378526269918, 11.11846759242831872, -0.7998128361456221525 ) ) ;
#14833 = CARTESIAN_POINT ( 'NONE',  ( 7.574201371528760163, 11.98831870009225931, 1.040834085586084257E-14 ) ) ;
#14835 = CARTESIAN_POINT ( 'NONE',  ( -9.826962411806732689, 10.35921099006301382, -0.7998128361456291469 ) ) ;
#14834 = DIRECTION ( 'NONE',  ( 1.276756478318932585E-15, -1.000000000000000000, 1.665334536937738262E-16 ) ) ;
#14836 = CYLINDRICAL_SURFACE ( 'NONE', #179373, 2.000000000000006661 ) ;
#14837 = CARTESIAN_POINT ( 'NONE',  ( 2.531515522815621200, -0.1936091499190935594, 2.010454966646264552 ) ) ;
#14838 = CARTESIAN_POINT ( 'NONE',  ( -1.364683531249997417, 3.759375000341423689, 1.214306433183764966E-14 ) ) ;
#14839 = CARTESIAN_POINT ( 'NONE',  ( 9.029367117021314115, 12.51771682229149008, -1.082531754730543083 ) ) ;
#14840 = CARTESIAN_POINT ( 'NONE',  ( 3.005316911853897821, 1.824354345256746557, 1.159134172154026032 ) ) ;
#14841 = CARTESIAN_POINT ( 'NONE',  ( 6.610000000000010090, 4.687934210475516394, 2.842562027763709587 ) ) ;
#14843 = CARTESIAN_POINT ( 'NONE',  ( 4.524302555594479358, 8.500379758160722332, 0.3357913727640315371 ) ) ;
#14842 = CARTESIAN_POINT ( 'NONE',  ( 7.842465510862060896, 8.114240948952696542, 0.000000000000000000 ) ) ;
#14844 = CARTESIAN_POINT ( 'NONE',  ( 10.34450801710256584, 11.17094022948226240, 0.7216878364870438212 ) ) ;
#14845 = CARTESIAN_POINT ( 'NONE',  ( 8.230276427067300560, 15.16059583899921037, -8.673450386635328968 ) ) ;
#14846 = CARTESIAN_POINT ( 'NONE',  ( -7.429504990608782222, 8.730472579540773381, 1.082531754730549967 ) ) ;
#14847 = CARTESIAN_POINT ( 'NONE',  ( -1.402160292154681736E-14, 0.6968750003414164729, -1.575800808251659024 ) ) ;
#14848 = CARTESIAN_POINT ( 'NONE',  ( 1.417800074541092137, -1.221294057239637576, -1.819523406426680090 ) ) ;
#14849 = CARTESIAN_POINT ( 'NONE',  ( 3.179715765502657554, 5.975770656120749535, -2.500000000000002220 ) ) ;
#14850 = CARTESIAN_POINT ( 'NONE',  ( 2.219920553356643289, -2.194584817558010936, 0.5498286310916412623 ) ) ;
#14851 = CARTESIAN_POINT ( 'NONE',  ( -7.751511138711140170, 10.06651563329490529, -1.599625672291263179 ) ) ;
#14852 = CARTESIAN_POINT ( 'NONE',  ( -4.921246571636213929, 4.843801876438091902, 0.7216878364870317197 ) ) ;
#14853 = CARTESIAN_POINT ( 'NONE',  ( 1.364683531249990311, 3.446875000341416584, 1.214306433183764966E-14 ) ) ;
#14854 = CARTESIAN_POINT ( 'NONE',  ( 5.886377668569586774, 7.162856863344262415, 1.137212067324339104 ) ) ;
#14855 = CARTESIAN_POINT ( 'NONE',  ( -1.500000000000008216, 11.49999999999999645, 3.469446951953614189E-15 ) ) ;
#14856 = CARTESIAN_POINT ( 'NONE',  ( 4.577813143269636065, 5.369812084349879555, -1.199719254218450271 ) ) ;
#14857 = CARTESIAN_POINT ( 'NONE',  ( 3.532247091833766284, 1.725908789131404220, 0.3905704408769093416 ) ) ;
#14858 = AXIS2_PLACEMENT_3D ( 'NONE', #156926, #206714, #58342 ) ;
#14859 = CARTESIAN_POINT ( 'NONE',  ( 6.194375513154499302, -2.195555142843173879, -0.2223249613259313806 ) ) ;
#14860 = CIRCLE ( 'NONE', #139531, 12.00000000000000178 ) ;
#14861 = CARTESIAN_POINT ( 'NONE',  ( 0.6823417656249969321, 9.526041667008065872, -1.181850606188757036 ) ) ;
#14862 = ORIENTED_EDGE ( 'NONE', *, *, #48534, .F. ) ;
#14863 = CARTESIAN_POINT ( 'NONE',  ( -6.448838341955544173, 7.552674816150118708, 1.199719254218452047 ) ) ;
#14864 = CARTESIAN_POINT ( 'NONE',  ( 5.607046053289695742, -0.04666138757647776691, 2.016035322322209389 ) ) ;
#14865 = ORIENTED_EDGE ( 'NONE', *, *, #139862, .T. ) ;
#14866 = CARTESIAN_POINT ( 'NONE',  ( 3.766346201128992988, -1.256895078192099335, 1.385637336983977397 ) ) ;
#14867 = CARTESIAN_POINT ( 'NONE',  ( 3.186448005867897670, 1.153939711166888982, -1.718631068965512210 ) ) ;
#14868 = CARTESIAN_POINT ( 'NONE',  ( -7.892254816486440561, 8.380254505421877553, 0.000000000000000000 ) ) ;
#14869 = DIRECTION ( 'NONE',  ( -1.735552045436534953E-14, 0.6004703560067730095, 0.7996470168499969500 ) ) ;
#14870 = CARTESIAN_POINT ( 'NONE',  ( -1.249999999999946487, 8.500000000000000000, 15.75000000000000000 ) ) ;
#14871 = CARTESIAN_POINT ( 'NONE',  ( -1.001543065824772872E-14, 4.384375000341417916, 1.575800808251672791 ) ) ;
#14872 = CARTESIAN_POINT ( 'NONE',  ( 1.845825534506392085, -1.251752223804462272, -1.445855903880132631 ) ) ;
#14873 = CARTESIAN_POINT ( 'NONE',  ( 3.174217076811707727, -0.9646401420641316227, -1.708233030250068785 ) ) ;
#14874 = CARTESIAN_POINT ( 'NONE',  ( 1.440779594245532369, 1.198675164295496920, 1.620935466883965503 ) ) ;
#14875 = CARTESIAN_POINT ( 'NONE',  ( -4.984557751679625781, 5.844347460828191565, 1.199719254218452935 ) ) ;
#14877 =( NAMED_UNIT ( * ) PLANE_ANGLE_UNIT ( ) SI_UNIT ( $, .RADIAN. ) );
#14876 = CARTESIAN_POINT ( 'NONE',  ( 8.555358625423188812, 9.940005470203933768, 1.199719254218462483 ) ) ;
#14878 = CARTESIAN_POINT ( 'NONE',  ( 6.186792457355818620, -0.2869052490914354991, -1.950236548312431317 ) ) ;
#14879 = CARTESIAN_POINT ( 'NONE',  ( 1.364683531249988535, 3.113541667008083991, 0.7879004041258500513 ) ) ;
#14880 = CARTESIAN_POINT ( 'NONE',  ( 1.845949328209312901, -1.318067166357287379, -1.521789114188701664 ) ) ;
#14882 = CARTESIAN_POINT ( 'NONE',  ( 2.583745723679788497, -0.6611301898758483730, 2.011445711247431323 ) ) ;
#14881 = CARTESIAN_POINT ( 'NONE',  ( -7.700668062882084719, 8.086460282891644979, -0.7216878364870278340 ) ) ;
#14883 = CARTESIAN_POINT ( 'NONE',  ( 9.449756383040847751, 11.01506308870569306, -7.402102152998049078 ) ) ;
#14884 = CARTESIAN_POINT ( 'NONE',  ( 4.070807014193541740, 1.466255041752505539, -1.461937513464212079 ) ) ;
#14885 = CARTESIAN_POINT ( 'NONE',  ( 3.250922972226694352, 7.014770244231638863, 0.7998128361456281477 ) ) ;
#14887 = CARTESIAN_POINT ( 'NONE',  ( 3.785751206713845018, 5.439795712631356750, 1.599625672291267398 ) ) ;
#14886 = CARTESIAN_POINT ( 'NONE',  ( 5.525362607580523111, -1.325732906064909677, -1.616523167544873241 ) ) ;
#14889 = ORIENTED_EDGE ( 'NONE', *, *, #91598, .T. ) ;
#14888 = CARTESIAN_POINT ( 'NONE',  ( 4.700122295916242088, -1.825221593135372578, -0.04401369772454033491 ) ) ;
#14890 = CARTESIAN_POINT ( 'NONE',  ( 8.727698198895078363, 11.20540053684285553, -1.599625672291257406 ) ) ;
#14891 = CARTESIAN_POINT ( 'NONE',  ( 6.890000000000005898, 7.052460701731090076, 2.598152593539102551 ) ) ;
#14893 = MECHANICAL_DESIGN_GEOMETRIC_PRESENTATION_REPRESENTATION (  '', ( #59920 ), #63328 ) ;
#14892 = CARTESIAN_POINT ( 'NONE',  ( 9.686381629184177555, 13.40773330361598248, 8.159561931930056744 ) ) ;
#14894 = CARTESIAN_POINT ( 'NONE',  ( 6.821333372217227797, -0.1664864972488830919, 2.170661319153658564 ) ) ;
#14895 = CARTESIAN_POINT ( 'NONE',  ( 0.6823417656249969321, 10.08854166700806587, -1.181850606188757036 ) ) ;
#14896 = VERTEX_POINT ( 'NONE', #28209 ) ;
#14897 = CARTESIAN_POINT ( 'NONE',  ( 4.986922676292999235, -1.801926769106906745, -0.6406197933803285949 ) ) ;
#14898 = CARTESIAN_POINT ( 'NONE',  ( -10.30827686509187835, 10.92074451889568643, 1.040834085586084257E-14 ) ) ;
#14899 = CARTESIAN_POINT ( 'NONE',  ( 6.608709811657416999, 9.797579649320619311, -1.199719254218440723 ) ) ;
#14900 = CARTESIAN_POINT ( 'NONE',  ( -0.6801582343750438575, 1.630208333674734611, -1.178068619123879834 ) ) ;
#14901 = CARTESIAN_POINT ( 'NONE',  ( 5.355107487273504496, 6.310342158982962246, -1.082531754730543083 ) ) ;
#14902 = CARTESIAN_POINT ( 'NONE',  ( 9.566809970445889988, -7.630846356335490022, -1.058098698307930843E-15 ) ) ;
#14903 = CARTESIAN_POINT ( 'NONE',  ( 8.634934822016738565, 13.76316009741527679, -8.269602696052166024 ) ) ;
#14904 = CARTESIAN_POINT ( 'NONE',  ( 0.4504185290156898502, -1.555054577268409899, -0.9855837367087336709 ) ) ;
#14905 = ORIENTED_EDGE ( 'NONE', *, *, #181245, .F. ) ;
#14906 =( LENGTH_UNIT ( ) NAMED_UNIT ( * ) SI_UNIT ( .MILLI., .METRE. ) );
#14907 = CARTESIAN_POINT ( 'NONE',  ( 5.237510374101456812, -1.321932271818569093, -1.323673891312632245 ) ) ;
#14908 = CARTESIAN_POINT ( 'NONE',  ( 10.99970480893080449, -5.740513804456437441, 0.08058608058608245084 ) ) ;
#14909 = CYLINDRICAL_SURFACE ( 'NONE', #44833, 0.5000000000000003331 ) ;
#14910 = DIRECTION ( 'NONE',  ( 0.000000000000000000, 0.000000000000000000, -1.000000000000000000 ) ) ;
#14911 = TOROIDAL_SURFACE ( 'NONE', #70267, 1.821370322827223553, 0.2000000000000000111 ) ;
#14912 = CARTESIAN_POINT ( 'NONE',  ( -5.694061328059534688, 8.626526735169329996, 1.082531754730548412 ) ) ;
#14913 = CARTESIAN_POINT ( 'NONE',  ( 3.337278367258157630, 7.045241861776501580, 0.7998128361456341429 ) ) ;
#14914 = CARTESIAN_POINT ( 'NONE',  ( 1.727339394501678838, 0.1499709341525606032, -1.963822474445919175 ) ) ;
#14915 = CARTESIAN_POINT ( 'NONE',  ( 2.021111450618333194, -1.799914642762674433, 0.9091633978678403949 ) ) ;
#14916 = CARTESIAN_POINT ( 'NONE',  ( -6.821723845970312894, 11.11042825360738284, 0.000000000000000000 ) ) ;
#14917 = CARTESIAN_POINT ( 'NONE',  ( 4.878955176071345434, 6.785476686873604280, -1.599625672291269396 ) ) ;
#14918 = DIRECTION ( 'NONE',  ( -5.578564026256490882E-16, -1.000000000000000000, -9.066213480720158442E-32 ) ) ;
#14919 = CARTESIAN_POINT ( 'NONE',  ( 2.519692321801832335, -1.262790281060278907, -1.790845962237663791 ) ) ;
#14920 = CARTESIAN_POINT ( 'NONE',  ( 2.540289672789934450, 0.3621416576072679083, -0.2590487051680201436 ) ) ;
#14921 = CARTESIAN_POINT ( 'NONE',  ( -9.996439331977562404, 10.55693406359564790, 0.7998128361456462443 ) ) ;
#14922 = DIRECTION ( 'NONE',  ( -0.7592566023652994600, 0.6507913734559651608, 0.000000000000000000 ) ) ;
#14923 = CARTESIAN_POINT ( 'NONE',  ( 5.531363484695498656, 5.555604941674001651, -0.7216878364870402685 ) ) ;
#14924 = CARTESIAN_POINT ( 'NONE',  ( 9.772729797352075920, 10.29593960653257234, -0.7998128361456281477 ) ) ;
#14925 = DIRECTION ( 'NONE',  ( 0.7592566023653005702, -0.6507913734559639396, 0.000000000000000000 ) ) ;
#14926 = CARTESIAN_POINT ( 'NONE',  ( 5.885648082108188461, 8.920320958217979879, 1.082531754730549967 ) ) ;
#14927 = ORIENTED_EDGE ( 'NONE', *, *, #212414, .T. ) ;
#14929 = CARTESIAN_POINT ( 'NONE',  ( 1.330727748098162078, 1.350296381755649922, -1.493239990923441951 ) ) ;
#14928 = CARTESIAN_POINT ( 'NONE',  ( 4.880324068823122197, -0.2306306682541107433, -1.826696389425507938 ) ) ;
#14930 = CARTESIAN_POINT ( 'NONE',  ( 3.620768967900461099, 0.5618574718093732878, -2.228542275653460969 ) ) ;
#14932 = CARTESIAN_POINT ( 'NONE',  ( 2.201794467188260995, 0.7177229581568910222, -1.717183780122087056 ) ) ;
#14931 = DIRECTION ( 'NONE',  ( 6.314299915563594049E-62, 8.546850786086437571E-32, 1.000000000000000000 ) ) ;
#14933 = CARTESIAN_POINT ( 'NONE',  ( 3.285556943749998737, -3.055208332855376518, -1.896917185911906500 ) ) ;
#14934 = SURFACE_STYLE_FILL_AREA ( #81030 ) ;
#14935 = CARTESIAN_POINT ( 'NONE',  ( 5.660397963661894849, 1.910509065610028090, 0.08734628876111423523 ) ) ;
#14936 = CARTESIAN_POINT ( 'NONE',  ( -9.481229494658258261, 9.955855920056455588, -0.7998128361456291469 ) ) ;
#14937 = EDGE_CURVE ( 'NONE', #15686, #155820, #116760, .T. ) ;
#14938 = CARTESIAN_POINT ( 'NONE',  ( -5.289089323106922258, 9.184704953684462936, 0.7216878364870267237 ) ) ;
#14940 = CARTESIAN_POINT ( 'NONE',  ( 3.133525119713890472, -1.255248497922526463, -1.387151338369890574 ) ) ;
#14939 = CARTESIAN_POINT ( 'NONE',  ( 4.669523271137602904, 1.205110262999141701, 1.708276167780866661 ) ) ;
#14941 = CARTESIAN_POINT ( 'NONE',  ( 7.782016984564065432, 8.181367358187307204, 0.7216878364870458196 ) ) ;
#14942 = CARTESIAN_POINT ( 'NONE',  ( 5.653808312887880660, 0.7519890275384639722, 1.680886247995525773 ) ) ;
#14943 = CARTESIAN_POINT ( 'NONE',  ( 2.171277156482887882, 5.684907115872006145, -0.7998128361456291469 ) ) ;
#14944 = CARTESIAN_POINT ( 'NONE',  ( -5.599154252763867134, 5.634694171087028636, 0.000000000000000000 ) ) ;
#14945 = CARTESIAN_POINT ( 'NONE',  ( 4.828557952505812878, 1.651878126777156730, 0.4964739870837226454 ) ) ;
#14946 = CARTESIAN_POINT ( 'NONE',  ( -6.196239896645333367, 7.187700286629718605, -1.199719254218446718 ) ) ;
#14947 = CARTESIAN_POINT ( 'NONE',  ( 0.8087042982808723135, 1.034539495461658465, -1.391586887084266921 ) ) ;
#14948 = CARTESIAN_POINT ( 'NONE',  ( 0.000000000000000000, 4.000000000000003553, 0.000000000000000000 ) ) ;
#14949 =( NAMED_UNIT ( * ) SI_UNIT ( $, .STERADIAN. ) SOLID_ANGLE_UNIT ( ) );
#14950 = CARTESIAN_POINT ( 'NONE',  ( 4.329095027809041873, -2.023602029403932079, -0.7869089946421561343 ) ) ;
#14951 = CARTESIAN_POINT ( 'NONE',  ( 3.316849939159485228, 1.650902842016691130, 0.7798126646740562995 ) ) ;
#14952 = CARTESIAN_POINT ( 'NONE',  ( 0.8132426064601482318, -1.654215606812576400, -1.054277637385622857 ) ) ;
#14953 = CARTESIAN_POINT ( 'NONE',  ( 5.841034576552271318, -1.817201478619561383, -1.086431860386444681 ) ) ;
#14955 = CARTESIAN_POINT ( 'NONE',  ( -1.364683531249997417, 3.571875000341423245, 1.214306433183764966E-14 ) ) ;
#14954 = CARTESIAN_POINT ( 'NONE',  ( 5.917577160708873407, -1.270305590232129633, -1.908037719346373784 ) ) ;
#14956 = CARTESIAN_POINT ( 'NONE',  ( 9.716492259128738596, -7.972382850425319134, -0.4652101495396395170 ) ) ;
#14957 = CARTESIAN_POINT ( 'NONE',  ( 7.567422294721922960, 11.98040977715095323, 0.7998128361456462443 ) ) ;
#14958 = CARTESIAN_POINT ( 'NONE',  ( 1.612141420133822223, -0.7113448269009944314, 1.997755531611951962 ) ) ;
#14959 = CARTESIAN_POINT ( 'NONE',  ( -5.111060722671894929, 5.065251719313053513, 0.000000000000000000 ) ) ;
#14960 = DIRECTION ( 'NONE',  ( 0.6507913734559640506, -0.7592566023653004592, 0.000000000000000000 ) ) ;
#14961 = CARTESIAN_POINT ( 'NONE',  ( -5.558479791478509568, 5.587240632920778438, 0.000000000000000000 ) ) ;
#14962 =( BOUNDED_CURVE ( )  B_SPLINE_CURVE ( 2, ( #137176, #72136, #55909, #3922, #203200, #86274, #74301 ),
 .UNSPECIFIED., .F., .T. ) 
 B_SPLINE_CURVE_WITH_KNOTS ( ( 3, 2, 2, 3 ),
 ( 0.1964285714285713413, 0.2023809523809523836, 0.2083333333333334536, 0.2142857142857144681 ),
 .UNSPECIFIED. ) 
 CURVE ( )  GEOMETRIC_REPRESENTATION_ITEM ( )  RATIONAL_B_SPLINE_CURVE ( ( 1.000000000000001776, 0.8660254037844368202, 1.000000000000000000, 0.8660254037844387076, 1.000000000000000000, 0.8660254037844343777, 1.000000000000004441 ) ) 
 REPRESENTATION_ITEM ( '' )  );
#14963 = CARTESIAN_POINT ( 'NONE',  ( 6.121977192509519661, 2.140326789316211453, -0.3632143409003502077 ) ) ;
#14965 = CARTESIAN_POINT ( 'NONE',  ( -1.500000000000008216, 12.28125000068279427, 3.469446951953614189E-15 ) ) ;
#14964 = CARTESIAN_POINT ( 'NONE',  ( 6.983263157960333700, 2.949816178198962024, 2.606004571833001382 ) ) ;
#14967 = ORIENTED_EDGE ( 'NONE', *, *, #198798, .F. ) ;
#14966 = CARTESIAN_POINT ( 'NONE',  ( 2.666879960053496479, 0.7507478997158049117, 2.090701262698462681 ) ) ;
#14968 = CARTESIAN_POINT ( 'NONE',  ( -0.1219072497536327904, -0.5225375287686329084, -2.247936139081475382 ) ) ;
#14970 = CARTESIAN_POINT ( 'NONE',  ( 5.260619331934998755, -0.6897241169346832734, -1.943984935097947675 ) ) ;
#14969 = CARTESIAN_POINT ( 'NONE',  ( 5.359550796103802028, 5.147230771742885125, -0.7998128361456231517 ) ) ;
#14972 = CARTESIAN_POINT ( 'NONE',  ( -1.737499999999997824, -2.041666666666667407, 3.009438278150925683 ) ) ;
#14971 = CARTESIAN_POINT ( 'NONE',  ( 4.206772801990143584, 8.129928378955675328, 0.7998128361456271485 ) ) ;
#14973 = CARTESIAN_POINT ( 'NONE',  ( 6.723917837734620484, 6.809268663637336516, 0.000000000000000000 ) ) ;
#14974 = B_SPLINE_CURVE_WITH_KNOTS ( 'NONE', 3,
 ( #194320, #161840, #15547, #13428, #181262, #146671, #49153, #113144, #79504, #115270, #211618, #179150, #30774, #64328 ),
 .UNSPECIFIED., .F., .F.,
 ( 4, 2, 2, 2, 2, 2, 4 ),
 ( 0.5002398796579472506, 0.5986944666282260075, 0.6971490535985047643, 0.7956036405687834101, 0.8202172873113531271, 0.8448309340539227330, 0.8940582275390620559 ),
 .UNSPECIFIED. ) ;
#14975 = CARTESIAN_POINT ( 'NONE',  ( 1.642778471875001811, -0.3427083328553758301, 2.845375778867859751 ) ) ;
#14976 = CARTESIAN_POINT ( 'NONE',  ( 0.2331563151865486128, 1.372759770070256291, -2.202161770551560149 ) ) ;
#14977 = CARTESIAN_POINT ( 'NONE',  ( 6.075717905342373548, -0.9791751913862613010, 1.559117742379905858 ) ) ;
#14979 = ORIENTED_EDGE ( 'NONE', *, *, #185505, .T. ) ;
#14978 = CARTESIAN_POINT ( 'NONE',  ( 3.981290663907289140, 7.796589541200495965, -0.7998128361456221525 ) ) ;
#14980 = CARTESIAN_POINT ( 'NONE',  ( 1.465380626080296400, 1.700101026837578466, -0.2896415544312477830 ) ) ;
#14981 = CARTESIAN_POINT ( 'NONE',  ( -0.2409995289980038091, -0.004801160710915519658, -2.000252362011435636 ) ) ;
#14982 = CARTESIAN_POINT ( 'NONE',  ( 2.004881263662112723, -2.228613174808518060, 0.5628491883087839431 ) ) ;
#14983 = CARTESIAN_POINT ( 'NONE',  ( 1.364683531249990311, 3.696875000341416584, 1.214306433183764966E-14 ) ) ;
#14984 =( BOUNDED_CURVE ( )  B_SPLINE_CURVE ( 2, ( #213662, #65287, #197436, #131434, #212615, #30700, #64255, #129346, #29627 ),
 .UNSPECIFIED., .F., .T. ) 
 B_SPLINE_CURVE_WITH_KNOTS ( ( 3, 2, 2, 2, 3 ),
 ( 0.2968749999999997780, 0.3020833333333333148, 0.3125000000000000000, 0.3229166666666666852, 0.3281250000000001665 ),
 .UNSPECIFIED. ) 
 CURVE ( )  GEOMETRIC_REPRESENTATION_ITEM ( )  RATIONAL_B_SPLINE_CURVE ( ( 0.9330127018922194093, 0.9330127018922165227, 1.000000000000000000, 0.8660254037844387076, 1.000000000000000000, 0.8660254037844387076, 1.000000000000000000, 0.9330127018922171889, 0.9330127018922194093 ) ) 
 REPRESENTATION_ITEM ( '' )  );
#14985 = CARTESIAN_POINT ( 'NONE',  ( 2.407839351892237634, -0.4975810599385386834, 2.206854368276117917 ) ) ;
#14986 = CARTESIAN_POINT ( 'NONE',  ( 4.529967234949650035, -1.295318019757265349, -1.660530462842347177 ) ) ;
#14987 = CARTESIAN_POINT ( 'NONE',  ( -5.953438850176548947, 9.959779401932374654, 0.000000000000000000 ) ) ;
#14988 = CARTESIAN_POINT ( 'NONE',  ( 2.758786678070863196, -1.537680025927037786, -0.8759604286991302668 ) ) ;
#14989 = CARTESIAN_POINT ( 'NONE',  ( 6.287230548435207567, 8.358188277972981695, -1.599625672291262513 ) ) ;
#14990 = CARTESIAN_POINT ( 'NONE',  ( 6.170369307550831017, 6.371388078330353366, 0.7216878364870328300 ) ) ;
#14991 = CARTESIAN_POINT ( 'NONE',  ( -6.358937740009323214, 7.377514437221045718, -1.199719254218446718 ) ) ;
#14992 = UNCERTAINTY_MEASURE_WITH_UNIT (LENGTH_MEASURE( 1.000000000000000082E-05 ), #112474, 'distance_accuracy_value', 'NONE');
#14993 = CARTESIAN_POINT ( 'NONE',  ( -0.7500000000000006661, 1.858333333333357595, -1.299038105676652011 ) ) ;
#14994 = CARTESIAN_POINT ( 'NONE',  ( 5.765950734523942245, 0.6451602502356535984, -2.125694943049365904 ) ) ;
#14995 = CARTESIAN_POINT ( 'NONE',  ( 3.890727776643727598, 1.851661642969665067, -1.171806376371389957 ) ) ;
#14996 = CARTESIAN_POINT ( 'NONE',  ( -4.436542580169821726, 6.199052314996659874, 1.599625672291267398 ) ) ;
#14997 = DIRECTION ( 'NONE',  ( 0.000000000000000000, -1.000000000000000000, 0.000000000000000000 ) ) ;
#14998 =( BOUNDED_SURFACE ( )  B_SPLINE_SURFACE ( 3, 2, ( 
 ( #101774, #167842, #85519 ),
 ( #135362, #201377, #117023 ),
 ( #180891, #53018, #32513 ),
 ( #149463, #1046, #16234 ),
 ( #166782, #183019, #102845 ),
 ( #168902, #18377, #70309 ) ),
 .UNSPECIFIED., .F., .F., .F. ) 
 B_SPLINE_SURFACE_WITH_KNOTS ( ( 4, 2, 4 ),
 ( 3, 3 ),
 ( 0.000000000000000000, 0.0003831416164015014384, 0.0007662832328030028768 ),
 ( 0.000000000000000000, 1.000000000000000000 ),
 .UNSPECIFIED. ) 
 GEOMETRIC_REPRESENTATION_ITEM ( )  RATIONAL_B_SPLINE_SURFACE ( (
 ( 1.000000000000000000, 0.7071067811865475727, 1.000000000000000000),
 ( 1.000000000000000000, 0.6829713513656784363, 1.000000000000000000),
 ( 1.000000000000000000, 0.6534833722367711095, 1.000000000000000000),
 ( 1.000000000000000000, 0.6054027484667287018, 1.000000000000000000),
 ( 1.000000000000000000, 0.5875453974411402047, 1.000000000000000000),
 ( 1.000000000000000000, 0.5879095031487528988, 1.000000000000000000) ) ) 
 REPRESENTATION_ITEM ( '' )  SURFACE ( )  );
#14999 = CARTESIAN_POINT ( 'NONE',  ( 6.428397668822618094, -0.9990526908794925554, -1.870407359624715937 ) ) ;
#15000 = STYLED_ITEM ( 'NONE', ( #143462 ), #66312 ) ;
#15001 = CARTESIAN_POINT ( 'NONE',  ( -1.364683531250012516, 2.738541667008090208, -0.7879004041258289570 ) ) ;
#15002 = CARTESIAN_POINT ( 'NONE',  ( -1.402160292154681736E-14, 9.171875000341396245, 1.575800808251682339 ) ) ;
#15003 = CARTESIAN_POINT ( 'NONE',  ( -3.118012141462980669, 6.581505231774690046, 0.7216878364870317197 ) ) ;
#15004 = CARTESIAN_POINT ( 'NONE',  ( 6.047156637250688860, 0.2094617991648151656, 2.110256208591613003 ) ) ;
#15005 = CARTESIAN_POINT ( 'NONE',  ( -5.885648082108231982, 7.959951743916638733, 1.443375672974058777 ) ) ;
#15006 = ORIENTED_EDGE ( 'NONE', *, *, #116999, .F. ) ;
#15009 = MECHANICAL_DESIGN_GEOMETRIC_PRESENTATION_REPRESENTATION (  '', ( #118843 ), #174174 ) ;
#15008 = CARTESIAN_POINT ( 'NONE',  ( 4.207966135563057541, 7.175396087857926375, 1.156120096431498379 ) ) ;
#15007 = CARTESIAN_POINT ( 'NONE',  ( -3.987506576194992824, 7.666191748953863794, 0.7216878364870338292 ) ) ;
#15010 = CARTESIAN_POINT ( 'NONE',  ( 6.328958779480917229, 6.278206752349526631, 0.7998128361456341429 ) ) ;
#15011 = ADVANCED_FACE ( 'NONE', ( #162489 ), #14062, .T. ) ;
#15012 = CARTESIAN_POINT ( 'NONE',  ( 5.864778394761136049, 0.1288883805774850844, -1.836796581567698539 ) ) ;
#15013 = CARTESIAN_POINT ( 'NONE',  ( -5.616896113772630983, 5.725669352255732036, 0.1283408312532021145 ) ) ;
#15014 = DIRECTION ( 'NONE',  ( -1.000000000000000000, 0.000000000000000000, 0.000000000000000000 ) ) ;
#15015 = CARTESIAN_POINT ( 'NONE',  ( -0.6823417656250212460, 4.363541667008085767, 1.181850606188767472 ) ) ;
#15016 = CARTESIAN_POINT ( 'NONE',  ( 2.524636229566870060, -1.623295675544262906, 0.6281775017502010394 ) ) ;
#15017 = CARTESIAN_POINT ( 'NONE',  ( -6.172557777799569934, 6.616364562750757905, -0.6295236542525488588 ) ) ;
#15018 = CARTESIAN_POINT ( 'NONE',  ( -9.499766273075886502, -10.00000000000010303, 0.06663900456894483737 ) ) ;
#15019 = CARTESIAN_POINT ( 'NONE',  ( -0.6823417656250246877, -0.3864583329919110688, 1.181850606188755259 ) ) ;
#15020 = CARTESIAN_POINT ( 'NONE',  ( 1.028703311283776586E-15, 0.000000000000000000, -8.300000000000000711 ) ) ;
#15021 = CARTESIAN_POINT ( 'NONE',  ( 6.209879897626497502, -2.145988306206991325, 0.2596296833028768347 ) ) ;
#15022 = CARTESIAN_POINT ( 'NONE',  ( -9.484092147959342967, 11.02352791316275216, 1.199719254218462483 ) ) ;
#15023 = CARTESIAN_POINT ( 'NONE',  ( -5.870317324592811303, 8.832158731124840401, -1.082531754730537976 ) ) ;
#15024 = CARTESIAN_POINT ( 'NONE',  ( 5.946190753372003535, 2.158995856162956084, 0.1107517376499680406 ) ) ;
#15026 = EDGE_LOOP ( 'NONE', ( #96487, #105535, #52255, #94848 ) ) ;
#15025 = CARTESIAN_POINT ( 'NONE',  ( -4.995253251992230581, 4.792493313604505367, 0.000000000000000000 ) ) ;
#15027 = CARTESIAN_POINT ( 'NONE',  ( -0.6823417656249969321, 4.967708333674755394, -1.181850606188749264 ) ) ;
#15028 = CARTESIAN_POINT ( 'NONE',  ( 5.782488548463037503, -1.922744423562244620, -0.4343835447332323740 ) ) ;
#15029 = CARTESIAN_POINT ( 'NONE',  ( 4.921093860428086941, 0.6645110682935355673, 1.601655696547391594 ) ) ;
#15031 = CARTESIAN_POINT ( 'NONE',  ( 2.366952063387484095, 0.1042156695447923470, -2.189191704635709890 ) ) ;
#15030 = CARTESIAN_POINT ( 'NONE',  ( 0.6801582343749883464, -0.6927083329919120347, -1.178068619123862515 ) ) ;
#15032 = CARTESIAN_POINT ( 'NONE',  ( 3.153680125570026416, -1.885591857120081372, -1.329971080218894874 ) ) ;
#15033 = CARTESIAN_POINT ( 'NONE',  ( 6.186805567823734364, -0.2977626877682394424, -2.039013576910824632 ) ) ;
#15034 = CARTESIAN_POINT ( 'NONE',  ( 0.8494333778440340543, 1.939759575794866242, -0.09477157414044742878 ) ) ;
#15035 = CARTESIAN_POINT ( 'NONE',  ( -5.870317324592812191, 7.871789516823500144, -1.443375672974051449 ) ) ;
#15036 = CARTESIAN_POINT ( 'NONE',  ( -5.327428015527048366, 5.180030537728460338, -0.7998128361456362523 ) ) ;
#15037 = CARTESIAN_POINT ( 'NONE',  ( -5.608665566507964328, 5.643324313368172973, -0.3498717110727275204 ) ) ;
#15038 = CARTESIAN_POINT ( 'NONE',  ( 3.463236921083117981, -1.731491641549892435, 1.224000437801611163 ) ) ;
#15039 = CARTESIAN_POINT ( 'NONE',  ( 0.000000000000000000, 8.500000000000000000, 0.000000000000000000 ) ) ;
#15040 = CARTESIAN_POINT ( 'NONE',  ( 1.793592486599729252, 1.492254607734722072, -1.356300734917381678 ) ) ;
#15041 = CARTESIAN_POINT ( 'NONE',  ( -5.300874872818844175, 7.207439989753867238, 1.443375672974064550 ) ) ;
#15042 = CARTESIAN_POINT ( 'NONE',  ( 5.087059579022827904, -0.2656672225294122169, -2.190654145894948890 ) ) ;
#15043 = CARTESIAN_POINT ( 'NONE',  ( 1.642778471875001811, -0.7802083328553761632, 2.845375778867859751 ) ) ;
#15044 = CARTESIAN_POINT ( 'NONE',  ( -2.130563195606704152, 5.637407494849765222, -0.3975762604357975238 ) ) ;
#15045 = CARTESIAN_POINT ( 'NONE',  ( -1.420000000000077423, 7.388542872122504157, 4.154462424328221104 ) ) ;
#15046 = CARTESIAN_POINT ( 'NONE',  ( -5.738844160334429567, 9.917344963690652548, 0.000000000000000000 ) ) ;
#15048 = CARTESIAN_POINT ( 'NONE',  ( -10.14375151705083766, -9.181160345032697734, 0.1770598413457937226 ) ) ;
#15047 = CARTESIAN_POINT ( 'NONE',  ( -5.012442140716328431, 8.020463026761962766, 1.150573971286508845 ) ) ;
#15049 = FILL_AREA_STYLE ('',( #165590 ) ) ;
#15050 = ORIENTED_EDGE ( 'NONE', *, *, #188144, .F. ) ;
#15051 = CARTESIAN_POINT ( 'NONE',  ( 4.645419472943275174, -1.591690889772362283, -1.309095959863779246 ) ) ;
#15052 = CARTESIAN_POINT ( 'NONE',  ( 4.057778671964185513, 7.726788352570485685, -0.5270377139656738930 ) ) ;
#15053 = B_SPLINE_CURVE_WITH_KNOTS ( 'NONE', 3,
 ( #77076, #27256, #144275, #78144 ),
 .UNSPECIFIED., .F., .F.,
 ( 4, 4 ),
 ( 0.000000000000000000, 9.170750102249612288E-05 ),
 .UNSPECIFIED. ) ;
#15054 = CARTESIAN_POINT ( 'NONE',  ( 0.5086597423466597823, 6.727065972568171404, -3.461085622288095021 ) ) ;
#15055 = CARTESIAN_POINT ( 'NONE',  ( -5.766295404513795297, 5.621766148221195358, 0.7998128361456341429 ) ) ;
#15056 = CARTESIAN_POINT ( 'NONE',  ( 3.194014839594649491, 1.283080201803546538, 1.559715919771433867 ) ) ;
#15057 = CARTESIAN_POINT ( 'NONE',  ( -0.7500000000000006661, -0.3916666666666443475, -1.299038105676652011 ) ) ;
#15058 = CARTESIAN_POINT ( 'NONE',  ( 9.734391104931951588, 11.41950637958454706, 1.082531754730548412 ) ) ;
#15059 = CARTESIAN_POINT ( 'NONE',  ( 7.630541526392844887, 7.796719957080126662, 0.7998128361456341429 ) ) ;
#15060 = CARTESIAN_POINT ( 'NONE',  ( 3.379809591947144032, 1.306296513425331263, 1.594013207155994261 ) ) ;
#15061 = CARTESIAN_POINT ( 'NONE',  ( -0.4000000000000243916, 2.999999999999999112, 7.500000000000000000 ) ) ;
#15062 = CARTESIAN_POINT ( 'NONE',  ( 5.355634372598031767, 6.206993841907870291, -1.199719254218445830 ) ) ;
#15063 = CARTESIAN_POINT ( 'NONE',  ( 3.186732694495420848, 1.586669336078951664, -1.244385354607212335 ) ) ;
#15064 =( BOUNDED_CURVE ( )  B_SPLINE_CURVE ( 2, ( #189731, #155119, #6701, #87975, #72778, #203828, #57613, #56548, #106412 ),
 .UNSPECIFIED., .F., .T. ) 
 B_SPLINE_CURVE_WITH_KNOTS ( ( 3, 2, 2, 2, 3 ),
 ( 0.5208333333333333703, 0.5277777777777777901, 0.5416666666666666297, 0.5555555555555555802, 0.5625000000000000000 ),
 .UNSPECIFIED. ) 
 CURVE ( )  GEOMETRIC_REPRESENTATION_ITEM ( )  RATIONAL_B_SPLINE_CURVE ( ( 0.9330127018922192983, 0.9330127018922198534, 1.000000000000000000, 0.8660254037844387076, 1.000000000000000000, 0.8660254037844387076, 1.000000000000000000, 0.9330127018922194093, 0.9330127018922194093 ) ) 
 REPRESENTATION_ITEM ( '' )  );
#15065 = CARTESIAN_POINT ( 'NONE',  ( -0.1409997244346088141, 7.629137130509076492, -2.600278764091648487 ) ) ;
#15066 = CARTESIAN_POINT ( 'NONE',  ( 1.552429278155377679, -1.578373273985161473, -0.9476568548090894550 ) ) ;
#15067 = CARTESIAN_POINT ( 'NONE',  ( 6.428370569364434850, 1.274405893209800356, -1.801548588985131039 ) ) ;
#15068 = CARTESIAN_POINT ( 'NONE',  ( 6.821687566331318564, 7.987665577921906568, 1.199719254218452935 ) ) ;
#15069 = CARTESIAN_POINT ( 'NONE',  ( 2.302237272444170202, -2.161155982280529297, 0.05054500047013688047 ) ) ;
#15070 = CARTESIAN_POINT ( 'NONE',  ( -3.958617665510283601, 4.681104033592509595, -1.082531754730549967 ) ) ;
#15071 = CARTESIAN_POINT ( 'NONE',  ( 1.956267901341804283, -1.236798062192035363, 1.592663274815858676 ) ) ;
#15072 = CARTESIAN_POINT ( 'NONE',  ( 2.460726772196987433, 1.776095029035225537, 1.458756201258274210 ) ) ;
#15073 = EDGE_CURVE ( 'NONE', #23490, #200201, #150501, .T. ) ;
#15074 = CARTESIAN_POINT ( 'NONE',  ( 3.642287698956710340, 3.120124397464730581, -2.499999999999995115 ) ) ;
#15075 = VECTOR ( 'NONE', #63072, 1000.000000000000227 ) ;
#15076 = CARTESIAN_POINT ( 'NONE',  ( -0.3986307598441150568, 6.926362299646860343, 3.868483066195463227 ) ) ;
#15077 = AXIS2_PLACEMENT_3D ( 'NONE', #208116, #207052, #92286 ) ;
#15078 = CARTESIAN_POINT ( 'NONE',  ( 4.047701786889636111, 0.6652045265579300537, -1.855968581334372702 ) ) ;
#15079 = CARTESIAN_POINT ( 'NONE',  ( 4.610564714392807240, 1.931124171932835809, 0.5807562064495259690 ) ) ;
#15081 = CARTESIAN_POINT ( 'NONE',  ( 9.531018800282598846, 12.14260790512831889, 1.443375672974076540 ) ) ;
#15080 = CARTESIAN_POINT ( 'NONE',  ( 1.364683531249990311, 3.884375000341417028, 1.214306433183764966E-14 ) ) ;
#15083 = CARTESIAN_POINT ( 'NONE',  ( 6.375619162920919791, 2.015872221316476143, -0.6097100970045774559 ) ) ;
#15082 = CARTESIAN_POINT ( 'NONE',  ( -7.549192604710863286, 7.701812881784464437, -0.7998128361456291469 ) ) ;
#15084 = AXIS2_PLACEMENT_3D ( 'NONE', #132118, #99580, #165644 ) ;
#15085 = CARTESIAN_POINT ( 'NONE',  ( 6.215297738502283842, -1.773692237561547147, -1.067698627785176768 ) ) ;
#15086 = CARTESIAN_POINT ( 'NONE',  ( 6.063521013809720195, 8.097193820909906137, 1.599625672291281386 ) ) ;
#15087 = CARTESIAN_POINT ( 'NONE',  ( -5.364222332501225488, 9.410009821226765325, 0.7998128361456481317 ) ) ;
#15088 = CARTESIAN_POINT ( 'NONE',  ( -1.445103857048130047, 8.688264192037886247, 2.625611233228264840 ) ) ;
#15089 = CARTESIAN_POINT ( 'NONE',  ( 5.853772736177474734, -1.465772220379698343, -1.389892856972896329 ) ) ;
#15090 = CARTESIAN_POINT ( 'NONE',  ( -1.500000000000001332, -0.06874999931718445145, 0.000000000000000000 ) ) ;
#15091 = CARTESIAN_POINT ( 'NONE',  ( 4.213705752388523962, -0.3967513169967327724, 2.273188601971836142 ) ) ;
#15092 = ADVANCED_FACE ( 'NONE', ( #118050 ), #117385, .T. ) ;
#15093 = CARTESIAN_POINT ( 'NONE',  ( 2.026308614600486280, 1.056755808076353276, 1.771133502622779243 ) ) ;
#15094 = CARTESIAN_POINT ( 'NONE',  ( 6.629573927402440781, 10.67832731537079383, 1.040834085586084257E-14 ) ) ;
#15096 = CARTESIAN_POINT ( 'NONE',  ( 6.042093733545556233, 7.078139439671806699, -1.199719254218452047 ) ) ;
#15095 = CONICAL_SURFACE ( 'NONE', #136187, 6.540947088288920241, 0.7853981633974536081 ) ;
#15097 = CARTESIAN_POINT ( 'NONE',  ( 3.888156192069020634, 7.758209000714329839, 1.040834085586084257E-14 ) ) ;
#15098 = CARTESIAN_POINT ( 'NONE',  ( 1.364683531249986537, 1.217708333674754950, -0.7879004041258239610 ) ) ;
#15099 = CARTESIAN_POINT ( 'NONE',  ( 3.230585741806197841, 6.991043475407723307, 0.7998128361456271485 ) ) ;
#15100 = B_SPLINE_CURVE_WITH_KNOTS ( 'NONE', 3,
 ( #90352, #142331, #75166, #43753, #207284, #24249, #26399, #191024, #42691, #174823, #6927 ),
 .UNSPECIFIED., .F., .F.,
 ( 4, 1, 1, 1, 1, 1, 1, 1, 4 ),
 ( 0.000000000000000000, 0.2254101072112788262, 0.3970395454107691902, 0.5239558410346354389, 0.6152342776129972046, 0.6800502191696807808, 0.7279184599320936977, 0.7685697607527866015, 1.000000000000000000 ),
 .UNSPECIFIED. ) ;
#15101 = CARTESIAN_POINT ( 'NONE',  ( 5.775410249297131315, 9.681803024247919609, 1.040834085586084257E-14 ) ) ;
#15103 = DIRECTION ( 'NONE',  ( 0.000000000000000000, -1.000000000000000000, 0.000000000000000000 ) ) ;
#15102 = CARTESIAN_POINT ( 'NONE',  ( 4.000555764329702946, 2.160365084594504381, 0.2165898760093481201 ) ) ;
#15105 = CARTESIAN_POINT ( 'NONE',  ( 2.911469271472226339, -0.9098125248445630975, -1.600700954789348263 ) ) ;
#15104 = CARTESIAN_POINT ( 'NONE',  ( -4.961921032921567054, 4.891255414604337659, 0.7216878364870317197 ) ) ;
#15106 = CARTESIAN_POINT ( 'NONE',  ( 1.364683531249988535, 4.405208333674754506, -0.7879004041258300672 ) ) ;
#15107 = CARTESIAN_POINT ( 'NONE',  ( 5.759372899636661991, 2.159370146098410714, -0.3733810082120898044 ) ) ;
#15108 = CARTESIAN_POINT ( 'NONE',  ( 8.727830756187987760, 13.53690963525370883, 8.169218635041765708 ) ) ;
#15109 = CARTESIAN_POINT ( 'NONE',  ( 5.893528310750998145, 1.708867279757080748, 1.482922863094847443 ) ) ;
#15110 = CARTESIAN_POINT ( 'NONE',  ( -5.657660137730037953, 6.307591819868396676, -1.155748867827746995 ) ) ;
#15111 = CARTESIAN_POINT ( 'NONE',  ( 4.966250736084032447, 8.070317005903060448, 1.090833899539983554 ) ) ;
#15112 = CARTESIAN_POINT ( 'NONE',  ( -6.089020385868876062, 6.276481003034692030, -0.7216878364870338292 ) ) ;
#15113 = CYLINDRICAL_SURFACE ( 'NONE', #45898, 1.500000000000000222 ) ;
#15114 = CARTESIAN_POINT ( 'NONE',  ( 6.186734212497608354, -0.2616995340462315300, -1.750118319643848119 ) ) ;
#15115 = CARTESIAN_POINT ( 'NONE',  ( 4.635406539864527886, -0.09663638271006223801, 2.010879464324326626 ) ) ;
#15116 = CARTESIAN_POINT ( 'NONE',  ( 7.156006149914539982, 7.243095351188763686, 1.040834085586084257E-14 ) ) ;
#15117 = CARTESIAN_POINT ( 'NONE',  ( 3.100711275163593239, -0.6099987009138232441, -2.015686496682663087 ) ) ;
#15118 = CARTESIAN_POINT ( 'NONE',  ( 2.091283074759576532, -0.4175699524238601357, 1.869371669076219211 ) ) ;
#15120 = EDGE_CURVE ( 'NONE', #23582, #57442, #17256, .T. ) ;
#15119 = CARTESIAN_POINT ( 'NONE',  ( 4.684505768721569652, 5.424010470718658716, -1.199719254218452047 ) ) ;
#15121 = CARTESIAN_POINT ( 'NONE',  ( 2.699605434738296506, -1.457443026130700758, -1.324932107022150918 ) ) ;
#15122 = CARTESIAN_POINT ( 'NONE',  ( 1.358040219746913024, 0.7549631825471068147, 1.711723683848711985 ) ) ;
#15123 = CARTESIAN_POINT ( 'NONE',  ( 1.047228354049560828, 1.731870006261830630, -0.9216698261682305660 ) ) ;
#15126 = ORIENTED_EDGE ( 'NONE', *, *, #166817, .F. ) ;
#15125 = CARTESIAN_POINT ( 'NONE',  ( -0.07025823700084612988, -1.875094440630159065, 0.3749275819610526916 ) ) ;
#15124 = CARTESIAN_POINT ( 'NONE',  ( 3.738627921261325149, 0.2550716744767547728, 1.705777993037333129 ) ) ;
#15128 = CARTESIAN_POINT ( 'NONE',  ( 4.365362273920238678, 7.076377838673507448, 1.082531754730558626 ) ) ;
#15127 = CARTESIAN_POINT ( 'NONE',  ( 0.8739773845415178544, 2.125910683164092152, -0.5920798734769525673 ) ) ;
#15129 = CARTESIAN_POINT ( 'NONE',  ( 1.364683531249988757, 0.6968750003414209138, 0.000000000000000000 ) ) ;
#15130 = CARTESIAN_POINT ( 'NONE',  ( 11.89839339040395139, 11.32877468403908772, 1.560885614203548100 ) ) ;
#15131 = CARTESIAN_POINT ( 'NONE',  ( -8.743186976631616147, 3.870433085555829766, -7.668514896535084446 ) ) ;
#15132 = CARTESIAN_POINT ( 'NONE',  ( -4.327420530893566486, 8.660440186815751673, 0.7750000000000001332 ) ) ;
#15133 = CARTESIAN_POINT ( 'NONE',  ( 6.754741982670550371, -0.5462536098296209008, -1.996853278248729824 ) ) ;
#15134 = CARTESIAN_POINT ( 'NONE',  ( 0.7485892145711986467, -2.054541080789675789, -0.2550698046258002005 ) ) ;
#15135 = CARTESIAN_POINT ( 'NONE',  ( 1.499999999999987121, 1.295833333333353377, -0.8660254037844253849 ) ) ;
#15136 = CARTESIAN_POINT ( 'NONE',  ( 5.289652487626049115, 9.323011668872403845, 0.7998128361456462443 ) ) ;
#15137 = CARTESIAN_POINT ( 'NONE',  ( -8.311311860377216476, 9.655284244316948872, -1.199719254218446718 ) ) ;
#15138 = CARTESIAN_POINT ( 'NONE',  ( 5.879395890181562834, 6.888325289080478697, -1.199719254218452047 ) ) ;
#15140 = EDGE_CURVE ( 'NONE', #62825, #21505, #10015, .T. ) ;
#15139 = CARTESIAN_POINT ( 'NONE',  ( 5.320985837513584116, 1.605487267134264595, -1.385306402853322405 ) ) ;
#15141 = B_SPLINE_CURVE_WITH_KNOTS ( 'NONE', 3,
 ( #55799, #155437, #104566, #204144, #173851, #108894, #191119, #124100, #43850, #93666, #26497, #172770 ),
 .UNSPECIFIED., .F., .F.,
 ( 4, 2, 2, 2, 2, 4 ),
 ( 2.082684362675771891E-18, 0.0006884729345724524986, 0.001376945869144903046, 0.002065418803717353376, 0.002409655271003578649, 0.002753891738289803923 ),
 .UNSPECIFIED. ) ;
#15142 = CARTESIAN_POINT ( 'NONE',  ( 3.627688620108284745, 6.389997935838436227, 1.199719254218452047 ) ) ;
#15143 = CARTESIAN_POINT ( 'NONE',  ( 1.364683531249988757, 1.134375000341421247, 0.000000000000000000 ) ) ;
#15144 = ADVANCED_FACE ( 'NONE', ( #114845 ), #134267, .T. ) ;
#15145 = CARTESIAN_POINT ( 'NONE',  ( -1.500000000000013101, 3.129166666666689967, -0.8660254037844313801 ) ) ;
#15147 = CARTESIAN_POINT ( 'NONE',  ( 4.955668840994886359, 5.740367388370866131, 1.199719254218462483 ) ) ;
#15146 = CARTESIAN_POINT ( 'NONE',  ( 6.478960399985357554, 1.830089090633261417, 0.7073212282268787066 ) ) ;
#15148 = CARTESIAN_POINT ( 'NONE',  ( 4.095077249698628741, 1.080899603560569799, -1.701687522498253946 ) ) ;
#15149 = CARTESIAN_POINT ( 'NONE',  ( 3.731564767512856040, 0.6402975007456043199, -1.805710188498848456 ) ) ;
#15150 = CARTESIAN_POINT ( 'NONE',  ( -1.878188943807104661, 3.299815425349231557, -0.4000000000000339395 ) ) ;
#15151 = CARTESIAN_POINT ( 'NONE',  ( 1.083813775577105565, -0.9808430935620198188, 1.959877696171570927 ) ) ;
#15152 = CARTESIAN_POINT ( 'NONE',  ( 0.1333692844072559003, 5.722267537706915874, -2.647605121726896105 ) ) ;
#15153 = CARTESIAN_POINT ( 'NONE',  ( 2.723731132150861711, -1.073666234122659713, -1.531540996774889640 ) ) ;
#15154 = CARTESIAN_POINT ( 'NONE',  ( 0.7499999999999885647, -0.4854166659838468623, 1.299038105676657340 ) ) ;
#15155 = CARTESIAN_POINT ( 'NONE',  ( -7.477485413136760073, 8.682486722536401302, -1.199719254218446718 ) ) ;
#15157 = CARTESIAN_POINT ( 'NONE',  ( 5.237957716521472129, 2.114759263080950635, -0.1049963987776857816 ) ) ;
#15156 = CARTESIAN_POINT ( 'NONE',  ( -3.470524135418294520, 6.992769224722559684, -0.7216878364870267237 ) ) ;
#15158 = CARTESIAN_POINT ( 'NONE',  ( -0.7807912181424305764, 13.24045051524828942, -1.280767376876722041 ) ) ;
#15160 = CARTESIAN_POINT ( 'NONE',  ( 4.000000000000012434, 6.499999999999999112, -0.7500000000000006661 ) ) ;
#15159 = CARTESIAN_POINT ( 'NONE',  ( 2.700817844316987237, 1.767710524334182853, 1.116111477495850934 ) ) ;
#15162 = ORIENTED_EDGE ( 'NONE', *, *, #105101, .F. ) ;
#15161 = CARTESIAN_POINT ( 'NONE',  ( 0.8676543833149966689, 0.8442763457921966808, 1.503926039954103677 ) ) ;
#15163 = CARTESIAN_POINT ( 'NONE',  ( 6.908042961362778733, 8.018137195466769285, 1.199719254218462483 ) ) ;
#15164 = FACE_OUTER_BOUND ( 'NONE', #178813, .T. ) ;
#15165 = CARTESIAN_POINT ( 'NONE',  ( 0.02890288085936086604, -9.971207159576023216, 9.579616049094571650 ) ) ;
#15166 = FACE_OUTER_BOUND ( 'NONE', #55996, .T. ) ;
#15168 = CARTESIAN_POINT ( 'NONE',  ( 7.415946836550703303, 11.59576237604377091, 0.7216878364870438212 ) ) ;
#15167 = CARTESIAN_POINT ( 'NONE',  ( 7.806797523370503811, 8.002351953554066810, 1.040834085586084257E-14 ) ) ;
#15169 = ORIENTED_EDGE ( 'NONE', *, *, #122354, .F. ) ;
#15171 = AXIS2_PLACEMENT_3D ( 'NONE', #14250, #80343, #32656 ) ;
#15170 = CARTESIAN_POINT ( 'NONE',  ( -0.4019237886467001974, 9.551335450315368902, 1.500000000000001998 ) ) ;
#15173 = CARTESIAN_POINT ( 'NONE',  ( 1.558926746901686089, -1.530267751544078347, 0.9690644009569903128 ) ) ;
#15172 = CARTESIAN_POINT ( 'NONE',  ( 4.355912491740495440, 8.303924683664389406, 0.000000000000000000 ) ) ;
#15174 = CARTESIAN_POINT ( 'NONE',  ( -8.016948904382338981, 8.247528564734524892, -0.7998128361456291469 ) ) ;
#15175 = CARTESIAN_POINT ( 'NONE',  ( 5.138703914779377158, 5.953908307786102583, 1.199719254218462483 ) ) ;
#15176 = CARTESIAN_POINT ( 'NONE',  ( 4.864343252252968597, 8.897093904262280972, 0.000000000000000000 ) ) ;
#15177 = CARTESIAN_POINT ( 'NONE',  ( 6.639320575229263888, 6.039109382135522175, 2.391643382086404923 ) ) ;
#15178 = CYLINDRICAL_SURFACE ( 'NONE', #111247, 0.3999999999999997446 ) ;
#15179 = CARTESIAN_POINT ( 'NONE',  ( 4.895304229855391043, 6.665267352516039523, 1.249363049274658799 ) ) ;
#15180 = CARTESIAN_POINT ( 'NONE',  ( 9.897088948295946764, 10.64895131587453569, 0.7216878364870438212 ) ) ;
#15181 = CARTESIAN_POINT ( 'NONE',  ( 2.804952713220637328, -1.548975583508698683, 1.031263495014663523 ) ) ;
#15182 = CARTESIAN_POINT ( 'NONE',  ( 0.4037314067151754893, -1.025472807287574506, -1.617813098647686632 ) ) ;
#15183 = CARTESIAN_POINT ( 'NONE',  ( 6.510771785681003010, 1.426997308145862453, -1.294280627073117529 ) ) ;
#15184 = DIRECTION ( 'NONE',  ( -0.000000000000000000, 1.000000000000000000, -0.000000000000000000 ) ) ;
#15185 = CARTESIAN_POINT ( 'NONE',  ( 4.879410147971469769, 4.944948943068641967, -0.7687999843507594688 ) ) ;
#15186 = CARTESIAN_POINT ( 'NONE',  ( 4.720979226589129496, 8.219560628541461966, -0.6735110442024627719 ) ) ;
#15187 = DIRECTION ( 'NONE',  ( 0.000000000000000000, 1.000000000000000000, 0.000000000000000000 ) ) ;
#15188 = CARTESIAN_POINT ( 'NONE',  ( -2.480778921620681921, 5.838066475291996404, 1.040834085586084257E-14 ) ) ;
#15189 = CARTESIAN_POINT ( 'NONE',  ( 8.270110514656026979, 10.67154823856396817, 1.443375672974076540 ) ) ;
#15190 = CARTESIAN_POINT ( 'NONE',  ( 5.014487319174643964, 0.7500019944287477092, 1.821250405324719823 ) ) ;
#15191 = CARTESIAN_POINT ( 'NONE',  ( 1.981254353800803836, -1.939921095825656305, -0.8566514584813912370 ) ) ;
#15192 = CARTESIAN_POINT ( 'NONE',  ( -4.530395885260773525, 8.437212299446219532, 0.7998128361456481317 ) ) ;
#15193 = FACE_OUTER_BOUND ( 'NONE', #134382, .T. ) ;
#15194 = CARTESIAN_POINT ( 'NONE',  ( 5.072158865288234786, 7.010880990960011161, 1.443375672974065660 ) ) ;
#15195 = CARTESIAN_POINT ( 'NONE',  ( 5.982419568921026887, -0.3181065885738461607, -2.168126298386578110 ) ) ;
#15196 = DIRECTION ( 'NONE',  ( 0.000000000000000000, 0.000000000000000000, 1.000000000000000000 ) ) ;
#15197 = CARTESIAN_POINT ( 'NONE',  ( 4.207974007929848881, -1.921269893987355593, 0.1410920886178046452 ) ) ;
#15198 = CARTESIAN_POINT ( 'NONE',  ( -5.357443255694392725, 9.402100898285455699, 0.000000000000000000 ) ) ;
#15199 = CARTESIAN_POINT ( 'NONE',  ( 0.4459769555512117511, 1.820297760642339391, 0.1397589855641478973 ) ) ;
#15200 = CARTESIAN_POINT ( 'NONE',  ( 1.524350002934187653, -1.228176919886795559, -1.833354347511229498 ) ) ;
#15201 = CARTESIAN_POINT ( 'NONE',  ( -6.019103170659795943, 7.082126295680237327, 1.053690733614056851 ) ) ;
#15202 = DIRECTION ( 'NONE',  ( 0.000000000000000000, 0.7071067811865445751, 0.7071067811865504593 ) ) ;
#15203 = VERTEX_POINT ( 'NONE', #181893 ) ;
#15204 = CARTESIAN_POINT ( 'NONE',  ( 3.445180431648323882, 6.073108699348104267, 1.082531754730549078 ) ) ;
#15205 = ORIENTED_EDGE ( 'NONE', *, *, #188735, .F. ) ;
#15206 = CARTESIAN_POINT ( 'NONE',  ( 6.455907338579963017, -0.6669464233056993097, 1.853184144328771543 ) ) ;
#15207 = CARTESIAN_POINT ( 'NONE',  ( 1.048265877425518688, -1.530107816300673829, 1.195853197770081255 ) ) ;
#15208 = CARTESIAN_POINT ( 'NONE',  ( 6.837282040791485827, -1.423258038995322661, 1.805902563099166080 ) ) ;
#15210 = CARTESIAN_POINT ( 'NONE',  ( 5.225394145299861570, 0.1845887361094991075, -1.851793659149820082 ) ) ;
#15209 = CARTESIAN_POINT ( 'NONE',  ( -7.767895665986912057, 8.027242796598338614, -0.7998128361456362523 ) ) ;
#15211 = CARTESIAN_POINT ( 'NONE',  ( 5.306037014901791693, 7.283738832175834510, 1.599625672291269396 ) ) ;
#15212 = FACE_OUTER_BOUND ( 'NONE', #194035, .T. ) ;
#15213 = CARTESIAN_POINT ( 'NONE',  ( 3.753485299433081845, 7.393166926064984601, -0.1880404715405732952 ) ) ;
#15214 = CARTESIAN_POINT ( 'NONE',  ( -6.124532705071231931, 8.168374127381657246, -1.599625672291263179 ) ) ;
#15215 = ADVANCED_FACE ( 'NONE', ( #64952 ), #133201, .F. ) ;
#15216 = CARTESIAN_POINT ( 'NONE',  ( -6.237633190739009237, 9.434933268240943249, 1.199719254218452047 ) ) ;
#15217 = CARTESIAN_POINT ( 'NONE',  ( 1.066276686178056377, -1.386418637449363889, 1.697306931840412370 ) ) ;
#15218 = CARTESIAN_POINT ( 'NONE',  ( 5.205967797967541166, 5.175976640491323444, -0.7216878364870197293 ) ) ;
#15219 = CARTESIAN_POINT ( 'NONE',  ( 0.3999999999999977462, 3.963633530850342090, -0.9046180958551371942 ) ) ;
#15220 =( NAMED_UNIT ( * ) PLANE_ANGLE_UNIT ( ) SI_UNIT ( $, .RADIAN. ) );
#15221 = CARTESIAN_POINT ( 'NONE',  ( 2.174178736149934732, -1.123764393468742684, 1.438770255985911684 ) ) ;
#15222 = CARTESIAN_POINT ( 'NONE',  ( -2.839543107058306592, 5.400218493954923815, -1.199719254218446718 ) ) ;
#15223 = CARTESIAN_POINT ( 'NONE',  ( -0.1966775781082229224, 3.362145428329805341, -1.992912547350113028 ) ) ;
#15224 = CARTESIAN_POINT ( 'NONE',  ( 6.509000000000011887, 2.430396405248925529, 2.482145556523357222 ) ) ;
#15225 = CARTESIAN_POINT ( 'NONE',  ( 8.041957671200231417, 12.53403438304231976, 1.040834085586084257E-14 ) ) ;
#15226 = CARTESIAN_POINT ( 'NONE',  ( -0.02299388927988389730, 0.001624902753813092359, -1.910968047046639251 ) ) ;
#15227 = CARTESIAN_POINT ( 'NONE',  ( 4.909014596843685574, -1.577992517845404619, 1.165349624694256736 ) ) ;
#15228 = CARTESIAN_POINT ( 'NONE',  ( -9.040589502214116280, 9.441775928871617651, 0.7998128361456462443 ) ) ;
#15229 = CARTESIAN_POINT ( 'NONE',  ( 4.937140493670735708, 8.911747675924535983, -0.7998128361456281477 ) ) ;
#15230 = CARTESIAN_POINT ( 'NONE',  ( 3.667680160636753506, 1.218766932906123479, 1.821211977396507198 ) ) ;
#15231 = EDGE_CURVE ( 'NONE', #114534, #73830, #30756, .T. ) ;
#15232 = CIRCLE ( 'NONE', #101678, 6.277139874739035008 ) ;
#15233 = CARTESIAN_POINT ( 'NONE',  ( 4.578903193113299963, 6.365139696764064325, 1.599625672291267175 ) ) ;
#15234 = CARTESIAN_POINT ( 'NONE',  ( 3.344645782512998267, -2.038826501179476391, -0.3585456059004287765 ) ) ;
#15236 = CARTESIAN_POINT ( 'NONE',  ( 0.6823417656249882723, 1.238541667008083547, -1.181850606188749264 ) ) ;
#15235 = CARTESIAN_POINT ( 'NONE',  ( 2.723338755101574638, 3.009222805659324429, 2.500000000000000444 ) ) ;
#15237 = ORIENTED_EDGE ( 'NONE', *, *, #11046, .F. ) ;
#15238 = CARTESIAN_POINT ( 'NONE',  ( 4.219567396149206395, 2.254377101126247229, 0.4485144814023647730 ) ) ;
#15239 = CARTESIAN_POINT ( 'NONE',  ( 7.239690840017413365, 10.42976116578691403, -1.082531754730537976 ) ) ;
#15241 = CARTESIAN_POINT ( 'NONE',  ( -3.285556943750000070, -0.1093749995220438809, 0.000000000000000000 ) ) ;
#15240 = CARTESIAN_POINT ( 'NONE',  ( 5.234856708652215751, 9.121433570154021453, 0.7216878364870317197 ) ) ;
#15242 = CARTESIAN_POINT ( 'NONE',  ( 6.620655732516684822, 7.053712996964945248, 2.324417015927725760 ) ) ;
#15243 = CARTESIAN_POINT ( 'NONE',  ( -10.29842937900060207, 4.863661338910580945, -6.166703023499271019 ) ) ;
#15244 = CARTESIAN_POINT ( 'NONE',  ( 3.415898659897542267, 1.231191954956109447, -1.501781470047100386 ) ) ;
#15245 = ORIENTED_EDGE ( 'NONE', *, *, #135027, .T. ) ;
#15246 = CARTESIAN_POINT ( 'NONE',  ( 8.717529583462633624, 13.11427558077437894, 0.7216878364870438212 ) ) ;
#15247 = EDGE_CURVE ( 'NONE', #28244, #23747, #137843, .T. ) ;
#15248 = CARTESIAN_POINT ( 'NONE',  ( 3.621269620730773298, 1.642686141288721480, 0.9789267784374030557 ) ) ;
#15249 = CARTESIAN_POINT ( 'NONE',  ( 4.800089777832203808, 5.120415418395356077, -0.7784788408505428636 ) ) ;
#15250 = CARTESIAN_POINT ( 'NONE',  ( 5.737229663476812291, -1.557457729854847983, 0.7413209835094927147 ) ) ;
#15251 = CARTESIAN_POINT ( 'NONE',  ( 4.716029918043215474, 1.032482702726954527, -1.731993998903176957 ) ) ;
#15252 =( BOUNDED_CURVE ( )  B_SPLINE_CURVE ( 2, ( #55862, #74258, #107888, #41776, #125217 ),
 .UNSPECIFIED., .F., .T. ) 
 B_SPLINE_CURVE_WITH_KNOTS ( ( 3, 2, 3 ),
 ( 0.04938056888445840203, 0.05000000000000000278, 0.05032235610909231716 ),
 .UNSPECIFIED. ) 
 CURVE ( )  GEOMETRIC_REPRESENTATION_ITEM ( )  RATIONAL_B_SPLINE_CURVE ( ( 0.9815633466012652075, 0.9900414359694351685, 1.000000000000000000, 0.9948174964536085074, 0.9900359397100743086 ) ) 
 REPRESENTATION_ITEM ( '' )  );
#15253 = CARTESIAN_POINT ( 'NONE',  ( 4.782019082252658926, 1.911913310736196081, -1.275919496871528169 ) ) ;
#15254 = CARTESIAN_POINT ( 'NONE',  ( 0.7860941533469123499, 1.484900681275106438, 1.632775826992872492 ) ) ;
#15256 = CARTESIAN_POINT ( 'NONE',  ( -4.502716413514301408, 7.306900678191715848, -1.082531754730549967 ) ) ;
#15255 = CARTESIAN_POINT ( 'NONE',  ( -3.854349547643701968, 7.486297264622638004, -0.2033521147656738026 ) ) ;
#15257 = CARTESIAN_POINT ( 'NONE',  ( 6.116413106003639300, 1.187136285548880066, -1.312641305385914947 ) ) ;
#15259 = CARTESIAN_POINT ( 'NONE',  ( 1.430038810223871026, 1.126473215625309887, -1.996311628086711254 ) ) ;
#15258 = CARTESIAN_POINT ( 'NONE',  ( 4.389807875774629942, 8.343469298370917997, 0.7998128361456271485 ) ) ;
#15260 = CARTESIAN_POINT ( 'NONE',  ( 1.183123967286016986, -0.7853004192260810701, 1.553138493749019133 ) ) ;
#15261 = CARTESIAN_POINT ( 'NONE',  ( 11.88172094500853504, 11.37999994398405867, -1.685553348215862446 ) ) ;
#15262 = CARTESIAN_POINT ( 'NONE',  ( 1.510678448032206189, 1.731588368038105896, 0.09119125932234918575 ) ) ;
#15263 = CARTESIAN_POINT ( 'NONE',  ( -1.360316468750038643, 0.4427083336747321130, 0.7853790794158701516 ) ) ;
#15264 = CARTESIAN_POINT ( 'NONE',  ( -11.94980361723156470, 13.50238056585419777, -1.099999926404080064 ) ) ;
#15265 = CARTESIAN_POINT ( 'NONE',  ( 0.8190779338598102033, -1.572544420714114821, 1.497277704674306431 ) ) ;
#15266 = CARTESIAN_POINT ( 'NONE',  ( 2.729704159269104924, 0.7212915320151757070, -1.883313052590728454 ) ) ;
#15267 = CARTESIAN_POINT ( 'NONE',  ( -0.7500000000000006661, 0.1395833340161536928, -1.299038105676652011 ) ) ;
#15268 = CARTESIAN_POINT ( 'NONE',  ( 5.391212663409540973, 1.697947877755761947, -0.9101574019480199729 ) ) ;
#15269 = CARTESIAN_POINT ( 'NONE',  ( 0.6823417656249969321, 12.52604166700806232, -1.181850606188757036 ) ) ;
#15270 = CARTESIAN_POINT ( 'NONE',  ( 2.514199509032362112, -0.6922678517280489441, 2.110887004458279481 ) ) ;
#15271 = ORIENTED_EDGE ( 'NONE', *, *, #181468, .F. ) ;
#15272 = CARTESIAN_POINT ( 'NONE',  ( -9.578353140444630043, -9.943513495888055331, 0.1579188828665830657 ) ) ;
#15273 = CARTESIAN_POINT ( 'NONE',  ( -1.402160292154681736E-14, -0.4124999999999747202, -1.732050807568870754 ) ) ;
#15274 = CARTESIAN_POINT ( 'NONE',  ( 9.890836756369282057, 11.49806328964105617, -1.199719254218440723 ) ) ;
#15275 = FACE_OUTER_BOUND ( 'NONE', #123458, .T. ) ;
#15276 = SURFACE_STYLE_USAGE ( .BOTH. , #48872 ) ;
#15277 = CARTESIAN_POINT ( 'NONE',  ( 5.390116981161272136, -0.4305884537129686662, -1.686203596905116342 ) ) ;
#15278 = CARTESIAN_POINT ( 'NONE',  ( 2.998438581075290266, 1.946722116546204306, 0.2428724957088539971 ) ) ;
#15280 = CARTESIAN_POINT ( 'NONE',  ( -5.721177635286839092, 9.618531641235897212, 0.7216878364870458196 ) ) ;
#15279 = CARTESIAN_POINT ( 'NONE',  ( 4.039439701867726384, 6.800097854565950506, 1.199719254218462483 ) ) ;
#15281 = EDGE_CURVE ( 'NONE', #14053, #135613, #88336, .T. ) ;
#15282 = CARTESIAN_POINT ( 'NONE',  ( -1.493145604987279107, 4.435543764411821854, 0.1636410324438698216 ) ) ;
#15283 = CARTESIAN_POINT ( 'NONE',  ( 4.675235532476687439, 0.006304645973906687281, -2.262578822721802219 ) ) ;
#15284 = CARTESIAN_POINT ( 'NONE',  ( 1.170463292146912915, -0.9257924050831314311, -1.843294045186917085 ) ) ;
#15285 = CARTESIAN_POINT ( 'NONE',  ( -6.287230548435221777, 8.358188277972981695, -1.599625672291263179 ) ) ;
#15286 = AXIS2_PLACEMENT_3D ( 'NONE', #179695, #180746, #164503 ) ;
#15287 = CARTESIAN_POINT ( 'NONE',  ( 2.553932558351139193, 0.6037834209405189556, -2.180390065951258283 ) ) ;
#15288 = VERTEX_POINT ( 'NONE', #35650 ) ;
#15289 = CARTESIAN_POINT ( 'NONE',  ( -1.500000000000015099, 0.6604166673494823447, -0.8660254037844313801 ) ) ;
#15290 = CARTESIAN_POINT ( 'NONE',  ( 3.092876253348992410, 1.606159189733218140, -0.9584765265276545820 ) ) ;
#15291 = CARTESIAN_POINT ( 'NONE',  ( 1.810757103121255707, 0.9981641815470091439, -1.417837687506792621 ) ) ;
#15292 = CARTESIAN_POINT ( 'NONE',  ( 5.267185993530860699, 2.112242253262315739, -0.5839428218426812034 ) ) ;
#15293 = CARTESIAN_POINT ( 'NONE',  ( 6.774459802350780713, -1.427793189328768753, 1.813748355473641549 ) ) ;
#15294 = CARTESIAN_POINT ( 'NONE',  ( 3.907220446582274853, 1.852832235905249370, 1.113321777468062823 ) ) ;
#15295 = CARTESIAN_POINT ( 'NONE',  ( 5.085854714555574141, -1.927481041573789744, -0.2360958376807794079 ) ) ;
#15296 = CARTESIAN_POINT ( 'NONE',  ( -3.592547517496941900, 5.214391408544949869, -1.443375672974051449 ) ) ;
#15297 = CARTESIAN_POINT ( 'NONE',  ( 6.854772330626868637, -1.445518619047950981, 1.186913843143226233 ) ) ;
#15298 = CARTESIAN_POINT ( 'NONE',  ( 0.6250000000000001110, -2.052068128417942283, 3.751950811937565850E-14 ) ) ;
#15299 = CARTESIAN_POINT ( 'NONE',  ( 0.9322618968498219694, 13.30364107006543861, 1.097267912408639967 ) ) ;
#15300 = CARTESIAN_POINT ( 'NONE',  ( 0.6801582343749987825, 2.723958333674732391, 1.178068619123836314 ) ) ;
#15301 = CARTESIAN_POINT ( 'NONE',  ( 6.152970239395502361, 1.038990588714868490, 1.728003889287746286 ) ) ;
#15302 = CARTESIAN_POINT ( 'NONE',  ( -2.941756144040970522, 5.415504020480993219, -1.082531754730543083 ) ) ;
#15303 = CARTESIAN_POINT ( 'NONE',  ( 6.272618624616828953, 10.46980549536166016, 1.040834085586084257E-14 ) ) ;
#15304 = CARTESIAN_POINT ( 'NONE',  ( 5.011674058906918638, 5.875983152593414971, 1.199719254218452047 ) ) ;
#15306 = CARTESIAN_POINT ( 'NONE',  ( 0.000000000000000000, 6.499999999999999112, 0.000000000000000000 ) ) ;
#15305 = CARTESIAN_POINT ( 'NONE',  ( 3.562960707638890501, -1.610701098693729350, -0.8595150645765645692 ) ) ;
#15307 = CARTESIAN_POINT ( 'NONE',  ( 10.95308175811721085, 11.29999999999999893, -1.800000000000001155 ) ) ;
#15308 = ORIENTED_EDGE ( 'NONE', *, *, #52716, .T. ) ;
#15309 = CARTESIAN_POINT ( 'NONE',  ( -5.031484404002922517, 6.963427452793760963, 1.443375672974058777 ) ) ;
#15310 = CARTESIAN_POINT ( 'NONE',  ( -3.285556943750000070, -4.046874999522040106, 0.000000000000000000 ) ) ;
#15311 = CARTESIAN_POINT ( 'NONE',  ( -7.700141177557535244, 11.07091624287075859, -1.199719254218446718 ) ) ;
#15312 = CARTESIAN_POINT ( 'NONE',  ( -0.07004771093476865051, -1.979950378243084730, 0.3982260095720979165 ) ) ;
#15313 = CARTESIAN_POINT ( 'NONE',  ( 1.559403367407938390, -1.789607135292633266, 1.137164086494051096 ) ) ;
#15314 = EDGE_CURVE ( 'NONE', #120691, #118760, #204537, .T. ) ;
#15315 = ORIENTED_EDGE ( 'NONE', *, *, #68075, .T. ) ;
#15316 = CARTESIAN_POINT ( 'NONE',  ( -4.599959256786493533, 8.588645909551377855, 0.000000000000000000 ) ) ;
#15317 = CARTESIAN_POINT ( 'NONE',  ( 4.273844736805816780, 6.009238164405336313, 1.599625672291267398 ) ) ;
#15318 = CARTESIAN_POINT ( 'NONE',  ( 6.332896556214961947, 0.1992470125839322093, 2.051223679500746133 ) ) ;
#15319 = CARTESIAN_POINT ( 'NONE',  ( 6.522112240665402183, -1.799906897009293738, 0.9091900463213120620 ) ) ;
#15320 = ORIENTED_EDGE ( 'NONE', *, *, #34340, .F. ) ;
#15321 = CARTESIAN_POINT ( 'NONE',  ( -9.459838494033043332, 12.05956421450382088, 1.599625672291281386 ) ) ;
#15322 = CARTESIAN_POINT ( 'NONE',  ( 5.996449078994045223, 10.21788403546024782, 0.7998128361456331437 ) ) ;
#15325 = VERTEX_POINT ( 'NONE', #148364 ) ;
#15324 = CARTESIAN_POINT ( 'NONE',  ( -3.147653791585727667, 8.920000000000001705, 2.499999999999999556 ) ) ;
#15323 = CARTESIAN_POINT ( 'NONE',  ( -4.945692173934974178, 8.992000979557944973, 0.000000000000000000 ) ) ;
#15326 = CARTESIAN_POINT ( 'NONE',  ( 6.059925523928845870, 7.140772946495586915, 1.155538509043469997 ) ) ;
#15327 = CARTESIAN_POINT ( 'NONE',  ( 5.554064478179312481, 1.779353385700060075, -0.9478964821433707444 ) ) ;
#15328 = CARTESIAN_POINT ( 'NONE',  ( 5.244037021109955177, 0.5378974813256987009, 1.760811445753920346 ) ) ;
#15329 = CARTESIAN_POINT ( 'NONE',  ( 10.10286202908859110, -8.578580700073974441, -0.6127037010540555828 ) ) ;
#15330 = CARTESIAN_POINT ( 'NONE',  ( 3.018547437338540806, -1.137872740210974287, -2.007595131770247843 ) ) ;
#15331 = CARTESIAN_POINT ( 'NONE',  ( 5.879395890181562834, 6.888325289080478697, -1.199719254218452047 ) ) ;
#15332 = EDGE_CURVE ( 'NONE', #115124, #19069, #28868, .T. ) ;
#15333 = CARTESIAN_POINT ( 'NONE',  ( 5.923154835166896781, -0.05960684409221649049, 2.160954015416292506 ) ) ;
#15334 = CARTESIAN_POINT ( 'NONE',  ( 6.934105498385400246, 10.17720795050327354, -1.199719254218441611 ) ) ;
#15335 = CARTESIAN_POINT ( 'NONE',  ( 0.9427985035241670531, -1.531986193156938292, -1.193500027965375354 ) ) ;
#15336 = CARTESIAN_POINT ( 'NONE',  ( -4.111146893441842920, 5.819424013814012753, 1.599625672291267398 ) ) ;
#15337 = EDGE_LOOP ( 'NONE', ( #6526, #108769, #61261, #64234 ) ) ;
#15338 = CARTESIAN_POINT ( 'NONE',  ( 5.062018989497997445, 1.914771916633486448, -1.271085502950035417 ) ) ;
#15339 = DIRECTION ( 'NONE',  ( 0.000000000000000000, -0.5005768354468319581, 0.8656921114426510133 ) ) ;
#15340 = CARTESIAN_POINT ( 'NONE',  ( -3.871735385154307263, 6.674719161725423788, -1.199719254218450271 ) ) ;
#15341 = CARTESIAN_POINT ( 'NONE',  ( 3.362029495745801899, 0.8400119854848131506, 1.671504782411597612 ) ) ;
#15344 = CARTESIAN_POINT ( 'NONE',  ( -6.611536185319534908, 7.742488966741438716, 1.199719254218452047 ) ) ;
#15343 = CARTESIAN_POINT ( 'NONE',  ( -1.402160292154681736E-14, -0.3812499993171785673, -1.732050807568870754 ) ) ;
#15342 = CARTESIAN_POINT ( 'NONE',  ( 1.582132296805271787, 0.9858968508435607125, 1.638552900098678045 ) ) ;
#15345 = CARTESIAN_POINT ( 'NONE',  ( 2.842613246588860942, 2.190307313262893185, 0.2694104812042824038 ) ) ;
#15346 = CARTESIAN_POINT ( 'NONE',  ( 6.983263157960361234, 3.701227967198342128, 2.360532479264612071 ) ) ;
#15347 = CARTESIAN_POINT ( 'NONE',  ( 3.297657676621871925, 4.870353260857385180, 1.599625672291267398 ) ) ;
#15348 = CARTESIAN_POINT ( 'NONE',  ( 6.333067150914816423, 7.521571443223021625, 1.082531754730549967 ) ) ;
#15349 = CARTESIAN_POINT ( 'NONE',  ( -3.110706179331648169, 5.716575411607132118, 1.199719254218462483 ) ) ;
#15350 = CARTESIAN_POINT ( 'NONE',  ( -7.065207446052809814, 9.336104335185325453, -1.443375672974066548 ) ) ;
#15351 = CARTESIAN_POINT ( 'NONE',  ( 1.071480742727632940, 1.901078573484305201, -0.5215319001752088957 ) ) ;
#15352 = CARTESIAN_POINT ( 'NONE',  ( 1.079649059555651824, -0.05968906897618533880, -2.306965765669062751 ) ) ;
#15354 = EDGE_CURVE ( 'NONE', #90575, #167635, #47094, .T. ) ;
#15353 = CARTESIAN_POINT ( 'NONE',  ( 1.908577322519442454, 0.6123880975643315461, 1.863924812142327525 ) ) ;
#15355 = CARTESIAN_POINT ( 'NONE',  ( 4.909062464502076395, -1.659793021533024548, 1.224303311577365161 ) ) ;
#15356 = CARTESIAN_POINT ( 'NONE',  ( 4.690757960648224589, 6.495636925554817864, 1.443375672974062551 ) ) ;
#15357 = CARTESIAN_POINT ( 'NONE',  ( 4.420840606507738357, 7.315341919971147355, 1.199719254218451159 ) ) ;
#15358 = ORIENTED_EDGE ( 'NONE', *, *, #50859, .F. ) ;
#15359 = CARTESIAN_POINT ( 'NONE',  ( -0.6823417656249969321, 5.780208333674756283, -1.181850606188749264 ) ) ;
#15360 = CARTESIAN_POINT ( 'NONE',  ( 1.394453263437886604E-15, -1.312499999999999556, 3.474999999999999645 ) ) ;
#15361 = CARTESIAN_POINT ( 'NONE',  ( 4.487385655998885170, 5.298000022495898520, 1.082531754730560403 ) ) ;
#15362 = CARTESIAN_POINT ( 'NONE',  ( 0.7608744453060071189, -0.7297706024342350828, -2.044895412143563185 ) ) ;
#15364 = CARTESIAN_POINT ( 'NONE',  ( 6.058133912487986272, -1.297239342979487509, 1.306937132449899508 ) ) ;
#15363 = CARTESIAN_POINT ( 'NONE',  ( -11.86145016429273191, 13.50587876334730453, 1.099999999999996758 ) ) ;
#15365 = CARTESIAN_POINT ( 'NONE',  ( 10.98241130803287646, 3.975933801733736672, -3.568401746111017570 ) ) ;
#15366 = CARTESIAN_POINT ( 'NONE',  ( -7.869907033622098425, -7.024005807131032064, 7.214015686748106226 ) ) ;
#15367 = CARTESIAN_POINT ( 'NONE',  ( 0.8427765623921362748, -1.607460297381148928, 0.9563107477488577146 ) ) ;
#15368 = CARTESIAN_POINT ( 'NONE',  ( 5.958325562381369345, 0.8699925256120243366, 1.978967057501494820 ) ) ;
#15369 = CARTESIAN_POINT ( 'NONE',  ( -5.656850995454980158, 6.308143005704411443, 1.156498089891801140 ) ) ;
#15370 = CARTESIAN_POINT ( 'NONE',  ( 0.07755575628183573877, 5.720052600789671260, -2.782970829007725744 ) ) ;
#15371 = CARTESIAN_POINT ( 'NONE',  ( 0.6823417656249882723, -1.157291666325249713, 1.181850606188755259 ) ) ;
#15372 = CARTESIAN_POINT ( 'NONE',  ( 2.561071438676546741, -1.588783617390630898, 1.063917234122884858 ) ) ;
#15373 = CARTESIAN_POINT ( 'NONE',  ( 2.553260254243350680, 0.4745879851475919842, -1.704939281604215706 ) ) ;
#15374 = CARTESIAN_POINT ( 'NONE',  ( 0.3988866192712777758, -0.2342882197893907670, -1.897819253221716851 ) ) ;
#15376 = CARTESIAN_POINT ( 'NONE',  ( 5.923430108280006934, -1.391030039757386039, -1.317302766908773126 ) ) ;
#15375 = CARTESIAN_POINT ( 'NONE',  ( 3.166866847460915846, -3.204376093797748126, 0.9919409734452371286 ) ) ;
#15377 = CARTESIAN_POINT ( 'NONE',  ( 6.285607346219458158, -1.855037422363578381, 0.6622139934589140742 ) ) ;
#15378 = CARTESIAN_POINT ( 'NONE',  ( 1.499999999999987121, 4.295833333333352044, -0.8660254037844323793 ) ) ;
#15379 = CARTESIAN_POINT ( 'NONE',  ( 1.160570123509139906, 2.118417766304943495, 0.09849428607798524360 ) ) ;
#15380 = PRESENTATION_STYLE_ASSIGNMENT (( #127113 ) ) ;
#15381 = CARTESIAN_POINT ( 'NONE',  ( 5.489076674590072535, 1.649195787720953987, -0.8828566466120502110 ) ) ;
#15383 = VERTEX_POINT ( 'NONE', #32468 ) ;
#15382 = CARTESIAN_POINT ( 'NONE',  ( 0.6975366375942676500, -0.6598540886826111951, 1.702458561391326342 ) ) ;
#15385 = CARTESIAN_POINT ( 'NONE',  ( 4.713861384769566953, 8.227931952640012980, -0.6562286284988675389 ) ) ;
#15384 = CARTESIAN_POINT ( 'NONE',  ( 4.864015066594513215, 2.183220759563545776, -0.3215228633955333759 ) ) ;
#15386 = CARTESIAN_POINT ( 'NONE',  ( -1.364683531250012516, 4.051041667008088432, -0.7879004041258300672 ) ) ;
#15387 = CARTESIAN_POINT ( 'NONE',  ( 2.295447401932719345, -1.843475527790199964, 0.9254330757148797604 ) ) ;
#15388 = CARTESIAN_POINT ( 'NONE',  ( 4.950698647284403009, 8.927565521807144577, 1.040834085586084257E-14 ) ) ;
#15390 = CARTESIAN_POINT ( 'NONE',  ( -6.991200766141138168, 11.30815132714001159, 0.7998128361456481317 ) ) ;
#15389 = AXIS2_PLACEMENT_3D ( 'NONE', #125071, #142336, #110930 ) ;
#15391 = DIRECTION ( 'NONE',  ( 0.000000000000000000, -1.000000000000000000, 0.000000000000000000 ) ) ;
#15392 = CARTESIAN_POINT ( 'NONE',  ( 10.40318394038753702, 11.03146944007395724, -0.7998128361456281477 ) ) ;
#15393 = CARTESIAN_POINT ( 'NONE',  ( -3.421712537580930302, -0.02252155983199216616, -0.4161442326466053832 ) ) ;
#15394 = CARTESIAN_POINT ( 'NONE',  ( 0.1753634416057740786, 1.334841368177059895, -2.397339160348281428 ) ) ;
#15395 = EDGE_LOOP ( 'NONE', ( #146551, #25720, #164995, #147572 ) ) ;
#15396 = CARTESIAN_POINT ( 'NONE',  ( 4.580570967453869713, 1.276285970795057345, -1.630082184409971324 ) ) ;
#15398 = CARTESIAN_POINT ( 'NONE',  ( -1.499999999999997780, 5.650000000000023448, 1.214306433183764966E-14 ) ) ;
#15397 = CIRCLE ( 'NONE', #43121, 0.08000000000000069555 ) ;
#15399 = CARTESIAN_POINT ( 'NONE',  ( 1.511231465835579879, 1.905624552496063995, 1.020381674553122231 ) ) ;
#15400 = CARTESIAN_POINT ( 'NONE',  ( -4.969355510774519757, 7.965585441469681172, -1.036248007939699178 ) ) ;
#15402 = ADVANCED_FACE ( 'NONE', ( #175021 ), #89505, .T. ) ;
#15401 = CARTESIAN_POINT ( 'NONE',  ( 2.279949990775688384, 1.980252038983502993, -0.3961774098769352825 ) ) ;
#15403 = CARTESIAN_POINT ( 'NONE',  ( 4.161361007603033180, 7.399433999391101580, -0.7812420967184935394 ) ) ;
#15404 = EDGE_CURVE ( 'NONE', #8341, #21442, #182089, .T. ) ;
#15406 = CARTESIAN_POINT ( 'NONE',  ( 8.161645285746708112, 9.584636257201740506, -1.082531754730543083 ) ) ;
#15405 = CARTESIAN_POINT ( 'NONE',  ( 3.475000000000000533, -2.654166666666666785, 2.006292185433948827 ) ) ;
#15407 = CARTESIAN_POINT ( 'NONE',  ( -0.08058608058608779379, -5.907420853759267843, 10.99970480893080804 ) ) ;
#15408 = CARTESIAN_POINT ( 'NONE',  ( 0.6554828803995507158, 1.942095732595986890, -0.5424746339172461518 ) ) ;
#15409 = CARTESIAN_POINT ( 'NONE',  ( 5.390230798962840630, -0.5317533105795355652, -2.125930911514521959 ) ) ;
#15410 = AXIS2_PLACEMENT_3D ( 'NONE', #185176, #167882, #118132 ) ;
#15411 = CARTESIAN_POINT ( 'NONE',  ( -1.500000000000011324, 5.202083334016151639, 0.8660254037844403729 ) ) ;
#15412 = CARTESIAN_POINT ( 'NONE',  ( 3.445477555875466891, -1.765175379189663607, 0.7362804355328658179 ) ) ;
#15413 = CARTESIAN_POINT ( 'NONE',  ( -4.765854690403601879, 5.518917546014321829, 1.199719254218462483 ) ) ;
#15414 = CARTESIAN_POINT ( 'NONE',  ( 6.277061933002777927, 8.346324893301817482, 1.443375672974076540 ) ) ;
#15416 = CARTESIAN_POINT ( 'NONE',  ( 2.390250109419411295, -0.7743331304885041622, -1.862010821188607945 ) ) ;
#15415 = CARTESIAN_POINT ( 'NONE',  ( -9.693716643646601128, 12.33242205571964512, 1.443375672974076540 ) ) ;
#15417 = CARTESIAN_POINT ( 'NONE',  ( -1.402160292154681736E-14, 12.98437500034139980, 1.575800808251682339 ) ) ;
#15419 = CARTESIAN_POINT ( 'NONE',  ( -4.004454267989906668, 5.765225627445230927, 1.599625672291270506 ) ) ;
#15418 = CARTESIAN_POINT ( 'NONE',  ( 0.9609334056123096657, -2.075215392668391168, -0.9741618742916816620 ) ) ;
#15420 = CARTESIAN_POINT ( 'NONE',  ( 4.313312247719586878, -0.2936513069345859650, 1.699412160066446909 ) ) ;
#15421 = CARTESIAN_POINT ( 'NONE',  ( 6.556249800660121529, 9.806652646482286073, 1.199719254218452047 ) ) ;
#15422 = CARTESIAN_POINT ( 'NONE',  ( 4.334856428067313416, 6.080418470877079429, -1.599625672291256295 ) ) ;
#15423 = PLANE ( 'NONE',  #119867 ) ;
#15424 = CARTESIAN_POINT ( 'NONE',  ( 2.693266070609028784, 6.293894182352508970, 0.000000000000000000 ) ) ;
#15425 = CARTESIAN_POINT ( 'NONE',  ( 0.07536363704230969462, 1.333366039338843789, -2.397125032416930424 ) ) ;
#15426 = ORIENTED_EDGE ( 'NONE', *, *, #40826, .F. ) ;
#15427 = CARTESIAN_POINT ( 'NONE',  ( 0.000000000000000000, 0.000000000000000000, 0.000000000000000000 ) ) ;
#15428 = ORIENTED_EDGE ( 'NONE', *, *, #203560, .F. ) ;
#15429 = CARTESIAN_POINT ( 'NONE',  ( 5.250580378299275708, 1.785639943600283219, 0.3038008075236381389 ) ) ;
#15430 = AXIS2_PLACEMENT_3D ( 'NONE', #164391, #149202, #213116 ) ;
#15431 = ORIENTED_EDGE ( 'NONE', *, *, #78162, .T. ) ;
#15432 = CARTESIAN_POINT ( 'NONE',  ( 6.215487077222150880, 6.216099443039444949, 0.000000000000000000 ) ) ;
#15433 = PLANE ( 'NONE',  #194463 ) ;
#15434 = CARTESIAN_POINT ( 'NONE',  ( 6.041655779063732190, -1.703243848673033023, 0.6171442250446981248 ) ) ;
#15435 = CARTESIAN_POINT ( 'NONE',  ( 5.329763783503544516, 9.232158490813878515, -0.7216878364870458196 ) ) ;
#15436 = CARTESIAN_POINT ( 'NONE',  ( 2.275802642753376404, 5.638713387891790774, -0.5397176953658294751 ) ) ;
#15437 = CARTESIAN_POINT ( 'NONE',  ( 2.906388222866810978, 1.586772471669075424, -1.511725739355776366 ) ) ;
#15439 = CARTESIAN_POINT ( 'NONE',  ( 7.879259827836241570, 12.34422023245099176, 1.040834085586084257E-14 ) ) ;
#15438 = CARTESIAN_POINT ( 'NONE',  ( 5.793359732304666387, -1.682316520808274429, 0.7960761923023454978 ) ) ;
#15440 = CARTESIAN_POINT ( 'NONE',  ( 4.218306492681688447, 1.879367783149912929, 0.3698934672397135581 ) ) ;
#15441 = DIRECTION ( 'NONE',  ( -1.276756478318932585E-15, 1.000000000000000000, -1.665334536937738262E-16 ) ) ;
#15442 =( GEOMETRIC_REPRESENTATION_CONTEXT ( 3 ) GLOBAL_UNCERTAINTY_ASSIGNED_CONTEXT ( ( #162350 ) ) GLOBAL_UNIT_ASSIGNED_CONTEXT ( ( #46512, #113706, #97404 ) ) REPRESENTATION_CONTEXT ( 'NONE', 'WORKASPACE' ) );
#15443 = CARTESIAN_POINT ( 'NONE',  ( 0.6823417656249864960, -0.5739583329919112353, -1.181850606188749264 ) ) ;
#15444 = CARTESIAN_POINT ( 'NONE',  ( 4.473827502829567315, 7.202920605734387749, -1.082531754730548412 ) ) ;
#15445 = CARTESIAN_POINT ( 'NONE',  ( -9.571693261567968847, 12.19006144329456731, 1.443375672974076540 ) ) ;
#15446 = CARTESIAN_POINT ( 'NONE',  ( 0.2511322555047851290, -1.735185354305257110, 1.289038484408123963 ) ) ;
#15447 = CARTESIAN_POINT ( 'NONE',  ( -6.635789839245807897, 6.706452665400368218, 0.7998128361456341429 ) ) ;
#15448 = PRESENTATION_LAYER_ASSIGNMENT (  '', '', ( #108926 ) ) ;
#15449 = CARTESIAN_POINT ( 'NONE',  ( 5.239300017038202917, 5.077214539491492928, 0.000000000000000000 ) ) ;
#15450 = CARTESIAN_POINT ( 'NONE',  ( 0.3404811318320751234, 0.3065618842239411501, 1.799498403862239915 ) ) ;
#15451 = CARTESIAN_POINT ( 'NONE',  ( -2.903417451620861289, 6.539070793532962611, 0.7998128361456341429 ) ) ;
#15452 = CARTESIAN_POINT ( 'NONE',  ( 3.451995160207482094, 1.825762228170942914, 0.001041782061617091849 ) ) ;
#15453 = CARTESIAN_POINT ( 'NONE',  ( 9.729489633724101694, 13.21513059140455759, -8.104625967152696120 ) ) ;
#15454 = CARTESIAN_POINT ( 'NONE',  ( 2.566550162062298579, 0.6480892470011965223, 1.799338185917313870 ) ) ;
#15455 = VERTEX_POINT ( 'NONE', #42895 ) ;
#15456 = CARTESIAN_POINT ( 'NONE',  ( 2.225000061332568890, -1.799552404990023113, -0.8009105870329900068 ) ) ;
#15457 = ORIENTED_EDGE ( 'NONE', *, *, #15859, .T. ) ;
#15458 = CARTESIAN_POINT ( 'NONE',  ( 5.407742453289367646, -0.8769457196468108950, -1.732881886176732777 ) ) ;
#15459 = EDGE_LOOP ( 'NONE', ( #169150, #151400, #72684, #117556, #124402 ) ) ;
#15460 = CARTESIAN_POINT ( 'NONE',  ( -7.096767062110449942, 7.244259425409119046, -0.7998128361456362523 ) ) ;
#15462 = CARTESIAN_POINT ( 'NONE',  ( 5.467072749063267345, -1.670387955228332277, 1.306269166133757986 ) ) ;
#15461 = CARTESIAN_POINT ( 'NONE',  ( 7.503511670520385479, 7.718794801887437274, 0.7998128361456281477 ) ) ;
#15463 = PLANE ( 'NONE',  #52674 ) ;
#15464 = CARTESIAN_POINT ( 'NONE',  ( 3.369685512061989741, 0.4621021693036463374, -1.855490417808260961 ) ) ;
#15465 = CARTESIAN_POINT ( 'NONE',  ( 5.722549628727856330, 6.269105753387675506, -1.057781258018471782 ) ) ;
#15466 = CARTESIAN_POINT ( 'NONE',  ( 4.821333023213275837, 4.797512413269824805, 0.000000000000000000 ) ) ;
#15467 = ORIENTED_EDGE ( 'NONE', *, *, #83083, .F. ) ;
#15468 = CARTESIAN_POINT ( 'NONE',  ( 5.225741863424510747, 5.061396693608882558, 0.7998128361456352531 ) ) ;
#15469 = CARTESIAN_POINT ( 'NONE',  ( 5.522248639467795428, 5.337044922334209573, -0.7998128361456231517 ) ) ;
#15470 = CARTESIAN_POINT ( 'NONE',  ( 3.879544890376307453, 0.2443292893146010170, -1.998135132051428231 ) ) ;
#15471 = CARTESIAN_POINT ( 'NONE',  ( -0.4461809497497640775, 3.122791860410086606, 1.949595486268987043 ) ) ;
#15472 = CARTESIAN_POINT ( 'NONE',  ( 5.373610676068619973, 1.758448663713826132, -0.4906839848310071139 ) ) ;
#15473 = CARTESIAN_POINT ( 'NONE',  ( 0.2564123431100414074, -2.069877475643782994, -0.05227228806716639753 ) ) ;
#15474 = CARTESIAN_POINT ( 'NONE',  ( -7.212574532790092974, 10.39812547402169862, -1.082531754730543971 ) ) ;
#15475 = CARTESIAN_POINT ( 'NONE',  ( -5.971735067414164710, 7.203215006737162085, 1.225879040106806706 ) ) ;
#15476 = CARTESIAN_POINT ( 'NONE',  ( -0.3645075752536049429, 3.999999999999980904, -0.9782388703847658684 ) ) ;
#15477 = CARTESIAN_POINT ( 'NONE',  ( 5.225416543158964977, -1.776039340814106637, 0.5876355328483380269 ) ) ;
#15478 = CARTESIAN_POINT ( 'NONE',  ( 7.287671262545424966, 8.461036880179857889, -1.199719254218451159 ) ) ;
#15479 = CYLINDRICAL_SURFACE ( 'NONE', #152461, 0.08000000000000041800 ) ;
#15480 = CARTESIAN_POINT ( 'NONE',  ( -0.6823417656250039265, 10.13020833367472839, -1.181850606188755259 ) ) ;
#15481 = CARTESIAN_POINT ( 'NONE',  ( -4.574986769607567894, 7.424902766929059261, 1.199719254218464037 ) ) ;
#15483 = CARTESIAN_POINT ( 'NONE',  ( -5.908321080505254841, 10.11506803722328129, 0.7998128361456291469 ) ) ;
#15482 = CARTESIAN_POINT ( 'NONE',  ( 3.440018289565364817, 5.036440642624797626, 1.599625672291267398 ) ) ;
#15484 = CARTESIAN_POINT ( 'NONE',  ( -6.851666526859749418, 9.086973262793417661, -1.599625672291271394 ) ) ;
#15485 = CARTESIAN_POINT ( 'NONE',  ( -6.566226467720086113, 6.555019055295208119, 1.040834085586084257E-14 ) ) ;
#15486 = CARTESIAN_POINT ( 'NONE',  ( 1.709917326824461181, 0.6048241955843024487, -1.979901091156407666 ) ) ;
#15487 = CARTESIAN_POINT ( 'NONE',  ( 1.810321443220731075, 1.215999664948445913, -1.733040945678490319 ) ) ;
#15488 = CARTESIAN_POINT ( 'NONE',  ( 8.540746701604824409, 12.05162268759261224, -1.199719254218446718 ) ) ;
#15489 = CARTESIAN_POINT ( 'NONE',  ( 0.3769810270647828698, 3.049942316455306113, 0.4288785890452298522 ) ) ;
#15490 = CARTESIAN_POINT ( 'NONE',  ( 6.965700764728601335, -0.4599482372066622249, 2.025938098699997525 ) ) ;
#15491 = CARTESIAN_POINT ( 'NONE',  ( 4.170588824514860349, 7.607689953969209995, 0.8569815457360376865 ) ) ;
#15492 = CARTESIAN_POINT ( 'NONE',  ( 5.070386261830877928, 5.978167395966564435, -1.082531754730548412 ) ) ;
#15494 = CARTESIAN_POINT ( 'NONE',  ( 2.093037498677865482, 1.000000000000000888, -11.70868840297833025 ) ) ;
#15493 = CARTESIAN_POINT ( 'NONE',  ( -4.791166081694341550, 4.882818525799564213, 0.4357780244859492669 ) ) ;
#15495 = CARTESIAN_POINT ( 'NONE',  ( 2.133172796342793998, -2.046422403899459841, 1.032916798664377911 ) ) ;
#15496 = CARTESIAN_POINT ( 'NONE',  ( 3.946537740505224878, 2.817530495244566335, 0.7750000000000135669 ) ) ;
#15497 = CARTESIAN_POINT ( 'NONE',  ( 2.654443970922310214, 1.898414275235399407, 0.2300336082040748686 ) ) ;
#15498 = VERTEX_POINT ( 'NONE', #124213 ) ;
#15499 = CARTESIAN_POINT ( 'NONE',  ( 7.904040366642695048, 9.284097184913720824, 1.082531754730558626 ) ) ;
#15500 = CARTESIAN_POINT ( 'NONE',  ( 0.9846361663228007099, -1.273826410524713459, 1.558997777263083417 ) ) ;
#15501 = CARTESIAN_POINT ( 'NONE',  ( 1.446067858876250112, -0.8869304882095051523, 1.749921244195346004 ) ) ;
#15502 = CARTESIAN_POINT ( 'NONE',  ( -9.917953063596627317, 11.52969898140628047, -1.199719254218441611 ) ) ;
#15503 = CARTESIAN_POINT ( 'NONE',  ( -7.172426956829277778, 8.326585190177668849, -1.199719254218452935 ) ) ;
#15504 = CARTESIAN_POINT ( 'NONE',  ( -7.710915694720370972, -5.615420858948579230, -7.765925996254657626 ) ) ;
#15506 = CARTESIAN_POINT ( 'NONE',  ( 2.254462534575492949, -1.370001101035130509, 1.120467526443365891 ) ) ;
#15505 = CARTESIAN_POINT ( 'NONE',  ( 3.767594164193796669, 1.161519562870310329, 1.738068047407430816 ) ) ;
#15507 = LINE ( 'NONE', #200650, #154304 ) ;
#15508 = CIRCLE ( 'NONE', #32850, 2.150000000000000799 ) ;
#15510 = CARTESIAN_POINT ( 'NONE',  ( 5.841781729209135854, 2.289337533263948288, 0.1180171966539828449 ) ) ;
#15509 = CARTESIAN_POINT ( 'NONE',  ( 2.189521126745244128, 5.706191747844753692, 0.2764223219648713759 ) ) ;
#15511 = CARTESIAN_POINT ( 'NONE',  ( 4.189205958701418986, -0.6631863921694808317, 1.609220651327713414 ) ) ;
#15512 = EDGE_CURVE ( 'NONE', #109831, #113379, #22916, .T. ) ;
#15513 = CARTESIAN_POINT ( 'NONE',  ( 8.914649696185335870, 10.35917838609310593, -1.199719254218446718 ) ) ;
#15514 = CARTESIAN_POINT ( 'NONE',  ( 0.000000000000000000, 0.7999999999999951594, 0.000000000000000000 ) ) ;
#15515 = CARTESIAN_POINT ( 'NONE',  ( 4.217908468276907463, -1.441162302510163640, -0.9635822893686758484 ) ) ;
#15516 = CARTESIAN_POINT ( 'NONE',  ( 5.037629062015871462, 2.027634951229041693, -0.7768168075839574360 ) ) ;
#15517 = CARTESIAN_POINT ( 'NONE',  ( 4.857899112398166075, 4.561970474086296079, 1.040834085586084257E-14 ) ) ;
#15518 = CARTESIAN_POINT ( 'NONE',  ( 5.436732529336289588, -1.586671906620169104, 1.244382051841623538 ) ) ;
#15519 = CARTESIAN_POINT ( 'NONE',  ( 6.750000000000005329, 2.348403055487757740, 2.372725748337465745 ) ) ;
#15520 = CARTESIAN_POINT ( 'NONE',  ( -1.201851678989727383E-14, 3.993750000682817713, 1.732050807568877637 ) ) ;
#15521 = CARTESIAN_POINT ( 'NONE',  ( 3.276308702328960099, -1.148522560162130501, 1.546420931960400758 ) ) ;
#15522 = CARTESIAN_POINT ( 'NONE',  ( 1.500000000000001332, 9.406250000682799595, 0.000000000000000000 ) ) ;
#15523 = CARTESIAN_POINT ( 'NONE',  ( 5.326523995474015116, -0.9991460305027520805, -1.984133879135864920 ) ) ;
#15524 = VERTEX_POINT ( 'NONE', #190175 ) ;
#15525 = CARTESIAN_POINT ( 'NONE',  ( 6.983263157960402090, -0.0002233252893329463486, 1.845923184817334084 ) ) ;
#15526 = CARTESIAN_POINT ( 'NONE',  ( 1.499999999999989120, 3.025000000000020783, 1.214306433183764966E-14 ) ) ;
#15527 = CARTESIAN_POINT ( 'NONE',  ( 5.124091990960999432, 8.065525525174782828, -1.199719254218452047 ) ) ;
#15528 = ADVANCED_FACE ( 'NONE', ( #58047 ), #77083, .F. ) ;
#15529 = CARTESIAN_POINT ( 'NONE',  ( 1.225557454335997054, 1.961257301181002388, 1.042886780478131215 ) ) ;
#15530 = CARTESIAN_POINT ( 'NONE',  ( 6.777797683793751915, -1.903277019102869616, 0.4755351429900215310 ) ) ;
#15531 = CARTESIAN_POINT ( 'NONE',  ( 6.643132081016111634, 9.733775946952057723, 1.082531754730558626 ) ) ;
#15532 = ADVANCED_FACE ( 'NONE', ( #201334 ), #52973, .F. ) ;
#15533 = LINE ( 'NONE', #78417, #24717 ) ;
#15534 = CARTESIAN_POINT ( 'NONE',  ( 6.048345925472166762, 10.07050432311064903, 0.7216878364870317197 ) ) ;
#15535 = CARTESIAN_POINT ( 'NONE',  ( -3.634994582239682526, 6.294558541704648569, 1.082531754730549967 ) ) ;
#15537 = CARTESIAN_POINT ( 'NONE',  ( 4.861816908638716406, -0.5531579045409695805, 1.987044815706548562 ) ) ;
#15536 = CARTESIAN_POINT ( 'NONE',  ( 8.920375002787457319, 12.49452237230570084, 1.199719254218450271 ) ) ;
#15538 = CARTESIAN_POINT ( 'NONE',  ( -4.603156847039612920, 5.329103395422994716, 1.199719254218462483 ) ) ;
#15539 = CARTESIAN_POINT ( 'NONE',  ( 1.364683531249986537, -0.09479166632524321789, -0.7879004041258309554 ) ) ;
#15540 = CARTESIAN_POINT ( 'NONE',  ( 5.764887228985436707, -1.690807747980655584, -0.8004016547063924625 ) ) ;
#15541 = CARTESIAN_POINT ( 'NONE',  ( 5.063005163341266268, -0.9570555141230531193, 1.445894719807367723 ) ) ;
#15542 = CARTESIAN_POINT ( 'NONE',  ( 4.282551955697760704, 1.552239185393188947, -0.7873791831930468943 ) ) ;
#15543 = CARTESIAN_POINT ( 'NONE',  ( 4.681643115420508039, 4.356338477612361260, 0.7998128361456341429 ) ) ;
#15544 = CARTESIAN_POINT ( 'NONE',  ( 2.261634143469380742, 2.247403939606710477, -0.4510662058269006569 ) ) ;
#15545 = CARTESIAN_POINT ( 'NONE',  ( -0.6823417656249969321, 4.780208333674755394, -1.181850606188749264 ) ) ;
#15546 = CARTESIAN_POINT ( 'NONE',  ( 0.8140990769837243013, 1.700254657383609036, 0.7068247239481675326 ) ) ;
#15547 = CARTESIAN_POINT ( 'NONE',  ( 5.499899648425819798, 6.417811729657633357, 1.282877755774240791 ) ) ;
#15548 = CARTESIAN_POINT ( 'NONE',  ( 2.362075219488588562, 0.7782009281872975803, 1.651537983114875763 ) ) ;
#15549 = CARTESIAN_POINT ( 'NONE',  ( 2.443982611291168450, -1.755769474653746665, -0.9913988478210812305 ) ) ;
#15550 = CARTESIAN_POINT ( 'NONE',  ( 1.728746526384251858, 0.2170652002222578369, 2.180672313318913869 ) ) ;
#15551 = CARTESIAN_POINT ( 'NONE',  ( 9.412040618821951199, 14.12872955391332930, -8.482482427019883531 ) ) ;
#15552 = CARTESIAN_POINT ( 'NONE',  ( -7.121056995675673740, 9.330985799753529264, -1.599625672291263179 ) ) ;
#15553 = CARTESIAN_POINT ( 'NONE',  ( 1.645070734656968625, -0.3017366986639741788, -2.048123538821471801 ) ) ;
#15554 = CARTESIAN_POINT ( 'NONE',  ( 4.924636110261782385, 6.768494766770632332, 1.599625672291267398 ) ) ;
#15555 = CARTESIAN_POINT ( 'NONE',  ( -2.954552044183079750E-14, 2.578125000341414452, -1.570758158831808249 ) ) ;
#15556 = CARTESIAN_POINT ( 'NONE',  ( 3.914780425095893968, -0.6665358524936615403, -2.013057630646164942 ) ) ;
#15557 = CARTESIAN_POINT ( 'NONE',  ( 1.364683531249986537, 0.1135416670080857532, 0.7879004041258500513 ) ) ;
#15558 = CARTESIAN_POINT ( 'NONE',  ( 6.270122753791413928, 0.9430518052575274091, 1.563124558401955300 ) ) ;
#15559 = ORIENTED_EDGE ( 'NONE', *, *, #197651, .F. ) ;
#15560 = CARTESIAN_POINT ( 'NONE',  ( -3.983063267364693960, 7.868933921892603323, -0.7998128361456481317 ) ) ;
#15561 = CARTESIAN_POINT ( 'NONE',  ( 8.536830278099042602, 13.11138575775759563, -0.7998128361456352531 ) ) ;
#15562 = CARTESIAN_POINT ( 'NONE',  ( 5.519577934094851202, 8.493239118869080784, 1.082531754730547524 ) ) ;
#15563 = CARTESIAN_POINT ( 'NONE',  ( 1.737500000000001155, -3.339583332377417335, 3.009438278150922130 ) ) ;
#15564 = CARTESIAN_POINT ( 'NONE',  ( -5.910464900553636269, 8.982960586366182554, -1.199719254218440723 ) ) ;
#15565 = CARTESIAN_POINT ( 'NONE',  ( 3.287372214357705325, 0.04529362468645367623, -2.019439401957975111 ) ) ;
#15566 = CARTESIAN_POINT ( 'NONE',  ( 1.255059265495124476, -1.660252808076821296, 1.295518548220045529 ) ) ;
#15567 = CARTESIAN_POINT ( 'NONE',  ( -5.257529707049291900, 9.355811434857983500, 0.7998128361456291469 ) ) ;
#15568 = CARTESIAN_POINT ( 'NONE',  ( 8.483651433849084711, 10.92067931095586886, 1.599625672291281386 ) ) ;
#15569 = CARTESIAN_POINT ( 'NONE',  ( 5.278104476702146108, -0.9935453584285673934, -1.573305019461817444 ) ) ;
#15570 = CARTESIAN_POINT ( 'NONE',  ( 8.402302512167096893, 10.82577223566020841, -1.599625672291268286 ) ) ;
#15571 = DIRECTION ( 'NONE',  ( 0.000000000000000000, 0.000000000000000000, 1.000000000000000000 ) ) ;
#15572 = CARTESIAN_POINT ( 'NONE',  ( -2.930533758848195447, 6.570706485298192234, -0.7998128361456281477 ) ) ;
#15573 = CARTESIAN_POINT ( 'NONE',  ( -6.693975156845199059, 8.832723654451292816, 1.599625672291283607 ) ) ;
#15574 = CARTESIAN_POINT ( 'NONE',  ( 6.174695665487812235, -1.956078286930991394, -0.6490473743868007128 ) ) ;
#15575 = MECHANICAL_DESIGN_GEOMETRIC_PRESENTATION_REPRESENTATION (  '', ( #181629 ), #67362 ) ;
#15577 = CARTESIAN_POINT ( 'NONE',  ( -4.081306271799089558, 7.708262650413779227, 0.6970576149333465032 ) ) ;
#15576 = CARTESIAN_POINT ( 'NONE',  ( -4.288121723672178476, 8.224835454251337552, -0.7998128361456362523 ) ) ;
#15578 = CARTESIAN_POINT ( 'NONE',  ( 0.6823417656249882723, 0.09270833367475139752, 1.181850606188755259 ) ) ;
#15579 = CARTESIAN_POINT ( 'NONE',  ( 3.321388563693925544, -1.314311947043474538, 1.130952296748084951 ) ) ;
#15580 = CARTESIAN_POINT ( 'NONE',  ( 1.358879374581365429, 1.715036991836488056, -0.2946001921160408821 ) ) ;
#15582 = CARTESIAN_POINT ( 'NONE',  ( 6.643132081016117851, 8.773406732650713025, 1.443375672974076540 ) ) ;
#15581 = CARTESIAN_POINT ( 'NONE',  ( 6.709642313893407817, -0.5169605766506181199, 2.257632290342121539 ) ) ;
#15583 = CARTESIAN_POINT ( 'NONE',  ( -10.97409330344778944, 4.894225957061862253, -4.351021568302368969 ) ) ;
#15584 = CARTESIAN_POINT ( 'NONE',  ( 2.196623993872096392, -0.5467073567838857118, -1.986887711889900432 ) ) ;
#15585 = CARTESIAN_POINT ( 'NONE',  ( 3.845709127770629010, 7.638411082374393146, 0.7998128361456321445 ) ) ;
#15586 = CARTESIAN_POINT ( 'NONE',  ( 1.634138513624566302, 0.1511188354343559470, -2.010518437453466589 ) ) ;
#15587 = CARTESIAN_POINT ( 'NONE',  ( 6.925078400183521943, 1.220207665023531174, 2.355644635573426182 ) ) ;
#15588 = CARTESIAN_POINT ( 'NONE',  ( -5.798046968499580345, 6.793418213784815585, 1.199719254218452935 ) ) ;
#15589 = CARTESIAN_POINT ( 'NONE',  ( 0.6374961883623613268, -1.392493025731633027, -1.395827840033945000 ) ) ;
#15590 = COLOUR_RGB ( '', 0.08235294, 0.09019608, 0.10196078) ;
#15592 = CARTESIAN_POINT ( 'NONE',  ( -7.770231434407805615, 8.237893892996801526, 0.000000000000000000 ) ) ;
#15591 = CARTESIAN_POINT ( 'NONE',  ( 5.027564050633359649, -0.2746679736120913318, 1.892429487827557599 ) ) ;
#15593 = CARTESIAN_POINT ( 'NONE',  ( 6.164705905600972535, -1.563586322211576674, 1.557672334054376773 ) ) ;
#15594 = CARTESIAN_POINT ( 'NONE',  ( -6.658462837642833421, 8.861568958707010779, 1.443375672974064550 ) ) ;
#15595 = CARTESIAN_POINT ( 'NONE',  ( 5.664274315459256748, 9.830346811336296398, -0.7998128361456481317 ) ) ;
#15596 = VECTOR ( 'NONE', #191566, 1000.000000000000000 ) ;
#15597 = CARTESIAN_POINT ( 'NONE',  ( -5.289089322662584358, 5.343228095960675716, 0.000000000000000000 ) ) ;
#15598 = CARTESIAN_POINT ( 'NONE',  ( 0.5924517288934522119, -1.120073279264972799, 1.680413856445305498 ) ) ;
#15599 = DIRECTION ( 'NONE',  ( 0.000000000000000000, 0.000000000000000000, 1.000000000000000000 ) ) ;
#15600 = CARTESIAN_POINT ( 'NONE',  ( 5.104635005266920267, -0.7716809915320420599, -2.174869537816104703 ) ) ;
#15602 = EDGE_CURVE ( 'NONE', #175384, #11599, #194446, .T. ) ;
#15601 = CARTESIAN_POINT ( 'NONE',  ( 4.475024536774164119, 1.792854848340214025, 0.7970393728587571447 ) ) ;
#15603 = CARTESIAN_POINT ( 'NONE',  ( 2.096468001391890823, 1.939661435718213811, 0.2929505381348077031 ) ) ;
#15604 = CARTESIAN_POINT ( 'NONE',  ( 8.238550898598388628, 12.76339314834017102, 0.7998128361456462443 ) ) ;
#15605 = CARTESIAN_POINT ( 'NONE',  ( -9.367496997601303832, 14.48154074412966175, 7.499999999995374367 ) ) ;
#15606 = ORIENTED_EDGE ( 'NONE', *, *, #110555, .T. ) ;
#15607 = CARTESIAN_POINT ( 'NONE',  ( -0.2056253921914633354, -0.9106808701126485328, -1.909331193683319050 ) ) ;
#15609 = CARTESIAN_POINT ( 'NONE',  ( -8.193204901359996128, 8.453160561208463264, 1.040834085586084257E-14 ) ) ;
#15608 = CARTESIAN_POINT ( 'NONE',  ( -6.084912014434944894, 5.993485526462540847, -0.7998128361456291469 ) ) ;
#15610 = CARTESIAN_POINT ( 'NONE',  ( 1.253568445147245525, 0.7445567558202557112, 1.684058134371092752 ) ) ;
#15611 = ORIENTED_EDGE ( 'NONE', *, *, #136238, .T. ) ;
#15612 = CARTESIAN_POINT ( 'NONE',  ( 3.731445244768144764, 0.05858319805804703545, -2.170454240781857003 ) ) ;
#15613 = CARTESIAN_POINT ( 'NONE',  ( 10.19663671862204524, 10.80960751611106829, -6.241374320370645989 ) ) ;
#15614 = CARTESIAN_POINT ( 'NONE',  ( 1.951583061186522583, -1.892041120407188304, 0.9578705467366486204 ) ) ;
#15615 = CARTESIAN_POINT ( 'NONE',  ( -1.201851678989727383E-14, 2.868750000682821266, -1.732050807568863648 ) ) ;
#15616 = CARTESIAN_POINT ( 'NONE',  ( 8.727698198895078363, 11.20540053684285553, -1.599625672291257406 ) ) ;
#15617 = FILL_AREA_STYLE ('',( #30846 ) ) ;
#15618 = CARTESIAN_POINT ( 'NONE',  ( 6.435676556713933572, 6.878741676577107889, -0.7109887800627444632 ) ) ;
#15619 = CARTESIAN_POINT ( 'NONE',  ( 2.530605077378933920, 1.998055600607269833, 0.5039824654343558752 ) ) ;
#15621 = CARTESIAN_POINT ( 'NONE',  ( 0.3273695209934923689, 0.9472894719858866441, -1.578709817245539604 ) ) ;
#15620 = CARTESIAN_POINT ( 'NONE',  ( -7.330154606482786050, 11.70359747420527619, 0.000000000000000000 ) ) ;
#15622 = CARTESIAN_POINT ( 'NONE',  ( -1.201851678989727383E-14, 3.196875000341420137, -1.575800808251660134 ) ) ;
#15623 = CARTESIAN_POINT ( 'NONE',  ( -0.02264175331115596268, 2.007280006360371960, -2.503048469261221598 ) ) ;
#15624 = EDGE_CURVE ( 'NONE', #147438, #81487, #126778, .T. ) ;
#15625 = DIRECTION ( 'NONE',  ( -1.000000000000000000, 7.771561172376097755E-16, 4.440892098500627148E-16 ) ) ;
#15626 = CARTESIAN_POINT ( 'NONE',  ( 5.742805640131908973, 1.844151595126357179, 0.5056804652876015771 ) ) ;
#15627 = B_SPLINE_CURVE_WITH_KNOTS ( 'NONE', 3,
 ( #87554, #71269, #30549, #96627, #162682, #80346, #212460, #130247, #56120, #190364 ),
 .UNSPECIFIED., .F., .F.,
 ( 4, 1, 1, 1, 1, 1, 1, 4 ),
 ( 0.000000000000000000, 0.09884949474608377418, 0.1930937302289311708, 0.2616037862002966730, 0.3630310524065313849, 0.5216543902990324888, 0.7338513509102306820, 0.9999999999999998890 ),
 .UNSPECIFIED. ) ;
#15628 = CARTESIAN_POINT ( 'NONE',  ( -5.558479791478509568, 5.587240632920778438, 0.000000000000000000 ) ) ;
#15629 = B_SPLINE_CURVE_WITH_KNOTS ( 'NONE', 3,
 ( #85970, #152045, #153105, #120684, #50276, #37217, #88108 ),
 .UNSPECIFIED., .F., .F.,
 ( 4, 3, 4 ),
 ( 0.000000000000000000, 3.012973846129562487E-05, 4.150524011425761568E-05 ),
 .UNSPECIFIED. ) ;
#15630 = CARTESIAN_POINT ( 'NONE',  ( 1.915646641569005659, -0.2780824042511415017, 2.245213254143724413 ) ) ;
#15631 = CARTESIAN_POINT ( 'NONE',  ( -8.622622508611375025, 12.04318144581317895, 1.082531754730560403 ) ) ;
#15632 = CARTESIAN_POINT ( 'NONE',  ( 1.669862777068024995, 1.806593842016694484, -0.1355503349984941153 ) ) ;
#15633 = CARTESIAN_POINT ( 'NONE',  ( 1.745192250125559008, 0.3234662751879986975, -1.888026716711376674 ) ) ;
#15634 = CARTESIAN_POINT ( 'NONE',  ( 3.455589482447298355, 1.630370400113918095, 1.275915752658786095 ) ) ;
#15635 = CARTESIAN_POINT ( 'NONE',  ( -1.364683531250012516, 1.842708333674749843, 0.7879004041258379498 ) ) ;
#15636 = CARTESIAN_POINT ( 'NONE',  ( 1.551575459862795325, 0.5740822587161975576, -1.886020533208163430 ) ) ;
#15637 = CARTESIAN_POINT ( 'NONE',  ( 5.233004834321499210, 0.1438781470856145273, 1.921186297865638215 ) ) ;
#15639 = CARTESIAN_POINT ( 'NONE',  ( 6.463930056324285189, 6.765849701160138174, -0.2895399612845122039 ) ) ;
#15638 = CARTESIAN_POINT ( 'NONE',  ( 1.700300771062040361, -0.7742048122164610913, 2.174079040713126076 ) ) ;
#15640 = CARTESIAN_POINT ( 'NONE',  ( 0.6823417656249899377, 2.592708333674753618, 1.181850606188767472 ) ) ;
#15641 = CARTESIAN_POINT ( 'NONE',  ( 5.037578369333176376, 1.925844591945893747, -0.7392275334625797445 ) ) ;
#15642 = CARTESIAN_POINT ( 'NONE',  ( -5.225778143063529946, 8.184159369294361497, 1.199719254218452047 ) ) ;
#15643 = CARTESIAN_POINT ( 'NONE',  ( 7.396136491454752715, 8.587579647240744407, 1.199719254218462483 ) ) ;
#15644 = CARTESIAN_POINT ( 'NONE',  ( -1.244150428499027239, 2.902476754118171520, 0.7750000000000117906 ) ) ;
#15646 = CARTESIAN_POINT ( 'NONE',  ( 1.499999999999989120, 4.504166666666688634, 0.8660254037844524744 ) ) ;
#15645 = CARTESIAN_POINT ( 'NONE',  ( 6.528360061338796427, 1.215782546000489850, -1.719372923949607390 ) ) ;
#15647 = CARTESIAN_POINT ( 'NONE',  ( -1.201851678989727383E-14, 3.134375000341420137, 1.575800808251672791 ) ) ;
#15648 = CARTESIAN_POINT ( 'NONE',  ( 4.323607124742586016, -2.069909602744592014, 0.6229453038564189971 ) ) ;
#15650 = ADVANCED_FACE ( 'NONE', ( #113276, #95914 ), #178214, .T. ) ;
#15649 = CARTESIAN_POINT ( 'NONE',  ( 5.901037506996139825, -0.2983434833860042490, -1.997397228102874234 ) ) ;
#15651 = CARTESIAN_POINT ( 'NONE',  ( 1.734723475976807094E-15, -3.469446951953614189E-15, 0.2971265334020881110 ) ) ;
#15652 = CARTESIAN_POINT ( 'NONE',  ( -5.043269954603569083, 7.867270132804026872, 1.082531754730560403 ) ) ;
#15653 = EDGE_CURVE ( 'NONE', #190021, #127784, #160437, .T. ) ;
#15656 = CARTESIAN_POINT ( 'NONE',  ( 3.524756749872944628, 7.056040608253000279, -0.7216878364870267237 ) ) ;
#15655 = CARTESIAN_POINT ( 'NONE',  ( 3.285556943750000514, -2.763541666188707335, 1.896917185911906500 ) ) ;
#15654 = CARTESIAN_POINT ( 'NONE',  ( 7.201315867513990554, 8.430565262634994284, -1.199719254218452047 ) ) ;
#15657 = CARTESIAN_POINT ( 'NONE',  ( -5.601453741101424022, 6.564059448486966986, -1.199719254218453823 ) ) ;
#15658 = CARTESIAN_POINT ( 'NONE',  ( 3.538296236868877731, 0.7303062672313584969, 1.879804216660937666 ) ) ;
#15659 = CARTESIAN_POINT ( 'NONE',  ( -7.934546212495630968, 10.28005655271014795, -1.599625672291263179 ) ) ;
#15661 = CARTESIAN_POINT ( 'NONE',  ( -8.068510813464099485, 8.585886501895810596, 0.7216878364870317197 ) ) ;
#15660 = CARTESIAN_POINT ( 'NONE',  ( -8.487040972474682476, 12.84537220128841817, 0.7216878364870338292 ) ) ;
#15662 = CARTESIAN_POINT ( 'NONE',  ( -1.364683531249997417, 5.259375000341425022, 1.214306433183764966E-14 ) ) ;
#15664 = CARTESIAN_POINT ( 'NONE',  ( -0.6823417656250039265, 9.317708333674733723, -1.181850606188755259 ) ) ;
#15663 = CARTESIAN_POINT ( 'NONE',  ( 4.698204674003193304, -2.161138953124014161, -0.05634304724232848394 ) ) ;
#15665 = CARTESIAN_POINT ( 'NONE',  ( 10.64229060209973454, 1.016282880930359234, -6.144329343916673736 ) ) ;
#15666 = CARTESIAN_POINT ( 'NONE',  ( -11.72945658997776519, 7.464408392728353547, -2.545424847964329995 ) ) ;
#15668 = CARTESIAN_POINT ( 'NONE',  ( 5.308220328704632784, 1.198845711980157214, -1.621194722098241003 ) ) ;
#15667 = CARTESIAN_POINT ( 'NONE',  ( -8.161645285302366659, 8.624267042381978499, 1.040834085586084257E-14 ) ) ;
#15669 = CARTESIAN_POINT ( 'NONE',  ( 0.6823417656249864960, -0.7614583329919113464, -1.181850606188749264 ) ) ;
#15670 = CARTESIAN_POINT ( 'NONE',  ( 0.9610595616070281011, 0.3405255003954327786, -1.690740162648683320 ) ) ;
#15671 = CARTESIAN_POINT ( 'NONE',  ( 5.747730777550676073, 5.670383760089384495, 0.000000000000000000 ) ) ;
#15673 = CARTESIAN_POINT ( 'NONE',  ( 6.587282531393223728, 8.778525268082516320, 1.599625672291268286 ) ) ;
#15672 = CARTESIAN_POINT ( 'NONE',  ( 8.622622508611357262, 9.162073802909148412, -0.7216878364870197293 ) ) ;
#15674 = CARTESIAN_POINT ( 'NONE',  ( -11.62989982712325521, 8.355808186217915434, -2.970614550598404069 ) ) ;
#15675 = CARTESIAN_POINT ( 'NONE',  ( 6.344977084850584426, -1.580176071495458023, 1.000667393836668362 ) ) ;
#15676 =( BOUNDED_CURVE ( )  B_SPLINE_CURVE ( 2, ( #103489, #2752, #169550, #134944, #52599, #118727, #203089, #168482, #171680 ),
 .UNSPECIFIED., .F., .T. ) 
 B_SPLINE_CURVE_WITH_KNOTS ( ( 3, 2, 2, 2, 3 ),
 ( 0.5982142857142856984, 0.6011904761904761640, 0.6071428571428570953, 0.6130952380952381375, 0.6160714285714286031 ),
 .UNSPECIFIED. ) 
 CURVE ( )  GEOMETRIC_REPRESENTATION_ITEM ( )  RATIONAL_B_SPLINE_CURVE ( ( 0.9330127018922194093, 0.9330127018922194093, 1.000000000000000000, 0.8660254037844387076, 1.000000000000000000, 0.8660254037844387076, 1.000000000000000000, 0.9330127018922194093, 0.9330127018922194093 ) ) 
 REPRESENTATION_ITEM ( '' )  );
#15677 = CARTESIAN_POINT ( 'NONE',  ( 0.9791529934419791470, -1.820790759202662423, -0.8588917989246074303 ) ) ;
#15678 =( NAMED_UNIT ( * ) PLANE_ANGLE_UNIT ( ) SI_UNIT ( $, .RADIAN. ) );
#15679 = CARTESIAN_POINT ( 'NONE',  ( 2.872332416675418276, 1.179501869419818494, 1.864919306664609921 ) ) ;
#15680 = CARTESIAN_POINT ( 'NONE',  ( -6.929625909916163451, 7.257187447756535903, 0.7216878364870317197 ) ) ;
#15681 = ORIENTED_EDGE ( 'NONE', *, *, #57019, .T. ) ;
#15682 = CARTESIAN_POINT ( 'NONE',  ( 8.175203438916005538, 11.52119253116861586, -1.082531754730543083 ) ) ;
#15684 = CARTESIAN_POINT ( 'NONE',  ( 1.985954055300429344, -2.015913623055834325, 0.05231662700833779323 ) ) ;
#15683 = CARTESIAN_POINT ( 'NONE',  ( 2.508575005364023003, -2.114979441823850337, -0.1534387461676611220 ) ) ;
#15686 = VERTEX_POINT ( 'NONE', #143613 ) ;
#15685 = CARTESIAN_POINT ( 'NONE',  ( 2.742218629285391174, 1.002941080561991161, -1.508394886552874237 ) ) ;
#15687 = CARTESIAN_POINT ( 'NONE',  ( 6.393551957296131683, 9.616838495890963401, 1.199719254218452047 ) ) ;
#15688 = ORIENTED_EDGE ( 'NONE', *, *, #79134, .F. ) ;
#15689 = COLOUR_RGB ( '', 0.66274510, 0.83137255, 0.94901961) ;
#15690 = CARTESIAN_POINT ( 'NONE',  ( 6.661133543015731462, 6.665743976473484267, -0.7998128361456281477 ) ) ;
#15692 = CARTESIAN_POINT ( 'NONE',  ( -0.2236198635829286518, -0.4190533842500678841, -1.875677477222786438 ) ) ;
#15691 = CARTESIAN_POINT ( 'NONE',  ( -2.740719608256871442, 6.349256642941639051, 0.7998128361456341429 ) ) ;
#15693 = CARTESIAN_POINT ( 'NONE',  ( -1.499999999999997780, 3.400000000000021227, 1.214306433183764966E-14 ) ) ;
#15694 = DIRECTION ( 'NONE',  ( 0.000000000000000000, 0.000000000000000000, 1.000000000000000000 ) ) ;
#15695 = CIRCLE ( 'NONE', #136790, 0.7499999999999997780 ) ;
#15696 = CARTESIAN_POINT ( 'NONE',  ( 4.812781342726850653, 8.558735966582574406, 0.7216878364870438212 ) ) ;
#15697 = CARTESIAN_POINT ( 'NONE',  ( -0.6823417656250212460, 0.8635416670080899859, 1.181850606188755259 ) ) ;
#15698 = LINE ( 'NONE', #81783, #153700 ) ;
#15699 = CARTESIAN_POINT ( 'NONE',  ( -9.917953063596627317, 11.52969898140628047, -1.199719254218441611 ) ) ;
#15700 = CARTESIAN_POINT ( 'NONE',  ( 5.331013795412237855, 0.1550192300789655642, 2.156197635354038411 ) ) ;
#15701 = CARTESIAN_POINT ( 'NONE',  ( -4.814553946628611136, 8.631080347793099961, 0.000000000000000000 ) ) ;
#15702 = CARTESIAN_POINT ( 'NONE',  ( 3.919715808126649659, 7.587102519540811940, 0.000000000000000000 ) ) ;
#15703 = CARTESIAN_POINT ( 'NONE',  ( 1.476976393720277780, -1.495863523836362896, 1.503369785937097136 ) ) ;
#15704 = DIRECTION ( 'NONE',  ( 5.551115123125764213E-17, 0.000000000000000000, -1.000000000000000000 ) ) ;
#15705 = CARTESIAN_POINT ( 'NONE',  ( 2.864479682042244679, -1.362014001507254379, 1.425398218059505728 ) ) ;
#15706 = CARTESIAN_POINT ( 'NONE',  ( 5.783449990912790106, 0.1341079605299954347, -1.907733270042926810 ) ) ;
#15707 = ORIENTED_EDGE ( 'NONE', *, *, #177065, .F. ) ;
#15708 = CARTESIAN_POINT ( 'NONE',  ( 1.754755943840834664, -0.9608980427861594231, 1.301694008101298428 ) ) ;
#15710 = EDGE_CURVE ( 'NONE', #156724, #37959, #96025, .T. ) ;
#15709 = CARTESIAN_POINT ( 'NONE',  ( 0.5552397518338060278, 1.722184604005328357, -1.148819969904082861 ) ) ;
#15711 = CARTESIAN_POINT ( 'NONE',  ( 1.271315641948435493, 1.156325127695263744, 1.560008962195078563 ) ) ;
#15712 = EDGE_LOOP ( 'NONE', ( #25730, #38611, #32130, #45142 ) ) ;
#15713 = DIRECTION ( 'NONE',  ( 1.000000000000000000, -7.387867266669436732E-31, 0.000000000000000000 ) ) ;
#15715 = CARTESIAN_POINT ( 'NONE',  ( 0.4645879757426182866, -7.605490376146398113, 10.08385597498928554 ) ) ;
#15714 = CARTESIAN_POINT ( 'NONE',  ( -7.431277594066160397, 7.842447745931541370, -0.7216878364870338292 ) ) ;
#15717 = CARTESIAN_POINT ( 'NONE',  ( 7.091078035147269532, 8.231678114882006625, 1.199719254218462483 ) ) ;
#15716 = CARTESIAN_POINT ( 'NONE',  ( 2.607466773009491146, -2.067780616408128935, 0.3074339443978144626 ) ) ;
#15719 = CARTESIAN_POINT ( 'NONE',  ( 4.028181036591620412, 7.713645286083276709, -0.7216878364870338292 ) ) ;
#15718 = CARTESIAN_POINT ( 'NONE',  ( 5.608269097547198712, 9.694731047113750222, -0.7998128361456281477 ) ) ;
#15721 = EDGE_LOOP ( 'NONE', ( #161453, #145540, #126899, #189962 ) ) ;
#15720 = CARTESIAN_POINT ( 'NONE',  ( 5.707647354773449422, 1.450964518888698596, 1.245719642194928811 ) ) ;
#15722 = CARTESIAN_POINT ( 'NONE',  ( 4.740968412965463230, 0.3751893352213676591, 2.174603215771487630 ) ) ;
#15723 = CARTESIAN_POINT ( 'NONE',  ( 1.571597221169357628, 0.1616201177277211132, -2.200922231076734903 ) ) ;
#15724 = CARTESIAN_POINT ( 'NONE',  ( 0.5570965697654255422, -1.639946202723217450, 0.9833419947904218361 ) ) ;
#15725 = CARTESIAN_POINT ( 'NONE',  ( -10.59781858645781405, 12.29999999999997939, 3.302687032930891498 ) ) ;
#15726 = DIRECTION ( 'NONE',  ( 0.9632918427306595976, 0.000000000000000000, -0.2684563758389253985 ) ) ;
#15727 = CARTESIAN_POINT ( 'NONE',  ( 4.141125838365485201, -0.1998502692034490602, -2.060677327190631569 ) ) ;
#15728 = AXIS2_PLACEMENT_3D ( 'NONE', #192854, #79117, #145232 ) ;
#15730 = CARTESIAN_POINT ( 'NONE',  ( 1.692469166403000491, -2.151312531270420436, -0.2117842694067117448 ) ) ;
#15729 = CARTESIAN_POINT ( 'NONE',  ( -2.927671105547157371, 5.503034492191895666, 1.199719254218462483 ) ) ;
#15731 = CARTESIAN_POINT ( 'NONE',  ( 4.230150181147958044, 2.149441460308566754, 0.4267382380854707336 ) ) ;
#15732 = CARTESIAN_POINT ( 'NONE',  ( -0.8683822406226825441, -0.9819185891646172726, 3.363299488115865543 ) ) ;
#15733 = FILL_AREA_STYLE ('',( #160948 ) ) ;
#15734 = DIRECTION ( 'NONE',  ( 0.000000000000000000, 1.000000000000000000, 0.000000000000000000 ) ) ;
#15735 = CARTESIAN_POINT ( 'NONE',  ( -1.402160292154681736E-14, 14.23437500034139624, 1.575800808251682339 ) ) ;
#15736 = CARTESIAN_POINT ( 'NONE',  ( -3.467853430045390706, 7.267855778353407459, 0.7998128361456352531 ) ) ;
#15737 = UNCERTAINTY_MEASURE_WITH_UNIT (LENGTH_MEASURE( 1.000000000000000082E-05 ), #142410, 'distance_accuracy_value', 'NONE');
#15738 = CARTESIAN_POINT ( 'NONE',  ( 0.7213275451133926985, 1.987047012402185731, 0.3419330716275259530 ) ) ;
#15740 = CARTESIAN_POINT ( 'NONE',  ( -9.544576954340667996, 11.19805653722800365, 1.082531754730558626 ) ) ;
#15739 = VECTOR ( 'NONE', #83387, 1000.000000000000000 ) ;
#15741 = CARTESIAN_POINT ( 'NONE',  ( 4.821179601816666604, -1.846891146645711412, -0.9356023351853595127 ) ) ;
#15742 = CARTESIAN_POINT ( 'NONE',  ( 5.501600788752927684, -2.065472302299308893, 0.4645820118519652930 ) ) ;
#15743 = CARTESIAN_POINT ( 'NONE',  ( 6.972971076130050072, 7.029554431773520129, 1.040834085586084257E-14 ) ) ;
#15744 = CARTESIAN_POINT ( 'NONE',  ( 9.574107575049751517, 3.767509416808738187, 7.159700411437358802 ) ) ;
#15745 = CARTESIAN_POINT ( 'NONE',  ( 4.223468175789964363, 0.2452432568937177593, -1.954070501097299850 ) ) ;
#15746 = CARTESIAN_POINT ( 'NONE',  ( 5.806620824396801162, 2.019002025885249463, 1.085389930784508961 ) ) ;
#15747 = CARTESIAN_POINT ( 'NONE',  ( 4.512205841073367196, -0.7830535718562798841, -1.649371741558727678 ) ) ;
#15748 = TOROIDAL_SURFACE ( 'NONE', #188631, 11.92000000000000171, 0.08000000000000000167 ) ;
#15749 = CARTESIAN_POINT ( 'NONE',  ( 4.095444919779759552, 6.935713618788495793, 1.199719254218451159 ) ) ;
#15750 = CARTESIAN_POINT ( 'NONE',  ( 3.484082288587588838, 7.008587070086755411, -0.7216878364870267237 ) ) ;
#15751 = CARTESIAN_POINT ( 'NONE',  ( -7.306918443122272677, 7.489436036589583345, 0.7998128361456341429 ) ) ;
#15752 = CARTESIAN_POINT ( 'NONE',  ( 4.694866332082116678, 8.699370830729650450, 0.7998128361456341429 ) ) ;
#15753 = ORIENTED_EDGE ( 'NONE', *, *, #123817, .T. ) ;
#15754 = CARTESIAN_POINT ( 'NONE',  ( 4.711194051470749322, 1.671412949727559383, -1.121937078508246755 ) ) ;
#15755 = CARTESIAN_POINT ( 'NONE',  ( 6.293571109369822558, 1.706569967861866877, -1.540138442258129459 ) ) ;
#15756 = CARTESIAN_POINT ( 'NONE',  ( 4.311346321947408633, -1.628642355029306987, -1.093319670275281652 ) ) ;
#15757 = CARTESIAN_POINT ( 'NONE',  ( -6.826694039680798021, 7.923230120171105284, -1.199719254218446718 ) ) ;
#15758 = CARTESIAN_POINT ( 'NONE',  ( -3.411848212133334446, 7.132240014130862171, 0.7998128361456341429 ) ) ;
#15759 = CARTESIAN_POINT ( 'NONE',  ( -0.1409997244346075651, 7.629137130509101361, -2.600278764091648487 ) ) ;
#15760 = CARTESIAN_POINT ( 'NONE',  ( -6.017840079619296567, 8.114175741012878973, -1.599625672291271394 ) ) ;
#15762 = CARTESIAN_POINT ( 'NONE',  ( 6.069200897874186040, 0.1259568369440123015, -1.765440829579780990 ) ) ;
#15761 = CARTESIAN_POINT ( 'NONE',  ( 0.7496951219271037470, 2.088183804393455301, -0.1063107438588738879 ) ) ;
#15763 = DIRECTION ( 'NONE',  ( -0.6507913734559650498, -0.7592566023652995710, 0.000000000000000000 ) ) ;
#15764 = CARTESIAN_POINT ( 'NONE',  ( 6.333930032320489900, 1.921166581771537318, 0.2825802787540276917 ) ) ;
#15765 = CARTESIAN_POINT ( 'NONE',  ( 1.482659311839970684, -0.3241159351022730450, -2.167229700873399612 ) ) ;
#15766 = CARTESIAN_POINT ( 'NONE',  ( 1.171013094284451439, 1.035884637911354877, 1.398405216058955514 ) ) ;
#15767 = CARTESIAN_POINT ( 'NONE',  ( 5.829115978871627135, 8.888053511070525659, 1.199719254218462483 ) ) ;
#15768 = CARTESIAN_POINT ( 'NONE',  ( 0.1335669894368500255, -0.0009366757763962055587, -2.153671288142432250 ) ) ;
#15769 = CARTESIAN_POINT ( 'NONE',  ( 1.242334483997083572, 0.3330332824765611099, 1.692230457194281223 ) ) ;
#15770 = CARTESIAN_POINT ( 'NONE',  ( 1.716621854089026344, 2.046377219401524616, 0.7848826361863747714 ) ) ;
#15771 = CARTESIAN_POINT ( 'NONE',  ( 4.582781371344160526, -2.140174514510746029, -0.5380331057033281850 ) ) ;
#15772 = CARTESIAN_POINT ( 'NONE',  ( 0.9366657375849207767, -1.207674400081097721, 1.803990093267322736 ) ) ;
#15773 = CARTESIAN_POINT ( 'NONE',  ( 0.3459771380207553593, 1.820543102168985961, 0.1377627428671979182 ) ) ;
#15774 = CARTESIAN_POINT ( 'NONE',  ( 2.307945874296753797, -1.223308491024234224, -1.728006348806595316 ) ) ;
#15775 = CARTESIAN_POINT ( 'NONE',  ( 6.639320575229254118, 2.070803455257670844, 2.204946390281757207 ) ) ;
#15776 = ORIENTED_EDGE ( 'NONE', *, *, #9604, .F. ) ;
#15778 = CARTESIAN_POINT ( 'NONE',  ( -1.402160292154681736E-14, 0.2593750003414224681, -1.575800808251665908 ) ) ;
#15777 = CARTESIAN_POINT ( 'NONE',  ( 2.490095330609965796, -2.286454923436448183, -0.1652806634409968445 ) ) ;
#15779 = CARTESIAN_POINT ( 'NONE',  ( 4.005544317833563461, 6.760553239859419250, -1.199719254218452047 ) ) ;
#15780 = EDGE_CURVE ( 'NONE', #134989, #76889, #171673, .T. ) ;
#15781 = CARTESIAN_POINT ( 'NONE',  ( 5.250715360749964589, 2.188191852258320136, 0.3812115871067219275 ) ) ;
#15782 = CARTESIAN_POINT ( 'NONE',  ( -6.643132081016132062, 8.773406732650713025, 1.443375672974078761 ) ) ;
#15783 = CARTESIAN_POINT ( 'NONE',  ( -1.843739406749240750, 9.999999999999998224, 0.7750000000000013545 ) ) ;
#15784 = CARTESIAN_POINT ( 'NONE',  ( 4.473827502829567315, 7.202920605734387749, -1.082531754730548412 ) ) ;
#15785 = B_SPLINE_CURVE_WITH_KNOTS ( 'NONE', 3,
 ( #148899, #51405, #19942, #18872, #472, #16737, #200813, #84956, #199761, #2614 ),
 .UNSPECIFIED., .F., .F.,
 ( 4, 3, 3, 4 ),
 ( 1.661478437462647650E-14, 3.125169445508157778E-05, 5.676984422619956599E-05, 8.229491417181853481E-05 ),
 .UNSPECIFIED. ) ;
#15786 = CARTESIAN_POINT ( 'NONE',  ( -7.822691444960713447, 9.189190109618056823, -1.082531754730543083 ) ) ;
#15787 = CARTESIAN_POINT ( 'NONE',  ( 3.933273961740286317, 7.602920365423422311, 0.7216878364870257245 ) ) ;
#15788 = VERTEX_POINT ( 'NONE', #29830 ) ;
#15789 = CARTESIAN_POINT ( 'NONE',  ( 3.375625116643202972, -0.3961014713874110305, -1.976955985980306307 ) ) ;
#15791 = CARTESIAN_POINT ( 'NONE',  ( 1.446217529737943153, -0.9311174319141333200, 1.840543939966767351 ) ) ;
#15790 = CARTESIAN_POINT ( 'NONE',  ( 6.089583550832340819, 10.25626457594641749, 1.040834085586084257E-14 ) ) ;
#15792 = FACE_BOUND ( 'NONE', #83613, .T. ) ;
#15793 = CARTESIAN_POINT ( 'NONE',  ( 4.055297343818931033, 6.784911763547157193, 1.082531754730549078 ) ) ;
#15794 = CARTESIAN_POINT ( 'NONE',  ( 1.500000000000001332, 8.656250000682797818, 0.000000000000000000 ) ) ;
#15795 = CARTESIAN_POINT ( 'NONE',  ( -0.6823417656250212460, 3.551041667008085323, 1.181850606188767472 ) ) ;
#15796 = CARTESIAN_POINT ( 'NONE',  ( 4.031328258368102269, -1.510625130563835627, -1.587819133214096734 ) ) ;
#15797 = CARTESIAN_POINT ( 'NONE',  ( 1.934220422044398813, -1.621183349045727473, -1.198859219795316955 ) ) ;
#15798 = CARTESIAN_POINT ( 'NONE',  ( 1.118424870118275738, -0.04499623084481922664, 1.840855209834332928 ) ) ;
#15799 = CARTESIAN_POINT ( 'NONE',  ( 8.620286740190458374, 8.951422706510690830, 1.040834085586084257E-14 ) ) ;
#15800 = EDGE_CURVE ( 'NONE', #211199, #42744, #188990, .T. ) ;
#15801 = CARTESIAN_POINT ( 'NONE',  ( 4.823181420811452291, -0.08861582515604787824, 1.823562061424352621 ) ) ;
#15802 = CARTESIAN_POINT ( 'NONE',  ( 5.942029771888944545, -1.730864577151491890, -1.034168155301495862 ) ) ;
#15803 = CARTESIAN_POINT ( 'NONE',  ( -6.530223543276495235, 10.77034456713125188, -0.7998128361456291469 ) ) ;
#15805 = CARTESIAN_POINT ( 'NONE',  ( -5.444481204339554736, 8.509589284108232121, 1.199719254218454489 ) ) ;
#15804 = CARTESIAN_POINT ( 'NONE',  ( 4.469752058069711431, 2.195618827641317772, -0.5456854893412068641 ) ) ;
#15806 = CARTESIAN_POINT ( 'NONE',  ( 1.295691649255722888, 1.595764685746006384, 1.374534258749359861 ) ) ;
#15807 = CARTESIAN_POINT ( 'NONE',  ( -7.422162748838431412, 7.623887726591770608, -0.7998128361456362523 ) ) ;
#15808 = CARTESIAN_POINT ( 'NONE',  ( 4.492674960910642667, 2.029786422369950216, 0.4070406814440513665 ) ) ;
#15809 = CARTESIAN_POINT ( 'NONE',  ( 9.185812768458653466, 10.67553530374532045, 1.199719254218453823 ) ) ;
#15810 = CARTESIAN_POINT ( 'NONE',  ( 1.360316468749961816, 2.817708333674743493, -0.7853790794159141164 ) ) ;
#15811 = DIRECTION ( 'NONE',  ( -0.4100809324301146752, 0.000000000000000000, 0.9120491373041518246 ) ) ;
#15812 = CARTESIAN_POINT ( 'NONE',  ( -8.341290820905609138, 10.75459192918846618, 1.599625672291269396 ) ) ;
#15813 =( LENGTH_UNIT ( ) NAMED_UNIT ( * ) SI_UNIT ( .MILLI., .METRE. ) );
#15814 = CARTESIAN_POINT ( 'NONE',  ( 6.851666526859736983, 9.086973262793417661, -1.599625672291269396 ) ) ;
#15815 = CARTESIAN_POINT ( 'NONE',  ( 5.373129273518238769, 6.310201232541126970, -1.074510414011679016 ) ) ;
#15816 = CARTESIAN_POINT ( 'NONE',  ( -4.060830702492950195, 4.696389560118578999, -1.199719254218452047 ) ) ;
#15818 = CARTESIAN_POINT ( 'NONE',  ( 2.197798511016679335, 2.028856164703813025, -0.9050913924920337417 ) ) ;
#15817 = CARTESIAN_POINT ( 'NONE',  ( 1.494549364340029163, -1.129948290531690658, 1.794289463044356436 ) ) ;
#15819 = CARTESIAN_POINT ( 'NONE',  ( -0.08053691275167716712, 15.51887838114830132, 11.99972973886013961 ) ) ;
#15820 = CARTESIAN_POINT ( 'NONE',  ( -5.752402313948099533, 9.933162809573264695, -0.7998128361456362523 ) ) ;
#15821 = CARTESIAN_POINT ( 'NONE',  ( 5.612185521052973414, 8.634967976948757951, -1.199719254218440723 ) ) ;
#15822 = CARTESIAN_POINT ( 'NONE',  ( 2.945700582358207864, 1.385421296276163838, 1.389331660621349274 ) ) ;
#15823 = CARTESIAN_POINT ( 'NONE',  ( 4.150767584078112193, 7.994312614733129152, 0.7998128361456321445 ) ) ;
#15824 = CARTESIAN_POINT ( 'NONE',  ( -4.037324417950741484, 7.593329901778307800, 0.3124507474575183297 ) ) ;
#15825 = CARTESIAN_POINT ( 'NONE',  ( 2.672928840188529609, 6.270167413528593414, 0.000000000000000000 ) ) ;
#15826 = CARTESIAN_POINT ( 'NONE',  ( -5.966997003790232235, 7.094489604910957148, -1.082531754730549967 ) ) ;
#15827 = CARTESIAN_POINT ( 'NONE',  ( -6.344852701515500293, 9.385783337534627790, 1.082531754730548412 ) ) ;
#15828 = CARTESIAN_POINT ( 'NONE',  ( 2.180079139336263516, 2.078761533942363737, -0.4183221158333137457 ) ) ;
#15829 = CARTESIAN_POINT ( 'NONE',  ( -5.586841817283045408, 8.675676665875643678, 1.199719254218454489 ) ) ;
#15830 = CARTESIAN_POINT ( 'NONE',  ( 5.916451087343006954, 0.7937011933104149985, 1.794315766958521241 ) ) ;
#15831 = CARTESIAN_POINT ( 'NONE',  ( 3.467792127863758456, 2.109446376165153847, -0.4717452660116944196 ) ) ;
#15832 = CARTESIAN_POINT ( 'NONE',  ( 2.489598673502769977, -1.836455140896048999, -0.1334285330320400531 ) ) ;
#15833 = CARTESIAN_POINT ( 'NONE',  ( -4.145235801320589886, 7.447099624555288067, -0.7035710955675591460 ) ) ;
#15834 = CARTESIAN_POINT ( 'NONE',  ( -1.402160292154681736E-14, -0.9906249996585834161, -1.575800808251665908 ) ) ;
#15835 = CARTESIAN_POINT ( 'NONE',  ( 4.734162553523208139, 0.3016713478377709423, 1.713805963711847680 ) ) ;
#15836 = CARTESIAN_POINT ( 'NONE',  ( 6.727182134110202050, 7.629137130509070275, 2.410944104600750038 ) ) ;
#15837 = CARTESIAN_POINT ( 'NONE',  ( 3.701012746850603996, 7.261672604726938651, 1.040834085586084257E-14 ) ) ;
#15838 = DIRECTION ( 'NONE',  ( 0.000000000000000000, 0.000000000000000000, -1.000000000000000000 ) ) ;
#15839 = CARTESIAN_POINT ( 'NONE',  ( 1.569428280142046717, 0.1587979871724466974, -2.155937297210829495 ) ) ;
#15840 = VECTOR ( 'NONE', #107578, 1000.000000000000000 ) ;
#15841 = CARTESIAN_POINT ( 'NONE',  ( 4.429064430395744267, 0.9478954142983322395, 1.779353956671766657 ) ) ;
#15842 = CARTESIAN_POINT ( 'NONE',  ( -8.554831740098665094, 11.00372300158037042, 1.443375672974064550 ) ) ;
#15843 = CARTESIAN_POINT ( 'NONE',  ( 1.112450467520700537, -0.9725818059473789745, -1.930612204972524282 ) ) ;
#15844 = CARTESIAN_POINT ( 'NONE',  ( 2.337131052746133975, -1.762546391092616238, 0.8830908230641126844 ) ) ;
#15845 = CIRCLE ( 'NONE', #105895, 0.05000000000000056483 ) ;
#15846 = CARTESIAN_POINT ( 'NONE',  ( 10.32992389895506413, 1.000000000000000888, 6.106772653521394645 ) ) ;
#15847 = CARTESIAN_POINT ( 'NONE',  ( 3.931145062177692218, -1.341491907185809795, -1.404491712913302104 ) ) ;
#15850 = ORIENTED_EDGE ( 'NONE', *, *, #100912, .T. ) ;
#15849 = DIRECTION ( 'NONE',  ( 1.276756478318932585E-15, -1.000000000000000000, 1.665334536937738262E-16 ) ) ;
#15848 = CARTESIAN_POINT ( 'NONE',  ( -9.232739420781982176, 12.75498451001223010, 1.082531754730558626 ) ) ;
#15851 = B_SPLINE_CURVE_WITH_KNOTS ( 'NONE', 3,
 ( #133956, #33214, #197839, #135005, #151245, #101413 ),
 .UNSPECIFIED., .F., .F.,
 ( 4, 2, 4 ),
 ( 0.000000000000000000, 0.0003155923098472859139, 0.0006311846196945721530 ),
 .UNSPECIFIED. ) ;
#15852 = CARTESIAN_POINT ( 'NONE',  ( -7.282664789195997912, 8.525472337930658284, 1.199719254218452047 ) ) ;
#15853 = CARTESIAN_POINT ( 'NONE',  ( 3.250922972226694352, 7.014770244231638863, 0.7998128361456281477 ) ) ;
#15855 = EDGE_LOOP ( 'NONE', ( #70311, #146301, #171842, #87400 ) ) ;
#15854 = CARTESIAN_POINT ( 'NONE',  ( -6.981522756394290319, 7.109807735406931783, 0.7998128361456341429 ) ) ;
#15856 = CARTESIAN_POINT ( 'NONE',  ( -8.880227426826648340, 11.38335130276301754, 1.443375672974064550 ) ) ;
#15857 = CARTESIAN_POINT ( 'NONE',  ( 1.659489206604364941, -1.893029981318217647, -1.133929415002648655 ) ) ;
#15859 = EDGE_CURVE ( 'NONE', #166249, #139889, #179281, .T. ) ;
#15858 = CARTESIAN_POINT ( 'NONE',  ( 1.001543065824772753E-15, -2.471874999522041705, 3.793834371823811669 ) ) ;
#15860 = CARTESIAN_POINT ( 'NONE',  ( 5.682460714699895554, 1.171467074228413674, -1.573401077569417605 ) ) ;
#15861 =( BOUNDED_CURVE ( )  B_SPLINE_CURVE ( 2, ( #42415, #161487, #126925 ),
 .UNSPECIFIED., .F., .T. ) 
 B_SPLINE_CURVE_WITH_KNOTS ( ( 3, 3 ),
 ( 0.1249999999999998751, 0.1276624645066395392 ),
 .UNSPECIFIED. ) 
 CURVE ( )  GEOMETRIC_REPRESENTATION_ITEM ( )  RATIONAL_B_SPLINE_CURVE ( ( 1.000000000000003997, 0.9143913742683281720, 0.9381891137235824907 ) ) 
 REPRESENTATION_ITEM ( '' )  );
#15862 = CARTESIAN_POINT ( 'NONE',  ( 3.819616621146375568, -1.462967937902563964, -1.530840818714680029 ) ) ;
#15863 = CARTESIAN_POINT ( 'NONE',  ( 1.499999999999989120, 2.535416667349483344, 0.8660254037844524744 ) ) ;
#15864 = CARTESIAN_POINT ( 'NONE',  ( 0.1745949693968874838, 0.2569705180060793404, -1.790672585839627740 ) ) ;
#15865 = CARTESIAN_POINT ( 'NONE',  ( 4.470543924053159479, -0.002573283451708791025, -1.841320590191763973 ) ) ;
#15866 = ORIENTED_EDGE ( 'NONE', *, *, #21052, .F. ) ;
#15867 = CARTESIAN_POINT ( 'NONE',  ( -8.681298431451969222, 9.022603012982438386, 1.040834085586084257E-14 ) ) ;
#15868 = CARTESIAN_POINT ( 'NONE',  ( -0.4000000000000243916, 2.999999999999999112, 7.500000000000000000 ) ) ;
#15869 = CARTESIAN_POINT ( 'NONE',  ( 5.273731010124149243, 0.4114677744767555878, -2.080124947408354963 ) ) ;
#15870 = DIRECTION ( 'NONE',  ( 0.000000000000000000, -1.000000000000000000, 0.000000000000000000 ) ) ;
#15871 = CARTESIAN_POINT ( 'NONE',  ( 7.122110765880372618, 7.203550736482235095, 0.7998128361456341429 ) ) ;
#15872 = CARTESIAN_POINT ( 'NONE',  ( 6.919229409281150822, -0.1609914934341447335, 2.026046322553672674 ) ) ;
#15875 = CARTESIAN_POINT ( 'NONE',  ( 3.825598141381767903, 0.9817388958630569595, -1.557492293685861284 ) ) ;
#15874 = CARTESIAN_POINT ( 'NONE',  ( 0.3087543870234563115, -1.498283157731963966, 1.103738804280843366 ) ) ;
#15873 = CARTESIAN_POINT ( 'NONE',  ( 1.499999999999987566, 6.120000000000041851, -2.499999999999995115 ) ) ;
#15876 = CARTESIAN_POINT ( 'NONE',  ( 7.313733799568044702, 10.62010763521636214, 1.199719254218460707 ) ) ;
#15877 = DIRECTION ( 'NONE',  ( 0.000000000000000000, 0.000000000000000000, 1.000000000000000000 ) ) ;
#15878 = CARTESIAN_POINT ( 'NONE',  ( -7.456058132872594335, 7.663432341298296535, 0.000000000000000000 ) ) ;
#15879 = CARTESIAN_POINT ( 'NONE',  ( -0.3123298761244324151, -8.144690279336741057, -9.521443730523929005 ) ) ;
#15880 = CIRCLE ( 'NONE', #136973, 0.7500000000000011102 ) ;
#15881 = CARTESIAN_POINT ( 'NONE',  ( 3.563272299071856164, -1.946135509614330239, -1.040604674307284316 ) ) ;
#15882 = CARTESIAN_POINT ( 'NONE',  ( 4.481858567196604248, 1.473221693029845181, 1.717120190082993103 ) ) ;
#15883 = CARTESIAN_POINT ( 'NONE',  ( -5.558479791922849245, 9.428717490644563881, 0.7216878364870458196 ) ) ;
#15884 = CARTESIAN_POINT ( 'NONE',  ( 4.869312882171149326, -1.534379415642408651, -0.9627496050425389251 ) ) ;
#15885 = CARTESIAN_POINT ( 'NONE',  ( 5.717977451880697615, 0.9379096786080630688, -1.670315906950563534 ) ) ;
#15886 = CARTESIAN_POINT ( 'NONE',  ( -1.364683531250010295, 5.301041667008085767, -0.7879004041258300672 ) ) ;
#15887 = CARTESIAN_POINT ( 'NONE',  ( 6.086763352761943580, -0.2763008855245497331, -1.850001521387992565 ) ) ;
#15888 = CARTESIAN_POINT ( 'NONE',  ( 6.408657378324259746, 0.5850815967071677504, 1.766781856238110127 ) ) ;
#15889 = FACE_OUTER_BOUND ( 'NONE', #110188, .T. ) ;
#15890 = PRESENTATION_LAYER_ASSIGNMENT (  '', '', ( #8954 ) ) ;
#15891 = CARTESIAN_POINT ( 'NONE',  ( 6.209784286858486269, -1.755916252942066436, 0.2208807251847556830 ) ) ;
#15892 = CARTESIAN_POINT ( 'NONE',  ( 1.059780186608853203, 1.205045252304644210, 1.616690996016925563 ) ) ;
#15894 = CARTESIAN_POINT ( 'NONE',  ( 3.158910222468692908, -1.594458197781272846, 1.376041720736504992 ) ) ;
#15893 = CARTESIAN_POINT ( 'NONE',  ( -2.779058300676974014, 6.186059084191009916, -0.7216878364870257245 ) ) ;
#15895 = CARTESIAN_POINT ( 'NONE',  ( 9.748476143425788720, 11.33197590787365172, -1.199719254218440723 ) ) ;
#15897 = CARTESIAN_POINT ( 'NONE',  ( -9.236128959407555072, 11.79856975744075598, -1.599625672291263179 ) ) ;
#15896 = DIRECTION ( 'NONE',  ( 0.8594003466332824637, -0.03762549425793430824, 0.5099170191202098135 ) ) ;
#15898 = CARTESIAN_POINT ( 'NONE',  ( -15.75000000000000000, 11.29999999999999893, 0.6999999999999992895 ) ) ;
#15900 = ADVANCED_FACE ( 'NONE', ( #81764 ), #159815, .F. ) ;
#15899 = CARTESIAN_POINT ( 'NONE',  ( 2.179950100978587990, 1.979969115219997189, -0.3981650194792104025 ) ) ;
#15901 = CARTESIAN_POINT ( 'NONE',  ( 1.364683531249988757, 2.134375000341422357, 1.214306433183764966E-14 ) ) ;
#15902 = AXIS2_PLACEMENT_3D ( 'NONE', #107468, #124804, #89033 ) ;
#15903 = CARTESIAN_POINT ( 'NONE',  ( 3.472859903394816872, 7.203420320602605287, -0.7998128361456291469 ) ) ;
#15904 = CARTESIAN_POINT ( 'NONE',  ( 3.286554482555790191, -2.129011082553730727, -0.3730605165198074835 ) ) ;
#15905 = CARTESIAN_POINT ( 'NONE',  ( 6.890000000000014779, 6.038692643467888921, 2.314896014905319266 ) ) ;
#15907 = CARTESIAN_POINT ( 'NONE',  ( -15.75000000000000000, 9.799999999999998934, 0.6999999999999992895 ) ) ;
#15906 = CARTESIAN_POINT ( 'NONE',  ( 5.259637247458703868, 5.100941308315409373, 0.000000000000000000 ) ) ;
#15908 = CARTESIAN_POINT ( 'NONE',  ( 9.368320956918614328, 10.99242454023565507, 1.082531754730549967 ) ) ;
#15909 = CARTESIAN_POINT ( 'NONE',  ( -1.500000000000043299, 3.952083334016152971, 0.8660254037844216102 ) ) ;
#15910 = CARTESIAN_POINT ( 'NONE',  ( -5.910991785878158211, 9.839981483592442402, -0.7216878364870278340 ) ) ;
#15911 = ADVANCED_FACE ( 'NONE', ( #119659 ), #118589, .F. ) ;
#15912 = CARTESIAN_POINT ( 'NONE',  ( -1.364683531250014514, 0.2802083336747505649, 0.7879004041258379498 ) ) ;
#15913 = CARTESIAN_POINT ( 'NONE',  ( 1.189316404147572337, 1.662717542896676504, 1.427817766309902314 ) ) ;
#15914 = CARTESIAN_POINT ( 'NONE',  ( 0.1471985351164479261, 7.029189141431359644, 1.995741298138908659 ) ) ;
#15915 = CARTESIAN_POINT ( 'NONE',  ( 1.587200854914575077, -0.3333832325802545404, -2.237697771577638051 ) ) ;
#15916 = CARTESIAN_POINT ( 'NONE',  ( -7.537443334193545397, 10.88110209227943770, -1.199719254218446718 ) ) ;
#15917 = CARTESIAN_POINT ( 'NONE',  ( -3.755245360860939297, 4.443836344834937613, -1.082531754730548412 ) ) ;
#15918 = CARTESIAN_POINT ( 'NONE',  ( -1.364683531249997417, 4.071875000341417028, 1.214306433183764966E-14 ) ) ;
#15919 = CARTESIAN_POINT ( 'NONE',  ( 4.739057715201537846, 8.198473722472776615, 0.7146191656044629248 ) ) ;
#15920 = CARTESIAN_POINT ( 'NONE',  ( 1.500000000000001332, 11.37499999999999645, 0.000000000000000000 ) ) ;
#15921 = CARTESIAN_POINT ( 'NONE',  ( 5.090160327287878594, 4.903218234782778850, -0.7998128361456481317 ) ) ;
#15922 = CARTESIAN_POINT ( 'NONE',  ( 3.672906134817868651, 0.04599029964666952880, -1.769319831623831663 ) ) ;
#15923 = CARTESIAN_POINT ( 'NONE',  ( 0.1300960903409088820, -1.296115720595720333, -1.660425602283533308 ) ) ;
#15924 = CARTESIAN_POINT ( 'NONE',  ( 1.364683531250000303, 9.255208333674733723, -0.7879004041258355073 ) ) ;
#15925 = ORIENTED_EDGE ( 'NONE', *, *, #152973, .F. ) ;
#15926 = CARTESIAN_POINT ( 'NONE',  ( -6.394605727500880299, 7.489403432619674561, -1.199719254218452047 ) ) ;
#15927 = CARTESIAN_POINT ( 'NONE',  ( 5.396111305808362957, -0.9091601233324579923, -1.799916296964368279 ) ) ;
#15928 = EDGE_LOOP ( 'NONE', ( #12206, #50682, #166097, #175057, #75827 ) ) ;
#15929 = CARTESIAN_POINT ( 'NONE',  ( 2.904993682805886213, 1.579364189935757778, 1.002181356900035070 ) ) ;
#15930 = CARTESIAN_POINT ( 'NONE',  ( 2.905202624773517872, -1.723727875341171556, 1.146311801414557241 ) ) ;
#15931 = EDGE_CURVE ( 'NONE', #108458, #76077, #15785, .T. ) ;
#15932 = CARTESIAN_POINT ( 'NONE',  ( -6.956742217143487395, 8.249192353823097790, 1.082531754730549078 ) ) ;
#15933 = CARTESIAN_POINT ( 'NONE',  ( 1.933716311909071006, -1.854087253938462521, 0.4680378644332866545 ) ) ;
#15934 = CARTESIAN_POINT ( 'NONE',  ( -0.6386677588215945445, 3.364506011487724990, 0.1366812159789567160 ) ) ;
#15935 = CARTESIAN_POINT ( 'NONE',  ( -1.566570994388993832, 8.685985410138266971, 2.500753655585676416 ) ) ;
#15936 = CARTESIAN_POINT ( 'NONE',  ( 1.364683531249988535, 4.217708333674752730, -0.7879004041258239610 ) ) ;
#15937 = CARTESIAN_POINT ( 'NONE',  ( 0.9141475326900461162, -1.912571728325638931, 0.002704284578637640782 ) ) ;
#15938 = CARTESIAN_POINT ( 'NONE',  ( 2.910546574502240968, 0.6583626327048962557, 1.848246418561696913 ) ) ;
#15939 = CARTESIAN_POINT ( 'NONE',  ( 0.1751529202326657098, -0.8592662624449104447, -1.822031250676876768 ) ) ;
#15940 = CARTESIAN_POINT ( 'NONE',  ( -4.111865726694519552, 8.019203457777400956, 0.000000000000000000 ) ) ;
#15942 = CARTESIAN_POINT ( 'NONE',  ( -1.286813488861823895, 3.652992958535467238, -0.4595522011843558574 ) ) ;
#15941 = CARTESIAN_POINT ( 'NONE',  ( 7.736899214892750010, 12.17813285068358020, 1.040834085586084257E-14 ) ) ;
#15943 = CARTESIAN_POINT ( 'NONE',  ( 0.4033012769992084245, -0.5052730135347226481, 1.800932346938296069 ) ) ;
#15944 = CARTESIAN_POINT ( 'NONE',  ( -0.6823417656250003738, 2.467708333674753618, -1.181850606188749264 ) ) ;
#15945 = CARTESIAN_POINT ( 'NONE',  ( 1.652591521987197831, 1.991881122867325660, 0.2913371046347946747 ) ) ;
#15946 = CIRCLE ( 'NONE', #137057, 2.250000000000006661 ) ;
#15948 = CARTESIAN_POINT ( 'NONE',  ( 1.687271568794300070, 1.762372639767064042, 1.173053760763353104 ) ) ;
#15947 = CARTESIAN_POINT ( 'NONE',  ( -6.209271165378811297, 10.18797409300986878, 0.7216878364870458196 ) ) ;
#15949 = CARTESIAN_POINT ( 'NONE',  ( -6.622231685632140596, 6.690634819517756959, 0.000000000000000000 ) ) ;
#15950 = CARTESIAN_POINT ( 'NONE',  ( 3.578635096964689843, 1.315621898185691974, -1.598582974826658010 ) ) ;
#15951 = CARTESIAN_POINT ( 'NONE',  ( 4.899292406491845497, 6.809203455697518947, -1.599625672291273171 ) ) ;
#15953 = CARTESIAN_POINT ( 'NONE',  ( 3.897079088924235712, 6.634010472798538949, 1.199719254218462483 ) ) ;
#15952 = CARTESIAN_POINT ( 'NONE',  ( 5.947236541613409422, 0.6080794538029854479, -2.000250932508009782 ) ) ;
#15955 = ORIENTED_EDGE ( 'NONE', *, *, #137980, .F. ) ;
#15954 = CARTESIAN_POINT ( 'NONE',  ( 4.137589658204786858, -1.258905094989383189, -1.322318538811013688 ) ) ;
#15956 = CARTESIAN_POINT ( 'NONE',  ( 10.55232363013785246, 11.20546574478267132, 0.000000000000000000 ) ) ;
#15957 = FILL_AREA_STYLE_COLOUR ( '', #202953 ) ;
#15958 = CARTESIAN_POINT ( 'NONE',  ( 10.42905686949577060, 8.762263237317901243, 3.815400753447676152 ) ) ;
#15959 = CARTESIAN_POINT ( 'NONE',  ( 5.297975422827020608, -0.7987165953184969247, 2.057335881587420534 ) ) ;
#15960 = CARTESIAN_POINT ( 'NONE',  ( -1.364683531250010740, 10.19270833367473017, 0.7879004041258445001 ) ) ;
#15961 = ORIENTED_EDGE ( 'NONE', *, *, #71135, .F. ) ;
#15962 = CARTESIAN_POINT ( 'NONE',  ( 5.303337639526568559, 1.684534858470821961, -0.9050978215178404618 ) ) ;
#15963 = CARTESIAN_POINT ( 'NONE',  ( -9.917953063596627317, 11.52969898140628047, -1.199719254218441611 ) ) ;
#15964 = CARTESIAN_POINT ( 'NONE',  ( 8.294891053462476904, 8.571794405328034827, 1.040834085586084257E-14 ) ) ;
#15965 = CARTESIAN_POINT ( 'NONE',  ( -4.957638175832625493E-14, 1.734375000341442208, 1.570758158831756068 ) ) ;
#15966 = CARTESIAN_POINT ( 'NONE',  ( 5.300874872818840622, 6.247070775452521652, 1.082531754730560403 ) ) ;
#15967 = CARTESIAN_POINT ( 'NONE',  ( 4.182432031930846947E-16, 4.099999999999999645, -2.350000000000007194 ) ) ;
#15968 = DIRECTION ( 'NONE',  ( -0.000000000000000000, -1.000000000000000000, -0.000000000000000000 ) ) ;
#15969 = CARTESIAN_POINT ( 'NONE',  ( 0.2043192855987647494, 1.601443664334546213, 0.9084302959305108338 ) ) ;
#15970 = ORIENTED_EDGE ( 'NONE', *, *, #17921, .T. ) ;
#15971 = CARTESIAN_POINT ( 'NONE',  ( -6.563028877466991595, 9.814561569423593923, 1.199719254218452935 ) ) ;
#15972 = CARTESIAN_POINT ( 'NONE',  ( 4.780451015977909002, -1.813929833846049666, -0.4561423458772846939 ) ) ;
#15973 = AXIS2_PLACEMENT_3D ( 'NONE', #161683, #65206, #28465 ) ;
#15974 = LINE ( 'NONE', #47463, #199100 ) ;
#15975 = CARTESIAN_POINT ( 'NONE',  ( -6.344852701515500293, 9.385783337534627790, 1.082531754730548412 ) ) ;
#15976 = TOROIDAL_SURFACE ( 'NONE', #178517, 10.92000000000000171, 0.08000000000000000167 ) ;
#15977 = CARTESIAN_POINT ( 'NONE',  ( 3.472859903394816872, 7.203420320602605287, -0.7998128361456291469 ) ) ;
#15978 = CARTESIAN_POINT ( 'NONE',  ( 1.674589265674136129, 1.326639880153294371, -1.455732889183375178 ) ) ;
#15979 = CARTESIAN_POINT ( 'NONE',  ( 1.898064762488653079, -0.9530305783747442527, -1.777002450075705120 ) ) ;
#15980 = CARTESIAN_POINT ( 'NONE',  ( -8.402302512167102222, 10.82577223566020841, -1.599625672291263179 ) ) ;
#15981 = CARTESIAN_POINT ( 'NONE',  ( 5.017399365509065845, 8.011327138806002779, -1.199719254218450271 ) ) ;
#15982 = CYLINDRICAL_SURFACE ( 'NONE', #108234, 0.7500000000000011102 ) ;
#15983 = CARTESIAN_POINT ( 'NONE',  ( 2.133021248740565756, -1.956732443736847182, 0.9868821405488172882 ) ) ;
#15984 = CARTESIAN_POINT ( 'NONE',  ( -9.499766273075884726, -9.919999999999998153, 0.06663900456894793212 ) ) ;
#15985 = CARTESIAN_POINT ( 'NONE',  ( -7.784352752540590004, 12.23349531127272094, 0.7998128361456481317 ) ) ;
#15986 = CARTESIAN_POINT ( 'NONE',  ( 6.825078400183575589, 6.038285016609903799, 2.450557349082567171 ) ) ;
#15987 = CARTESIAN_POINT ( 'NONE',  ( 1.386567914617462760, 8.090296256147720300, 10.72428812184712044 ) ) ;
#15988 = CARTESIAN_POINT ( 'NONE',  ( 6.048345925472191631, 6.229027465905275562, 0.7216878364870328300 ) ) ;
#15989 = CARTESIAN_POINT ( 'NONE',  ( 9.610031953988080744, 10.10612545594124967, -0.7998128361456281477 ) ) ;
#15990 = CARTESIAN_POINT ( 'NONE',  ( -3.325722479476970861, 7.699077257576049327, -2.499999999999995115 ) ) ;
#15991 = CARTESIAN_POINT ( 'NONE',  ( 5.383996398402570271, 9.295429874862735531, 0.000000000000000000 ) ) ;
#15992 = ORIENTED_EDGE ( 'NONE', *, *, #129225, .F. ) ;
#15994 = CARTESIAN_POINT ( 'NONE',  ( 1.576815760046655912, -1.422047136828644476, 1.425140908648862448 ) ) ;
#15993 = CARTESIAN_POINT ( 'NONE',  ( 5.144037045698616417, 0.5398437887287730330, 1.760322748975438500 ) ) ;
#15995 = CARTESIAN_POINT ( 'NONE',  ( 3.655889646864494580, -0.4445778678274399098, -2.254845314064676032 ) ) ;
#15997 = CARTESIAN_POINT ( 'NONE',  ( 0.5669689972240202769, 1.615300940711749789, 0.9240007631576854230 ) ) ;
#15996 = CARTESIAN_POINT ( 'NONE',  ( 2.223174002961016082, 5.537527403522402025, -0.7216878364870267237 ) ) ;
#15998 = CARTESIAN_POINT ( 'NONE',  ( 3.285556943749998737, -1.655208332855374609, -1.896917185911906500 ) ) ;
#15999 = CARTESIAN_POINT ( 'NONE',  ( -4.129789846611330972, 3.920435697242382833, -0.2706067644339962830 ) ) ;
#16000 = CARTESIAN_POINT ( 'NONE',  ( 5.273660385517703553, 0.3669835118517566497, -1.876681294024808988 ) ) ;
#16001 = CARTESIAN_POINT ( 'NONE',  ( -9.643927338022246332, 10.14567007064778004, -0.7998128361456291469 ) ) ;
#16002 = CARTESIAN_POINT ( 'NONE',  ( -7.431277594066160397, 7.842447745931541370, -0.7216878364870338292 ) ) ;
#16004 = CARTESIAN_POINT ( 'NONE',  ( 2.641296366799699147, -1.384790685969448099, -1.257831364775918503 ) ) ;
#16003 = CARTESIAN_POINT ( 'NONE',  ( 4.177344015168626079, 1.367166224251268547, 1.581858325755406858 ) ) ;
#16005 = CARTESIAN_POINT ( 'NONE',  ( 6.588899466561449536, 9.670504563421618016, -1.082531754730537088 ) ) ;
#16006 = CARTESIAN_POINT ( 'NONE',  ( 5.952668924537682038, -1.582617586749142102, -0.9407850039931386910 ) ) ;
#16007 = CARTESIAN_POINT ( 'NONE',  ( 4.857899112398166075, 4.561970474086296079, 1.040834085586084257E-14 ) ) ;
#16009 = CARTESIAN_POINT ( 'NONE',  ( 5.192936529234042808, 6.017179691316550283, -1.199719254218452047 ) ) ;
#16008 = CARTESIAN_POINT ( 'NONE',  ( -6.484567079770452658, -6.583980363594976737, -7.100579091573040458 ) ) ;
#16010 = CARTESIAN_POINT ( 'NONE',  ( 5.461458274417386072, 0.3306134467882023142, -1.692711794494299538 ) ) ;
#16011 = CARTESIAN_POINT ( 'NONE',  ( -6.364663046611467756, 9.512858423433634414, 1.199719254218452047 ) ) ;
#16012 = CARTESIAN_POINT ( 'NONE',  ( 0.8614527929159084829, -0.04078779759817893064, -1.733857029152048757 ) ) ;
#16013 = FILL_AREA_STYLE_COLOUR ( '', #115960 ) ;
#16014 = AXIS2_PLACEMENT_3D ( 'NONE', #40234, #6633, #5549 ) ;
#16015 = CARTESIAN_POINT ( 'NONE',  ( -10.84254087577847869, 4.919568073182958301, 5.035408296252059657 ) ) ;
#16016 = CARTESIAN_POINT ( 'NONE',  ( 4.663029205760478746, 1.682383395889605282, -1.372325453836314768 ) ) ;
#16017 = CARTESIAN_POINT ( 'NONE',  ( 3.070728972534173096, -1.687097908962056803, -0.6982200720766564839 ) ) ;
#16018 = CARTESIAN_POINT ( 'NONE',  ( 0.6374591745182572877, 1.832550977151351290, -0.7006947966294306829 ) ) ;
#16019 = CARTESIAN_POINT ( 'NONE',  ( 6.034383107294147841, 0.6662506799693500570, 2.009816206752083723 ) ) ;
#16021 = CARTESIAN_POINT ( 'NONE',  ( -1.364683531249997417, 4.321875000341417028, 1.214306433183764966E-14 ) ) ;
#16020 = CARTESIAN_POINT ( 'NONE',  ( 5.776963781812925802, 2.119385065811297597, -0.8740618393795733798 ) ) ;
#16022 = CARTESIAN_POINT ( 'NONE',  ( -4.312804375668592982, 3.926026614568435935, 0.2365836213946782007 ) ) ;
#16023 = CARTESIAN_POINT ( 'NONE',  ( 8.860417081730671995, 10.29590700256267155, 1.199719254218453823 ) ) ;
#16025 = ADVANCED_FACE ( 'NONE', ( #152102 ), #20996, .F. ) ;
#16024 = AXIS2_PLACEMENT_3D ( 'NONE', #62734, #29185, #193800 ) ;
#16026 = CARTESIAN_POINT ( 'NONE',  ( 1.524255003590764046, -2.104078925693805502, 0.2628582283784736684 ) ) ;
#16027 = CARTESIAN_POINT ( 'NONE',  ( -2.806174608348664723, 6.217694776474651519, 1.040834085586084257E-14 ) ) ;
#16028 = DIRECTION ( 'NONE',  ( 0.000000000000000000, 0.000000000000000000, -1.000000000000000000 ) ) ;
#16029 = CARTESIAN_POINT ( 'NONE',  ( -3.402733366905605905, 6.913679994791092298, 0.7216878364870317197 ) ) ;
#16030 = CARTESIAN_POINT ( 'NONE',  ( 5.998927374810688384, 0.4157333352466702769, 2.130747042934706403 ) ) ;
#16032 = CARTESIAN_POINT ( 'NONE',  ( -1.500000000000015099, 12.01041666734946034, -0.8660254037844309360 ) ) ;
#16031 = CARTESIAN_POINT ( 'NONE',  ( 6.883263157960363365, 3.690127339433949327, 2.567897385111846731 ) ) ;
#16033 = ORIENTED_EDGE ( 'NONE', *, *, #99218, .T. ) ;
#16035 = ORIENTED_EDGE ( 'NONE', *, *, #37798, .F. ) ;
#16034 = CARTESIAN_POINT ( 'NONE',  ( 1.893536009595264469, -0.1129285828431712546, -2.218558826778730619 ) ) ;
#16036 = CARTESIAN_POINT ( 'NONE',  ( 5.801407773674092105, 1.352156682446105984, -1.496049708713815374 ) ) ;
#16038 = CARTESIAN_POINT ( 'NONE',  ( 6.069198595068595381, 1.816300881853601723, 0.9774375683993684616 ) ) ;
#16037 = CARTESIAN_POINT ( 'NONE',  ( 4.578903193113299963, 6.365139696764064325, 1.599625672291267398 ) ) ;
#16040 = CARTESIAN_POINT ( 'NONE',  ( -0.2409995289980003397, 0.7158067089181943121, -2.082568332340509087 ) ) ;
#16039 = CARTESIAN_POINT ( 'NONE',  ( 6.540882763950133238, 6.595727744222092959, 0.000000000000000000 ) ) ;
#16041 = CARTESIAN_POINT ( 'NONE',  ( 5.794130544993763898, 7.853181283949808744, 1.599625672291269396 ) ) ;
#16042 = CARTESIAN_POINT ( 'NONE',  ( 1.001543065824772753E-15, -2.909374999522043925, 3.793834371823811669 ) ) ;
#16043 = CARTESIAN_POINT ( 'NONE',  ( 0.1331565106231571705, 2.881392620029461504, -2.434650611646618223 ) ) ;
#16044 = CARTESIAN_POINT ( 'NONE',  ( 4.915489835137424102, -0.9894786724786635013, -1.552603174752004600 ) ) ;
#16045 = AXIS2_PLACEMENT_3D ( 'NONE', #96032, #28875, #179401 ) ;
#16046 = CARTESIAN_POINT ( 'NONE',  ( 5.515469562660962666, 5.329135999392899947, 0.7998128361456341429 ) ) ;
#16047 = CARTESIAN_POINT ( 'NONE',  ( 2.080655396751258213, -0.08067463971387846267, -1.723007254337567407 ) ) ;
#16048 = CARTESIAN_POINT ( 'NONE',  ( 0.005092704479254389627, -0.09411098085002241043, 2.014433268766747887 ) ) ;
#16049 = CARTESIAN_POINT ( 'NONE',  ( 2.391599454647721945, -0.8833308501894185927, -2.122370812339502422 ) ) ;
#16050 = CARTESIAN_POINT ( 'NONE',  ( -1.364683531250010295, 3.842708333674751398, 0.7879004041258379498 ) ) ;
#16051 = CARTESIAN_POINT ( 'NONE',  ( 1.300488321244117618, -2.262578820359177012, 9.798025588786393801E-05 ) ) ;
#16052 = CARTESIAN_POINT ( 'NONE',  ( 3.862027066150780730, 2.090197335813360979, -0.2575193119012611498 ) ) ;
#16053 = CARTESIAN_POINT ( 'NONE',  ( -5.171509248969888617, 4.998125310078441075, 0.7998128361456281477 ) ) ;
#16054 = CARTESIAN_POINT ( 'NONE',  ( 2.002845679596281681, 1.468101958376843985, 0.9879206967360052438 ) ) ;
#16055 = CARTESIAN_POINT ( 'NONE',  ( 5.276094334012385367, 9.307193822989793475, 1.040834085586084257E-14 ) ) ;
#16056 = CARTESIAN_POINT ( 'NONE',  ( 5.275531169048895741, 7.248148678680751189, -1.443375672974078761 ) ) ;
#16057 = CARTESIAN_POINT ( 'NONE',  ( -5.762378981008047241, 6.681529218386182301, 1.199719254218450271 ) ) ;
#16058 = CARTESIAN_POINT ( 'NONE',  ( 6.792271770322100721, 7.026664608238323950, -0.7216878364870257245 ) ) ;
#16059 = CARTESIAN_POINT ( 'NONE',  ( 1.499999999999989120, 2.775000000000020339, 1.214306433183764966E-14 ) ) ;
#16060 = CARTESIAN_POINT ( 'NONE',  ( 4.834350099735578610, -1.189287197132185669, -1.876079791293260079 ) ) ;
#16061 = CARTESIAN_POINT ( 'NONE',  ( 3.837968455498752096, 2.180838135830205804, 0.2153102754597763235 ) ) ;
#16062 = CARTESIAN_POINT ( 'NONE',  ( -4.415151579544611238, 8.302760609444034046, -0.7998128361456281477 ) ) ;
#16063 = CARTESIAN_POINT ( 'NONE',  ( -3.851398154733808088, 6.650992392901508232, -1.199719254218450271 ) ) ;
#16064 = FACE_OUTER_BOUND ( 'NONE', #158643, .T. ) ;
#16065 = CARTESIAN_POINT ( 'NONE',  ( 1.364683531249988535, 3.363541667008084879, 0.7879004041258500513 ) ) ;
#16066 = CARTESIAN_POINT ( 'NONE',  ( 6.890000000000025437, 1.315307137738566556, 1.839292676857922304 ) ) ;
#16067 = CARTESIAN_POINT ( 'NONE',  ( -3.714570900464290393, 5.356752022006865843, 1.443375672974064550 ) ) ;
#16068 = CARTESIAN_POINT ( 'NONE',  ( 5.906510592826289319, -2.110524776404258507, -0.2060971850248518311 ) ) ;
#16069 = CARTESIAN_POINT ( 'NONE',  ( -6.129694847154211423, 9.205042184104968328, -1.082531754730549967 ) ) ;
#16070 = ORIENTED_EDGE ( 'NONE', *, *, #32218, .T. ) ;
#16072 = CARTESIAN_POINT ( 'NONE',  ( -1.451998047843676476, 7.315968950353781253, 4.301760722578348073 ) ) ;
#16071 = CARTESIAN_POINT ( 'NONE',  ( -5.234856708652269042, 7.200695141551334721, 1.443375672974058777 ) ) ;
#16073 = CARTESIAN_POINT ( 'NONE',  ( 3.845709127770629010, 7.638411082374393146, 0.7998128361456321445 ) ) ;
#16074 = CARTESIAN_POINT ( 'NONE',  ( 0.7499999999999885647, 3.066666666666689522, -1.299038105676658228 ) ) ;
#16075 = CARTESIAN_POINT ( 'NONE',  ( -0.7500000000000006661, 9.489583334016129967, -1.299038105676657340 ) ) ;
#16076 = DIRECTION ( 'NONE',  ( 0.000000000000000000, 1.000000000000000000, 0.000000000000000000 ) ) ;
#16077 = CARTESIAN_POINT ( 'NONE',  ( -1.364683531250010295, 3.842708333674751398, 0.7879004041258379498 ) ) ;
#16078 = CARTESIAN_POINT ( 'NONE',  ( 1.522608870468153741, -1.638875412371978646, 0.5861679430564836757 ) ) ;
#16079 = CARTESIAN_POINT ( 'NONE',  ( 3.195971524519376494, 4.751719416737803847, -1.599625672291262513 ) ) ;
#16080 = CARTESIAN_POINT ( 'NONE',  ( -9.578928831967228774, -10.00000000000000178, 0.1215685829351347697 ) ) ;
#16081 = CARTESIAN_POINT ( 'NONE',  ( -1.364683531250012516, 0.5927083336747520637, 0.7879004041258379498 ) ) ;
#16082 = CARTESIAN_POINT ( 'NONE',  ( -0.3728825314829133375, 3.227879828479718327, -0.5317689764002342390 ) ) ;
#16083 = CARTESIAN_POINT ( 'NONE',  ( 6.385629968321593353, 1.486944277142748572, 1.569300510047972219 ) ) ;
#16084 = CARTESIAN_POINT ( 'NONE',  ( -2.937312835655025101, 6.578615408239493867, 1.040834085586084257E-14 ) ) ;
#16085 = CARTESIAN_POINT ( 'NONE',  ( -5.816084710138169633, 8.768887347594400694, 1.082531754730548412 ) ) ;
#16086 = CARTESIAN_POINT ( 'NONE',  ( 6.209879897626497502, -2.145988306206991325, 0.2596296833028768347 ) ) ;
#16088 = EDGE_LOOP ( 'NONE', ( #104066, #153254, #75735 ) ) ;
#16087 = CARTESIAN_POINT ( 'NONE',  ( -3.149236820124241110, 6.896136400112061970, -0.7998128361456481317 ) ) ;
#16089 = CARTESIAN_POINT ( 'NONE',  ( -1.364683531250012516, 3.238541667008084879, -0.7879004041258289570 ) ) ;
#16090 = CARTESIAN_POINT ( 'NONE',  ( 5.571542166969843279, 1.900665388187183114, -0.5230325980125193341 ) ) ;
#16091 = CARTESIAN_POINT ( 'NONE',  ( 4.885968428070557756, -0.08385511083567295798, 1.731956597358391470 ) ) ;
#16093 = CARTESIAN_POINT ( 'NONE',  ( 2.226364491882920404, 2.126620374013419301, 0.5291077681483095096 ) ) ;
#16092 = CARTESIAN_POINT ( 'NONE',  ( -1.360316468750024876, -0.5885416663252728275, 0.7853790794158701516 ) ) ;
#16094 = CARTESIAN_POINT ( 'NONE',  ( 3.188805362043587888, -2.273175341261697291, -0.3962186847288259317 ) ) ;
#16095 = CARTESIAN_POINT ( 'NONE',  ( 4.446593522994434444, 0.5459629501111874506, 1.987092823586662504 ) ) ;
#16096 = CARTESIAN_POINT ( 'NONE',  ( 0.2693405865131668353, 1.117251289913205881, 1.588187351064213715 ) ) ;
#16097 = CARTESIAN_POINT ( 'NONE',  ( -6.927853306458756855, 9.105581495667113501, 1.443375672974078761 ) ) ;
#16098 = PRODUCT_DEFINITION_SHAPE ( 'NONE', 'NONE',  #214431 ) ;
#16099 = CARTESIAN_POINT ( 'NONE',  ( -3.657667580636712934, 7.489305620709952649, -0.7998128361456481317 ) ) ;
#16100 = CARTESIAN_POINT ( 'NONE',  ( 4.650083499807235121, 5.295740330745369207, 1.082471891955963716 ) ) ;
#16101 = CARTESIAN_POINT ( 'NONE',  ( 3.639029512587122372, 2.014767915268770082, 0.6618469929612482705 ) ) ;
#16102 = CARTESIAN_POINT ( 'NONE',  ( 0.000000000000000000, 6.999999999999999112, 0.000000000000000000 ) ) ;
#16103 = CARTESIAN_POINT ( 'NONE',  ( 0.8443752267504719411, 0.3905955241953715795, -1.978051186352240309 ) ) ;
#16104 = CARTESIAN_POINT ( 'NONE',  ( -6.033015167956805591, 8.061603667414825480, -1.443375672974058777 ) ) ;
#16105 = CARTESIAN_POINT ( 'NONE',  ( 4.946401613871811875, 2.200551846729232430, 0.1665617540023768828 ) ) ;
#16106 = CARTESIAN_POINT ( 'NONE',  ( 3.285556943750000070, -0.7218749995220423710, 0.000000000000000000 ) ) ;
#16107 = CARTESIAN_POINT ( 'NONE',  ( -7.750016138724920900, -6.480061791515684178, 7.806764249273700607 ) ) ;
#16108 = CARTESIAN_POINT ( 'NONE',  ( -8.086512275908061653, 8.398962174839683215, 0.000000000000000000 ) ) ;
#16111 = CONICAL_SURFACE ( 'NONE', #68053, 4.000000000000000000, 0.8960553845713404852 ) ;
#16110 = DIRECTION ( 'NONE',  ( 0.000000000000000000, 1.000000000000000000, 0.000000000000000000 ) ) ;
#16109 = CARTESIAN_POINT ( 'NONE',  ( -5.072456052330698739, 7.961014115122230450, -1.198640345919316674 ) ) ;
#16112 = DIRECTION ( 'NONE',  ( 0.000000000000000000, 8.546850786086437571E-32, 1.000000000000000000 ) ) ;
#16113 = EDGE_LOOP ( 'NONE', ( #16490, #12251, #70332, #82896 ) ) ;
#16114 = CARTESIAN_POINT ( 'NONE',  ( 4.012614562483146408, 1.458688259485216854, -1.456115939812257620 ) ) ;
#16115 = CARTESIAN_POINT ( 'NONE',  ( -1.360316468750013108, 1.390625000341414008, -3.469446951953614189E-15 ) ) ;
#16116 = UNCERTAINTY_MEASURE_WITH_UNIT (LENGTH_MEASURE( 1.000000000000000082E-05 ), #64787, 'distance_accuracy_value', 'NONE');
#16117 = CARTESIAN_POINT ( 'NONE',  ( -5.915435094264120508, 5.795762452929912101, 0.000000000000000000 ) ) ;
#16118 = CARTESIAN_POINT ( 'NONE',  ( 3.668621814757520916, 0.7290426041848938610, 1.883679974206926122 ) ) ;
#16119 = CARTESIAN_POINT ( 'NONE',  ( 0.7499999999999885647, -0.7666666666666446250, 1.299038105676657340 ) ) ;
#16120 = CARTESIAN_POINT ( 'NONE',  ( 2.171277156482887882, 5.684907115872006145, -0.7998128361456291469 ) ) ;
#16121 = CARTESIAN_POINT ( 'NONE',  ( 8.444030743212801227, 8.745790710036752458, 0.7998128361456462443 ) ) ;
#16122 = CARTESIAN_POINT ( 'NONE',  ( 2.852473085487742477, 0.6931051061056427987, 1.940986274177344706 ) ) ;
#16123 = CARTESIAN_POINT ( 'NONE',  ( 4.111308439460083619, 3.971718457827854376, 0.3900462783498518937 ) ) ;
#16124 = CARTESIAN_POINT ( 'NONE',  ( 4.843287188579786573, 6.673587691474970107, -1.599625672291256295 ) ) ;
#16125 = CARTESIAN_POINT ( 'NONE',  ( -0.2409995289980003397, 2.873648158547074338, -2.488896373646624749 ) ) ;
#16126 = CARTESIAN_POINT ( 'NONE',  ( 1.640310086786896049, -1.556016536173940645, 0.9838780322720328542 ) ) ;
#16127 = CARTESIAN_POINT ( 'NONE',  ( 6.721333373144884327, -0.1645177889858795151, 2.170883633896856679 ) ) ;
#16128 = CARTESIAN_POINT ( 'NONE',  ( 5.956828388357757298, 8.042995434541133193, 1.599625672291269396 ) ) ;
#16129 = CARTESIAN_POINT ( 'NONE',  ( 0.9136071317731933039, -0.3180670004044767740, 2.137961049616762921 ) ) ;
#16130 = CARTESIAN_POINT ( 'NONE',  ( -4.460269349215930212, 4.305995116947750390, 1.214306433183764966E-14 ) ) ;
#16131 = CARTESIAN_POINT ( 'NONE',  ( 2.237517880698642880, 0.5331670712399002587, -1.944730990508992008 ) ) ;
#16132 = AXIS2_PLACEMENT_3D ( 'NONE', #53453, #200745, #84886 ) ;
#16133 = CARTESIAN_POINT ( 'NONE',  ( -6.143440778383317813, 6.339971461045375456, 7.509178883279419847E-06 ) ) ;
#16134 = CARTESIAN_POINT ( 'NONE',  ( 0.3560485870845608858, 0.7116971694140910021, 1.730184004908103867 ) ) ;
#16135 = CARTESIAN_POINT ( 'NONE',  ( 4.768415704089838947, -1.288333767974993327, 1.492341041399107393 ) ) ;
#16136 = AXIS2_PLACEMENT_3D ( 'NONE', #83388, #118101, #149472 ) ;
#16137 = CARTESIAN_POINT ( 'NONE',  ( 4.452361426671761713, -1.313546101436880109, 1.530156479064001207 ) ) ;
#16139 = CARTESIAN_POINT ( 'NONE',  ( 9.612367721964607981, 12.23751498042398289, -1.443375672974058777 ) ) ;
#16138 = CARTESIAN_POINT ( 'NONE',  ( 1.364683531249988757, 2.384375000341422357, 1.214306433183764966E-14 ) ) ;
#16141 = CARTESIAN_POINT ( 'NONE',  ( 6.041652760897754604, -1.524265013729691143, -1.453574456173498231 ) ) ;
#16140 = CARTESIAN_POINT ( 'NONE',  ( -6.551614543901706611, 8.666636272683888365, 1.599625672291283607 ) ) ;
#16142 = CARTESIAN_POINT ( 'NONE',  ( 5.353992430378140099, -0.7485205528568983357, 1.930488744064068785 ) ) ;
#16143 = CARTESIAN_POINT ( 'NONE',  ( 7.305145839664861640, 7.417091655897478653, 0.7998128361456341429 ) ) ;
#16144 = CARTESIAN_POINT ( 'NONE',  ( -6.911959384868566758, 6.958374125301778790, 1.040834085586084257E-14 ) ) ;
#16145 = CARTESIAN_POINT ( 'NONE',  ( 6.539320575229258026, 7.052651068779801413, 2.601414540040230428 ) ) ;
#16146 = CARTESIAN_POINT ( 'NONE',  ( 5.642833896779382741, 1.947644361699039983, 0.5348221497712030148 ) ) ;
#16147 = CARTESIAN_POINT ( 'NONE',  ( -0.7500000000000249800, -1.027083332650516212, 1.299038105676659116 ) ) ;
#16148 = CARTESIAN_POINT ( 'NONE',  ( 2.860362167425280600, 2.296499369387979606, -0.2270692390979132391 ) ) ;
#16149 = CARTESIAN_POINT ( 'NONE',  ( 1.498963261266316183, 0.3983865470186908064, 2.023570823014529729 ) ) ;
#16150 = CARTESIAN_POINT ( 'NONE',  ( 7.456621297836072415, 9.722477485607340597, 1.443375672974076540 ) ) ;
#16151 = CARTESIAN_POINT ( 'NONE',  ( 6.047819040147648373, 9.213483425884394507, 1.199719254218452047 ) ) ;
#16152 = CARTESIAN_POINT ( 'NONE',  ( 5.200434439293556643, 8.224868058221247225, -1.199719254218452047 ) ) ;
#16153 = CARTESIAN_POINT ( 'NONE',  ( -1.402160292154681736E-14, 0.7593750003414168059, -1.575800808251659024 ) ) ;
#16154 = CARTESIAN_POINT ( 'NONE',  ( 4.553559489343365740, 6.405848385690952718, -1.599625672291269396 ) ) ;
#16155 = CARTESIAN_POINT ( 'NONE',  ( 7.117667457050084856, 7.406292909420979953, -0.7216878364870257245 ) ) ;
#16157 = FILL_AREA_STYLE_COLOUR ( '', #55709 ) ;
#16156 = CARTESIAN_POINT ( 'NONE',  ( 4.580651514471745678, 1.339088007528920210, -1.708959110978137019 ) ) ;
#16159 = CARTESIAN_POINT ( 'NONE',  ( 2.806014743833367131, 1.331929863061011465, -1.271513748034671654 ) ) ;
#16158 = CARTESIAN_POINT ( 'NONE',  ( -4.934804725694231564, 5.819988937140460727, -1.082531754730544860 ) ) ;
#16160 = EDGE_CURVE ( 'NONE', #79990, #211004, #116451, .T. ) ;
#16161 = CARTESIAN_POINT ( 'NONE',  ( 1.364683531249990311, 4.863541667008084879, 0.7879004041258500513 ) ) ;
#16162 = CARTESIAN_POINT ( 'NONE',  ( 4.493798347139664529, -2.191065130646638437, -0.05333993539427539510 ) ) ;
#16163 = CARTESIAN_POINT ( 'NONE',  ( 8.589851454039761691, 13.83000113107204143, 8.380017385823880005 ) ) ;
#16164 = CARTESIAN_POINT ( 'NONE',  ( 6.315309700038255869, -0.2845791475536703086, 2.244501093609466924 ) ) ;
#16165 = CARTESIAN_POINT ( 'NONE',  ( -5.688173390364544169, 6.286868445634342883, -1.126660468825124273 ) ) ;
#16166 = CARTESIAN_POINT ( 'NONE',  ( 5.213898493288036562, 7.712005038449616379, -1.200564631081424416 ) ) ;
#16167 = CARTESIAN_POINT ( 'NONE',  ( -5.356880090730904875, 7.343055753976412525, 1.443375672974058777 ) ) ;
#16168 = CARTESIAN_POINT ( 'NONE',  ( 4.963693636378940788, 5.923969009597785274, -1.082531754730548412 ) ) ;
#16169 = CARTESIAN_POINT ( 'NONE',  ( 6.468005306911782881, 0.9119784028226736172, 1.516475106587056532 ) ) ;
#16170 = STYLED_ITEM ( 'NONE', ( #130869 ), #100155 ) ;
#16171 = CARTESIAN_POINT ( 'NONE',  ( 4.688143804000614701, 1.160868117455503556, 1.644480612105477579 ) ) ;
#16172 = CARTESIAN_POINT ( 'NONE',  ( 8.308449207076147758, 8.587612251210650527, -0.7998128361456281477 ) ) ;
#16173 = CARTESIAN_POINT ( 'NONE',  ( 2.731583703245387351, -1.965451047913500116, 0.7568412939000405126 ) ) ;
#16174 = CARTESIAN_POINT ( 'NONE',  ( 1.950665421479770067, -1.752291233380006474, -0.7743663792006536539 ) ) ;
#16175 = CARTESIAN_POINT ( 'NONE',  ( 4.172158584703322681, 5.890604320285754980, -1.599625672291256295 ) ) ;
#16176 = CARTESIAN_POINT ( 'NONE',  ( 3.262113425008953183, -1.967426182293503079, 0.09390151542597660606 ) ) ;
#16177 = CARTESIAN_POINT ( 'NONE',  ( 4.834242814930416188, -1.083969679716361156, -1.704088710659272810 ) ) ;
#16178 = CARTESIAN_POINT ( 'NONE',  ( 0.1626889888870358680, -1.668787113083155305, -0.8454427722031019332 ) ) ;
#16179 = CARTESIAN_POINT ( 'NONE',  ( 0.7132427667453158371, -1.655377960257615966, -1.052639099659122390 ) ) ;
#16181 = ORIENTED_EDGE ( 'NONE', *, *, #66045, .T. ) ;
#16180 = CARTESIAN_POINT ( 'NONE',  ( 0.2637284958507991606, 0.5978344860198721022, -1.816641584731902626 ) ) ;
#16182 = CARTESIAN_POINT ( 'NONE',  ( 6.019457014787495730, 6.125047393447951016, -0.7216878364870257245 ) ) ;
#16183 = AXIS2_PLACEMENT_3D ( 'NONE', #190347, #194622, #77675 ) ;
#16184 = CARTESIAN_POINT ( 'NONE',  ( -1.364683531250014514, 0.3427083336747508424, 0.7879004041258379498 ) ) ;
#16185 = CARTESIAN_POINT ( 'NONE',  ( 5.893391625361732444, 1.417579469995243091, 1.220656814419220249 ) ) ;
#16186 = CARTESIAN_POINT ( 'NONE',  ( 10.05353459973327368, 11.68787744023238417, -1.199719254218440723 ) ) ;
#16187 = CARTESIAN_POINT ( 'NONE',  ( -4.517335436343488553, 8.499999999999996447, 0.7749999999999996891 ) ) ;
#16188 = CARTESIAN_POINT ( 'NONE',  ( 6.977413707831522593, -0.1558467299303326059, 2.036386162850227333 ) ) ;
#16189 = CARTESIAN_POINT ( 'NONE',  ( 0.000000000000000000, 0.000000000000000000, 0.4894596299587841703 ) ) ;
#16190 = EDGE_CURVE ( 'NONE', #161612, #60255, #19521, .T. ) ;
#16191 = CARTESIAN_POINT ( 'NONE',  ( 0.7837444799244470683, -1.966470238067185905, 0.6478734989143407619 ) ) ;
#16192 = CARTESIAN_POINT ( 'NONE',  ( -1.402160292154681736E-14, 1.837500000000019895, -1.732050807568863648 ) ) ;
#16193 = CARTESIAN_POINT ( 'NONE',  ( 6.962275575817444384, 8.081408578997208991, -1.199719254218446718 ) ) ;
#16194 = CARTESIAN_POINT ( 'NONE',  ( -7.527801604085656351, 9.805521176231838609, 1.599625672291295375 ) ) ;
#16195 = CARTESIAN_POINT ( 'NONE',  ( 5.228604516725597229, 6.129068686715179126, -1.199719254218450271 ) ) ;
#16196 = CARTESIAN_POINT ( 'NONE',  ( 5.795592431653455279, 1.959276243578732091, -0.8114611383256833399 ) ) ;
#16197 = CARTESIAN_POINT ( 'NONE',  ( 3.736153849017632922, 6.516540702899320081, -1.199719254218453823 ) ) ;
#16198 = CARTESIAN_POINT ( 'NONE',  ( 1.364683531249988535, 1.363541667008083769, 0.7879004041258500513 ) ) ;
#16199 = CARTESIAN_POINT ( 'NONE',  ( -1.500000000000013101, 2.379166666666686414, -0.8660254037844313801 ) ) ;
#16201 = CARTESIAN_POINT ( 'NONE',  ( 3.659811400685081040, 6.357198169852855685, -1.199719254218446718 ) ) ;
#16200 = CARTESIAN_POINT ( 'NONE',  ( 5.986763597034562068, 1.890319730748804439, 0.5246630281777532323 ) ) ;
#16202 = CARTESIAN_POINT ( 'NONE',  ( 4.850935385407137979, -0.9528642855485233154, 1.776740034556321568 ) ) ;
#16203 = CARTESIAN_POINT ( 'NONE',  ( 3.590956263468424225, 1.645886154840708659, 0.9800325279442632098 ) ) ;
#16204 = CARTESIAN_POINT ( 'NONE',  ( -1.001543065824772872E-14, 4.493750000682820378, 1.732050807568877637 ) ) ;
#16205 = CARTESIAN_POINT ( 'NONE',  ( 1.259612756803454303, 2.158328104161820526, -0.3793702838810894540 ) ) ;
#16206 = CARTESIAN_POINT ( 'NONE',  ( 0.2331713839410602396, 7.629137130509072939, -2.553349835631549603 ) ) ;
#16207 = CARTESIAN_POINT ( 'NONE',  ( 3.497188413392815498, 1.472618687456558773, 1.153256759092120554 ) ) ;
#16208 = CARTESIAN_POINT ( 'NONE',  ( -1.402160292154681736E-14, -0.006249999317184824418, 1.732050807568877637 ) ) ;
#16209 = CARTESIAN_POINT ( 'NONE',  ( -6.509886312855995172, 10.74661779830734254, -0.7998128361456291469 ) ) ;
#16211 = CARTESIAN_POINT ( 'NONE',  ( 5.079753589751704546, -0.7609352437839884686, 1.975942822842210234 ) ) ;
#16210 = CARTESIAN_POINT ( 'NONE',  ( -3.606105671554953318, 7.150947683548662503, 0.7216878364870317197 ) ) ;
#16212 = CARTESIAN_POINT ( 'NONE',  ( -1.364683531250014514, 8.901041667008069425, -0.7879004041258335089 ) ) ;
#16213 = CARTESIAN_POINT ( 'NONE',  ( 6.725056259267968350, -1.891221747171191403, -0.8428681758992571105 ) ) ;
#16215 = CARTESIAN_POINT ( 'NONE',  ( 4.008199524592567897, 7.584238231759597326, 0.2402771892247856922 ) ) ;
#16214 = CARTESIAN_POINT ( 'NONE',  ( 2.876600747729184615, -0.1562720264073799992, -2.084980456524800019 ) ) ;
#16217 = ORIENTED_EDGE ( 'NONE', *, *, #910, .T. ) ;
#16216 = CARTESIAN_POINT ( 'NONE',  ( 1.148929321228649991, -1.355925326379325391, -1.065857193176344309 ) ) ;
#16218 = CARTESIAN_POINT ( 'NONE',  ( 5.750629710490689384, 9.860818428881154674, -0.7998128361456291469 ) ) ;
#16219 = CARTESIAN_POINT ( 'NONE',  ( -1.500000000000001110, 12.05208333401613174, 0.8660254037844418162 ) ) ;
#16220 = DIRECTION ( 'NONE',  ( 0.000000000000000000, 1.000000000000000000, 0.000000000000000000 ) ) ;
#16221 = CARTESIAN_POINT ( 'NONE',  ( 6.773846765316601903, -7.473374494057218875, -6.773846765316623220 ) ) ;
#16223 = CARTESIAN_POINT ( 'NONE',  ( 8.798878505144646311, 11.28844422746735532, -1.443375672974052559 ) ) ;
#16222 = CARTESIAN_POINT ( 'NONE',  ( 7.253775878511261155, 8.421492265473332850, 1.199719254218462483 ) ) ;
#16224 = DIRECTION ( 'NONE',  ( 0.000000000000000000, -1.000000000000000000, 0.000000000000000000 ) ) ;
#16226 = CARTESIAN_POINT ( 'NONE',  ( 1.805022944457121081, 1.575911691392884117, -0.8931387472532796856 ) ) ;
#16225 = CARTESIAN_POINT ( 'NONE',  ( 6.042093733545556233, 7.078139439671806699, -1.199719254218452047 ) ) ;
#16227 = CARTESIAN_POINT ( 'NONE',  ( -5.520141099058386125, 9.591915048876776595, 0.000000000000000000 ) ) ;
#16228 = CARTESIAN_POINT ( 'NONE',  ( 3.330499290451326200, 7.037332938835193730, -0.7998128361456291469 ) ) ;
#16229 = CARTESIAN_POINT ( 'NONE',  ( -6.486760921661624657, 6.767311426390788753, 0.2083394120615672529 ) ) ;
#16230 = CARTESIAN_POINT ( 'NONE',  ( 4.712340909201580885, 7.655425606447271214, -1.199719254218452047 ) ) ;
#16231 = ADVANCED_FACE ( 'NONE', ( #169411 ), #87092, .T. ) ;
#16232 = CARTESIAN_POINT ( 'NONE',  ( 0.000000000000000000, -0.5000000000000004441, 0.000000000000000000 ) ) ;
#16233 = LINE ( 'NONE', #148410, #62770 ) ;
#16234 = CARTESIAN_POINT ( 'NONE',  ( -11.43190902327453529, 11.15522128257853396, 3.649704988378119186 ) ) ;
#16235 = CARTESIAN_POINT ( 'NONE',  ( 8.242994207428692377, 12.56065097540143327, -0.7216878364870328300 ) ) ;
#16236 = VERTEX_POINT ( 'NONE', #100143 ) ;
#16237 = CARTESIAN_POINT ( 'NONE',  ( 3.385049140913086507, 0.04320281034062402326, 1.860716667189839635 ) ) ;
#16238 = CARTESIAN_POINT ( 'NONE',  ( 0.03459428079104728826, -1.538086888106354522, 1.141608027856432450 ) ) ;
#16239 = CARTESIAN_POINT ( 'NONE',  ( 6.247092716751994068, -1.627016005604764670, 1.031123616215999794 ) ) ;
#16240 = CARTESIAN_POINT ( 'NONE',  ( -1.844607821789273627, 8.931289555339859021, 0.7750000000000013545 ) ) ;
#16241 = CARTESIAN_POINT ( 'NONE',  ( 4.743613802917549194, 8.193193991156523026, -0.7244234545457691743 ) ) ;
#16242 = CARTESIAN_POINT ( 'NONE',  ( -3.280709984826970516, 6.771319382366015383, 0.7216878364870317197 ) ) ;
#16243 = CARTESIAN_POINT ( 'NONE',  ( 9.259855728453651125, 9.905512559391842942, 1.040834085586084257E-14 ) ) ;
#16244 = CARTESIAN_POINT ( 'NONE',  ( 4.715651637508523564, 0.4355733895117944177, -1.920488317121961108 ) ) ;
#16245 = CARTESIAN_POINT ( 'NONE',  ( 1.910938629679886480, -0.5684797485801665884, -2.042784538176869003 ) ) ;
#16246 = CARTESIAN_POINT ( 'NONE',  ( -4.720210035852093533, 8.658662141802762946, -0.7998128361456281477 ) ) ;
#16247 = CARTESIAN_POINT ( 'NONE',  ( -10.56141428364488277, 5.615930626961760375, 5.603115303083649579 ) ) ;
#16248 = CARTESIAN_POINT ( 'NONE',  ( 9.488725015150309972, -6.691474851359264342, -0.09393477316944856548 ) ) ;
#16249 = B_SPLINE_CURVE_WITH_KNOTS ( 'NONE', 3,
 ( #178446, #75603, #127646, #207724 ),
 .UNSPECIFIED., .F., .F.,
 ( 4, 4 ),
 ( 0.000000000000000000, 0.0007717018656778088046 ),
 .UNSPECIFIED. ) ;
#16250 = CARTESIAN_POINT ( 'NONE',  ( 5.419949545929089396, 1.307550890958172785, -1.758484179531449421 ) ) ;
#16251 = CARTESIAN_POINT ( 'NONE',  ( -1.500000000000008216, 10.03125000068279959, 3.469446951953614189E-15 ) ) ;
#16252 = CARTESIAN_POINT ( 'NONE',  ( 4.243131921826915232, -1.676359970754065731, 0.9489593035170663660 ) ) ;
#16253 = CARTESIAN_POINT ( 'NONE',  ( -7.542413527904030524, 7.693903958843159252, 1.040834085586084257E-14 ) ) ;
#16254 = CARTESIAN_POINT ( 'NONE',  ( 0.4811275135914867551, 1.705355465787803171, -0.6520327999673739550 ) ) ;
#16255 = CARTESIAN_POINT ( 'NONE',  ( 0.5224629442122545875, -1.184049029929446828, -1.862174541895258217 ) ) ;
#16256 = ORIENTED_EDGE ( 'NONE', *, *, #150960, .T. ) ;
#16258 =( BOUNDED_SURFACE ( )  B_SPLINE_SURFACE ( 1, 2, ( 
 ( #117421, #66437, #132579, #118489, #103245, #202844, #1439, #199650, #183418, #35021, #86986, #119553, #120637, #167179, #38241, #18768, #153057, #150942, #2505, #52360, #7855, #190872, #154130, #138961, #8931, #59822, #41466, #42538, #123852, #89144, #5700, #155198, #108641, #187678, #9996, #56628, #172520, #203912, #107575, #173609, #122792, #188751, #40390, #206060, #174669, #141121, #25182, #73941, #191932, #71777, #106494, #140036, #104315, #170364, #207132, #21948, #75011, #204983, #6779, #137893, #24105, #90208, #156272, #158398, #142173, #92361, #57695, #189816, #91283, #157342, #121714, #88058, #58757, #124909, #105401, #26242, #76073, #171439, #72854, #39306, #208189, #125975, #55559, #23029, #78200, #95556, #177853, #81404, #60887, #144325, #196230, #159454, #127047, #77133, #161607, #28389, #212451, #79273, #47872, #130237, #175720, #80336, #65130, #109715, #163735, #11052, #46799, #110774, #30538, #147487, #64095, #146438, #145391, #213509, #96618, #29465, #179980, #45730, #113983, #31601, #61961, #13197, #112912, #94485, #143254, #97677, #211389, #63017, #129186, #195164, #209243, #193007, #15316, #44660, #43596, #131288, #176774, #178923, #160523, #194078, #12128, #27312, #162672, #93417, #14242, #210324, #128118, #111849, #200460, #198331, #52106, #197275, #148547, #82458, #201521, #113, #32651, #36906, #16379, #167986, #181035, #118234, #184218, #3321, #169046, #4381, #101920, #66180, #48915, #132325, #83524, #53169, #100843, #68326, #2250, #134457, #115035, #35841, #19591, #199394, #70453, #98729, #49971, #85664, #86732, #151750, #69390, #18522, #20643, #135498, #117163, #119297, #51040, #185283, #102988, #1189, #166928, #152802, #33712, #164787, #116090, #183166, #84600, #150688, #182081, #99789, #165855, #17440, #149606, #67253, #133388, #34770, #172264, #71527, #72604, #105142, #190615, #189563, #8674, #40128, #121456, #123598, #25988, #139779, #137638, #205806, #136568, #87806, #21694, #140858, #153879, #186354, #42273, #170108, #107315, #120379, #57437, #41208, #157085, #108386, #158150 ),
 ( #7596, #156008, #73680, #202589, #173339, #24919, #138704, #9743, #54241, #91023, #37989, #74756, #171182, #39056, #104061, #154943, #122535, #56371, #174411, #92096, #124658, #106238, #206872, #22772, #58503, #5448, #203657, #204721, #6527, #55307, #88889, #187427, #188496, #23851, #89958, #127870, #96361, #145124, #161346, #60627, #11869, #94229, #30275, #175467, #126790, #62754, #125718, #27053, #43340, #77946, #76872, #211130, #144067, #128914, #194895, #207937, #12927, #13992, #141925, #178663, #191679, #45468, #176522, #79008, #46533, #44402, #210062, #111585, #142992, #109460, #112654, #160267, #61702, #193820, #177595, #93160, #159197, #162415, #10798, #75817, #80076, #208991, #29207, #192745, #95297, #110522, #59559, #28133, #141557, #172959, #39743, #41902, #158831, #58126, #55993, #124285, #54925, #6142, #154566, #59186, #72212, #104755, #109082, #88504, #25612, #38676, #190244, #108013, #75444, #26684, #76500, #174039, #138319, #121077, #204335, #155628, #125341, #24538, #140483, #74382, #206495, #187044, #91724, #157775, #57061, #142611, #170804, #9373, #22395, #207564, #89579, #171875, #122144, #73287, #40827, #189190, #175097, #92786, #42972, #90646, #191304, #7213, #10428, #188112, #105848, #123225, #139390, #23471, #205423, #106936, #156707, #8297, #11500, #79703, #32028, #163107, #179356, #28830, #46165, #128552, #98114, #77571, #94918, #146871, #110146, #143694, #27759, #112279, #193460, #14687, #29902, #212893, #80783, #126410, #30978, #15751, #60253, #114410, #176159, #211823, #61330, #195601, #164165, #64525, #97053, #95987, #81835, #47236, #194517, #130670, #196658, #209686, #208619, #180410, #93855, #162039, #127489, #144756, #177216, #48299, #113351, #192372, #178295, #45104, #44028, #159893, #63460, #111214, #129614, #160967, #12557, #78631, #210767, #62387, #13630, #145818, #52048, #165798, #67193, #69327, #35782, #102925, #180972, #152738, #149545, #185219, #168986, #66121, #101858, #100783, #135437, #32595, #17382, #167926, #4320, #134396, #201459, #2188, #182022, #98671, #33652 ) ),
 .UNSPECIFIED., .F., .F., .F. ) 
 B_SPLINE_SURFACE_WITH_KNOTS ( ( 2, 2 ),
 ( 3, 2, 2, 2, 2, 2, 2, 2, 2, 2, 2, 2, 2, 2, 2, 2, 2, 2, 2, 2, 2, 2, 2, 2, 2, 2, 2, 2, 2, 2, 2, 2, 2, 2, 2, 2, 2, 2, 2, 2, 2, 2, 2, 2, 2, 2, 2, 2, 2, 2, 2, 2, 2, 2, 2, 2, 2, 2, 2, 2, 2, 2, 2, 2, 2, 2, 2, 2, 2, 2, 2, 2, 2, 2, 2, 2, 2, 2, 2, 2, 2, 2, 2, 2, 2, 2, 2, 2, 2, 2, 2, 2, 2, 2, 2, 2, 2, 2, 2, 2, 2, 2, 2, 2, 2, 2, 2, 2, 2, 2, 2, 2, 2, 2, 2, 2, 2, 2, 2, 2, 3 ),
 ( 0.000000000000000000, 1.000000000000000000 ),
 ( 0.000000000000000000, 0.008333333333333333218, 0.01666666666666666644, 0.02500000000000000139, 0.03333333333333333287, 0.04166666666666666435, 0.05000000000000000278, 0.05833333333333333426, 0.06666666666666666574, 0.07499999999999999722, 0.08333333333333332871, 0.09166666666666666019, 0.1000000000000000056, 0.1083333333333333370, 0.1166666666666666685, 0.1250000000000000000, 0.1333333333333333315, 0.1416666666666666630, 0.1499999999999999944, 0.1583333333333333259, 0.1666666666666666574, 0.1749999999999999889, 0.1833333333333333204, 0.1916666666666666796, 0.2000000000000000111, 0.2083333333333333426, 0.2166666666666666741, 0.2250000000000000056, 0.2333333333333333370, 0.2416666666666666685, 0.2500000000000000000, 0.2583333333333333592, 0.2666666666666666630, 0.2750000000000000222, 0.2833333333333333259, 0.2916666666666666852, 0.2999999999999999889, 0.3083333333333333481, 0.3166666666666666519, 0.3250000000000000111, 0.3333333333333333148, 0.3416666666666666741, 0.3499999999999999778, 0.3583333333333333370, 0.3666666666666666408, 0.3750000000000000000, 0.3833333333333333592, 0.3916666666666666630, 0.4000000000000000222, 0.4083333333333333259, 0.4166666666666666852, 0.4249999999999999889, 0.4333333333333333481, 0.4416666666666666519, 0.4500000000000000111, 0.4583333333333333148, 0.4666666666666666741, 0.4749999999999999778, 0.4833333333333333370, 0.4916666666666666408, 0.5000000000000000000, 0.5083333333333333037, 0.5166666666666667185, 0.5250000000000000222, 0.5333333333333333259, 0.5416666666666666297, 0.5500000000000000444, 0.5583333333333333481, 0.5666666666666666519, 0.5749999999999999556, 0.5833333333333333703, 0.5916666666666666741, 0.5999999999999999778, 0.6083333333333332815, 0.6166666666666666963, 0.6250000000000000000, 0.6333333333333333037, 0.6416666666666667185, 0.6500000000000000222, 0.6583333333333333259, 0.6666666666666666297, 0.6750000000000000444, 0.6833333333333333481, 0.6916666666666666519, 0.6999999999999999556, 0.7083333333333333703, 0.7166666666666666741, 0.7249999999999999778, 0.7333333333333332815, 0.7416666666666666963, 0.7500000000000000000, 0.7583333333333333037, 0.7666666666666667185, 0.7750000000000000222, 0.7833333333333333259, 0.7916666666666666297, 0.8000000000000000444, 0.8083333333333333481, 0.8166666666666666519, 0.8249999999999999556, 0.8333333333333333703, 0.8416666666666666741, 0.8499999999999999778, 0.8583333333333332815, 0.8666666666666666963, 0.8750000000000000000, 0.8833333333333333037, 0.8916666666666667185, 0.9000000000000000222, 0.9083333333333333259, 0.9166666666666666297, 0.9250000000000000444, 0.9333333333333333481, 0.9416666666666666519, 0.9499999999999999556, 0.9583333333333333703, 0.9666666666666666741, 0.9749999999999999778, 0.9833333333333332815, 0.9916666666666666963, 1.000000000000000000 ),
 .UNSPECIFIED. ) 
 GEOMETRIC_REPRESENTATION_ITEM ( )  RATIONAL_B_SPLINE_SURFACE ( (
 ( 1.000000000000000000, 0.8660254037844387076, 1.000000000000000000, 0.8660254037844387076, 1.000000000000000000, 0.8660254037844387076, 1.000000000000000000, 0.8660254037844387076, 1.000000000000000000, 0.8660254037844387076, 1.000000000000000000, 0.8660254037844387076, 1.000000000000000000, 0.8660254037844387076, 1.000000000000000000, 0.8660254037844387076, 1.000000000000000000, 0.8660254037844387076, 1.000000000000000000, 0.8660254037844387076, 1.000000000000000000, 0.8660254037844387076, 1.000000000000000000, 0.8660254037844387076, 1.000000000000000000, 0.8660254037844387076, 1.000000000000000000, 0.8660254037844387076, 1.000000000000000000, 0.8660254037844387076, 1.000000000000000000, 0.8660254037844387076, 1.000000000000000000, 0.8660254037844387076, 1.000000000000000000, 0.8660254037844387076, 1.000000000000000000, 0.8660254037844387076, 1.000000000000000000, 0.8660254037844387076, 1.000000000000000000, 0.8660254037844387076, 1.000000000000000000, 0.8660254037844387076, 1.000000000000000000, 0.8660254037844387076, 1.000000000000000000, 0.8660254037844387076, 1.000000000000000000, 0.8660254037844387076, 1.000000000000000000, 0.8660254037844387076, 1.000000000000000000, 0.8660254037844387076, 1.000000000000000000, 0.8660254037844387076, 1.000000000000000000, 0.8660254037844387076, 1.000000000000000000, 0.8660254037844387076, 1.000000000000000000, 0.8660254037844387076, 1.000000000000000000, 0.8660254037844387076, 1.000000000000000000, 0.8660254037844387076, 1.000000000000000000, 0.8660254037844387076, 1.000000000000000000, 0.8660254037844387076, 1.000000000000000000, 0.8660254037844387076, 1.000000000000000000, 0.8660254037844387076, 1.000000000000000000, 0.8660254037844387076, 1.000000000000000000, 0.8660254037844387076, 1.000000000000000000, 0.8660254037844387076, 1.000000000000000000, 0.8660254037844387076, 1.000000000000000000, 0.8660254037844387076, 1.000000000000000000, 0.8660254037844387076, 1.000000000000000000, 0.8660254037844387076, 1.000000000000000000, 0.8660254037844387076, 1.000000000000000000, 0.8660254037844387076, 1.000000000000000000, 0.8660254037844387076, 1.000000000000000000, 0.8660254037844387076, 1.000000000000000000, 0.8660254037844387076, 1.000000000000000000, 0.8660254037844387076, 1.000000000000000000, 0.8660254037844387076, 1.000000000000000000, 0.8660254037844387076, 1.000000000000000000, 0.8660254037844387076, 1.000000000000000000, 0.8660254037844387076, 1.000000000000000000, 0.8660254037844387076, 1.000000000000000000, 0.8660254037844387076, 1.000000000000000000, 0.8660254037844387076, 1.000000000000000000, 0.8660254037844387076, 1.000000000000000000, 0.8660254037844387076, 1.000000000000000000, 0.8660254037844387076, 1.000000000000000000, 0.8660254037844387076, 1.000000000000000000, 0.8660254037844387076, 1.000000000000000000, 0.8660254037844387076, 1.000000000000000000, 0.8660254037844387076, 1.000000000000000000, 0.8660254037844387076, 1.000000000000000000, 0.8660254037844387076, 1.000000000000000000, 0.8660254037844387076, 1.000000000000000000, 0.8660254037844387076, 1.000000000000000000, 0.8660254037844387076, 1.000000000000000000, 0.8660254037844387076, 1.000000000000000000, 0.8660254037844387076, 1.000000000000000000, 0.8660254037844387076, 1.000000000000000000, 0.8660254037844387076, 1.000000000000000000, 0.8660254037844387076, 1.000000000000000000, 0.8660254037844387076, 1.000000000000000000, 0.8660254037844387076, 1.000000000000000000, 0.8660254037844387076, 1.000000000000000000, 0.8660254037844387076, 1.000000000000000000, 0.8660254037844387076, 1.000000000000000000, 0.8660254037844387076, 1.000000000000000000, 0.8660254037844387076, 1.000000000000000000, 0.8660254037844387076, 1.000000000000000000, 0.8660254037844387076, 1.000000000000000000, 0.8660254037844387076, 1.000000000000000000, 0.8660254037844387076, 1.000000000000000000, 0.8660254037844387076, 1.000000000000000000, 0.8660254037844387076, 1.000000000000000000, 0.8660254037844387076, 1.000000000000000000, 0.8660254037844387076, 1.000000000000000000, 0.8660254037844387076, 1.000000000000000000, 0.8660254037844387076, 1.000000000000000000, 0.8660254037844387076, 1.000000000000000000, 0.8660254037844387076, 1.000000000000000000, 0.8660254037844387076, 1.000000000000000000, 0.8660254037844387076, 1.000000000000000000, 0.8660254037844387076, 1.000000000000000000, 0.8660254037844387076, 1.000000000000000000, 0.8660254037844387076, 1.000000000000000000, 0.8660254037844387076, 1.000000000000000000, 0.8660254037844387076, 1.000000000000000000, 0.8660254037844387076, 1.000000000000000000, 0.8660254037844387076, 1.000000000000000000, 0.8660254037844387076, 1.000000000000000000, 0.8660254037844387076, 1.000000000000000000, 0.8660254037844387076, 1.000000000000000000, 0.8660254037844387076, 1.000000000000000000, 0.8660254037844387076, 1.000000000000000000, 0.8660254037844387076, 1.000000000000000000, 0.8660254037844387076, 1.000000000000000000, 0.8660254037844387076, 1.000000000000000000, 0.8660254037844387076, 1.000000000000000000, 0.8660254037844387076, 1.000000000000000000, 0.8660254037844387076, 1.000000000000000000, 0.8660254037844387076, 1.000000000000000000, 0.8660254037844387076, 1.000000000000000000, 0.8660254037844387076, 1.000000000000000000, 0.8660254037844387076, 1.000000000000000000, 0.8660254037844387076, 1.000000000000000000, 0.8660254037844387076, 1.000000000000000000, 0.8660254037844387076, 1.000000000000000000),
 ( 1.000000000000000000, 0.8660254037844387076, 1.000000000000000000, 0.8660254037844387076, 1.000000000000000000, 0.8660254037844387076, 1.000000000000000000, 0.8660254037844387076, 1.000000000000000000, 0.8660254037844387076, 1.000000000000000000, 0.8660254037844387076, 1.000000000000000000, 0.8660254037844387076, 1.000000000000000000, 0.8660254037844387076, 1.000000000000000000, 0.8660254037844387076, 1.000000000000000000, 0.8660254037844387076, 1.000000000000000000, 0.8660254037844387076, 1.000000000000000000, 0.8660254037844387076, 1.000000000000000000, 0.8660254037844387076, 1.000000000000000000, 0.8660254037844387076, 1.000000000000000000, 0.8660254037844387076, 1.000000000000000000, 0.8660254037844387076, 1.000000000000000000, 0.8660254037844387076, 1.000000000000000000, 0.8660254037844387076, 1.000000000000000000, 0.8660254037844387076, 1.000000000000000000, 0.8660254037844387076, 1.000000000000000000, 0.8660254037844387076, 1.000000000000000000, 0.8660254037844387076, 1.000000000000000000, 0.8660254037844387076, 1.000000000000000000, 0.8660254037844387076, 1.000000000000000000, 0.8660254037844387076, 1.000000000000000000, 0.8660254037844387076, 1.000000000000000000, 0.8660254037844387076, 1.000000000000000000, 0.8660254037844387076, 1.000000000000000000, 0.8660254037844387076, 1.000000000000000000, 0.8660254037844387076, 1.000000000000000000, 0.8660254037844387076, 1.000000000000000000, 0.8660254037844387076, 1.000000000000000000, 0.8660254037844387076, 1.000000000000000000, 0.8660254037844387076, 1.000000000000000000, 0.8660254037844387076, 1.000000000000000000, 0.8660254037844387076, 1.000000000000000000, 0.8660254037844387076, 1.000000000000000000, 0.8660254037844387076, 1.000000000000000000, 0.8660254037844387076, 1.000000000000000000, 0.8660254037844387076, 1.000000000000000000, 0.8660254037844387076, 1.000000000000000000, 0.8660254037844387076, 1.000000000000000000, 0.8660254037844387076, 1.000000000000000000, 0.8660254037844387076, 1.000000000000000000, 0.8660254037844387076, 1.000000000000000000, 0.8660254037844387076, 1.000000000000000000, 0.8660254037844387076, 1.000000000000000000, 0.8660254037844387076, 1.000000000000000000, 0.8660254037844387076, 1.000000000000000000, 0.8660254037844387076, 1.000000000000000000, 0.8660254037844387076, 1.000000000000000000, 0.8660254037844387076, 1.000000000000000000, 0.8660254037844387076, 1.000000000000000000, 0.8660254037844387076, 1.000000000000000000, 0.8660254037844387076, 1.000000000000000000, 0.8660254037844387076, 1.000000000000000000, 0.8660254037844387076, 1.000000000000000000, 0.8660254037844387076, 1.000000000000000000, 0.8660254037844387076, 1.000000000000000000, 0.8660254037844387076, 1.000000000000000000, 0.8660254037844387076, 1.000000000000000000, 0.8660254037844387076, 1.000000000000000000, 0.8660254037844387076, 1.000000000000000000, 0.8660254037844387076, 1.000000000000000000, 0.8660254037844387076, 1.000000000000000000, 0.8660254037844387076, 1.000000000000000000, 0.8660254037844387076, 1.000000000000000000, 0.8660254037844387076, 1.000000000000000000, 0.8660254037844387076, 1.000000000000000000, 0.8660254037844387076, 1.000000000000000000, 0.8660254037844387076, 1.000000000000000000, 0.8660254037844387076, 1.000000000000000000, 0.8660254037844387076, 1.000000000000000000, 0.8660254037844387076, 1.000000000000000000, 0.8660254037844387076, 1.000000000000000000, 0.8660254037844387076, 1.000000000000000000, 0.8660254037844387076, 1.000000000000000000, 0.8660254037844387076, 1.000000000000000000, 0.8660254037844387076, 1.000000000000000000, 0.8660254037844387076, 1.000000000000000000, 0.8660254037844387076, 1.000000000000000000, 0.8660254037844387076, 1.000000000000000000, 0.8660254037844387076, 1.000000000000000000, 0.8660254037844387076, 1.000000000000000000, 0.8660254037844387076, 1.000000000000000000, 0.8660254037844387076, 1.000000000000000000, 0.8660254037844387076, 1.000000000000000000, 0.8660254037844387076, 1.000000000000000000, 0.8660254037844387076, 1.000000000000000000, 0.8660254037844387076, 1.000000000000000000, 0.8660254037844387076, 1.000000000000000000, 0.8660254037844387076, 1.000000000000000000, 0.8660254037844387076, 1.000000000000000000, 0.8660254037844387076, 1.000000000000000000, 0.8660254037844387076, 1.000000000000000000, 0.8660254037844387076, 1.000000000000000000, 0.8660254037844387076, 1.000000000000000000, 0.8660254037844387076, 1.000000000000000000, 0.8660254037844387076, 1.000000000000000000, 0.8660254037844387076, 1.000000000000000000, 0.8660254037844387076, 1.000000000000000000, 0.8660254037844387076, 1.000000000000000000, 0.8660254037844387076, 1.000000000000000000, 0.8660254037844387076, 1.000000000000000000, 0.8660254037844387076, 1.000000000000000000, 0.8660254037844387076, 1.000000000000000000, 0.8660254037844387076, 1.000000000000000000, 0.8660254037844387076, 1.000000000000000000, 0.8660254037844387076, 1.000000000000000000, 0.8660254037844387076, 1.000000000000000000, 0.8660254037844387076, 1.000000000000000000, 0.8660254037844387076, 1.000000000000000000, 0.8660254037844387076, 1.000000000000000000, 0.8660254037844387076, 1.000000000000000000, 0.8660254037844387076, 1.000000000000000000, 0.8660254037844387076, 1.000000000000000000, 0.8660254037844387076, 1.000000000000000000, 0.8660254037844387076, 1.000000000000000000, 0.8660254037844387076, 1.000000000000000000, 0.8660254037844387076, 1.000000000000000000) ) ) 
 REPRESENTATION_ITEM ( '' )  SURFACE ( )  );
#16257 = CARTESIAN_POINT ( 'NONE',  ( -2.788906526875773208E-15, 10.71875000068279604, -1.499999999999998446 ) ) ;
#16259 = ORIENTED_EDGE ( 'NONE', *, *, #137350, .F. ) ;
#16260 = CARTESIAN_POINT ( 'NONE',  ( 5.981301965652664698, -0.05197358493889753933, 1.968944643851434639 ) ) ;
#16261 = CARTESIAN_POINT ( 'NONE',  ( 1.136160399770862250, 0.3804006922196729867, 1.904278901077125052 ) ) ;
#16262 = COLOUR_RGB ( '', 0.08235294, 0.09019608, 0.10196078) ;
#16263 = CARTESIAN_POINT ( 'NONE',  ( 6.854781963242574605, -0.9897500569795645298, 2.071502949204959254 ) ) ;
#16265 = CARTESIAN_POINT ( 'NONE',  ( 5.506657433377460720, 0.5384353192533465338, 1.781376027434707687 ) ) ;
#16264 = CARTESIAN_POINT ( 'NONE',  ( -7.781453819600577582, 8.043060642480948985, 0.000000000000000000 ) ) ;
#16266 = CARTESIAN_POINT ( 'NONE',  ( 6.249382461256315580, 6.255644057745969988, -0.7998128361456481317 ) ) ;
#16267 = SURFACE_STYLE_USAGE ( .BOTH. , #164683 ) ;
#16268 = CARTESIAN_POINT ( 'NONE',  ( -6.403528624356093601, 6.365204904703887223, 1.040834085586084257E-14 ) ) ;
#16269 = CARTESIAN_POINT ( 'NONE',  ( -3.365144920186191158, -0.9421578975231510444, 0.09679790593341147664 ) ) ;
#16270 = CARTESIAN_POINT ( 'NONE',  ( 0.8904706703079521279, -0.5376514911656914419, -2.124458794526106864 ) ) ;
#16271 = CARTESIAN_POINT ( 'NONE',  ( 5.192409644353875642, 5.160158794608717514, 1.040834085586084257E-14 ) ) ;
#16272 = ORIENTED_EDGE ( 'NONE', *, *, #77102, .T. ) ;
#16273 = CARTESIAN_POINT ( 'NONE',  ( 10.98997987423603817, -6.893137084989856334, -0.4694063952341778756 ) ) ;
#16275 =( BOUNDED_CURVE ( )  B_SPLINE_CURVE ( 2, ( #155853, #7440, #153721, #4229, #203497 ),
 .UNSPECIFIED., .F., .T. ) 
 B_SPLINE_CURVE_WITH_KNOTS ( ( 3, 2, 3 ),
 ( 0.2500000000000002776, 0.2541666666666667074, 0.2546568312040279891 ),
 .UNSPECIFIED. ) 
 CURVE ( )  GEOMETRIC_REPRESENTATION_ITEM ( )  RATIONAL_B_SPLINE_CURVE ( ( 0.9999999999999911182, 0.8660254037844475894, 1.000000000000000000, 0.9842392969666786673, 0.9721867560345496262 ) ) 
 REPRESENTATION_ITEM ( '' )  );
#16274 =( LENGTH_UNIT ( ) NAMED_UNIT ( * ) SI_UNIT ( .MILLI., .METRE. ) );
#16276 = CARTESIAN_POINT ( 'NONE',  ( 2.103868193876055503, -1.825329726703457833, 0.04394198290156441783 ) ) ;
#16277 = CARTESIAN_POINT ( 'NONE',  ( -3.948449050077848632, 5.629609863222681199, 1.599625672291267398 ) ) ;
#16278 = CARTESIAN_POINT ( 'NONE',  ( 0.003115319777771509598, 2.586180586277187388, -2.083632524825635990 ) ) ;
#16279 = CARTESIAN_POINT ( 'NONE',  ( 6.509000000000014552, 2.959959533984284352, 2.552917358632576850 ) ) ;
#16280 = CARTESIAN_POINT ( 'NONE',  ( 0.1331565106231598072, 7.629137130509052511, -2.545925718843544239 ) ) ;
#16281 = CARTESIAN_POINT ( 'NONE',  ( 6.182242880246401562, -0.9723386526096773341, 1.545037271442825100 ) ) ;
#16282 = CARTESIAN_POINT ( 'NONE',  ( 4.715648799723409113, 0.4337510919622395988, -1.913030730064477547 ) ) ;
#16283 = CARTESIAN_POINT ( 'NONE',  ( -6.516665389662827934, 10.75452672124865217, 0.000000000000000000 ) ) ;
#16284 = CARTESIAN_POINT ( 'NONE',  ( 5.276094334012385367, 9.307193822989793475, 1.040834085586084257E-14 ) ) ;
#16285 = EDGE_CURVE ( 'NONE', #95583, #60268, #124474, .T. ) ;
#16286 = CARTESIAN_POINT ( 'NONE',  ( 4.406960118137589255, -0.4655763551070742912, -2.068578822641816473 ) ) ;
#16287 = CARTESIAN_POINT ( 'NONE',  ( -7.645908563102897126, 11.00764485934031889, 1.199719254218453823 ) ) ;
#16288 = CIRCLE ( 'NONE', #147763, 9.999999999999998224 ) ;
#16289 = CARTESIAN_POINT ( 'NONE',  ( 3.649115900372475796, 7.409052317076538330, 1.040834085586084257E-14 ) ) ;
#16290 = CARTESIAN_POINT ( 'NONE',  ( 2.553653463975919635, 1.597511423921485818, 1.316731848974454833 ) ) ;
#16292 = CARTESIAN_POINT ( 'NONE',  ( 1.364683531249986537, -0.5739583329919174526, 0.7879004041258500513 ) ) ;
#16291 = CARTESIAN_POINT ( 'NONE',  ( -0.2442642247113720744, -5.209160580580717514, -10.99754090108938875 ) ) ;
#16293 = ORIENTED_EDGE ( 'NONE', *, *, #56964, .F. ) ;
#16294 = CARTESIAN_POINT ( 'NONE',  ( 2.760663040853128525, 2.181856774409622890, -0.7236605881647265592 ) ) ;
#16295 = CARTESIAN_POINT ( 'NONE',  ( 7.727784370109387346, 10.99920361756089093, -1.082531754730543083 ) ) ;
#16297 = CARTESIAN_POINT ( 'NONE',  ( 1.001543065824772753E-15, -1.771874999522040861, 3.793834371823811669 ) ) ;
#16296 = CARTESIAN_POINT ( 'NONE',  ( 4.909461021924231616, 8.741805268971372556, 0.7216878364870317197 ) ) ;
#16298 = CARTESIAN_POINT ( 'NONE',  ( 6.620655732516647518, 0.007553340620044743381, 1.826407896915738238 ) ) ;
#16299 =( LENGTH_UNIT ( ) NAMED_UNIT ( * ) SI_UNIT ( .MILLI., .METRE. ) );
#16300 = ORIENTED_EDGE ( 'NONE', *, *, #102591, .F. ) ;
#16302 = EDGE_CURVE ( 'NONE', #198860, #158402, #185431, .T. ) ;
#16301 = CARTESIAN_POINT ( 'NONE',  ( -0.1329251406260706092, -9.135512438678663472, 9.499304248211860369 ) ) ;
#16303 = CARTESIAN_POINT ( 'NONE',  ( 4.131050151015442928, 1.750605847248308145, 0.7702136748066327199 ) ) ;
#16304 = CARTESIAN_POINT ( 'NONE',  ( -6.007394966791244961, 6.077829431809393945, -0.6506939885215150543 ) ) ;
#16305 = CARTESIAN_POINT ( 'NONE',  ( 5.491107761985050573, 1.519353413045966494, -0.8162815091526542943 ) ) ;
#16306 = CARTESIAN_POINT ( 'NONE',  ( 3.784388871581423786, -0.6371526190629381858, -1.913262240507591416 ) ) ;
#16307 = CARTESIAN_POINT ( 'NONE',  ( 5.256544959696739738, 2.216068975266134000, -0.6104820095701003480 ) ) ;
#16308 = CARTESIAN_POINT ( 'NONE',  ( -11.44779963594995387, 12.69999999999999041, -3.600000000000078693 ) ) ;
#16309 = CARTESIAN_POINT ( 'NONE',  ( 0.4345545588612038657, 1.130843733186673639, -1.894998796914903139 ) ) ;
#16310 = CARTESIAN_POINT ( 'NONE',  ( -5.329763783947941036, 5.390681634126922361, 0.000000000000000000 ) ) ;
#16311 = CARTESIAN_POINT ( 'NONE',  ( 5.518734381310105519, 1.635532185772445857, 0.6765044976165290880 ) ) ;
#16313 = CARTESIAN_POINT ( 'NONE',  ( 1.834309667284042433, 2.267783887084608097, 0.3333485250246841503 ) ) ;
#16312 = CARTESIAN_POINT ( 'NONE',  ( 5.899733120602060232, 6.912052057904395141, -1.199719254218452047 ) ) ;
#16314 = CARTESIAN_POINT ( 'NONE',  ( 6.263598714517844890, 0.9507720431706818687, 1.576509192756641697 ) ) ;
#16315 = CARTESIAN_POINT ( 'NONE',  ( -2.123823618835070537, 5.629544655282869847, 1.040834085586084257E-14 ) ) ;
#16316 = SURFACE_SIDE_STYLE ('',( #84538 ) ) ;
#16317 = CARTESIAN_POINT ( 'NONE',  ( -3.654804927335652209, 6.421633627603656080, 1.199719254218452935 ) ) ;
#16318 = CARTESIAN_POINT ( 'NONE',  ( -1.360316468750021768, 0.1718750003414371008, -3.295974604355933479E-14 ) ) ;
#16319 = DIRECTION ( 'NONE',  ( 0.000000000000000000, 0.000000000000000000, 1.000000000000000000 ) ) ;
#16320 = CARTESIAN_POINT ( 'NONE',  ( 6.812946544903684121, -1.603000239855886466, 1.309962327488790157 ) ) ;
#16321 = CARTESIAN_POINT ( 'NONE',  ( 2.167204200501818612, 1.841733140229084853, -0.8216742516050157263 ) ) ;
#16322 = AXIS2_PLACEMENT_3D ( 'NONE', #36666, #53999, #87570 ) ;
#16323 =( BOUNDED_CURVE ( )  B_SPLINE_CURVE ( 3, ( #170962, #54020, #120159, #87589 ),
 .UNSPECIFIED., .F., .T. ) 
 B_SPLINE_CURVE_WITH_KNOTS ( ( 4, 4 ),
 ( 0.000000000000000000, 0.4999999999999995004 ),
 .UNSPECIFIED. ) 
 CURVE ( )  GEOMETRIC_REPRESENTATION_ITEM ( )  RATIONAL_B_SPLINE_CURVE ( ( 1.000000000000000000, 0.3333333333333340365, 0.3333333333333333703, 0.9999999999999993339 ) ) 
 REPRESENTATION_ITEM ( '' )  );
#16324 = CARTESIAN_POINT ( 'NONE',  ( 1.499999999999987121, 0.5770833340161539704, -0.8660254037844253849 ) ) ;
#16325 = CARTESIAN_POINT ( 'NONE',  ( 5.813098442667213206, 1.700071987003290763, 0.9061822306820240813 ) ) ;
#16326 = CARTESIAN_POINT ( 'NONE',  ( -0.6823417656250003738, 13.15104166700806232, 1.181850606188754593 ) ) ;
#16327 = CARTESIAN_POINT ( 'NONE',  ( 2.373529451608622054, -1.935128245189758012, -1.090680762624636868 ) ) ;
#16328 = VERTEX_POINT ( 'NONE', #9043 ) ;
#16329 = FACE_OUTER_BOUND ( 'NONE', #174362, .T. ) ;
#16330 = LINE ( 'NONE', #35796, #75197 ) ;
#16332 = EDGE_CURVE ( 'NONE', #110797, #23962, #158502, .T. ) ;
#16331 = CARTESIAN_POINT ( 'NONE',  ( 8.204655514564224816, 12.72384853363364066, 1.040834085586084257E-14 ) ) ;
#16333 = CARTESIAN_POINT ( 'NONE',  ( -0.7500000000000215383, 5.222916667349482012, 1.299038105676671107 ) ) ;
#16334 = PRESENTATION_STYLE_ASSIGNMENT (( #15276 ) ) ;
#16335 = CARTESIAN_POINT ( 'NONE',  ( 4.950617407298735451, -1.474004690277466834, -0.9251219707713809193 ) ) ;
#16337 = CARTESIAN_POINT ( 'NONE',  ( 3.490630252122445931, 1.913478943654752129, 0.4322817992908412621 ) ) ;
#16336 = COLOUR_RGB ( '', 0.09019608, 0.27058824, 0.51372549) ;
#16339 = CARTESIAN_POINT ( 'NONE',  ( -7.131225611108100715, 9.342849184424693476, 1.443375672974078761 ) ) ;
#16338 = CARTESIAN_POINT ( 'NONE',  ( 4.416205349749311004, 6.175325546172740765, 1.599625672291267398 ) ) ;
#16340 = CARTESIAN_POINT ( 'NONE',  ( -5.890076507333620981, 6.013243542187837853, -0.2543948676220365024 ) ) ;
#16341 = CARTESIAN_POINT ( 'NONE',  ( 4.464347054923422320, 1.061364745222750372, 1.997979292561928633 ) ) ;
#16342 = CARTESIAN_POINT ( 'NONE',  ( 1.381380011782725958, -0.05272402391268657396, 2.062171479924046036 ) ) ;
#16343 = CARTESIAN_POINT ( 'NONE',  ( -8.681298431451969222, 9.022603012982438386, 1.040834085586084257E-14 ) ) ;
#16344 = CARTESIAN_POINT ( 'NONE',  ( -4.907688418022547516, 4.827984030555475314, 1.214306433183764966E-14 ) ) ;
#16345 = CARTESIAN_POINT ( 'NONE',  ( 2.026610535765199561, 1.302222112816675326, -1.850007447375429104 ) ) ;
#16346 = ORIENTED_EDGE ( 'NONE', *, *, #5319, .T. ) ;
#16348 = ADVANCED_FACE ( 'NONE', ( #5806, #122899 ), #56731, .T. ) ;
#16347 = CARTESIAN_POINT ( 'NONE',  ( 1.499999999999989120, 0.05625000068281565957, 0.000000000000000000 ) ) ;
#16349 = CARTESIAN_POINT ( 'NONE',  ( 2.161206213664386144, 0.3243885794495802721, -1.842051381961368639 ) ) ;
#16350 = CARTESIAN_POINT ( 'NONE',  ( 1.758077109659747395, 1.659224110165247179, -0.5040892880595440051 ) ) ;
#16351 = CARTESIAN_POINT ( 'NONE',  ( 5.601184584505256581, -0.5335315006234629953, 2.125516261704554211 ) ) ;
#16352 = CARTESIAN_POINT ( 'NONE',  ( 6.563506341781633502, 0.4036857245812221495, -2.271876217655709240 ) ) ;
#16353 = CARTESIAN_POINT ( 'NONE',  ( 1.182575006203628210, -2.010449142642761089, -0.4523898644508434486 ) ) ;
#16354 = CARTESIAN_POINT ( 'NONE',  ( 4.066302494797935374, -1.812431348068560988, -0.6977731361806001065 ) ) ;
#16355 = AXIS2_PLACEMENT_3D ( 'NONE', #45653, #28315, #80263 ) ;
#16356 = CARTESIAN_POINT ( 'NONE',  ( -3.348500752450953577, 4.929670182657964084, 1.443375672974062551 ) ) ;
#16357 = EDGE_CURVE ( 'NONE', #101393, #80951, #99247, .T. ) ;
#16358 = DIRECTION ( 'NONE',  ( 0.000000000000000000, 1.000000000000000000, 0.000000000000000000 ) ) ;
#16359 = CARTESIAN_POINT ( 'NONE',  ( 1.250000000000001110, 7.216295638291068821E-14, 2.052068128417951609 ) ) ;
#16360 = CARTESIAN_POINT ( 'NONE',  ( 0.6253970069214125349, 13.29757588023696435, 1.303592148572699339 ) ) ;
#16361 = CARTESIAN_POINT ( 'NONE',  ( 6.819686488043297246, -1.560180513003786462, 1.276622200526676743 ) ) ;
#16362 = CARTESIAN_POINT ( 'NONE',  ( 1.360316468749963592, 1.286458333674703969, -0.7853790794158961308 ) ) ;
#16363 = CARTESIAN_POINT ( 'NONE',  ( 5.063125043234593115, -1.117834493326537393, 1.678003986596336761 ) ) ;
#16364 = CARTESIAN_POINT ( 'NONE',  ( -10.34217224912604571, 10.96028913360221502, 0.7998128361456462443 ) ) ;
#16365 = CARTESIAN_POINT ( 'NONE',  ( 8.067265095331215718, 9.370563018429956870, 1.199719254218462483 ) ) ;
#16366 = CARTESIAN_POINT ( 'NONE',  ( 5.252858170651868441, 5.093032385374103299, -0.7998128361456481317 ) ) ;
#16368 = CARTESIAN_POINT ( 'NONE',  ( -4.163571889515733204, 7.868871248772474125, 0.07198445825242587304 ) ) ;
#16367 = CARTESIAN_POINT ( 'NONE',  ( 1.787459277025660542, 1.258035843444211155, 1.323286951131589895 ) ) ;
#16369 = FACE_OUTER_BOUND ( 'NONE', #173976, .T. ) ;
#16370 = CARTESIAN_POINT ( 'NONE',  ( -6.972266317189433020E-16, 1.750000000682810475, -1.225000000000013634 ) ) ;
#16371 = ORIENTED_EDGE ( 'NONE', *, *, #31880, .F. ) ;
#16372 = CARTESIAN_POINT ( 'NONE',  ( -4.787437638956935082, 6.678706226906775179, -1.443375672974066548 ) ) ;
#16373 = UNCERTAINTY_MEASURE_WITH_UNIT (LENGTH_MEASURE( 1.000000000000000082E-05 ), #147075, 'distance_accuracy_value', 'NONE');
#16374 = CARTESIAN_POINT ( 'NONE',  ( 0.000000000000000000, 4.400000000000001243, 0.000000000000000000 ) ) ;
#16375 = CARTESIAN_POINT ( 'NONE',  ( -9.104463846776669200, 10.58062822844965645, -1.199719254218441611 ) ) ;
#16376 = CARTESIAN_POINT ( 'NONE',  ( 6.516272353977101695, -2.019191618876531091, 0.05163682429563941356 ) ) ;
#16377 = CARTESIAN_POINT ( 'NONE',  ( -0.04015575566676531788, -1.641981170221142872, -1.341450104213978589 ) ) ;
#16378 = ORIENTED_EDGE ( 'NONE', *, *, #103623, .T. ) ;
#16379 = CARTESIAN_POINT ( 'NONE',  ( -5.478376588373717659, 8.549133898814758936, -1.199719254218452047 ) ) ;
#16380 = CARTESIAN_POINT ( 'NONE',  ( 4.320244504248938355, 8.192035688265757898, 1.040834085586084257E-14 ) ) ;
#16381 = CARTESIAN_POINT ( 'NONE',  ( 0.08116279290028630133, -0.1557560750096824431, -2.127278773206460638 ) ) ;
#16382 = CARTESIAN_POINT ( 'NONE',  ( 4.623672751230786027, 0.3474658942751901458, 1.986100912583692812 ) ) ;
#16383 = ORIENTED_EDGE ( 'NONE', *, *, #115804, .T. ) ;
#16384 = ORIENTED_EDGE ( 'NONE', *, *, #23869, .T. ) ;
#16385 = CARTESIAN_POINT ( 'NONE',  ( 3.606672709164983726, 7.347373054203803378, 0.3819235613196003687 ) ) ;
#16386 = CARTESIAN_POINT ( 'NONE',  ( 4.000000000000001776, 5.999999999999998224, -2.024999999999999911 ) ) ;
#16389 = ORIENTED_EDGE ( 'NONE', *, *, #15653, .F. ) ;
#16388 = DIRECTION ( 'NONE',  ( -3.330669073875478989E-16, 3.330669073875478989E-16, 1.000000000000000000 ) ) ;
#16387 = CARTESIAN_POINT ( 'NONE',  ( -5.387385936583832802, 7.378645907471495846, -1.599625672291271394 ) ) ;
#16390 = CARTESIAN_POINT ( 'NONE',  ( 5.803742400754204667, 7.332416669035665358, 1.290654366993408297 ) ) ;
#16391 = CARTESIAN_POINT ( 'NONE',  ( 5.325545996062735377, -1.462220743079494012, 1.388274341532859335 ) ) ;
#16392 = CARTESIAN_POINT ( 'NONE',  ( 4.470543924053159479, -0.002573283451708791025, -1.841320590191763973 ) ) ;
#16393 = CARTESIAN_POINT ( 'NONE',  ( -0.02319159430947542733, 0.7471999394491578572, -1.895068635927643630 ) ) ;
#16394 = CARTESIAN_POINT ( 'NONE',  ( 3.528207577792912719, -1.374008478127983546, -1.853924954965507466 ) ) ;
#16395 = CARTESIAN_POINT ( 'NONE',  ( 7.503511670520385479, 7.718794801887437274, 0.7998128361456281477 ) ) ;
#16396 = CARTESIAN_POINT ( 'NONE',  ( 5.887991582945824476, -0.9777203880148609416, 1.927937229880334113 ) ) ;
#16398 = CARTESIAN_POINT ( 'NONE',  ( 7.416473721875251890, 8.611306416064660851, 1.199719254218462483 ) ) ;
#16397 = CARTESIAN_POINT ( 'NONE',  ( 3.432827581131673522, -1.645759781613131967, 1.164986487700324425 ) ) ;
#16399 = CARTESIAN_POINT ( 'NONE',  ( 1.540467339043756434, -1.639628711884850265, 1.040515435762645380 ) ) ;
#16400 = CARTESIAN_POINT ( 'NONE',  ( -4.273844736805832767, 6.009238164405336313, 1.599625672291267398 ) ) ;
#16401 = CARTESIAN_POINT ( 'NONE',  ( 4.868718825205943901, -0.6189299756741394321, 2.213421903294809034 ) ) ;
#16402 = CARTESIAN_POINT ( 'NONE',  ( -9.438383064689515933, 15.32552904735514687, -7.309821827856222143 ) ) ;
#16403 = CARTESIAN_POINT ( 'NONE',  ( -5.666381855868691808, 5.575476684793721383, 0.000000000000000000 ) ) ;
#16404 = CARTESIAN_POINT ( 'NONE',  ( 3.748781033766034998, -1.529746656882627454, 1.076398355447941491 ) ) ;
#16407 = CARTESIAN_POINT ( 'NONE',  ( -7.096767062110449942, 7.244259425409119046, -0.7998128361456362523 ) ) ;
#16406 = CARTESIAN_POINT ( 'NONE',  ( 0.7499999999999885647, -1.235416665983847473, 1.299038105676657340 ) ) ;
#16405 = CARTESIAN_POINT ( 'NONE',  ( 1.423922367354793606, -1.897583212610975734, 0.2371896777705190806 ) ) ;
#16408 = CARTESIAN_POINT ( 'NONE',  ( 3.088704478669739295, -2.174299887604825177, -0.3769171259565203269 ) ) ;
#16409 = CARTESIAN_POINT ( 'NONE',  ( -1.558944071570950163, 8.694263516232775046, -2.499999999999761080 ) ) ;
#16410 = CARTESIAN_POINT ( 'NONE',  ( 2.517010073631369860, 6.088262185878572375, -0.7998128361456281477 ) ) ;
#16411 = CARTESIAN_POINT ( 'NONE',  ( 6.089020385868848528, 8.197219431637373432, -1.443375672974078761 ) ) ;
#16412 = CARTESIAN_POINT ( 'NONE',  ( -4.973143418114339021, 4.696422164088486895, 0.7998128361456341429 ) ) ;
#16413 = CARTESIAN_POINT ( 'NONE',  ( -5.573810548549546162, 9.516879716700865188, 0.7216878364870267237 ) ) ;
#16414 = CARTESIAN_POINT ( 'NONE',  ( 0.9660189047021714437, 0.9680410686894457273, 1.717217487461615955 ) ) ;
#16415 = CARTESIAN_POINT ( 'NONE',  ( 0.09532371275382427178, -0.5158531520006398585, -2.257940698305866967 ) ) ;
#16416 = CARTESIAN_POINT ( 'NONE',  ( 1.416376618315864144, 0.7919773292732554815, 1.795081228748253377 ) ) ;
#16417 = CARTESIAN_POINT ( 'NONE',  ( 5.436407774000851845, -1.150348206634976833, 1.711801118168945202 ) ) ;
#16418 = CARTESIAN_POINT ( 'NONE',  ( 5.694061328059515148, 5.745419092265303007, -0.7216878364870207285 ) ) ;
#16419 = CARTESIAN_POINT ( 'NONE',  ( 5.318541398310776103, 9.426991741329731056, -0.7998128361456481317 ) ) ;
#16420 = EDGE_LOOP ( 'NONE', ( #68221, #187077, #179832, #15162 ) ) ;
#16421 = CARTESIAN_POINT ( 'NONE',  ( -1.364683531250010295, 5.342708333674750953, 0.7879004041258379498 ) ) ;
#16422 = DIRECTION ( 'NONE',  ( -0.000000000000000000, -1.000000000000000000, -0.000000000000000000 ) ) ;
#16423 = CARTESIAN_POINT ( 'NONE',  ( 4.704316113817540668, 5.551085556617666228, -1.082531754730548412 ) ) ;
#16424 = CARTESIAN_POINT ( 'NONE',  ( 1.077284259287077495, 2.005170101804130578, 0.8328141809181826005 ) ) ;
#16425 = B_SPLINE_CURVE_WITH_KNOTS ( 'NONE', 3,
 ( #111007, #161841, #162902, #47030, #177012, #129417, #80573, #29703, #76303, #60052 ),
 .UNSPECIFIED., .F., .F.,
 ( 4, 2, 2, 2, 4 ),
 ( 0.000000000000000000, 0.2499999999999998890, 0.4999999999999998890, 0.7500000000000000000, 1.000000000000000000 ),
 .UNSPECIFIED. ) ;
#16427 = FACE_OUTER_BOUND ( 'NONE', #166921, .T. ) ;
#16426 = CARTESIAN_POINT ( 'NONE',  ( 1.347111479062087616E-15, -9.999999999999994671, -10.99999999999999112 ) ) ;
#16428 = EDGE_CURVE ( 'NONE', #34978, #36555, #15946, .T. ) ;
#16429 = CARTESIAN_POINT ( 'NONE',  ( 6.745922712994594228, -7.817744194000437297, 6.689586359223958389 ) ) ;
#16430 = FACE_OUTER_BOUND ( 'NONE', #140565, .T. ) ;
#16431 = CARTESIAN_POINT ( 'NONE',  ( 1.809613641711980359, -1.857008771552502768, 0.2239427725650791623 ) ) ;
#16432 = CARTESIAN_POINT ( 'NONE',  ( 5.659502677682959337, 0.4278135246765999988, -2.118672983663777654 ) ) ;
#16433 = CARTESIAN_POINT ( 'NONE',  ( -6.121777486219434294, 6.006025806897081765, -0.2357381234046468377 ) ) ;
#16434 = CARTESIAN_POINT ( 'NONE',  ( 0.000000000000000000, 19.00000000000000000, 0.000000000000000000 ) ) ;
#16435 = CARTESIAN_POINT ( 'NONE',  ( 0.6823417656249899377, 5.238541667008086655, -1.181850606188754593 ) ) ;
#16436 = CARTESIAN_POINT ( 'NONE',  ( 1.207504981961624813, 1.448612403150219885, 1.248453992567559512 ) ) ;
#16437 = CARTESIAN_POINT ( 'NONE',  ( 2.887294646099856532, 1.250245360129684791, 1.252957939402859600 ) ) ;
#16438 = CARTESIAN_POINT ( 'NONE',  ( 0.2934254677693093338, 1.784247535656303230, -0.6883866973072181317 ) ) ;
#16440 = CARTESIAN_POINT ( 'NONE',  ( 5.114804650195723390, 0.1453347504645576271, 1.910168102697987313 ) ) ;
#16439 = CARTESIAN_POINT ( 'NONE',  ( -5.604676892713675862, 5.547648157612228736, -0.09596228114882204840 ) ) ;
#16441 = CARTESIAN_POINT ( 'NONE',  ( 6.408657466097477773, 0.6165391127177908270, 1.870651749748206916 ) ) ;
#16442 = CARTESIAN_POINT ( 'NONE',  ( 0.7499999999999920064, 4.733333333333352932, 1.299038105676669330 ) ) ;
#16443 = CARTESIAN_POINT ( 'NONE',  ( 0.9496594531581278309, -1.914679731917130479, 0.9119059213342151082 ) ) ;
#16444 = CARTESIAN_POINT ( 'NONE',  ( 2.335253425310769071, -0.1017894593877440301, -0.4879271257269311990 ) ) ;
#16445 = CARTESIAN_POINT ( 'NONE',  ( 3.696050037196423332, -1.868490534004090931, -0.09263902202472777681 ) ) ;
#16446 = CARTESIAN_POINT ( 'NONE',  ( 1.066719475142905216, -1.649486405746130258, -0.7827983987617056494 ) ) ;
#16448 = CARTESIAN_POINT ( 'NONE',  ( 4.720979226589129496, 8.219560628541461966, -0.6735110442024627719 ) ) ;
#16447 = CARTESIAN_POINT ( 'NONE',  ( 4.635508124736155366, -2.018492079602551392, 0.8926152185086615454 ) ) ;
#16449 = CARTESIAN_POINT ( 'NONE',  ( -1.201851678989727383E-14, 4.759375000341419693, -1.575800808251660134 ) ) ;
#16450 = EDGE_CURVE ( 'NONE', #21539, #150774, #121464, .T. ) ;
#16451 = CARTESIAN_POINT ( 'NONE',  ( 1.697793086734213697, -1.492557772401803318, -1.423914585240863673 ) ) ;
#16452 = CARTESIAN_POINT ( 'NONE',  ( 5.799137018343234473, 7.788745826199009237, -1.599625672291262513 ) ) ;
#16453 = CARTESIAN_POINT ( 'NONE',  ( -6.665805079413154921, 10.92852302595736447, 0.7998128361456481317 ) ) ;
#16454 = PLANE ( 'NONE',  #175134 ) ;
#16455 = CARTESIAN_POINT ( 'NONE',  ( 11.94980361058168938, 10.90000000000000036, -1.100000000000000311 ) ) ;
#16456 = LINE ( 'NONE', #149686, #92926 ) ;
#16457 = COLOUR_RGB ( '', 0.08235294, 0.09019608, 0.10196078) ;
#16458 = ORIENTED_EDGE ( 'NONE', *, *, #202477, .F. ) ;
#16459 = CARTESIAN_POINT ( 'NONE',  ( 4.826661161267837841, -1.354893614093263254, 1.565527137264411728 ) ) ;
#16460 = CARTESIAN_POINT ( 'NONE',  ( 1.499999999999989120, 5.254166666666684193, 0.8660254037844524744 ) ) ;
#16461 = CARTESIAN_POINT ( 'NONE',  ( 0.9487563388480976245, 0.6265645459165304354, 2.068816658077163861 ) ) ;
#16462 = CARTESIAN_POINT ( 'NONE',  ( -5.857301623663916601, 7.199535845156014524, -1.157093103336486628 ) ) ;
#16463 = CARTESIAN_POINT ( 'NONE',  ( 2.473312253293189489, -1.758384921082667862, -0.9933899200572825494 ) ) ;
#16464 = FACE_OUTER_BOUND ( 'NONE', #214224, .T. ) ;
#16465 = VERTEX_POINT ( 'NONE', #121813 ) ;
#16466 = ORIENTED_EDGE ( 'NONE', *, *, #199193, .F. ) ;
#16468 = CARTESIAN_POINT ( 'NONE',  ( 7.456621297836061757, 11.64321591421002644, 0.7216878364870438212 ) ) ;
#16467 = CARTESIAN_POINT ( 'NONE',  ( -3.475000000000000533, -2.829166666666666607, -2.006292185433948827 ) ) ;
#16469 = CARTESIAN_POINT ( 'NONE',  ( 0.07926560466934955140, 14.48322640536331818, 11.99972816967691891 ) ) ;
#16470 = CARTESIAN_POINT ( 'NONE',  ( -0.1882626618336727398, -1.244567986390752390, -1.587255334073833790 ) ) ;
#16471 = CARTESIAN_POINT ( 'NONE',  ( 6.539320575229278454, 2.035006821797652687, 2.408631514295301645 ) ) ;
#16472 = CARTESIAN_POINT ( 'NONE',  ( 5.407841436338867602, -0.9846607899807978681, -1.957994596084790206 ) ) ;
#16473 = CARTESIAN_POINT ( 'NONE',  ( -1.499999999999997780, 3.181250000682818602, 1.214306433183764966E-14 ) ) ;
#16474 = CARTESIAN_POINT ( 'NONE',  ( 3.480628297764537304, -1.280852673386581486, 1.420289963180096260 ) ) ;
#16475 = CARTESIAN_POINT ( 'NONE',  ( -4.613852347352193739, 4.277249248199312071, 1.214306433183764966E-14 ) ) ;
#16476 = CARTESIAN_POINT ( 'NONE',  ( 3.023105065722948126, 6.470780310077995701, 0.7216878364870338292 ) ) ;
#16478 = CARTESIAN_POINT ( 'NONE',  ( 2.566029989117986077, -1.034146858587611906, 1.730878619409223163 ) ) ;
#16477 = CARTESIAN_POINT ( 'NONE',  ( 0.3999999999999681033, 3.372708439410100567, 0.4999999999999501510 ) ) ;
#16479 = CARTESIAN_POINT ( 'NONE',  ( 1.364683531249996529, 12.52604166700806054, 0.7879004041258405033 ) ) ;
#16481 = CARTESIAN_POINT ( 'NONE',  ( -4.787964524281469458, 5.614988695530339413, -1.199719254218453823 ) ) ;
#16480 = CARTESIAN_POINT ( 'NONE',  ( 0.2402843302407534631, 2.286812847775396840, 0.1605059593563825382 ) ) ;
#16482 = CARTESIAN_POINT ( 'NONE',  ( 4.014446192991796281, 1.219382930577699309, -1.220076339321971570 ) ) ;
#16483 = CARTESIAN_POINT ( 'NONE',  ( -0.1394461523061013564, 4.080274402048936544, -2.835111295649892060 ) ) ;
#16484 = CARTESIAN_POINT ( 'NONE',  ( 2.835626683552519012, 6.459981564119914310, 0.000000000000000000 ) ) ;
#16485 = CARTESIAN_POINT ( 'NONE',  ( -1.230761180058552950, 2.935133534840178804, -0.7749999999999988010 ) ) ;
#16486 = CARTESIAN_POINT ( 'NONE',  ( 0.6548940681232479077, -1.578012236938080015, -1.004313744925364071 ) ) ;
#16487 = CARTESIAN_POINT ( 'NONE',  ( 2.679707916995359263, 6.278076336469897711, -0.7998128361456291469 ) ) ;
#16488 = CARTESIAN_POINT ( 'NONE',  ( 0.07556134207193415664, 4.081186479400328082, -2.798928192855642649 ) ) ;
#16489 = CARTESIAN_POINT ( 'NONE',  ( 0.3564121386029559524, -2.069725681613205026, -0.05427943458365809548 ) ) ;
#16490 = ORIENTED_EDGE ( 'NONE', *, *, #103236, .F. ) ;
#16491 = CARTESIAN_POINT ( 'NONE',  ( 4.793523346383269157, 1.688353701584244915, -0.6568948891843768845 ) ) ;
#16492 = VERTEX_POINT ( 'NONE', #71883 ) ;
#16493 = CARTESIAN_POINT ( 'NONE',  ( 5.529746549527311039, 7.544733289238903851, -1.599625672291281386 ) ) ;
#16494 = CARTESIAN_POINT ( 'NONE',  ( -0.1104750535120269106, 7.629137130509076492, -2.703481013110929698 ) ) ;
#16495 = CARTESIAN_POINT ( 'NONE',  ( 5.567019150587803722, -1.423986762948417972, 1.119560556780722083 ) ) ;
#16496 = CARTESIAN_POINT ( 'NONE',  ( 6.712695452097489301, 7.964471127936110229, -1.082531754730548412 ) ) ;
#16497 = CARTESIAN_POINT ( 'NONE',  ( 7.592810154713589835E-16, -0.2000000000000057288, -6.200000000000000178 ) ) ;
#16498 = CARTESIAN_POINT ( 'NONE',  ( 5.237746300327911442, 6.405127287353401755, -1.156737470277836355 ) ) ;
#16499 = CIRCLE ( 'NONE', #179041, 0.09999999999999982514 ) ;
#16500 = ADVANCED_FACE ( 'NONE', ( #74051 ), #144216, .T. ) ;
#16502 = CARTESIAN_POINT ( 'NONE',  ( 9.134442807305049428, 11.67993591332117376, 1.599625672291281386 ) ) ;
#16501 = CARTESIAN_POINT ( 'NONE',  ( 6.777813018113469923, -1.804774468322063452, 0.4538611949938906043 ) ) ;
#16503 = CARTESIAN_POINT ( 'NONE',  ( 3.796418445691573940, 1.352171417773648132, -1.357169225504866406 ) ) ;
#16504 = DIRECTION ( 'NONE',  ( 0.000000000000000000, -1.000000000000000000, 0.000000000000000000 ) ) ;
#16505 = CARTESIAN_POINT ( 'NONE',  ( -1.364683531250000748, 0.2593750003414205252, 0.000000000000000000 ) ) ;
#16506 = CARTESIAN_POINT ( 'NONE',  ( 5.327991180490514012, 9.159814110640187579, 1.040834085586084257E-14 ) ) ;
#16508 = CARTESIAN_POINT ( 'NONE',  ( 5.858642105998121963, -2.011370865819528397, -0.6617598028889163375 ) ) ;
#16507 = CARTESIAN_POINT ( 'NONE',  ( -8.676855123066012254, 12.10645282934361866, -1.082531754730543971 ) ) ;
#16509 = CARTESIAN_POINT ( 'NONE',  ( 0.5148121308554790554, 1.489681748880047563, -1.566682057046256071 ) ) ;
#16510 = CARTESIAN_POINT ( 'NONE',  ( -4.274563570058511175, 8.209017608368725405, 0.000000000000000000 ) ) ;
#16511 = CARTESIAN_POINT ( 'NONE',  ( 5.740951700743842423, 5.662474837148078421, -0.7998128361456481317 ) ) ;
#16512 = CARTESIAN_POINT ( 'NONE',  ( 1.254616015376356586, -1.441780481750528420, 1.119729341354458452 ) ) ;
#16513 = CARTESIAN_POINT ( 'NONE',  ( -3.144601563365788444, 5.756120026313656268, -1.199719254218452935 ) ) ;
#16514 = CARTESIAN_POINT ( 'NONE',  ( 3.522295995157863846, 1.158834602800838498, -1.410599190884161747 ) ) ;
#16515 = CARTESIAN_POINT ( 'NONE',  ( 12.20411482740001574, 8.058544339043594462, 4.983824382154795174 ) ) ;
#16516 = CARTESIAN_POINT ( 'NONE',  ( 2.918110517850933672, -1.910018876965378309, 0.09814724848770939314 ) ) ;
#16517 = EDGE_LOOP ( 'NONE', ( #60543, #107253, #189168, #213500 ) ) ;
#16518 = CARTESIAN_POINT ( 'NONE',  ( 2.928127725102438461, 1.051234477803453027, 1.665338043752979447 ) ) ;
#16519 = CARTESIAN_POINT ( 'NONE',  ( 4.897963269493502025, -0.6577025220009655726, -1.827417481390420928 ) ) ;
#16520 = CARTESIAN_POINT ( 'NONE',  ( -7.923814432544069142, 8.209148024248356990, 0.000000000000000000 ) ) ;
#16522 = CARTESIAN_POINT ( 'NONE',  ( 5.010073305087408002, -0.7609581946756528437, 1.979555329295646260 ) ) ;
#16521 = CARTESIAN_POINT ( 'NONE',  ( 6.587282531393223728, 8.778525268082516320, 1.599625672291268286 ) ) ;
#16523 = DIRECTION ( 'NONE',  ( -1.276756478318932585E-15, 1.000000000000000000, -1.665334536937738262E-16 ) ) ;
#16524 = CARTESIAN_POINT ( 'NONE',  ( 2.965378323150099860, -1.564627974442783342, -1.099164922500090347 ) ) ;
#16525 = CARTESIAN_POINT ( 'NONE',  ( 6.001708393183096568, 6.086876045059843143, 0.6039332608892417076 ) ) ;
#16526 = CARTESIAN_POINT ( 'NONE',  ( 0.2331563151865729544, 2.882199166944008795, -2.434502449063076224 ) ) ;
#16527 = ORIENTED_EDGE ( 'NONE', *, *, #68847, .T. ) ;
#16528 = CARTESIAN_POINT ( 'NONE',  ( 5.415556014015861841, 5.282846535965431300, -0.7998128361456481317 ) ) ;
#16529 = CARTESIAN_POINT ( 'NONE',  ( 5.332434488876471868, 5.115595079977664383, 0.7998128361456341429 ) ) ;
#16530 = CARTESIAN_POINT ( 'NONE',  ( 4.143230477514478594, 0.1011454402246019235, 2.010680395766785811 ) ) ;
#16531 = DIRECTION ( 'NONE',  ( -5.578564026256490882E-16, -1.000000000000000000, -9.066213480720158442E-32 ) ) ;
#16532 = CARTESIAN_POINT ( 'NONE',  ( 5.145057536039753465, -1.563975785779356587, 0.9416349707431559413 ) ) ;
#16533 = CARTESIAN_POINT ( 'NONE',  ( 1.100149375694438714, 0.8407228983892693908, -1.892171374333020628 ) ) ;
#16534 = CARTESIAN_POINT ( 'NONE',  ( -7.212574532790087645, 11.35849468832304154, -0.7216878364870267237 ) ) ;
#16535 = CARTESIAN_POINT ( 'NONE',  ( -5.689102680971802606, 7.419971068449684459, 1.333831099742349480 ) ) ;
#16536 = CARTESIAN_POINT ( 'NONE',  ( 3.475000000000000533, -2.960416665710750905, 2.006292185433948827 ) ) ;
#16537 = CARTESIAN_POINT ( 'NONE',  ( 5.190257414508706368, -1.856628772771324210, -0.2281712211116558864 ) ) ;
#16538 = CARTESIAN_POINT ( 'NONE',  ( 5.262536180398716290, 9.291375977107183104, -0.7998128361456291469 ) ) ;
#16539 = CARTESIAN_POINT ( 'NONE',  ( -5.220052836461385404, 6.048815383081766583, -1.199719254218446718 ) ) ;
#16540 = EDGE_CURVE ( 'NONE', #213971, #71609, #82927, .T. ) ;
#16541 = AXIS2_PLACEMENT_3D ( 'NONE', #24474, #106873, #159835 ) ;
#16542 = CARTESIAN_POINT ( 'NONE',  ( -1.402160292154681736E-14, 9.984375000341401574, 1.575800808251682339 ) ) ;
#16543 = CARTESIAN_POINT ( 'NONE',  ( -4.238895582566952314, 8.097128612970093897, 1.040834085586084257E-14 ) ) ;
#16544 = CARTESIAN_POINT ( 'NONE',  ( 3.009020027229115879, 5.597941567487558778, -1.199719254218446718 ) ) ;
#16545 = CARTESIAN_POINT ( 'NONE',  ( -4.678972410047611774, 5.591794245544547515, 1.082531754730549078 ) ) ;
#16546 = CARTESIAN_POINT ( 'NONE',  ( -5.042743069279040036, 7.970618449879118828, 1.199719254218464037 ) ) ;
#16547 = CARTESIAN_POINT ( 'NONE',  ( 0.5497785174156321064, 1.531638494488884339, 1.392999266381978130 ) ) ;
#16548 = CARTESIAN_POINT ( 'NONE',  ( 2.601287765717251510, -0.2046159961377100600, 2.107301599238825318 ) ) ;
#16549 = CARTESIAN_POINT ( 'NONE',  ( 8.483651433849084711, 10.92067931095586886, 1.599625672291281386 ) ) ;
#16550 = CARTESIAN_POINT ( 'NONE',  ( -2.696596522755091208, 2.993039318081801792, 2.500000000000000444 ) ) ;
#16551 = CARTESIAN_POINT ( 'NONE',  ( 6.227406488038683463, 0.1581931229415085571, -2.064300627111630870 ) ) ;
#16552 = CARTESIAN_POINT ( 'NONE',  ( 4.193481561896174270, 7.343914482741291216, -0.8359065270147625348 ) ) ;
#16553 = CARTESIAN_POINT ( 'NONE',  ( 6.480434237652135998, 6.662854153456708950, 0.7216878364870317197 ) ) ;
#16555 = LINE ( 'NONE', #161785, #177448 ) ;
#16554 = DIRECTION ( 'NONE',  ( 3.330669073875478989E-16, -3.540251991789410786E-16, -1.000000000000000000 ) ) ;
#16556 = CARTESIAN_POINT ( 'NONE',  ( 2.221020806870691366, 0.002245647979397680065, 2.292435215953308791 ) ) ;
#16558 = CARTESIAN_POINT ( 'NONE',  ( 6.938893903907228378E-15, 10.64264068711930733, 1.214306433183764966E-14 ) ) ;
#16557 = CARTESIAN_POINT ( 'NONE',  ( -9.492899823913846902, -8.233137084989849086, 0.3774118403930767918 ) ) ;
#16559 = CARTESIAN_POINT ( 'NONE',  ( 2.689602200614676697, 1.814610489020528350, -0.6038049036062518304 ) ) ;
#16560 = ORIENTED_EDGE ( 'NONE', *, *, #3854, .F. ) ;
#16562 = ADVANCED_FACE ( 'NONE', ( #105506 ), #190974, .T. ) ;
#16561 = CARTESIAN_POINT ( 'NONE',  ( 8.093854517234030155, 8.545177812968924869, -0.7216878364870267237 ) ) ;
#16563 = CARTESIAN_POINT ( 'NONE',  ( 0.6154903249990024694, 1.648289601840571938, 1.155678142064648917 ) ) ;
#16564 = CARTESIAN_POINT ( 'NONE',  ( 0.9011314981347726683, -1.685442764318560771, 1.003610994683441948 ) ) ;
#16565 = DIRECTION ( 'NONE',  ( -0.000000000000000000, -1.000000000000000000, -0.000000000000000000 ) ) ;
#16566 = CARTESIAN_POINT ( 'NONE',  ( -6.177711549321182716, 10.35908057418338402, 0.7998128361456481317 ) ) ;
#16567 = CARTESIAN_POINT ( 'NONE',  ( 1.001543065824772753E-15, -0.4593749995220425819, 3.793834371823811669 ) ) ;
#16569 = CARTESIAN_POINT ( 'NONE',  ( 2.113771285056417426, -0.8311870117129838142, -1.562508279020339064 ) ) ;
#16568 = CARTESIAN_POINT ( 'NONE',  ( 3.539087885488776397, -1.583190213782994515, -1.365486535101219534 ) ) ;
#16570 = CARTESIAN_POINT ( 'NONE',  ( 4.074186250656476993, 7.493853916489129574, -0.5595503573846259959 ) ) ;
#16572 = CARTESIAN_POINT ( 'NONE',  ( 5.701222307317492799, -0.5618967582242094805, 2.222226568792139645 ) ) ;
#16571 = CARTESIAN_POINT ( 'NONE',  ( -11.93239723206674618, 7.875908177015204181, -1.297019848843022238 ) ) ;
#16573 = CARTESIAN_POINT ( 'NONE',  ( 4.048569170814999119, -1.448435850583905671, -0.9644227198624519826 ) ) ;
#16574 = CARTESIAN_POINT ( 'NONE',  ( 9.673906298550626559, 11.24497775551929557, 1.199719254218452047 ) ) ;
#16575 = CARTESIAN_POINT ( 'NONE',  ( 3.982994815507484354, 7.308283119008860851, -0.9368446653362592080 ) ) ;
#16576 = CARTESIAN_POINT ( 'NONE',  ( 3.040114402249920911, 1.647253858686392958, -0.5413168154804471888 ) ) ;
#16577 = CARTESIAN_POINT ( 'NONE',  ( 4.264261594705793357, -2.165624863444326920, 0.1558643175220644772 ) ) ;
#16578 = CARTESIAN_POINT ( 'NONE',  ( 4.467575310902914154, 5.170924936596891008, 1.199719254218464037 ) ) ;
#16579 = CARTESIAN_POINT ( 'NONE',  ( 5.401577436481666439, -1.966305606708594667, 0.4464985920552416720 ) ) ;
#16580 = CARTESIAN_POINT ( 'NONE',  ( 0.3749999999841767684, 2.052068128807281955, -2.222409888604170519E-14 ) ) ;
#16581 = COLOUR_RGB ( '', 0.72549020, 0.75294118, 0.79215686) ;
#16582 = CARTESIAN_POINT ( 'NONE',  ( 1.499999999999990896, 4.306250000682819490, 1.214306433183764966E-14 ) ) ;
#16583 = CARTESIAN_POINT ( 'NONE',  ( 2.168856224914788466, -1.760356022852540114, -0.7827933968581005653 ) ) ;
#16584 = CARTESIAN_POINT ( 'NONE',  ( -0.7500000000000006661, 9.739583334016129967, -1.299038105676657340 ) ) ;
#16585 = CARTESIAN_POINT ( 'NONE',  ( 5.537407084817251857, -0.05464564937080264306, 2.220880467482534204 ) ) ;
#16586 = ORIENTED_EDGE ( 'NONE', *, *, #128001, .F. ) ;
#16587 = CARTESIAN_POINT ( 'NONE',  ( 6.983263157960363010, 3.696136926403908340, 2.460428995873820579 ) ) ;
#16588 = CARTESIAN_POINT ( 'NONE',  ( 1.499999999999987121, 1.545833333333354487, -0.8660254037844253849 ) ) ;
#16589 = CARTESIAN_POINT ( 'NONE',  ( 6.205881626753210867, 8.263281202677319470, 1.599625672291281386 ) ) ;
#16590 = CARTESIAN_POINT ( 'NONE',  ( 5.002595493318194642, 4.938708951733754127, -0.7216878364870197293 ) ) ;
#16591 = CARTESIAN_POINT ( 'NONE',  ( 1.594693315975799441, -1.184698573716694847, 1.878835628132907054 ) ) ;
#16592 = CARTESIAN_POINT ( 'NONE',  ( -3.475000000000000533, -1.035416665710751527, -2.006292185433948827 ) ) ;
#16593 = CARTESIAN_POINT ( 'NONE',  ( 8.948018195339340508, 9.541702104091804415, -0.7216878364870197293 ) ) ;
#16594 = CARTESIAN_POINT ( 'NONE',  ( 0.4144236700470090295, 2.998638349210888343, 1.957873639358022722 ) ) ;
#16595 = CARTESIAN_POINT ( 'NONE',  ( 4.692003678781083487, 7.631698837623355658, -1.199719254218450271 ) ) ;
#16597 = AXIS2_PLACEMENT_3D ( 'NONE', #77300, #205141, #122951 ) ;
#16596 =( GEOMETRIC_REPRESENTATION_CONTEXT ( 3 ) GLOBAL_UNCERTAINTY_ASSIGNED_CONTEXT ( ( #200168 ) ) GLOBAL_UNIT_ASSIGNED_CONTEXT ( ( #60805, #78116, #144246 ) ) REPRESENTATION_CONTEXT ( 'NONE', 'WORKASPACE' ) );
#16598 = CARTESIAN_POINT ( 'NONE',  ( -5.017926250833627755, 5.026871178826882947, 0.7216878364870257245 ) ) ;
#16599 = CARTESIAN_POINT ( 'NONE',  ( 4.281722439037777050, -1.974808133235542495, 0.5956899724020509046 ) ) ;
#16600 = CARTESIAN_POINT ( 'NONE',  ( -4.416205349749324327, 6.175325546172740765, 1.599625672291267398 ) ) ;
#16602 = EDGE_CURVE ( 'NONE', #23394, #15686, #93334, .T. ) ;
#16601 = CARTESIAN_POINT ( 'NONE',  ( -1.500000000000011324, 5.202083334016151639, 0.8660254037844403729 ) ) ;
#16603 = CARTESIAN_POINT ( 'NONE',  ( -0.6823417656250003738, -0.03229166632524871350, -1.181850606188749264 ) ) ;
#16604 = CARTESIAN_POINT ( 'NONE',  ( 6.186763334926775215, -0.2743023915687745617, -1.850177433978140051 ) ) ;
#16605 = CARTESIAN_POINT ( 'NONE',  ( 4.676219527341594073, 1.289314336954486384, 1.159937944992680547 ) ) ;
#16606 = CARTESIAN_POINT ( 'NONE',  ( 4.669343813871559945, 1.007284801977660349, 1.419122490755047705 ) ) ;
#16607 = CARTESIAN_POINT ( 'NONE',  ( 4.359110081993588182, 5.044382169536003602, -1.199719254218452047 ) ) ;
#16608 = CARTESIAN_POINT ( 'NONE',  ( 1.576131469712481303, -1.221787821332357860, 1.939473486982680628 ) ) ;
#16609 = CARTESIAN_POINT ( 'NONE',  ( -1.364683531250000748, -1.240624999658580752, 0.000000000000000000 ) ) ;
#16610 = CARTESIAN_POINT ( 'NONE',  ( 6.251524270843968445, 2.085125267542327965, -0.1543399900023248728 ) ) ;
#16611 = CARTESIAN_POINT ( 'NONE',  ( 1.693040327840355408, -0.6214066371539993527, 1.733238834403828754 ) ) ;
#16612 = EDGE_CURVE ( 'NONE', #6901, #173454, #104421, .T. ) ;
#16613 = CARTESIAN_POINT ( 'NONE',  ( 10.73535870392234237, 11.41900666419791399, 0.000000000000000000 ) ) ;
#16614 = CARTESIAN_POINT ( 'NONE',  ( 1.793592486599729252, 1.492254607734722072, -1.356300734917381678 ) ) ;
#16615 = CARTESIAN_POINT ( 'NONE',  ( 0.3049557181189037625, 1.908793570626087455, 1.076422248949958638 ) ) ;
#16616 = CARTESIAN_POINT ( 'NONE',  ( 9.212836904423678419, 13.91817412819898259, -6.903416813961001708 ) ) ;
#16617 = CARTESIAN_POINT ( 'NONE',  ( -6.201965203247477909, 9.323044272842313518, 1.199719254218452047 ) ) ;
#16618 = CARTESIAN_POINT ( 'NONE',  ( 1.856005582152659317, -0.6995316168164237292, 1.948720873434762080 ) ) ;
#16619 = CARTESIAN_POINT ( 'NONE',  ( 4.680589345215795838, 6.483773540883647435, -1.599625672291256295 ) ) ;
#16620 = CARTESIAN_POINT ( 'NONE',  ( 0.6801582343749970061, -0.4947916663252532876, 1.178068619123832983 ) ) ;
#16621 = CARTESIAN_POINT ( 'NONE',  ( 3.545663791850160784, -1.958584582392399742, 0.8131309587096480218 ) ) ;
#16622 = CARTESIAN_POINT ( 'NONE',  ( 1.364683531249986537, -0.5947916663252456049, -0.7879004041258309554 ) ) ;
#16623 = CARTESIAN_POINT ( 'NONE',  ( 5.268108045213575785, 0.9031548532531764595, 1.586571422427636824 ) ) ;
#16624 = VERTEX_POINT ( 'NONE', #202952 ) ;
#16625 = CARTESIAN_POINT ( 'NONE',  ( -6.818824913030298696, 6.919993584815607335, 0.7998128361456341429 ) ) ;
#16626 = CARTESIAN_POINT ( 'NONE',  ( 8.910733272679570049, 11.41894145625809820, -1.599625672291255185 ) ) ;
#16627 = CARTESIAN_POINT ( 'NONE',  ( 6.658462837642799670, 7.901199744405670522, 1.082531754730549967 ) ) ;
#16628 = CARTESIAN_POINT ( 'NONE',  ( 0.000000000000000000, -3.193749999044083410, -4.012584370867899430 ) ) ;
#16629 = CARTESIAN_POINT ( 'NONE',  ( -5.961834861707238531, 7.978559976790334574, -1.599625672291263179 ) ) ;
#16630 = CARTESIAN_POINT ( 'NONE',  ( 3.832289616293593770, -1.041828873002103917, -1.730228960026259255 ) ) ;
#16631 = CARTESIAN_POINT ( 'NONE',  ( 0.4464868854077256866, 2.100361318156780399, 0.1544987475943972732 ) ) ;
#16632 = CARTESIAN_POINT ( 'NONE',  ( -5.121948170912633991, 9.197632976031879792, -0.7998128361456362523 ) ) ;
#16633 = CARTESIAN_POINT ( 'NONE',  ( 9.541187415715040032, 12.15447128979948310, -1.599625672291262513 ) ) ;
#16634 = CARTESIAN_POINT ( 'NONE',  ( 5.295690652966449363, -1.314428334581790203, -1.317609258728233756 ) ) ;
#16635 = CARTESIAN_POINT ( 'NONE',  ( 8.925345196497941558, 9.307324238869423283, 1.040834085586084257E-14 ) ) ;
#16636 = CARTESIAN_POINT ( 'NONE',  ( 11.94105721237523277, 13.40000000000000036, -1.187919463087249827 ) ) ;
#16638 = CARTESIAN_POINT ( 'NONE',  ( -4.451154503988200339, 4.087435097607984957, 1.214306433183764966E-14 ) ) ;
#16637 = AXIS2_PLACEMENT_3D ( 'NONE', #21550, #87660, #55160 ) ;
#16639 = CARTESIAN_POINT ( 'NONE',  ( -8.016948904382338981, 8.247528564734524892, -0.7998128361456291469 ) ) ;
#16640 = CARTESIAN_POINT ( 'NONE',  ( 0.2335756976950612018, -1.975703151049061024, 0.8776370805363906680 ) ) ;
#16642 = CARTESIAN_POINT ( 'NONE',  ( -4.565105001785453531, 7.177652750280781646, 1.346018956990787885 ) ) ;
#16641 = CARTESIAN_POINT ( 'NONE',  ( -6.611536185319534908, 7.742488966741438716, 1.199719254218452047 ) ) ;
#16643 = CARTESIAN_POINT ( 'NONE',  ( -0.6823417656250003738, 0.9677083336747521747, -1.181850606188749264 ) ) ;
#16644 = CARTESIAN_POINT ( 'NONE',  ( 1.844673738135360175, -0.9321790797625574276, 1.461707330738234667 ) ) ;
#16645 = CARTESIAN_POINT ( 'NONE',  ( 0.7963321702096434196, 1.420339700582837539, 1.005379078535458159 ) ) ;
#16647 = CARTESIAN_POINT ( 'NONE',  ( 5.816084710582486217, 9.729256562414162701, 1.040834085586084257E-14 ) ) ;
#16646 = CARTESIAN_POINT ( 'NONE',  ( 6.375599228498684212, 2.210405824868751701, -0.6629917143727501738 ) ) ;
#16648 = CARTESIAN_POINT ( 'NONE',  ( 3.553118775233146120, 6.302999783484076524, -1.199719254218453823 ) ) ;
#16649 = CARTESIAN_POINT ( 'NONE',  ( 2.495449868850362574, 1.590812333473600626, 1.309970014422021212 ) ) ;
#16650 = CARTESIAN_POINT ( 'NONE',  ( 5.843727902690005749, 6.776436293681846301, -1.199719254218445830 ) ) ;
#16651 = VECTOR ( 'NONE', #114883, 1000.000000000000000 ) ;
#16652 = CARTESIAN_POINT ( 'NONE',  ( 0.8958609827393304581, 0.1455075039201655374, 2.010896580075637541 ) ) ;
#16653 = CARTESIAN_POINT ( 'NONE',  ( 3.475000000000000533, -1.574999999999999956, 0.000000000000000000 ) ) ;
#16654 = CARTESIAN_POINT ( 'NONE',  ( -4.990283058281743678, 7.979691447040783814, -1.199719254218453823 ) ) ;
#16655 = CARTESIAN_POINT ( 'NONE',  ( 6.438356904408193415, 1.850619875698428674, 0.2722718653145329015 ) ) ;
#16657 = CARTESIAN_POINT ( 'NONE',  ( -6.292392690518209264, 8.434487120394948079, -1.443375672974066548 ) ) ;
#16656 = CARTESIAN_POINT ( 'NONE',  ( 4.113462262696740979, 1.539102623358613586, 1.134910093507961237 ) ) ;
#16658 = CARTESIAN_POINT ( 'NONE',  ( 6.568967528192747096, -2.015767819289843388, -0.8987472251835016968 ) ) ;
#16659 = B_SPLINE_CURVE_WITH_KNOTS ( 'NONE', 3,
 ( #97548, #32522, #98597, #24515, #181953, #90625 ),
 .UNSPECIFIED., .F., .F.,
 ( 4, 2, 4 ),
 ( 0.000000000000000000, 0.0003845013059668464604, 0.0007690026119336929207 ),
 .UNSPECIFIED. ) ;
#16660 = CARTESIAN_POINT ( 'NONE',  ( -6.631346530415505036, 7.869564052640446228, 1.082531754730549078 ) ) ;
#16661 = CARTESIAN_POINT ( 'NONE',  ( 7.635176783151273128, 8.936736330878529699, 1.199719254218452935 ) ) ;
#16662 = CARTESIAN_POINT ( 'NONE',  ( -6.084577077482911101, 10.32070003369722144, 0.000000000000000000 ) ) ;
#16663 = CARTESIAN_POINT ( 'NONE',  ( 0.5397205009909338269, -1.917025550485540908, 0.6358503350361620621 ) ) ;
#16664 = ORIENTED_EDGE ( 'NONE', *, *, #27793, .T. ) ;
#16665 = CARTESIAN_POINT ( 'NONE',  ( -0.003376046620573100454, -7.161464053357560644, -9.586610838029425707 ) ) ;
#16666 = CARTESIAN_POINT ( 'NONE',  ( 4.102763937057193999, -0.7201832649769298600, -2.192400882750038971 ) ) ;
#16667 = CARTESIAN_POINT ( 'NONE',  ( 5.107842384611220865, 0.6171798735227496113, -1.862306164846748491 ) ) ;
#16668 = CARTESIAN_POINT ( 'NONE',  ( 2.412880707699780025, -1.519673801815585312, 1.240645658979570909 ) ) ;
#16669 = CARTESIAN_POINT ( 'NONE',  ( 10.73535870392234237, 11.41900666419791399, 0.000000000000000000 ) ) ;
#16670 = CARTESIAN_POINT ( 'NONE',  ( 0.4499999999999712563, 3.949999999999981526, -6.938893903907228378E-15 ) ) ;
#16671 = CARTESIAN_POINT ( 'NONE',  ( 0.6556431738361043760, 2.038855430691276727, -0.5708433468438726122 ) ) ;
#16673 = CARTESIAN_POINT ( 'NONE',  ( -7.320512876374914768, 10.62801655815766999, 1.199719254218453823 ) ) ;
#16672 = CARTESIAN_POINT ( 'NONE',  ( -4.141125853970233806, 6.918731698685530063, -1.199719254218452047 ) ) ;
#16674 = CARTESIAN_POINT ( 'NONE',  ( 0.4625323210639306071, 0.1833022542275381528, -1.831979997761295165 ) ) ;
#16675 = ORIENTED_EDGE ( 'NONE', *, *, #1928, .T. ) ;
#16676 = CARTESIAN_POINT ( 'NONE',  ( 4.680651438812245324, 1.340593046976858771, -1.707629433300766664 ) ) ;
#16677 = CARTESIAN_POINT ( 'NONE',  ( 10.72165486764792952, 9.918110100757866476, -5.398860479493060360 ) ) ;
#16678 = CARTESIAN_POINT ( 'NONE',  ( 1.441811196653530747, -1.994930912159533332, 0.7194735443712959588 ) ) ;
#16679 = CARTESIAN_POINT ( 'NONE',  ( 0.7499999999999902300, 3.597916667349487785, -1.299038105676658228 ) ) ;
#16680 = CARTESIAN_POINT ( 'NONE',  ( 9.077347539549325717, 10.54899253668443393, -1.199719254218446718 ) ) ;
#16681 = CARTESIAN_POINT ( 'NONE',  ( 6.333059215844621725, 6.948315255594014417, 0.8781869475623119703 ) ) ;
#16682 = CIRCLE ( 'NONE', #137789, 11.18000000000000149 ) ;
#16683 = CARTESIAN_POINT ( 'NONE',  ( 1.897801681018367548, -0.6972820500400818133, 1.939346266731331259 ) ) ;
#16685 = DIRECTION ( 'NONE',  ( 5.578174157656880098E-15, 1.000000000000000000, 7.437565543542506798E-15 ) ) ;
#16684 = CARTESIAN_POINT ( 'NONE',  ( -9.016335848287868160, 10.47781223021269170, 1.199719254218462483 ) ) ;
#16686 = CARTESIAN_POINT ( 'NONE',  ( -1.364683531250012516, 2.738541667008090208, -0.7879004041258289570 ) ) ;
#16687 = CARTESIAN_POINT ( 'NONE',  ( 0.07735805125225460321, 2.008365972388022946, -2.502973720202539276 ) ) ;
#16688 = DIRECTION ( 'NONE',  ( 1.000000000000000000, 0.000000000000000000, 0.000000000000000000 ) ) ;
#16689 = CARTESIAN_POINT ( 'NONE',  ( 5.022078740994724733, -1.902695638548990820, 0.1913334245251183119 ) ) ;
#16690 = CARTESIAN_POINT ( 'NONE',  ( 11.86239285000045918, 12.29999999999999716, -1.812080536912752837 ) ) ;
#16691 = CARTESIAN_POINT ( 'NONE',  ( 2.003560550249494199, 1.880309486893988913, 1.257863985149072938 ) ) ;
#16692 = CARTESIAN_POINT ( 'NONE',  ( -3.735435015764967837, 4.316761258935923884, -1.199719254218452047 ) ) ;
#16693 = CARTESIAN_POINT ( 'NONE',  ( 1.353448696812571850, -1.313440895511051032, -1.247944760566013223 ) ) ;
#16694 = CARTESIAN_POINT ( 'NONE',  ( 1.639701460626964868, 1.910339084310968660, -0.1447352371885517186 ) ) ;
#16695 = VECTOR ( 'NONE', #209626, 1000.000000000000000 ) ;
#16696 = CARTESIAN_POINT ( 'NONE',  ( 3.437997351728830697, 1.311287738946330439, 1.602184970737066116 ) ) ;
#16697 = CARTESIAN_POINT ( 'NONE',  ( 1.364683531249986537, 1.217708333674754950, -0.7879004041258239610 ) ) ;
#16698 = CARTESIAN_POINT ( 'NONE',  ( 0.9011734813738042638, 1.610450750236171125, 1.136898926478569383 ) ) ;
#16699 = CARTESIAN_POINT ( 'NONE',  ( 5.057218277682078877, -1.628452160524866521, -1.029070375190293873 ) ) ;
#16701 = CARTESIAN_POINT ( 'NONE',  ( 5.925280661667059690, 7.134359284303951831, -1.114000666120490868 ) ) ;
#16700 = CARTESIAN_POINT ( 'NONE',  ( 0.8917866929778429652, 2.032703844138737725, -1.092514170908296833 ) ) ;
#16702 = CARTESIAN_POINT ( 'NONE',  ( -1.402160292154681736E-14, 1.696875000341421469, -1.575800808251659024 ) ) ;
#16703 = CARTESIAN_POINT ( 'NONE',  ( 5.020015070024019366, 2.040704184028362178, -0.2994381943521097766 ) ) ;
#16704 = CARTESIAN_POINT ( 'NONE',  ( -5.168682875307782254, 7.053215992657626110, -1.599625672291256295 ) ) ;
#16705 = CARTESIAN_POINT ( 'NONE',  ( 7.800018446563675489, 7.994443030612759848, -0.7998128361456281477 ) ) ;
#16706 = CARTESIAN_POINT ( 'NONE',  ( -1.257539916218630927, 2.908837156058346807, 0.7750000000000117906 ) ) ;
#16708 = CARTESIAN_POINT ( 'NONE',  ( 1.499999999999987121, 4.795833333333353821, -0.8660254037844323793 ) ) ;
#16707 = CARTESIAN_POINT ( 'NONE',  ( 6.335009839202000670, 0.2025031609870796001, 2.096191850513532184 ) ) ;
#16709 = CARTESIAN_POINT ( 'NONE',  ( 1.364683531249988535, 2.426041667008088432, 0.7879004041258500513 ) ) ;
#16710 = CARTESIAN_POINT ( 'NONE',  ( 4.850933092205481856, -1.739298515662604405, 1.283314429840809234 ) ) ;
#16711 = CARTESIAN_POINT ( 'NONE',  ( 5.039715841750210146, -1.917062458738912012, 0.6357382205050918778 ) ) ;
#16712 = DIRECTION ( 'NONE',  ( 0.000000000000000000, 0.000000000000000000, 1.000000000000000000 ) ) ;
#16713 = CARTESIAN_POINT ( 'NONE',  ( -5.910991785878175975, 6.958873840688411860, -1.082531754730544860 ) ) ;
#16716 = CARTESIAN_POINT ( 'NONE',  ( 4.799223189557548785, 7.582548906917042864, -1.082531754730549078 ) ) ;
#16715 = CARTESIAN_POINT ( 'NONE',  ( 1.001543065824772753E-15, -2.121874999522043836, 3.793834371823811669 ) ) ;
#16714 = CARTESIAN_POINT ( 'NONE',  ( 5.515134625708930649, 9.656350506627580543, 0.000000000000000000 ) ) ;
#16717 = CARTESIAN_POINT ( 'NONE',  ( -3.481411583659053566, 7.283673624236017830, 0.000000000000000000 ) ) ;
#16718 = CARTESIAN_POINT ( 'NONE',  ( 3.397672961473942266, -1.985868886743065609, 0.3494831190506141883 ) ) ;
#16719 = CARTESIAN_POINT ( 'NONE',  ( -9.016335848287868160, 10.47781223021269170, 1.199719254218462483 ) ) ;
#16721 = CARTESIAN_POINT ( 'NONE',  ( 1.579999999999989413, 6.280000000000042881, -2.579999999999995630 ) ) ;
#16720 = CARTESIAN_POINT ( 'NONE',  ( -10.03267048443264109, 11.76749898900197877, 1.082531754730558626 ) ) ;
#16722 = CARTESIAN_POINT ( 'NONE',  ( -1.364683531250010295, 5.488541667008087543, -0.7879004041258300672 ) ) ;
#16724 = CARTESIAN_POINT ( 'NONE',  ( -11.89204169242383458, 12.30000000000000071, -0.8046421800350854747 ) ) ;
#16723 = CARTESIAN_POINT ( 'NONE',  ( 5.418883921851007202, 1.995750516393671514, 0.8311057252617033431 ) ) ;
#16725 = FILL_AREA_STYLE ('',( #17784 ) ) ;
#16726 = CARTESIAN_POINT ( 'NONE',  ( -11.72847922660204034, 7.461677940835538259, 2.549820816093626430 ) ) ;
#16728 = CARTESIAN_POINT ( 'NONE',  ( 5.659779856126235131, 1.203369751103126717, 1.617807692209995984 ) ) ;
#16727 = CARTESIAN_POINT ( 'NONE',  ( -6.168596704093453731, 10.14052055484361325, 0.7216878364870458196 ) ) ;
#16729 = CARTESIAN_POINT ( 'NONE',  ( -1.402160292154681736E-14, -0.1156249996585793222, 1.575800808251672791 ) ) ;
#16730 = CARTESIAN_POINT ( 'NONE',  ( 0.8731895615166852531, 1.663438651979048277, -0.4559567554138827528 ) ) ;
#16731 = CARTESIAN_POINT ( 'NONE',  ( 5.520104819419390907, 6.469152373191302985, 1.199719254218452935 ) ) ;
#16733 = CARTESIAN_POINT ( 'NONE',  ( 7.517069824134078537, 7.734612647770044092, 0.000000000000000000 ) ) ;
#16732 = CARTESIAN_POINT ( 'NONE',  ( 7.456621297836067086, 10.68284669990868174, 1.082531754730558626 ) ) ;
#16734 = CARTESIAN_POINT ( 'NONE',  ( -3.402733366905634327, 6.913679994791067429, 0.7216878364870540352 ) ) ;
#16735 = CARTESIAN_POINT ( 'NONE',  ( 0.2096995604969940641, -0.7494040810181783474, -1.602093636072899008 ) ) ;
#16736 = CARTESIAN_POINT ( 'NONE',  ( 1.190090860395363492, 1.200783890555771283, 1.615600688039710020 ) ) ;
#16737 = CARTESIAN_POINT ( 'NONE',  ( -4.234859498635395347, 3.979834430640218468, 0.5021729129214658194 ) ) ;
#16738 =( GEOMETRIC_REPRESENTATION_CONTEXT ( 3 ) GLOBAL_UNCERTAINTY_ASSIGNED_CONTEXT ( ( #20359 ) ) GLOBAL_UNIT_ASSIGNED_CONTEXT ( ( #16274, #15220, #184119 ) ) REPRESENTATION_CONTEXT ( 'NONE', 'WORKASPACE' ) );
#16739 = CARTESIAN_POINT ( 'NONE',  ( -7.580417283372126391, 8.016444050121833698, 0.7216878364870317197 ) ) ;
#16740 = ORIENTED_EDGE ( 'NONE', *, *, #109311, .T. ) ;
#16741 = CARTESIAN_POINT ( 'NONE',  ( 8.039621902779343188, 12.32338328664385507, -0.7216878364870328300 ) ) ;
#16743 = CARTESIAN_POINT ( 'NONE',  ( 1.810172953844836119, 1.158670025852935437, -1.650096248209936167 ) ) ;
#16742 = CARTESIAN_POINT ( 'NONE',  ( 2.631617588254760776, -0.2053842346896698201, 2.110501108333342035 ) ) ;
#16744 = CARTESIAN_POINT ( 'NONE',  ( 2.179683618226692321, 1.775955819808447966, -0.3565394459093262358 ) ) ;
#16745 = CARTESIAN_POINT ( 'NONE',  ( 5.501576472095266901, 9.640532660744973725, -0.7998128361456481317 ) ) ;
#16746 = EDGE_CURVE ( 'NONE', #184334, #107993, #107683, .T. ) ;
#16747 = CARTESIAN_POINT ( 'NONE',  ( 6.051685545382852638, 0.6321331830463626789, -2.067208725892249799 ) ) ;
#16748 = ADVANCED_FACE ( 'NONE', ( #174774 ), #24203, .T. ) ;
#16749 = CARTESIAN_POINT ( 'NONE',  ( 7.447506452608354088, 7.583179037664891098, 0.7998128361456341429 ) ) ;
#16751 = CARTESIAN_POINT ( 'NONE',  ( 0.5146670378583360073, 0.1438656263933698054, 1.910404373559170477 ) ) ;
#16750 = CARTESIAN_POINT ( 'NONE',  ( -4.391951695823077984, 7.211361847513815704, 1.199719254218464037 ) ) ;
#16752 = AXIS2_PLACEMENT_3D ( 'NONE', #74669, #61611, #139694 ) ;
#16753 = CARTESIAN_POINT ( 'NONE',  ( 0.3870405448657153191, 1.264806443676224301, -11.85654951141427560 ) ) ;
#16754 = LINE ( 'NONE', #101215, #176720 ) ;
#16755 = CARTESIAN_POINT ( 'NONE',  ( 6.466876083594112146, 6.647036307055676829, -0.7216878364870257245 ) ) ;
#16756 = CARTESIAN_POINT ( 'NONE',  ( -1.402160292154681736E-14, 0.2593750003414224681, -1.575800808251665908 ) ) ;
#16757 = CARTESIAN_POINT ( 'NONE',  ( 4.216222584169931231, 4.021273891060765493, 1.214306433183764966E-14 ) ) ;
#16758 = CARTESIAN_POINT ( 'NONE',  ( -7.797910906154257304, 12.24931315715533486, 0.000000000000000000 ) ) ;
#16759 = CARTESIAN_POINT ( 'NONE',  ( 4.311504812833309330, -0.3723461477018601418, 2.129241309423899775 ) ) ;
#16760 = CARTESIAN_POINT ( 'NONE',  ( -5.424670859243583720, 8.382514198209223721, 1.082531754730550855 ) ) ;
#16761 = CARTESIAN_POINT ( 'NONE',  ( 4.990809943606266508, 6.915973915664348937, -1.443375672974068769 ) ) ;
#16762 = CARTESIAN_POINT ( 'NONE',  ( 2.373420902723611725, -1.847293605357634982, -1.041186957106011723 ) ) ;
#16763 = CARTESIAN_POINT ( 'NONE',  ( 3.486133158594716510E-16, 2.437499999999986677, -1.225000000000021849 ) ) ;
#16764 = CARTESIAN_POINT ( 'NONE',  ( 3.743400255998735382, -1.490684086824107357, -1.290067496309046158 ) ) ;
#16765 = CARTESIAN_POINT ( 'NONE',  ( 5.730699431777452446, 1.279516236652695316, -1.421498520143074540 ) ) ;
#16766 = ORIENTED_EDGE ( 'NONE', *, *, #187556, .F. ) ;
#16767 = DIRECTION ( 'NONE',  ( 1.276756478318932585E-15, -1.000000000000000000, 1.665334536937738262E-16 ) ) ;
#16768 = CARTESIAN_POINT ( 'NONE',  ( 5.969198390587827419, 1.736284540159404033, 0.9297856951416498816 ) ) ;
#16769 = CARTESIAN_POINT ( 'NONE',  ( 1.411946100005515126, 1.304364503314077162, -1.438846909250802053 ) ) ;
#16770 = ORIENTED_EDGE ( 'NONE', *, *, #29782, .F. ) ;
#16771 = CARTESIAN_POINT ( 'NONE',  ( -4.014095998097799267, 6.840806543492835345, -1.199719254218450271 ) ) ;
#16773 = CARTESIAN_POINT ( 'NONE',  ( -2.346281263894411939E-15, -6.452016312669646148, 11.25751254361626685 ) ) ;
#16772 = CARTESIAN_POINT ( 'NONE',  ( -5.139949633356594383, 9.010708648975750634, 0.000000000000000000 ) ) ;
#16775 = CARTESIAN_POINT ( 'NONE',  ( 8.118635056484817980, 8.366162408854107113, 0.7998128361456481317 ) ) ;
#16774 = CARTESIAN_POINT ( 'NONE',  ( 2.044979492446592939, -1.679722130475280961, -1.244493991799436650 ) ) ;
#16777 = CARTESIAN_POINT ( 'NONE',  ( 4.326460416092276162, 7.101268681199365496, -1.082531754730548412 ) ) ;
#16776 = CARTESIAN_POINT ( 'NONE',  ( 6.795661308947685164, 8.951357498570873261, -1.599625672291262513 ) ) ;
#16779 = VERTEX_POINT ( 'NONE', #94588 ) ;
#16778 = CARTESIAN_POINT ( 'NONE',  ( 6.463533315534490065, -1.538886664202097965, -1.134999244291827747 ) ) ;
#16780 = CARTESIAN_POINT ( 'NONE',  ( 4.758537496233657293, 0.8426522330295079799, 2.039869969286691731 ) ) ;
#16781 = CARTESIAN_POINT ( 'NONE',  ( 2.274722540679521288, -1.357913018379176995, 1.739418515187239223 ) ) ;
#16782 =( LENGTH_UNIT ( ) NAMED_UNIT ( * ) SI_UNIT ( .MILLI., .METRE. ) );
#16783 = CARTESIAN_POINT ( 'NONE',  ( 0.7856316122640573107, 1.842795011522216697, -0.5104879603500325214 ) ) ;
#16784 = LINE ( 'NONE', #99141, #93936 ) ;
#16785 = CARTESIAN_POINT ( 'NONE',  ( 11.33772463945043718, 13.40000000000000924, -3.600000000000078693 ) ) ;
#16786 = CARTESIAN_POINT ( 'NONE',  ( 3.912603064140641518, 0.7423916865902053797, 1.932869565047180327 ) ) ;
#16787 = CARTESIAN_POINT ( 'NONE',  ( -3.899941742225307539, 7.701682465904834629, 0.7998128361456341429 ) ) ;
#16789 = CARTESIAN_POINT ( 'NONE',  ( 1.920999885407469243, 2.016935458891587096, 0.7782144962657986387 ) ) ;
#16788 = CARTESIAN_POINT ( 'NONE',  ( 0.1412570932018001879, -6.646059016331635760, 10.87798840695972657 ) ) ;
#16790 = CARTESIAN_POINT ( 'NONE',  ( 3.544632465004614374, -1.790652189326558563, 1.263247045326252094 ) ) ;
#16791 = CARTESIAN_POINT ( 'NONE',  ( -4.124095526617549778E-13, -0.9769569599453676867, 3.449959810851647823 ) ) ;
#16792 =( NAMED_UNIT ( * ) PLANE_ANGLE_UNIT ( ) SI_UNIT ( $, .RADIAN. ) );
#16793 = DIRECTION ( 'NONE',  ( -1.000000000000000000, 1.045014142154703195E-15, 0.000000000000000000 ) ) ;
#16794 = CARTESIAN_POINT ( 'NONE',  ( 0.6823417656249969321, 14.58854166700806410, -1.181850606188757036 ) ) ;
#16795 = CARTESIAN_POINT ( 'NONE',  ( -5.815521545619021460, 5.749472989502435460, -0.7998128361456362523 ) ) ;
#16796 = CARTESIAN_POINT ( 'NONE',  ( 5.783786074351109363, 1.412321387942861328, -1.005976269456631211 ) ) ;
#16797 = CARTESIAN_POINT ( 'NONE',  ( -10.03267048443264109, 11.76749898900197877, 1.082531754730558626 ) ) ;
#16798 = CARTESIAN_POINT ( 'NONE',  ( 4.715722526854881913, 0.4587184135333640111, -2.018627749927892179 ) ) ;
#16799 = CARTESIAN_POINT ( 'NONE',  ( 5.220359425914078422, 2.086072958538415012, 0.3609885457144176302 ) ) ;
#16800 = CARTESIAN_POINT ( 'NONE',  ( 7.122110765880372618, 7.203550736482235095, 0.7998128361456341429 ) ) ;
#16801 = FACE_BOUND ( 'NONE', #23516, .T. ) ;
#16802 = CARTESIAN_POINT ( 'NONE',  ( 2.588665490599820096, 1.909050991929973629, 0.4833708566103470661 ) ) ;
#16803 = CARTESIAN_POINT ( 'NONE',  ( 5.701222307317492799, -0.5618967582242094805, 2.222226568792139645 ) ) ;
#16804 = CARTESIAN_POINT ( 'NONE',  ( 2.508196354075361789, -0.6984789837382252564, -1.686990664346368796 ) ) ;
#16805 = CARTESIAN_POINT ( 'NONE',  ( 3.984117037569365305, 5.741498858621315371, 1.599625672291261402 ) ) ;
#16807 = EDGE_CURVE ( 'NONE', #166496, #128985, #145500, .T. ) ;
#16806 = CARTESIAN_POINT ( 'NONE',  ( 3.673896439178918172, 6.269667698141953238, 1.082531754730558626 ) ) ;
#16808 = CARTESIAN_POINT ( 'NONE',  ( -6.531277313481209212, 8.642909503859968368, 1.599625672291283607 ) ) ;
#16809 = CARTESIAN_POINT ( 'NONE',  ( 4.746236293235721604, 7.694970221153795364, 1.199719254218451159 ) ) ;
#16810 = ORIENTED_EDGE ( 'NONE', *, *, #116226, .T. ) ;
#16811 = ORIENTED_EDGE ( 'NONE', *, *, #179751, .T. ) ;
#16812 = CARTESIAN_POINT ( 'NONE',  ( 3.867443265902783534, -1.676145683993632618, -1.114854040202686969 ) ) ;
#16813 = CARTESIAN_POINT ( 'NONE',  ( 4.785966450049039089, -1.203721183051874810, -1.548998264137561254 ) ) ;
#16814 = CARTESIAN_POINT ( 'NONE',  ( -5.194745412330402878, 9.212286747694129474, 0.000000000000000000 ) ) ;
#16815 = CARTESIAN_POINT ( 'NONE',  ( -4.680589345215810049, 6.483773540883647435, -1.599625672291256295 ) ) ;
#16816 =( NAMED_UNIT ( * ) PLANE_ANGLE_UNIT ( ) SI_UNIT ( $, .RADIAN. ) );
#16818 = CARTESIAN_POINT ( 'NONE',  ( 6.192257685097896314, -1.761771181780842577, -0.1690057029742654260 ) ) ;
#16817 = CARTESIAN_POINT ( 'NONE',  ( 0.1696251593464107033, 1.207222248521317765, 1.706790159955206887 ) ) ;
#16819 = CARTESIAN_POINT ( 'NONE',  ( 11.33772463945037146, 13.39999999999998259, 3.679999999999999272 ) ) ;
#16820 = CARTESIAN_POINT ( 'NONE',  ( 2.062683196291382082, -2.004346222996217897, -0.8864330828558324438 ) ) ;
#16821 = CARTESIAN_POINT ( 'NONE',  ( 0.8545597497816240784, 0.3412253653619911065, -1.706464705969434670 ) ) ;
#16822 = VECTOR ( 'NONE', #209264, 1000.000000000000114 ) ;
#16823 = CARTESIAN_POINT ( 'NONE',  ( 6.311484202361478779, 7.322151976631905868, -1.199719254218446718 ) ) ;
#16824 = CARTESIAN_POINT ( 'NONE',  ( 0.2335667940002320309, 1.326312899344052276, -2.404742575607053734 ) ) ;
#16825 = CARTESIAN_POINT ( 'NONE',  ( 0.4160739966224377140, 1.193427498895651029, -1.245624518738875697 ) ) ;
#16826 = CARTESIAN_POINT ( 'NONE',  ( 0.8436309607196719185, -1.274966737007717343, 1.912178556870794521 ) ) ;
#16828 = EDGE_CURVE ( 'NONE', #71815, #212637, #195967, .T. ) ;
#16827 = CARTESIAN_POINT ( 'NONE',  ( -0.04112450405316381286, -1.960553898366865555, -0.9795403211517728082 ) ) ;
#16829 = CARTESIAN_POINT ( 'NONE',  ( 2.737190076726934151, 0.2709513247245790013, 2.190122135706531914 ) ) ;
#16830 = CARTESIAN_POINT ( 'NONE',  ( 1.481551236908748237, -0.05589941666775917473, 2.170521761658677828 ) ) ;
#16831 = CARTESIAN_POINT ( 'NONE',  ( -0.01727558406095473439, -0.1313277740116538805, -1.795991579427682616 ) ) ;
#16832 = CARTESIAN_POINT ( 'NONE',  ( 2.624332661740484962, 2.101919520188862744, 0.2543673568942694252 ) ) ;
#16833 = CARTESIAN_POINT ( 'NONE',  ( 6.827182134110222123, 4.687887262399931920, 2.751577338787388083 ) ) ;
#16834 = CARTESIAN_POINT ( 'NONE',  ( 5.860362583224701716, 0.7811062513497173398, 1.761092865462327239 ) ) ;
#16835 = VERTEX_POINT ( 'NONE', #144429 ) ;
#16836 = CONICAL_SURFACE ( 'NONE', #134414, 11.53746066217573762, 0.1181278931043537039 ) ;
#16838 = CARTESIAN_POINT ( 'NONE',  ( -1.364683531250014514, 0.05104166700808546175, -0.7879004041258359514 ) ) ;
#16837 = CARTESIAN_POINT ( 'NONE',  ( 2.068323803795060645, -1.406806521851681424, 1.809881060044524093 ) ) ;
#16839 = CARTESIAN_POINT ( 'NONE',  ( 3.765413976293345844, 5.416068943807445635, 1.599625672291267398 ) ) ;
#16840 = CARTESIAN_POINT ( 'NONE',  ( 3.493197133815315603, 7.227147089426516402, -0.7998128361456291469 ) ) ;
#16841 = CARTESIAN_POINT ( 'NONE',  ( 4.828890449103202975, 1.532327986240004103, -1.608379539844583705 ) ) ;
#16842 = CARTESIAN_POINT ( 'NONE',  ( -8.541273586929371220, 9.067166727613487964, 0.7216878364870438212 ) ) ;
#16843 = CARTESIAN_POINT ( 'NONE',  ( -0.1309013025973339017, -5.411711732698793575, -10.96028113393447256 ) ) ;
#16844 = CARTESIAN_POINT ( 'NONE',  ( 4.690757960648213931, 8.416375354157496602, 0.7216878364870438212 ) ) ;
#16845 = CARTESIAN_POINT ( 'NONE',  ( -6.033015167956794933, 9.982342096017511324, -0.7216878364870267237 ) ) ;
#16846 = CARTESIAN_POINT ( 'NONE',  ( 4.258669648468278446, 7.022179452304728287, 1.082531754730549078 ) ) ;
#16847 = ORIENTED_EDGE ( 'NONE', *, *, #45640, .F. ) ;
#16848 = CARTESIAN_POINT ( 'NONE',  ( 2.883435573726996548, -0.5880205015329244000, -1.928751729079546173 ) ) ;
#16850 = CARTESIAN_POINT ( 'NONE',  ( 1.252863987647494515, -0.4972004349026898362, -2.001653351804733028 ) ) ;
#16849 = CARTESIAN_POINT ( 'NONE',  ( 5.452350330990040739, 9.512825819463730070, 0.7998128361456462443 ) ) ;
#16851 = CARTESIAN_POINT ( 'NONE',  ( 4.892490983285298967, 4.880530033246584409, 0.06831354469134912066 ) ) ;
#16852 = CARTESIAN_POINT ( 'NONE',  ( 5.695833931072550094, 5.817763472438987726, 0.000000000000000000 ) ) ;
#16853 = B_SPLINE_CURVE_WITH_KNOTS ( 'NONE', 3,
 ( #195816, #27186, #47455, #171307, #89017, #204849, #73814, #139907, #32249, #19183 ),
 .UNSPECIFIED., .F., .F.,
 ( 4, 3, 3, 4 ),
 ( 0.000000000000000000, 6.198155766681710474E-05, 0.0001239631899706914050, 0.0002326595646014659722 ),
 .UNSPECIFIED. ) ;
#16855 = ADVANCED_FACE ( 'NONE', ( #111956 ), #160630, .F. ) ;
#16854 = CARTESIAN_POINT ( 'NONE',  ( 1.499999999999993117, 8.635416667349460340, 0.8660254037844408170 ) ) ;
#16856 = CARTESIAN_POINT ( 'NONE',  ( -1.364683531249997417, 3.259375000341423245, 1.214306433183764966E-14 ) ) ;
#16857 = CARTESIAN_POINT ( 'NONE',  ( 4.435597005726048536, 0.9382243502508281763, -1.980580373504265301 ) ) ;
#16858 = CARTESIAN_POINT ( 'NONE',  ( 1.090470458312575053, -0.4872005951904456733, 1.956561897242928172 ) ) ;
#16859 = CARTESIAN_POINT ( 'NONE',  ( 1.399689850468607277, -0.6632477835330424787, -1.717811453623831808 ) ) ;
#16860 = CARTESIAN_POINT ( 'NONE',  ( 4.751808913491627706, 0.7073710267669359730, 1.700028372310140368 ) ) ;
#16861 = EDGE_CURVE ( 'NONE', #84638, #18660, #116530, .T. ) ;
#16862 = CARTESIAN_POINT ( 'NONE',  ( 7.771848369131631351, 10.09024240211882351, -1.599625672291262513 ) ) ;
#16863 = FILL_AREA_STYLE ('',( #165268 ) ) ;
#16864 = CARTESIAN_POINT ( 'NONE',  ( 5.420859398437725574, 1.687492901312273474, 0.6969783729503381542 ) ) ;
#16865 = CARTESIAN_POINT ( 'NONE',  ( 6.135388727473008785, 0.6351960432287793168, 1.913804721665197883 ) ) ;
#16866 = CARTESIAN_POINT ( 'NONE',  ( -9.124801077197171040, 10.60435499727357289, -1.199719254218441611 ) ) ;
#16868 = CARTESIAN_POINT ( 'NONE',  ( -6.252245114557387851, 7.323316050852266557, -1.199719254218453823 ) ) ;
#16867 = CARTESIAN_POINT ( 'NONE',  ( 5.120128864776952504, -1.205885850527373293, -1.914207236704228654 ) ) ;
#16869 = CARTESIAN_POINT ( 'NONE',  ( 0.5398470734442856189, -1.490880511344143011, -1.487817205855391789 ) ) ;
#16870 = CARTESIAN_POINT ( 'NONE',  ( 4.932118098221458524, 1.189261692661430114, 1.694535115018414917 ) ) ;
#16871 = CARTESIAN_POINT ( 'NONE',  ( 9.297140650669039275, 11.86975006391249643, 1.599625672291281386 ) ) ;
#16872 = SURFACE_STYLE_USAGE ( .BOTH. , #179418 ) ;
#16873 = APPLICATION_PROTOCOL_DEFINITION ( 'draft international standard', 'automotive_design', 1998, #169602 ) ;
#16874 = CARTESIAN_POINT ( 'NONE',  ( -7.557780564614042795, 10.90482886110335414, -1.199719254218446718 ) ) ;
#16875 = PRESENTATION_STYLE_ASSIGNMENT (( #180474 ) ) ;
#16876 = CARTESIAN_POINT ( 'NONE',  ( 7.201315867513990554, 8.430565262634994284, -1.199719254218452047 ) ) ;
#16877 = CARTESIAN_POINT ( 'NONE',  ( 4.825424889954152086, 6.722588627200480893, -1.249340337910074705 ) ) ;
#16878 = CARTESIAN_POINT ( 'NONE',  ( -3.358669367883384105, 4.941533567329135401, -1.599625672291262513 ) ) ;
#16880 = CARTESIAN_POINT ( 'NONE',  ( 1.723182734256373916, 1.642088205692782132, -1.496221191757711066 ) ) ;
#16879 = CARTESIAN_POINT ( 'NONE',  ( 1.160570123509139906, 2.118417766304943495, 0.09849428607798524360 ) ) ;
#16881 = CARTESIAN_POINT ( 'NONE',  ( -1.500000000000079270, 7.360305807095733677, 4.205660139708331080 ) ) ;
#16882 = CARTESIAN_POINT ( 'NONE',  ( -8.086512275908061653, 8.398962174839683215, 0.000000000000000000 ) ) ;
#16883 = CARTESIAN_POINT ( 'NONE',  ( 5.099838337034727331, 9.101561826515851550, -0.7998128361456281477 ) ) ;
#16884 = CARTESIAN_POINT ( 'NONE',  ( 2.840232074097197579, -1.010955899468408248, 1.681206195012739046 ) ) ;
#16885 = CARTESIAN_POINT ( 'NONE',  ( 4.313465427442102929, 8.184126765324453601, 0.7998128361456462443 ) ) ;
#16886 = CARTESIAN_POINT ( 'NONE',  ( -4.055583655087145800, 7.567422049930973671, -0.4132208808486706464 ) ) ;
#16887 = CARTESIAN_POINT ( 'NONE',  ( 4.334856428067313416, 6.080418470877079429, -1.599625672291256295 ) ) ;
#16888 = CARTESIAN_POINT ( 'NONE',  ( -4.990809943606269172, 8.836712344267034780, -0.7216878364870338292 ) ) ;
#16889 = CARTESIAN_POINT ( 'NONE',  ( -7.022760382198764084, 11.13704484596649635, 0.7216878364870458196 ) ) ;
#16891 = CARTESIAN_POINT ( 'NONE',  ( 2.285534418239891785, 0.09939759515392716793, -2.118372479656557061 ) ) ;
#16890 = AXIS2_PLACEMENT_3D ( 'NONE', #145836, #63478, #127508 ) ;
#16892 = CARTESIAN_POINT ( 'NONE',  ( -7.110325215724114578, 7.260077271291732082, 0.000000000000000000 ) ) ;
#16893 = CARTESIAN_POINT ( 'NONE',  ( 3.930091730393743710, 1.087902980620155891, 1.632394305395828304 ) ) ;
#16894 = CARTESIAN_POINT ( 'NONE',  ( 3.538091169922503276, 0.9737216987566952309, -1.930062384640649054 ) ) ;
#16895 = CARTESIAN_POINT ( 'NONE',  ( 2.454439063956286304, -1.602943312447857593, -0.9057913635923324769 ) ) ;
#16896 = CARTESIAN_POINT ( 'NONE',  ( -4.295541959788370612, 7.266047401097770475, -0.9601269197386901322 ) ) ;
#16897 = CARTESIAN_POINT ( 'NONE',  ( 0.6823417656249882723, -0.8447916663252494907, 1.181850606188755259 ) ) ;
#16898 = CARTESIAN_POINT ( 'NONE',  ( 4.470479574576804005, -0.003715868306445029284, -1.740516468156935836 ) ) ;
#16899 = CARTESIAN_POINT ( 'NONE',  ( -7.247736482492233456, 16.00000000000443023, -10.57961706324464402 ) ) ;
#16900 = CARTESIAN_POINT ( 'NONE',  ( 4.853455804012222430, 5.725081861844796727, 1.082531754730560403 ) ) ;
#16901 = CARTESIAN_POINT ( 'NONE',  ( -0.4373347461412381287, -7.712532583864843083, 10.97876033714414135 ) ) ;
#16902 = CARTESIAN_POINT ( 'NONE',  ( 2.395597313961893349, 1.670541196947441520, 1.371929806955954012 ) ) ;
#16903 = CARTESIAN_POINT ( 'NONE',  ( 4.727888646976695419, -1.799647678597478206, -0.9090046787488814672 ) ) ;
#16904 = CARTESIAN_POINT ( 'NONE',  ( -8.961576348508641487, 11.47825837805867799, -1.443375672974058777 ) ) ;
#16905 = CIRCLE ( 'NONE', #196754, 0.08000000000000009881 ) ;
#16906 = CARTESIAN_POINT ( 'NONE',  ( 1.797963993548271411, -0.7283430984801853025, 2.035426966748521860 ) ) ;
#16907 = CARTESIAN_POINT ( 'NONE',  ( 3.520352277729906998, 1.251605784994310300, -1.523194303571529185 ) ) ;
#16908 = CARTESIAN_POINT ( 'NONE',  ( 2.934795777137487516, 0.2378783870938088740, 1.956871125110821952 ) ) ;
#16909 = DIRECTION ( 'NONE',  ( 1.000000000000000000, 0.000000000000000000, 0.000000000000000000 ) ) ;
#16910 = CARTESIAN_POINT ( 'NONE',  ( 3.913568440338021315, -1.001196544591560933, -1.663976088286099886 ) ) ;
#16913 = ORIENTED_EDGE ( 'NONE', *, *, #186479, .F. ) ;
#16912 = CARTESIAN_POINT ( 'NONE',  ( -1.326716514427061987E-15, 2.999999999999988454, -1.225000000000003864 ) ) ;
#16911 = CARTESIAN_POINT ( 'NONE',  ( -10.10046125205659173, 10.88621900359527572, -0.7216878364870267237 ) ) ;
#16914 = CARTESIAN_POINT ( 'NONE',  ( -2.984203208339354152, 6.495671153122273722, 0.000000000000000000 ) ) ;
#16915 = CARTESIAN_POINT ( 'NONE',  ( 4.573896719763862251, 6.429575154514868274, -1.599625672291273171 ) ) ;
#16916 = CARTESIAN_POINT ( 'NONE',  ( -5.794130544993808307, 7.853181283949808744, 1.599625672291263179 ) ) ;
#16917 = CARTESIAN_POINT ( 'NONE',  ( -7.809133291347029271, 12.05447990663947877, 0.000000000000000000 ) ) ;
#16918 = CARTESIAN_POINT ( 'NONE',  ( 1.167327668269029228, -1.995579438226593894, -0.9423882379527288577 ) ) ;
#16919 = CARTESIAN_POINT ( 'NONE',  ( 3.285556943750000514, -3.813541666188710710, 1.896917185911906500 ) ) ;
#16920 = CARTESIAN_POINT ( 'NONE',  ( 5.084793414397763556, 1.876112756342168675, 0.5732009990792874543 ) ) ;
#16921 = VERTEX_POINT ( 'NONE', #161716 ) ;
#16922 = CARTESIAN_POINT ( 'NONE',  ( 3.784452290478927505, -0.6679156082517538895, -2.009268603764336358 ) ) ;
#16923 = CARTESIAN_POINT ( 'NONE',  ( -1.201851678989727383E-14, 2.493750000682819046, 1.732050807568877637 ) ) ;
#16925 = CARTESIAN_POINT ( 'NONE',  ( -5.205440912643032547, 8.160432600470439723, 1.199719254218452047 ) ) ;
#16924 = CARTESIAN_POINT ( 'NONE',  ( 0.1745949693968510408, 0.7659234433113177865, -1.841618699378000601 ) ) ;
#16926 = CARTESIAN_POINT ( 'NONE',  ( 3.960763856159645879, 0.2235175650571289141, -1.827449369368571386 ) ) ;
#16927 = VERTEX_POINT ( 'NONE', #64206 ) ;
#16928 = ADVANCED_FACE ( 'NONE', ( #113021 ), #189146, .T. ) ;
#16929 = CARTESIAN_POINT ( 'NONE',  ( -7.537443334193545397, 10.88110209227943770, -1.199719254218446718 ) ) ;
#16930 = CARTESIAN_POINT ( 'NONE',  ( 5.027636390373714903, -0.3086946445357250379, 2.097867224209007730 ) ) ;
#16931 = CARTESIAN_POINT ( 'NONE',  ( 0.000000000000000000, -2.079999999999998295, 10.91999999999999105 ) ) ;
#16932 = CARTESIAN_POINT ( 'NONE',  ( 5.717788096661236885, 7.693838750903348789, 1.599625672291267398 ) ) ;
#16933 = CARTESIAN_POINT ( 'NONE',  ( 5.501267734246070518, 1.682208477397129975, 1.190076826167464352 ) ) ;
#16934 = TOROIDAL_SURFACE ( 'NONE', #165701, 11.92000000000000348, 0.08000000000000000167 ) ;
#16937 = CARTESIAN_POINT ( 'NONE',  ( 2.559893532628489954, -1.268187297466142338, 1.335118840784771166 ) ) ;
#16936 = CARTESIAN_POINT ( 'NONE',  ( 1.258004785490075994, -1.861241886096485221, -0.004951839839751126689 ) ) ;
#16935 = CARTESIAN_POINT ( 'NONE',  ( -3.810548893104253487, 8.469546410357084554, -2.499999999999999112 ) ) ;
#16938 = CARTESIAN_POINT ( 'NONE',  ( 6.923409998072794558, 11.22906209772695618, 1.040834085586084257E-14 ) ) ;
#16939 = FACE_OUTER_BOUND ( 'NONE', #130765, .T. ) ;
#16940 =( BOUNDED_CURVE ( )  B_SPLINE_CURVE ( 2, ( #75776, #22729, #123556 ),
 .UNSPECIFIED., .F., .T. ) 
 B_SPLINE_CURVE_WITH_KNOTS ( ( 3, 3 ),
 ( 0.4750000000000003664, 0.4832995304647380586 ),
 .UNSPECIFIED. ) 
 CURVE ( )  GEOMETRIC_REPRESENTATION_ITEM ( )  RATIONAL_B_SPLINE_CURVE ( ( 0.9999999999999937828, 0.8665688508649624922, 0.9989175146558251228 ) ) 
 REPRESENTATION_ITEM ( '' )  );
#16941 = CARTESIAN_POINT ( 'NONE',  ( -4.821467422361007671, 5.083637263933393768, -0.9394917190213262215 ) ) ;
#16942 = CARTESIAN_POINT ( 'NONE',  ( -0.008219159353565024667, -7.627132808484227589, -9.567202289542832361 ) ) ;
#16943 = CARTESIAN_POINT ( 'NONE',  ( 2.596532132193625664, -2.201043451360765957, -0.1612727490639675743 ) ) ;
#16944 = CARTESIAN_POINT ( 'NONE',  ( 5.184992917819648994, -0.2698046931138863846, -2.246192962944548732 ) ) ;
#16945 = CARTESIAN_POINT ( 'NONE',  ( -7.714226216495749355, 8.102278128774251797, 1.040834085586084257E-14 ) ) ;
#16946 = CARTESIAN_POINT ( 'NONE',  ( 5.132992444152020717, 1.676870426783064083, 0.6860526005390086279 ) ) ;
#16947 = CARTESIAN_POINT ( 'NONE',  ( 5.049963001771692106, 0.9498492218114750196, 1.663612537209507858 ) ) ;
#16948 = CARTESIAN_POINT ( 'NONE',  ( 1.364683531249988535, 5.467708333674750953, -0.7879004041258300672 ) ) ;
#16949 = CARTESIAN_POINT ( 'NONE',  ( 4.908994958506140982, 1.627828031611065152, 0.9215782234750914403 ) ) ;
#16950 = AXIS2_PLACEMENT_3D ( 'NONE', #49609, #23225, #155385 ) ;
#16951 = CARTESIAN_POINT ( 'NONE',  ( 4.562867621930529971, 1.439169320343157921, -1.179982364782502069 ) ) ;
#16952 = DIRECTION ( 'NONE',  ( -8.638326563840814399E-31, 0.000000000000000000, -1.000000000000000000 ) ) ;
#16953 = CARTESIAN_POINT ( 'NONE',  ( 5.963686863811354932, 1.742942877579903405, -0.3063674984340163387 ) ) ;
#16954 = CARTESIAN_POINT ( 'NONE',  ( -0.1882626618336727398, -1.244567986390752390, -1.587255334073833790 ) ) ;
#16956 = CARTESIAN_POINT ( 'NONE',  ( 2.666745002694201450, -1.451881433263510601, 1.525875076051644408 ) ) ;
#16955 = CARTESIAN_POINT ( 'NONE',  ( -8.631737353394710155, 13.22211067893587533, 1.040834085586084257E-14 ) ) ;
#16957 = CARTESIAN_POINT ( 'NONE',  ( 8.561083932025322696, 12.07534945641652158, -1.199719254218446718 ) ) ;
#16959 = CARTESIAN_POINT ( 'NONE',  ( 0.07479286986305369589, 4.095183424177953668, -2.410510762676120411 ) ) ;
#16958 = DIRECTION ( 'NONE',  ( 3.330669073875478989E-16, -4.632576442341012461E-16, -1.000000000000000000 ) ) ;
#16960 = CARTESIAN_POINT ( 'NONE',  ( 0.000000000000000000, 8.999999999999998224, 0.000000000000000000 ) ) ;
#16961 = CARTESIAN_POINT ( 'NONE',  ( 1.529563250702131727, -0.2428666551740152890, 2.005035470024270960 ) ) ;
#16962 = CARTESIAN_POINT ( 'NONE',  ( -0.6823417656250212460, 2.301041667008084435, 1.181850606188767472 ) ) ;
#16963 = CARTESIAN_POINT ( 'NONE',  ( 4.521807925357579805, 5.234196320127330715, -1.199719254218452047 ) ) ;
#16964 = ORIENTED_EDGE ( 'NONE', *, *, #574, .T. ) ;
#16965 = CARTESIAN_POINT ( 'NONE',  ( 2.056162960589353883, 2.155939639820044107, -0.1567802445739118478 ) ) ;
#16966 = CARTESIAN_POINT ( 'NONE',  ( 6.890000000000004121, 6.033562824179531603, 2.874897443939719910 ) ) ;
#16969 = CARTESIAN_POINT ( 'NONE',  ( 0.000000000000000000, 1.899999999999999023, 0.000000000000000000 ) ) ;
#16968 = DIRECTION ( 'NONE',  ( 0.000000000000000000, 0.000000000000000000, -1.000000000000000000 ) ) ;
#16967 = CARTESIAN_POINT ( 'NONE',  ( 2.911969131885072670, 6.619324097166378706, 0.000000000000000000 ) ) ;
#16970 = CARTESIAN_POINT ( 'NONE',  ( 8.527715432871318058, 12.89282573841782664, -0.7216878364870338292 ) ) ;
#16971 = CARTESIAN_POINT ( 'NONE',  ( -7.720982897393580124, -6.134628647623485698, 7.834948825496934610 ) ) ;
#16972 = CARTESIAN_POINT ( 'NONE',  ( -8.365017589951714072, 8.861534731139549592, 1.040834085586084257E-14 ) ) ;
#16973 = CARTESIAN_POINT ( 'NONE',  ( 1.066276686178056377, -1.386418637449363889, 1.697306931840412370 ) ) ;
#16974 = CARTESIAN_POINT ( 'NONE',  ( -0.006158830626143650504, 7.078243236992579845, 2.121324627965421872 ) ) ;
#16975 = CARTESIAN_POINT ( 'NONE',  ( 1.903560677580185656, 1.881515123832262715, 1.256258119677531315 ) ) ;
#16976 = CARTESIAN_POINT ( 'NONE',  ( -6.659026002606323047, 10.92061410301605662, 0.000000000000000000 ) ) ;
#16977 = CARTESIAN_POINT ( 'NONE',  ( -4.243338890952901288, 6.934017225211593249, -1.082531754730548412 ) ) ;
#16979 =( GEOMETRIC_REPRESENTATION_CONTEXT ( 3 ) GLOBAL_UNCERTAINTY_ASSIGNED_CONTEXT ( ( #86164 ) ) GLOBAL_UNIT_ASSIGNED_CONTEXT ( ( #137126, #151244, #51611 ) ) REPRESENTATION_CONTEXT ( 'NONE', 'WORKASPACE' ) );
#16978 = CARTESIAN_POINT ( 'NONE',  ( 1.364683531249988535, 3.676041667008087099, 0.7879004041258500513 ) ) ;
#16980 = CARTESIAN_POINT ( 'NONE',  ( 4.601545839464173504, 8.365386937211251706, 0.1680730238927778675 ) ) ;
#16981 = EDGE_CURVE ( 'NONE', #80197, #96352, #199150, .T. ) ;
#16982 = CARTESIAN_POINT ( 'NONE',  ( -0.7500000000000179856, 11.54166666666666607, 1.299038105676658228 ) ) ;
#16983 = CARTESIAN_POINT ( 'NONE',  ( 3.390420931869152721, 6.113185632892752075, -1.199719254218452047 ) ) ;
#16984 = CARTESIAN_POINT ( 'NONE',  ( 2.899370140885823233, -0.5591585085688542955, 1.679125488999051452 ) ) ;
#16985 = CARTESIAN_POINT ( 'NONE',  ( 0.2004011508093841987, -2.105512755765154509, -0.05116925900590372361 ) ) ;
#16986 = CARTESIAN_POINT ( 'NONE',  ( -1.364683531250000748, 15.42187500034139447, 0.000000000000000000 ) ) ;
#16987 = ORIENTED_EDGE ( 'NONE', *, *, #109243, .T. ) ;
#16988 = AXIS2_PLACEMENT_3D ( 'NONE', #30384, #180880, #196082 ) ;
#16989 = CARTESIAN_POINT ( 'NONE',  ( -6.611536185319534908, 7.742488966741438716, 1.199719254218452047 ) ) ;
#16990 = CARTESIAN_POINT ( 'NONE',  ( 4.956657736208940790, -1.899625167328807374, -0.6766988040120130998 ) ) ;
#16991 = ORIENTED_EDGE ( 'NONE', *, *, #170571, .T. ) ;
#16992 = EDGE_CURVE ( 'NONE', #143616, #210726, #150079, .T. ) ;
#16993 = CIRCLE ( 'NONE', #65541, 3.100000000000000089 ) ;
#16994 = CARTESIAN_POINT ( 'NONE',  ( 2.500682550815761740, 1.503739811390795378, -1.112508705057350999 ) ) ;
#16995 = EDGE_CURVE ( 'NONE', #54853, #25107, #50771, .T. ) ;
#16996 = CARTESIAN_POINT ( 'NONE',  ( 2.940353189855488658, -1.068159618217549234, 1.773299548953041871 ) ) ;
#16997 = CARTESIAN_POINT ( 'NONE',  ( -6.577113915960828727, 9.727031097712693253, -1.082531754730549967 ) ) ;
#16998 = CARTESIAN_POINT ( 'NONE',  ( 1.599720133015330337, 1.321132142916726204, 1.382909031182079307 ) ) ;
#16999 = B_SPLINE_CURVE_WITH_KNOTS ( 'NONE', 3,
 ( #123771, #139953, #41384, #73859, #105315, #107495 ),
 .UNSPECIFIED., .F., .F.,
 ( 4, 2, 4 ),
 ( 0.000000000000000000, 0.0003779448103413554985, 0.0007558896206827109970 ),
 .UNSPECIFIED. ) ;
#17000 = DIRECTION ( 'NONE',  ( 0.000000000000000000, 0.000000000000000000, 1.000000000000000000 ) ) ;
#17001 = CARTESIAN_POINT ( 'NONE',  ( -10.78926753850537423, 5.463497890167042570, -6.588879020148982413 ) ) ;
#17002 =( NAMED_UNIT ( * ) PLANE_ANGLE_UNIT ( ) SI_UNIT ( $, .RADIAN. ) );
#17003 = CARTESIAN_POINT ( 'NONE',  ( -1.364683531250012516, 4.051041667008088432, -0.7879004041258300672 ) ) ;
#17004 = CARTESIAN_POINT ( 'NONE',  ( 0.8262462788446512940, -0.8622288892402606431, -1.707089296137359158 ) ) ;
#17005 = CARTESIAN_POINT ( 'NONE',  ( 4.909461021924231616, 8.741805268971372556, 0.7216878364870317197 ) ) ;
#17006 = CARTESIAN_POINT ( 'NONE',  ( 3.068751266904270025, 1.422870340827029345, -1.350941015047700366 ) ) ;
#17007 = CARTESIAN_POINT ( 'NONE',  ( 1.715338164143669353, -0.7127732114542313369, 0.8729459113246081925 ) ) ;
#17008 = CARTESIAN_POINT ( 'NONE',  ( -3.623772196602547346, 7.449761006003425834, 0.000000000000000000 ) ) ;
#17009 = CARTESIAN_POINT ( 'NONE',  ( 5.062787373817619674, 0.6179034821891696838, 2.028544477791139222 ) ) ;
#17011 = CARTESIAN_POINT ( 'NONE',  ( -5.436456409399874623, 5.444880020495701523, 0.000000000000000000 ) ) ;
#17010 = CARTESIAN_POINT ( 'NONE',  ( 8.666686507633574621, 11.13422023037111330, 1.599625672291281386 ) ) ;
#17012 = CARTESIAN_POINT ( 'NONE',  ( 6.169206948603202179, 0.1476589778573663692, -1.965905794126821426 ) ) ;
#17013 = CARTESIAN_POINT ( 'NONE',  ( 1.364683531249986537, 1.905208333674750287, -0.7879004041258239610 ) ) ;
#17014 = CARTESIAN_POINT ( 'NONE',  ( 2.039316462420410758, 0.004210374635823382894, 2.013376229890501357 ) ) ;
#17016 = CARTESIAN_POINT ( 'NONE',  ( 0.6325982246286944166, 0.6188553777890459795, 2.024753282845246805 ) ) ;
#17015 = CARTESIAN_POINT ( 'NONE',  ( -5.883875478650828050, 9.808345791827219884, 0.7216878364870458196 ) ) ;
#17017 = CARTESIAN_POINT ( 'NONE',  ( 10.00676670411244196, 9.850953729071504128, -6.649899283857078736 ) ) ;
#17018 = CARTESIAN_POINT ( 'NONE',  ( 2.506376218629560171, 2.069854378281150709, 0.05321039126485183068 ) ) ;
#17019 = CARTESIAN_POINT ( 'NONE',  ( 3.715816618597135523, 6.492813934075403637, -1.199719254218453823 ) ) ;
#17020 = CARTESIAN_POINT ( 'NONE',  ( 5.896870467300973750, 5.844380064798101237, 0.7998128361456352531 ) ) ;
#17021 = EDGE_LOOP ( 'NONE', ( #64383, #144286, #151370 ) ) ;
#17023 = CARTESIAN_POINT ( 'NONE',  ( 4.192495815123822744, 5.914331089109666983, -1.599625672291255185 ) ) ;
#17022 = CARTESIAN_POINT ( 'NONE',  ( 5.736299646367586824, 0.4068676293152873602, 2.050479918790772960 ) ) ;
#17024 = CARTESIAN_POINT ( 'NONE',  ( 4.049673113991675955, 0.6152068410551281286, -1.718917501701062278 ) ) ;
#17025 = CARTESIAN_POINT ( 'NONE',  ( 9.728138913005292210, 11.30824913904973705, -1.199719254218440723 ) ) ;
#17026 = CARTESIAN_POINT ( 'NONE',  ( -1.201851678989727383E-14, 2.837500000000024336, -1.732050807568863648 ) ) ;
#17027 = CARTESIAN_POINT ( 'NONE',  ( 9.297838506356004729, 13.23377696881822274, -6.730568833096490344 ) ) ;
#17028 = CARTESIAN_POINT ( 'NONE',  ( 4.893709131440695081, 1.632385321431808256, 1.485157849447714451 ) ) ;
#17029 = CARTESIAN_POINT ( 'NONE',  ( -1.364683531250010740, 10.69270833367473195, 0.7879004041258445001 ) ) ;
#17030 = ORIENTED_EDGE ( 'NONE', *, *, #147441, .T. ) ;
#17031 = CARTESIAN_POINT ( 'NONE',  ( 3.967365900211225593, -1.591558630706500832, -1.059764132600553355 ) ) ;
#17032 = CARTESIAN_POINT ( 'NONE',  ( -9.378489572351046633, 11.96465713920816043, -1.599625672291263179 ) ) ;
#17033 = AXIS2_PLACEMENT_3D ( 'NONE', #135425, #185207, #52036 ) ;
#17034 = CARTESIAN_POINT ( 'NONE',  ( 7.741869408603235136, 8.990934717247309749, 1.199719254218462483 ) ) ;
#17035 = CARTESIAN_POINT ( 'NONE',  ( 1.360316468749992236, 1.546875000341396689, -1.040834085586084257E-14 ) ) ;
#17036 = CARTESIAN_POINT ( 'NONE',  ( 4.568734577680873876, 6.353276312092901890, -1.443375672974051449 ) ) ;
#17037 = CARTESIAN_POINT ( 'NONE',  ( 6.515165533258342023, -2.126321577054360201, 0.5302794918828001025 ) ) ;
#17038 = CARTESIAN_POINT ( 'NONE',  ( 8.656189917073545459, 13.74873789216364628, -8.313119079178678206 ) ) ;
#17039 = CARTESIAN_POINT ( 'NONE',  ( -0.04178991631376138827, -1.644041690304678616, -0.8291446804715857377 ) ) ;
#17040 = CARTESIAN_POINT ( 'NONE',  ( 5.371549237029319634, 7.622127557927130148, 1.287608608630997464 ) ) ;
#17041 = CARTESIAN_POINT ( 'NONE',  ( 4.798043669735932326, -1.870115615568968881, -0.04763329477865811679 ) ) ;
#17042 = CARTESIAN_POINT ( 'NONE',  ( 6.831329296439236032, 9.063246493969506545, -1.599625672291267398 ) ) ;
#17043 = CARTESIAN_POINT ( 'NONE',  ( -11.07124251632621537, 13.79999999999999538, -0.8054525327832626758 ) ) ;
#17044 = CARTESIAN_POINT ( 'NONE',  ( -7.212574532790102744, 8.477387045419011002, -1.082531754730550855 ) ) ;
#17045 = CARTESIAN_POINT ( 'NONE',  ( 3.323720213644492993, 7.029424015893889433, 1.040834085586084257E-14 ) ) ;
#17046 = CARTESIAN_POINT ( 'NONE',  ( 1.076931260867712625, 1.817606662292377218, 0.7587987759381797925 ) ) ;
#17047 = CARTESIAN_POINT ( 'NONE',  ( 1.827750133516142128, 0.7691037069590834774, -1.864176919362303675 ) ) ;
#17048 = CARTESIAN_POINT ( 'NONE',  ( -7.645908563102897126, 11.00764485934031889, 1.199719254218453823 ) ) ;
#17049 = CARTESIAN_POINT ( 'NONE',  ( 5.397027666691686321, 8.454226823519094935, 1.199719254218451159 ) ) ;
#17050 = CARTESIAN_POINT ( 'NONE',  ( 6.713552092917008274, -7.189371949512688431, 6.722000117219741000 ) ) ;
#17051 = CARTESIAN_POINT ( 'NONE',  ( 2.379091696419192381, 2.003018898301941686, -0.8894332929959417600 ) ) ;
#17052 = CARTESIAN_POINT ( 'NONE',  ( 5.883392091387670497, 1.685093539698417242, -0.7030590484572999399 ) ) ;
#17053 = CARTESIAN_POINT ( 'NONE',  ( -4.647747731386360215, 4.316793862905830892, 0.7998128361456341429 ) ) ;
#17054 = CARTESIAN_POINT ( 'NONE',  ( 6.825078400183553384, 0.5907600490881077526, 1.908621492364571903 ) ) ;
#17055 = FACE_OUTER_BOUND ( 'NONE', #20642, .T. ) ;
#17056 = CARTESIAN_POINT ( 'NONE',  ( 5.411112705629925301, 5.485588709422586362, 0.000000000000000000 ) ) ;
#17058 = EDGE_CURVE ( 'NONE', #56474, #19248, #62072, .T. ) ;
#17057 = CARTESIAN_POINT ( 'NONE',  ( 9.745613490124728884, 10.26430391476735338, 0.7998128361456462443 ) ) ;
#17059 = FACE_OUTER_BOUND ( 'NONE', #62667, .T. ) ;
#17060 = CARTESIAN_POINT ( 'NONE',  ( 5.560252395380206103, 8.540692657035327429, 1.082531754730547524 ) ) ;
#17061 = EDGE_LOOP ( 'NONE', ( #77138, #132250, #78062, #39506 ) ) ;
#17062 = ORIENTED_EDGE ( 'NONE', *, *, #43825, .F. ) ;
#17064 = CARTESIAN_POINT ( 'NONE',  ( 0.7154901591317133214, 1.647040347281914396, 1.157252022262734714 ) ) ;
#17063 = CARTESIAN_POINT ( 'NONE',  ( 4.686955257832659427, 1.367739038236553517, 1.232883728221023212 ) ) ;
#17065 = CARTESIAN_POINT ( 'NONE',  ( 2.829810162582825139, -1.586297295151902986, 1.663386555757565555 ) ) ;
#17067 = CARTESIAN_POINT ( 'NONE',  ( 0.9009385260731802569, -1.599958946562014539, 0.9501217156336287939 ) ) ;
#17066 = CARTESIAN_POINT ( 'NONE',  ( 3.768803514918948938, 4.459654191235965293, -1.082531754730543083 ) ) ;
#17068 = CARTESIAN_POINT ( 'NONE',  ( -3.285556943750000514, -3.988541666188710089, -1.896917185911906500 ) ) ;
#17069 = CARTESIAN_POINT ( 'NONE',  ( -4.765854690403601879, 5.518917546014321829, 1.199719254218462483 ) ) ;
#17070 = CARTESIAN_POINT ( 'NONE',  ( -9.586151930456434656, 15.23390131771004974, -7.218760142018259884 ) ) ;
#17071 = CARTESIAN_POINT ( 'NONE',  ( 4.131050151015442928, 1.750605847248308145, 0.7702136748066327199 ) ) ;
#17072 = CARTESIAN_POINT ( 'NONE',  ( -8.134002093194872884, 11.57708731111429401, 1.199719254218453823 ) ) ;
#17073 = CARTESIAN_POINT ( 'NONE',  ( -5.614485009834902840, 9.564333254867113610, 0.7216878364870267237 ) ) ;
#17075 = CARTESIAN_POINT ( 'NONE',  ( 2.834663617355744680, 0.2272019944037397543, 1.856728029318695627 ) ) ;
#17074 = CARTESIAN_POINT ( 'NONE',  ( 4.019144481351099252, -2.000086177330139492, 0.6089195546459759134 ) ) ;
#17076 = CARTESIAN_POINT ( 'NONE',  ( 7.076992996653421741, 10.23994701519558781, -1.082531754730537976 ) ) ;
#17077 = CARTESIAN_POINT ( 'NONE',  ( 1.364683531249990311, 5.426041667008087543, 0.7879004041258499402 ) ) ;
#17078 = CARTESIAN_POINT ( 'NONE',  ( 5.759284750224211713, 1.812880138157666465, -0.3211251414683007899 ) ) ;
#17079 = CIRCLE ( 'NONE', #99986, 12.00000000000000178 ) ;
#17080 = CARTESIAN_POINT ( 'NONE',  ( 2.361091307074211887, 5.906356958228550447, 0.7998128361456462443 ) ) ;
#17081 = CARTESIAN_POINT ( 'NONE',  ( 5.756345505848640798, 6.148709499980903992, 0.8262799378709930753 ) ) ;
#17082 = CARTESIAN_POINT ( 'NONE',  ( 5.162619097868246243, -1.245661315326980212, 1.193383824415847450 ) ) ;
#17083 = CARTESIAN_POINT ( 'NONE',  ( -6.093499974338126179, 9.196501505781426999, -1.199719254218440723 ) ) ;
#17084 = CARTESIAN_POINT ( 'NONE',  ( 0.2813449273042024079, 1.443300801228193153, -0.9609375900588543740 ) ) ;
#17085 = SURFACE_SIDE_STYLE ('',( #180672 ) ) ;
#17086 = CARTESIAN_POINT ( 'NONE',  ( 5.049771808528761952, 1.604214368398539925, 1.463040072455735974 ) ) ;
#17087 = CARTESIAN_POINT ( 'NONE',  ( 2.912524513316586461, 1.322148455168963510, -1.259233298254287536 ) ) ;
#17088 = CARTESIAN_POINT ( 'NONE',  ( 0.5495624486224827132, 1.449728300881658383, 1.321815246172884040 ) ) ;
#17089 = CARTESIAN_POINT ( 'NONE',  ( 5.788306078712673219, -0.7643476728274435361, -1.974717070840046107 ) ) ;
#17090 = VERTEX_POINT ( 'NONE', #80449 ) ;
#17092 = CARTESIAN_POINT ( 'NONE',  ( 1.364683531249988535, 4.176041667008081326, 0.7879004041258500513 ) ) ;
#17091 = CARTESIAN_POINT ( 'NONE',  ( 6.374598633881160659, -0.1077809834691043772, -2.289980472931157252 ) ) ;
#17093 = CARTESIAN_POINT ( 'NONE',  ( 7.892817981449907982, 12.36003807833360391, 0.7998128361456462443 ) ) ;
#17094 = CARTESIAN_POINT ( 'NONE',  ( 1.664851754375612058, 0.6682523891239250391, 2.012492909199379731 ) ) ;
#17095 = CARTESIAN_POINT ( 'NONE',  ( -4.989037340148921196, 5.883260320670900434, 1.082531754730560403 ) ) ;
#17096 = CARTESIAN_POINT ( 'NONE',  ( 3.705121118284530279, 7.544668081299086282, -1.734723475976807094E-15 ) ) ;
#17097 = CARTESIAN_POINT ( 'NONE',  ( -3.578989363883261277, 7.119311991265024453, 1.040834085586084257E-14 ) ) ;
#17098 = CARTESIAN_POINT ( 'NONE',  ( 6.245025782124020708, -0.3104734683975469145, -2.148636169971326559 ) ) ;
#17100 = CARTESIAN_POINT ( 'NONE',  ( 0.7500000000000006661, 12.61458333401613352, 1.299038105676657340 ) ) ;
#17099 = CARTESIAN_POINT ( 'NONE',  ( 6.983263157960368339, 1.232032666090671302, 2.265420076015733031 ) ) ;
#17102 = EDGE_LOOP ( 'NONE', ( #199387, #158418, #71365, #154063 ) ) ;
#17101 = CARTESIAN_POINT ( 'NONE',  ( 1.788022372910631486, 2.124507586210178989, -0.6485351029156469771 ) ) ;
#17103 = CARTESIAN_POINT ( 'NONE',  ( 6.469375277500488686, -1.978045142091336306, -0.3906011616893814709 ) ) ;
#17105 = CARTESIAN_POINT ( 'NONE',  ( 4.047761193102417110, 1.490534549623608873, 1.425871689066391168 ) ) ;
#17104 = CARTESIAN_POINT ( 'NONE',  ( 3.551346171775753735, 6.230655402791975384, 1.199719254218462483 ) ) ;
#17107 = CARTESIAN_POINT ( 'NONE',  ( 3.475000000000000533, -3.295833333333334725, -2.006292185433951047 ) ) ;
#17106 = CARTESIAN_POINT ( 'NONE',  ( 5.855142236255289845, 7.924361590421551860, -1.599625672291281386 ) ) ;
#17108 = CARTESIAN_POINT ( 'NONE',  ( 4.552505719138623341, 8.533283448962240669, 0.7998128361456341429 ) ) ;
#17110 = EDGE_CURVE ( 'NONE', #138803, #127411, #11159, .T. ) ;
#17109 = CARTESIAN_POINT ( 'NONE',  ( -1.642778471875000035, -0.1677083328553742592, -2.845375778867859751 ) ) ;
#17111 = CARTESIAN_POINT ( 'NONE',  ( 0.1329588055935760349, 6.948069629093068578, -2.440977959956799115 ) ) ;
#17112 = CARTESIAN_POINT ( 'NONE',  ( 0.7090669197488512765, -0.3047467688393705187, 2.068175119304823451 ) ) ;
#17113 = CARTESIAN_POINT ( 'NONE',  ( 4.036529152626888717, -1.599951230533543267, 0.9111318136766360931 ) ) ;
#17114 = CARTESIAN_POINT ( 'NONE',  ( 5.789495288235341874, 6.713164910151406595, 1.199719254218462483 ) ) ;
#17115 = CARTESIAN_POINT ( 'NONE',  ( 1.887319702290214840, 1.186364228098319762, 1.252193311579427482 ) ) ;
#17116 = CARTESIAN_POINT ( 'NONE',  ( 0.1632964843477149597, 1.879801964727344732, -0.7303121171872913875 ) ) ;
#17117 =( BOUNDED_CURVE ( )  B_SPLINE_CURVE ( 2, ( #151343, #86330, #187020, #38653, #88481, #152401, #136163, #203258, #70049 ),
 .UNSPECIFIED., .F., .T. ) 
 B_SPLINE_CURVE_WITH_KNOTS ( ( 3, 2, 2, 2, 3 ),
 ( 0.7053571428571427937, 0.7083333333333333703, 0.7142857142857143016, 0.7202380952380952328, 0.7232142857142856984 ),
 .UNSPECIFIED. ) 
 CURVE ( )  GEOMETRIC_REPRESENTATION_ITEM ( )  RATIONAL_B_SPLINE_CURVE ( ( 0.9330127018922194093, 0.9330127018922180770, 1.000000000000000000, 0.8660254037844387076, 1.000000000000000000, 0.8660254037844387076, 1.000000000000000000, 0.9330127018922194093, 0.9330127018922194093 ) ) 
 REPRESENTATION_ITEM ( '' )  );
#17118 = CARTESIAN_POINT ( 'NONE',  ( 1.477568294945711180, -2.288151160537778672, -0.2198310841375460678 ) ) ;
#17119 = CARTESIAN_POINT ( 'NONE',  ( -4.415151579544611238, 8.302760609444034046, -0.7998128361456281477 ) ) ;
#17120 = CARTESIAN_POINT ( 'NONE',  ( 1.423510532338147394, -0.05571650319935492202, 2.261890015172054458 ) ) ;
#17121 = CARTESIAN_POINT ( 'NONE',  ( 4.213572796808015219, -0.3603392467595716298, 2.074844637031019623 ) ) ;
#17122 = CARTESIAN_POINT ( 'NONE',  ( -3.526002468005825286, 6.271364091718859335, -1.199719254218450271 ) ) ;
#17123 = CARTESIAN_POINT ( 'NONE',  ( 2.477515592860125349, 1.084993897938502760, 1.398054747847920609 ) ) ;
#17125 = EDGE_CURVE ( 'NONE', #108467, #143793, #102559, .T. ) ;
#17124 = CARTESIAN_POINT ( 'NONE',  ( 5.829115978871627135, 8.888053511070525659, 1.199719254218462483 ) ) ;
#17126 = CARTESIAN_POINT ( 'NONE',  ( 5.899206235277530297, 7.015400374979486209, -1.082531754730548412 ) ) ;
#17127 = CARTESIAN_POINT ( 'NONE',  ( 6.375000000015829116, 2.052068128807268188, -3.630807684676397404E-13 ) ) ;
#17128 = CARTESIAN_POINT ( 'NONE',  ( -4.388035272317281077, 8.271124917678806199, 0.7998128361456481317 ) ) ;
#17129 = CARTESIAN_POINT ( 'NONE',  ( -0.7500000000000006661, 1.608333333333357373, -1.299038105676652011 ) ) ;
#17130 = CARTESIAN_POINT ( 'NONE',  ( -5.284980951228653190, 5.060232619388524533, 0.000000000000000000 ) ) ;
#17131 = CARTESIAN_POINT ( 'NONE',  ( 4.693709758858874537, 2.072258576215581183, -0.8006532145865407069 ) ) ;
#17132 = CARTESIAN_POINT ( 'NONE',  ( 3.047022719409075986, -1.791863632763015968, -1.261349808265788797 ) ) ;
#17133 = CARTESIAN_POINT ( 'NONE',  ( -5.949330478298285207, 5.835307067636438028, 0.7998128361456341429 ) ) ;
#17134 = CARTESIAN_POINT ( 'NONE',  ( -5.334207092333882017, 5.187939460669764635, 0.7998128361456281477 ) ) ;
#17135 = CARTESIAN_POINT ( 'NONE',  ( 5.830757645730302308, 1.424217953154560012, -1.571192434731554677 ) ) ;
#17136 = CARTESIAN_POINT ( 'NONE',  ( 0.6823417656249917140, 3.592708333674754506, 1.181850606188765695 ) ) ;
#17137 = CARTESIAN_POINT ( 'NONE',  ( 6.890000000000004121, 6.033562824179531603, 2.874897443939719910 ) ) ;
#17138 = CARTESIAN_POINT ( 'NONE',  ( -4.853455804012230423, 6.685451076146141425, 1.443375672974064550 ) ) ;
#17139 = CARTESIAN_POINT ( 'NONE',  ( 5.379186226027963258, -1.918017450862268714, -0.9047448674902383026 ) ) ;
#17140 = CARTESIAN_POINT ( 'NONE',  ( -5.289089323106922258, 9.184704953684462936, 0.7216878364870267237 ) ) ;
#17141 = ORIENTED_EDGE ( 'NONE', *, *, #39340, .T. ) ;
#17143 = CARTESIAN_POINT ( 'NONE',  ( 6.561405286136595905, 0.3748316153167965403, -2.128808860954830795 ) ) ;
#17142 = CARTESIAN_POINT ( 'NONE',  ( -4.340018570150309785, 7.117086527600392287, -1.082531754730551743 ) ) ;
#17144 = CARTESIAN_POINT ( 'NONE',  ( 4.143988507271280319, 7.986403691791820414, -0.7998128361456221525 ) ) ;
#17145 = CARTESIAN_POINT ( 'NONE',  ( 6.128435733830499998, 0.1874100934057248424, 1.831705376836203936 ) ) ;
#17146 = SURFACE_STYLE_USAGE ( .BOTH. , #119008 ) ;
#17147 = CARTESIAN_POINT ( 'NONE',  ( -1.201851678989727383E-14, 2.634375000341417916, 1.575800808251672791 ) ) ;
#17148 = CARTESIAN_POINT ( 'NONE',  ( 0.9424304438642245874, -1.370989592614113795, -1.072060877835380621 ) ) ;
#17149 = CARTESIAN_POINT ( 'NONE',  ( 2.333974999846879061, 5.874721266463329705, -0.7998128361456291469 ) ) ;
#17150 = LINE ( 'NONE', #83226, #35742 ) ;
#17151 = CARTESIAN_POINT ( 'NONE',  ( -1.364683531250014514, -0.6572916663252459379, 0.7879004041258379498 ) ) ;
#17152 = DIRECTION ( 'NONE',  ( 0.000000000000000000, 0.000000000000000000, 1.000000000000000000 ) ) ;
#17153 = CIRCLE ( 'NONE', #165925, 0.08000000000000020983 ) ;
#17154 = CARTESIAN_POINT ( 'NONE',  ( 5.612251347527116963, -0.9680786960581324596, -1.932885698521320528 ) ) ;
#17155 = CARTESIAN_POINT ( 'NONE',  ( -2.839543107058306592, 5.400218493954923815, -1.199719254218446718 ) ) ;
#17156 = EDGE_CURVE ( 'NONE', #18033, #7438, #95796, .T. ) ;
#17157 = CARTESIAN_POINT ( 'NONE',  ( -7.524412065460066579, 7.880828285899290186, 0.7216878364870317197 ) ) ;
#17158 = CARTESIAN_POINT ( 'NONE',  ( 4.768538688506021472, -1.414568798902924307, 1.634688457493836289 ) ) ;
#17160 = ORIENTED_EDGE ( 'NONE', *, *, #142193, .F. ) ;
#17159 = CARTESIAN_POINT ( 'NONE',  ( -4.981695098378565945, 4.776675467721892332, -0.7998128361456362523 ) ) ;
#17161 = CARTESIAN_POINT ( 'NONE',  ( -0.6823417656250212460, 3.301041667008085323, 1.181850606188767472 ) ) ;
#17162 = CARTESIAN_POINT ( 'NONE',  ( 5.448493488195655488, 0.5694873833897282633, 1.887333253073280703 ) ) ;
#17163 = CARTESIAN_POINT ( 'NONE',  ( 4.991369361657826964, 1.659364262194364725, 0.5025568866975324012 ) ) ;
#17165 = CARTESIAN_POINT ( 'NONE',  ( 1.593588134247824639, -0.7342643958434189599, 2.065040727587868830 ) ) ;
#17164 = CARTESIAN_POINT ( 'NONE',  ( -0.6801582343750438575, -0.5677083329919535570, 1.178068619123803451 ) ) ;
#17166 = CARTESIAN_POINT ( 'NONE',  ( 1.923324260599985402, 2.153519634812319783, 0.8294600792757185204 ) ) ;
#17167 = CARTESIAN_POINT ( 'NONE',  ( 4.253237527111143557, -1.711175411557999348, -1.148025453137695662 ) ) ;
#17168 = CARTESIAN_POINT ( 'NONE',  ( 0.02324440041187331510, -1.194077796415137449, -1.532174088482601837 ) ) ;
#17169 = CARTESIAN_POINT ( 'NONE',  ( -6.466876083594135238, 9.528143949959703818, 1.082531754730548412 ) ) ;
#17170 = CARTESIAN_POINT ( 'NONE',  ( -5.490125858891038213, 5.369844688319787451, -0.7998128361456362523 ) ) ;
#17171 = FACE_OUTER_BOUND ( 'NONE', #58730, .T. ) ;
#17172 = CARTESIAN_POINT ( 'NONE',  ( 3.937823072884456099, -2.028283017459261650, 0.6187693826033290323 ) ) ;
#17173 = DIRECTION ( 'NONE',  ( 0.000000000000000000, 0.000000000000000000, 1.000000000000000000 ) ) ;
#17174 = CARTESIAN_POINT ( 'NONE',  ( 1.600232647554021392, -0.2440283035436350279, 2.001511509883910911 ) ) ;
#17175 = CARTESIAN_POINT ( 'NONE',  ( -6.005898860729463884, 9.950706404252290582, 0.7216878364870458196 ) ) ;
#17176 = CARTESIAN_POINT ( 'NONE',  ( 4.542132036680512464, 0.9468659437555368985, -1.993456357439137960 ) ) ;
#17177 = CARTESIAN_POINT ( 'NONE',  ( 1.642778471875001811, -2.180208332855374742, 2.845375778867859751 ) ) ;
#17178 = CARTESIAN_POINT ( 'NONE',  ( -0.1290005225502675879, 2.860092606084875033, -2.662085506130333457 ) ) ;
#17179 = DIRECTION ( 'NONE',  ( -0.000000000000000000, 1.000000000000000000, -0.000000000000000000 ) ) ;
#17180 = CARTESIAN_POINT ( 'NONE',  ( 4.064661395739702421, 3.791390914876744844, -2.445650119220917240 ) ) ;
#17182 = CARTESIAN_POINT ( 'NONE',  ( -10.39398850336074709, -8.287668210030888716, 0.6181847325715009722 ) ) ;
#17181 = CARTESIAN_POINT ( 'NONE',  ( -4.586114404036374381, 8.497146329035404122, -0.08355658565369419866 ) ) ;
#17183 = ORIENTED_EDGE ( 'NONE', *, *, #182687, .T. ) ;
#17184 = CARTESIAN_POINT ( 'NONE',  ( 3.450122203709057533, 2.061077815303002936, 0.001625369314967386580 ) ) ;
#17185 = CARTESIAN_POINT ( 'NONE',  ( -1.360316468750040642, 1.911458333674787236, 0.7853790794158660438 ) ) ;
#17186 = CARTESIAN_POINT ( 'NONE',  ( -5.368138756007025947, 8.350246751061767725, 1.199719254218452047 ) ) ;
#17187 = CARTESIAN_POINT ( 'NONE',  ( 2.947920495102425154, -1.358134161044775245, -1.495000266999703564 ) ) ;
#17188 = CARTESIAN_POINT ( 'NONE',  ( -1.402160292154681736E-14, -0.6624999999999758860, -1.732050807568870754 ) ) ;
#17189 = CARTESIAN_POINT ( 'NONE',  ( 10.56143847536557878, 11.42402576412244386, 0.000000000000000000 ) ) ;
#17190 = CARTESIAN_POINT ( 'NONE',  ( 1.639600518753115521, -1.491979387419887892, -1.421952917470001632 ) ) ;
#17191 = CARTESIAN_POINT ( 'NONE',  ( -9.445283354644308460, 14.68100100830176125, -7.300214616139029999 ) ) ;
#17192 = CARTESIAN_POINT ( 'NONE',  ( 5.494078562035752178, 7.432844293840273231, -1.599625672291262513 ) ) ;
#17193 = PRESENTATION_LAYER_ASSIGNMENT (  '', '', ( #210933 ) ) ;
#17194 = CARTESIAN_POINT ( 'NONE',  ( -0.2409995289980246258, 2.020898751655671788, -2.415740196953279462 ) ) ;
#17195 = CARTESIAN_POINT ( 'NONE',  ( 1.429379046243149931, 0.9088080074306194023, -1.601118750654044964 ) ) ;
#17196 = CARTESIAN_POINT ( 'NONE',  ( 0.1886478520232073020, -1.081937125009281964, 2.038365869624358506 ) ) ;
#17197 = CARTESIAN_POINT ( 'NONE',  ( 6.547661840756936691, 6.603636667163397256, 0.7998128361456352531 ) ) ;
#17198 = CARTESIAN_POINT ( 'NONE',  ( 1.950665695202157046, 0.6760947502928333908, 2.053231632317173538 ) ) ;
#17199 = CARTESIAN_POINT ( 'NONE',  ( -2.494337075234348777, 5.853884321174607663, -0.7216878364870267237 ) ) ;
#17200 = CARTESIAN_POINT ( 'NONE',  ( 1.675017921984035096, 1.752138005693338441, -0.9981273289914743829 ) ) ;
#17201 = CARTESIAN_POINT ( 'NONE',  ( 2.091588275066556868, 1.323615364194903554, -1.878831054484223495 ) ) ;
#17202 = LINE ( 'NONE', #116921, #153026 ) ;
#17203 = CARTESIAN_POINT ( 'NONE',  ( 0.08069323953814251660, -0.1329233695197447052, -1.840450602299897431 ) ) ;
#17204 = CARTESIAN_POINT ( 'NONE',  ( 11.33772467203841572, 11.00732847981847584, 3.599999999999999201 ) ) ;
#17205 = CARTESIAN_POINT ( 'NONE',  ( 4.381683959536594841, 1.286834623079432083, 1.493660651562748853 ) ) ;
#17206 = CARTESIAN_POINT ( 'NONE',  ( 3.046111529846948329, 0.9110102549910354952, 1.799122713138465279 ) ) ;
#17208 = CARTESIAN_POINT ( 'NONE',  ( 9.747949258101261449, 11.43532422494874368, -1.082531754730537088 ) ) ;
#17207 = CARTESIAN_POINT ( 'NONE',  ( -1.364683531250012516, 2.238541667008087988, -0.7879004041258289570 ) ) ;
#17210 = CARTESIAN_POINT ( 'NONE',  ( 6.358053323650514344, 2.100580423050825818, -0.1529390103112079069 ) ) ;
#17209 = CARTESIAN_POINT ( 'NONE',  ( -7.446452682403657874, 9.710614100936176385, -1.599625672291263179 ) ) ;
#17211 = CARTESIAN_POINT ( 'NONE',  ( 5.178213324540339002, -1.104578422852561914, -1.750899486206449751 ) ) ;
#17212 = CARTESIAN_POINT ( 'NONE',  ( 6.877010230629674759, 9.046264573866535486, 1.599625672291281386 ) ) ;
#17213 = CARTESIAN_POINT ( 'NONE',  ( -5.377780486114890124, 9.425827667109372143, 0.000000000000000000 ) ) ;
#17214 = CARTESIAN_POINT ( 'NONE',  ( 6.539320575229236709, 3.694699318329996540, 2.517509839998680832 ) ) ;
#17215 = CARTESIAN_POINT ( 'NONE',  ( 5.660417604421997595, 2.017665076342503916, 0.09485465564632548918 ) ) ;
#17216 = CARTESIAN_POINT ( 'NONE',  ( -0.7500000000000006661, -0.6104166659838470288, -1.299038105676652011 ) ) ;
#17217 = CARTESIAN_POINT ( 'NONE',  ( 3.405163318333865874, 1.819529416799025912, -1.419322092190724138 ) ) ;
#17218 = CARTESIAN_POINT ( 'NONE',  ( 1.147418581349904265, 1.820775857560010369, -0.9689367605143526241 ) ) ;
#17219 = CARTESIAN_POINT ( 'NONE',  ( 7.266807147244743526, 11.42176607185347414, -0.7216878364870267237 ) ) ;
#17220 = CARTESIAN_POINT ( 'NONE',  ( 7.679767667498067496, 7.924426798361372093, 0.000000000000000000 ) ) ;
#17221 = CARTESIAN_POINT ( 'NONE',  ( 4.227110032410640095, 8.153655147779589996, 0.7998128361456271485 ) ) ;
#17222 = CARTESIAN_POINT ( 'NONE',  ( -1.201851678989727383E-14, 0.8843750003414173610, 1.575800808251672791 ) ) ;
#17223 = CARTESIAN_POINT ( 'NONE',  ( 3.691562964670865199, 7.528850235416478576, -0.7998128361456362523 ) ) ;
#17224 = CARTESIAN_POINT ( 'NONE',  ( 5.951666246274784910, 9.887435020721849099, 0.7216878364870438212 ) ) ;
#17226 = DIRECTION ( 'NONE',  ( 0.9781476007338056888, 0.000000000000000000, 0.2079116908177593703 ) ) ;
#17225 = CARTESIAN_POINT ( 'NONE',  ( 3.139314614211644816, -0.1572037376256547880, -2.165524352769617078 ) ) ;
#17227 = DIRECTION ( 'NONE',  ( 0.000000000000000000, -1.000000000000000000, 0.000000000000000000 ) ) ;
#17229 = CARTESIAN_POINT ( 'NONE',  ( 3.245484093776138668, 1.841430844176932480, -0.003062914905635482320 ) ) ;
#17228 = CARTESIAN_POINT ( 'NONE',  ( -4.121315508874262790, 6.791656612786516334, -1.082531754730549967 ) ) ;
#17230 = CARTESIAN_POINT ( 'NONE',  ( -1.001543065824772872E-14, 4.321875000341417916, 1.575800808251672791 ) ) ;
#17231 = CARTESIAN_POINT ( 'NONE',  ( 4.652002595327206613, 0.8389548150543740812, 2.024815518666116088 ) ) ;
#17232 = CARTESIAN_POINT ( 'NONE',  ( -0.08000000000000367928, -9.900000000000005684, -9.579665964948867796 ) ) ;
#17233 = CARTESIAN_POINT ( 'NONE',  ( 4.522535110384587220, 1.395170471642327437, -1.781064426588598426 ) ) ;
#17234 = CARTESIAN_POINT ( 'NONE',  ( -5.856132087369688044, 6.175168335346238990, -0.9273813317931516309 ) ) ;
#17235 = CARTESIAN_POINT ( 'NONE',  ( 5.258270873920524835, 7.671714958958308017, -1.216365610458163715 ) ) ;
#17236 = PRESENTATION_LAYER_ASSIGNMENT (  '', '', ( #155498 ) ) ;
#17237 = CARTESIAN_POINT ( 'NONE',  ( -4.760321331729590710, 8.567808963744235839, 0.7216878364870267237 ) ) ;
#17238 = CARTESIAN_POINT ( 'NONE',  ( 3.431622278034673901, 7.017660067766835930, -1.734723475976807094E-15 ) ) ;
#17239 = CARTESIAN_POINT ( 'NONE',  ( 6.010986587707961348, 1.561705629380090832, 0.8325338966498199156 ) ) ;
#17240 = CARTESIAN_POINT ( 'NONE',  ( 4.318997845537309033, 1.554796018123940193, -1.278706705004019506 ) ) ;
#17241 = CARTESIAN_POINT ( 'NONE',  ( 6.109920781252839994, 10.27999134477033216, 1.040834085586084257E-14 ) ) ;
#17242 = CARTESIAN_POINT ( 'NONE',  ( 3.381953601626528361, 1.334784698733671560, 1.628938261321200232 ) ) ;
#17243 = CARTESIAN_POINT ( 'NONE',  ( 0.4740638213791115718, -1.901237768712552345, -0.2334040896743785343 ) ) ;
#17244 = CARTESIAN_POINT ( 'NONE',  ( 4.857899112398166075, 4.561970474086296079, 1.040834085586084257E-14 ) ) ;
#17245 = CARTESIAN_POINT ( 'NONE',  ( 1.732793293511214472, -1.869146454778564559, -0.6209850235064825474 ) ) ;
#17246 = CARTESIAN_POINT ( 'NONE',  ( 0.9537216069140028729, 1.868711056098860235, -0.08788249432020722729 ) ) ;
#17247 = CARTESIAN_POINT ( 'NONE',  ( 1.135121963537696566, -0.04462593873827064989, -1.961518378280776354 ) ) ;
#17249 = VERTEX_POINT ( 'NONE', #212567 ) ;
#17248 = CARTESIAN_POINT ( 'NONE',  ( -0.01753026575586694516, -1.247696154478775021, 1.449428981083925150 ) ) ;
#17250 = CARTESIAN_POINT ( 'NONE',  ( 6.182154858151487353, 6.314861544039274577, -0.7216878364870257245 ) ) ;
#17251 = ADVANCED_FACE ( 'NONE', ( #196336 ), #97991, .F. ) ;
#17252 = CARTESIAN_POINT ( 'NONE',  ( 1.364683531249986537, 1.217708333674754950, -0.7879004041258239610 ) ) ;
#17253 = AXIS2_PLACEMENT_3D ( 'NONE', #197110, #100676, #147318 ) ;
#17254 = CARTESIAN_POINT ( 'NONE',  ( 6.174654088403855212, -1.776896415251895789, -0.5849557326117056366 ) ) ;
#17255 = CARTESIAN_POINT ( 'NONE',  ( 8.367353357928214663, 12.91366268422496688, 1.040834085586084257E-14 ) ) ;
#17256 = LINE ( 'NONE', #164601, #107026 ) ;
#17257 = CARTESIAN_POINT ( 'NONE',  ( 6.684440181240522527, 1.196966437107028547, -1.688953195037292243 ) ) ;
#17258 = SURFACE_STYLE_USAGE ( .BOTH. , #165669 ) ;
#17259 = CARTESIAN_POINT ( 'NONE',  ( 0.4673438449808891004, 1.800595422158430825, 1.021790579661909781 ) ) ;
#17260 = CARTESIAN_POINT ( 'NONE',  ( -0.7500000000000006661, 0.1083333333333560966, -1.299038105676652011 ) ) ;
#17261 = CARTESIAN_POINT ( 'NONE',  ( 7.786460292950004636, 7.978625184730144149, 1.040834085586084257E-14 ) ) ;
#17262 = CARTESIAN_POINT ( 'NONE',  ( -8.148614017013223076, 9.465470093725620870, -1.199719254218446718 ) ) ;
#17263 = CARTESIAN_POINT ( 'NONE',  ( 4.355912491740495440, 8.303924683664389406, 0.000000000000000000 ) ) ;
#17264 = CARTESIAN_POINT ( 'NONE',  ( 5.584674446412367210, -1.345185468269005424, 1.639207791927596247 ) ) ;
#17265 = CARTESIAN_POINT ( 'NONE',  ( 3.573456005653643519, 6.326726552307992080, -1.199719254218453823 ) ) ;
#17266 = CARTESIAN_POINT ( 'NONE',  ( -1.402160292154681736E-14, 1.196875000341419026, -1.575800808251659024 ) ) ;
#17267 = CARTESIAN_POINT ( 'NONE',  ( -1.201851678989727383E-14, 2.462500000000023004, 1.732050807568877637 ) ) ;
#17269 = CARTESIAN_POINT ( 'NONE',  ( 4.009460741339333723, 5.700790169694431420, -1.599625672291256295 ) ) ;
#17268 = CARTESIAN_POINT ( 'NONE',  ( 6.391066755906244623, 0.1909826923555627554, 1.952524381009380861 ) ) ;
#17270 = CARTESIAN_POINT ( 'NONE',  ( 3.145861080134567000, -0.1455099638626895786, -2.010896398064919488 ) ) ;
#17271 = CARTESIAN_POINT ( 'NONE',  ( 3.801880972252824176, -0.9895533254376009946, -1.640229128645746215 ) ) ;
#17272 = EDGE_CURVE ( 'NONE', #22857, #113870, #95632, .T. ) ;
#17273 = CARTESIAN_POINT ( 'NONE',  ( 11.91826849282518275, 10.19999999999999929, -1.400000000000001465 ) ) ;
#17274 = CARTESIAN_POINT ( 'NONE',  ( 1.839652601550560096, 0.8350199954420146620, -2.026445374841173930 ) ) ;
#17275 = CARTESIAN_POINT ( 'NONE',  ( 0.2333690889706925564, 2.018283468528142777, -2.468684669820114586 ) ) ;
#17276 = CARTESIAN_POINT ( 'NONE',  ( 3.128041797164154758, 1.042111378005972311, -1.553157497896196393 ) ) ;
#17277 = CARTESIAN_POINT ( 'NONE',  ( -1.500000000000001332, -0.06874999931718445145, 0.000000000000000000 ) ) ;
#17278 = CARTESIAN_POINT ( 'NONE',  ( -6.886651960737580680, 10.12184548991413457, -1.199719254218440723 ) ) ;
#17280 = CARTESIAN_POINT ( 'NONE',  ( 5.220359425914078422, 2.086072958538415012, 0.3609885457144176302 ) ) ;
#17279 = CARTESIAN_POINT ( 'NONE',  ( -5.097502569058221411, 6.009803087731781623, -1.082531754730544860 ) ) ;
#17281 = CARTESIAN_POINT ( 'NONE',  ( -8.012344526598182026E-15, 8.609375000341403350, -1.575800808251669460 ) ) ;
#17282 = CARTESIAN_POINT ( 'NONE',  ( 6.672334155782003506, -0.9722939650993901450, -1.827837255792996718 ) ) ;
#17284 = CARTESIAN_POINT ( 'NONE',  ( 4.074186250656476993, 7.493853916489129574, -0.5595503573846259959 ) ) ;
#17283 = CARTESIAN_POINT ( 'NONE',  ( 2.753556666441462131, 2.080443298914707917, -0.2074443561481206788 ) ) ;
#17286 = ORIENTED_EDGE ( 'NONE', *, *, #152973, .T. ) ;
#17285 = CARTESIAN_POINT ( 'NONE',  ( 1.025878534523045449, 1.032422052977323590, -1.381481875464431797 ) ) ;
#17287 = CARTESIAN_POINT ( 'NONE',  ( 5.601490020740366838, 9.686822124172440596, 1.040834085586084257E-14 ) ) ;
#17288 =( NAMED_UNIT ( * ) SI_UNIT ( $, .STERADIAN. ) SOLID_ANGLE_UNIT ( ) );
#17289 = PLANE ( 'NONE',  #106917 ) ;
#17290 = CARTESIAN_POINT ( 'NONE',  ( -10.14895191633106819, 5.000000000000002665, 7.601392964450658596 ) ) ;
#17292 = CARTESIAN_POINT ( 'NONE',  ( 7.443063143778065438, 7.785921210603627962, -0.7216878364870257245 ) ) ;
#17291 = CARTESIAN_POINT ( 'NONE',  ( 7.416473721875251890, 8.611306416064660851, 1.199719254218462483 ) ) ;
#17293 = CARTESIAN_POINT ( 'NONE',  ( -2.788906526875773208E-15, 9.437499999999998224, -1.499999999999998446 ) ) ;
#17295 = CARTESIAN_POINT ( 'NONE',  ( 0.4514444101613367955, -1.279852094280601760, -1.282217761895942720 ) ) ;
#17294 = CARTESIAN_POINT ( 'NONE',  ( 5.505492895601038938, 8.580769590579979678, -1.199719254218452047 ) ) ;
#17296 = CARTESIAN_POINT ( 'NONE',  ( -5.682838942422375084, 9.781729199468104596, 0.000000000000000000 ) ) ;
#17297 = CARTESIAN_POINT ( 'NONE',  ( 4.005544317833563461, 6.760553239859419250, -1.199719254218452047 ) ) ;
#17298 = CARTESIAN_POINT ( 'NONE',  ( -6.423141557142870717, 6.808251908967412724, 0.4733936187572094223 ) ) ;
#17299 = CARTESIAN_POINT ( 'NONE',  ( 5.203297092594585393, 9.292540051327542017, 0.7998128361456341429 ) ) ;
#17300 = CARTESIAN_POINT ( 'NONE',  ( 6.539320575229228716, 1.281788455817688188, 2.013036689384885225 ) ) ;
#17301 = CARTESIAN_POINT ( 'NONE',  ( 4.000000000000012434, 0.000000000000000000, 0.7500000000000006661 ) ) ;
#17302 = CARTESIAN_POINT ( 'NONE',  ( 4.008122245411202655, 7.584344604122328803, -0.2404964666735086298 ) ) ;
#17303 = CARTESIAN_POINT ( 'NONE',  ( 8.920901888111989919, 11.43080484092926241, 1.443375672974076540 ) ) ;
#17304 = VERTEX_POINT ( 'NONE', #186466 ) ;
#17305 = AXIS2_PLACEMENT_3D ( 'NONE', #23184, #24255, #71934 ) ;
#17306 = CARTESIAN_POINT ( 'NONE',  ( 2.646735056387524043, -0.3148485976074810733, -1.834047879892097388 ) ) ;
#17307 = CARTESIAN_POINT ( 'NONE',  ( 0.3158528693416655653, 0.9839445311579012587, -1.643420606830671815 ) ) ;
#17308 = CARTESIAN_POINT ( 'NONE',  ( 0.1647065507319189492, -1.628042339203483957, -0.8261295386280396169 ) ) ;
#17309 = DIRECTION ( 'NONE',  ( -5.551115123125765446E-17, 0.000000000000000000, 1.000000000000000000 ) ) ;
#17310 = CARTESIAN_POINT ( 'NONE',  ( -1.510657702057710340E-15, 1.375000000682792267, 1.224999999999963229 ) ) ;
#17311 = CARTESIAN_POINT ( 'NONE',  ( 1.237941840314000785, -1.374772708486730943, 1.500000000000001332 ) ) ;
#17312 = CARTESIAN_POINT ( 'NONE',  ( -3.877268743828284681, 5.546566172598190292, 1.443375672974064550 ) ) ;
#17313 = CARTESIAN_POINT ( 'NONE',  ( 9.408995418203975447, 10.07950886410055524, 0.7216878364870438212 ) ) ;
#17314 = CARTESIAN_POINT ( 'NONE',  ( 4.891434682365626507, -1.802310843600445800, 0.7943598514809721012 ) ) ;
#17315 = CARTESIAN_POINT ( 'NONE',  ( 1.436355765274465623, -1.180822252328097344, -1.761085815303937929 ) ) ;
#17316 = CARTESIAN_POINT ( 'NONE',  ( -4.855791571988752331, 8.816840600628864877, 0.7998128361456481317 ) ) ;
#17317 = CARTESIAN_POINT ( 'NONE',  ( -11.59499170316466099, 8.293181854556747723, 2.924389865657003540 ) ) ;
#17318 = CARTESIAN_POINT ( 'NONE',  ( 9.492660725451591119, -6.771447601804259975, -0.03895569783345582265 ) ) ;
#17319 = CARTESIAN_POINT ( 'NONE',  ( 5.771465802492605768, 1.302860414194568550, 1.761948869136241047 ) ) ;
#17320 = CARTESIAN_POINT ( 'NONE',  ( 4.436495903120683870, 1.889097993355067562, 0.3764034397915373975 ) ) ;
#17321 = CARTESIAN_POINT ( 'NONE',  ( -7.206322340863467346, 8.366129804884193888, 1.199719254218450271 ) ) ;
#17322 = CARTESIAN_POINT ( 'NONE',  ( -1.743066579297358008E-15, 2.250000000682787160, -1.225000000000020739 ) ) ;
#17323 = CARTESIAN_POINT ( 'NONE',  ( 0.9618826090718561872, 0.4271145061440981272, -2.164990749644220447 ) ) ;
#17324 = CARTESIAN_POINT ( 'NONE',  ( 0.000000000000000000, -9.006862915010128035, 0.000000000000000000 ) ) ;
#17325 = ORIENTED_EDGE ( 'NONE', *, *, #31532, .F. ) ;
#17326 = CARTESIAN_POINT ( 'NONE',  ( 0.4019237886466847653, 10.60491455036742892, 1.499999999999997113 ) ) ;
#17327 = EDGE_LOOP ( 'NONE', ( #66567, #70195, #176527, #91238 ) ) ;
#17328 = CARTESIAN_POINT ( 'NONE',  ( 5.752784996495730496, -0.4749413952093975433, -1.911207028377271522 ) ) ;
#17329 = CARTESIAN_POINT ( 'NONE',  ( 1.610778572542032050, -0.2360344744354908597, 1.927585326284560585 ) ) ;
#17330 = CARTESIAN_POINT ( 'NONE',  ( 6.468148293998644327, 1.905381763673856810, 1.285138856061205148 ) ) ;
#17332 = CARTESIAN_POINT ( 'NONE',  ( 4.785918264633797214, -1.142728415277466159, -1.468712688171626812 ) ) ;
#17331 = CARTESIAN_POINT ( 'NONE',  ( -5.596483547390937119, 9.751257581923240991, 0.000000000000000000 ) ) ;
#17333 = CARTESIAN_POINT ( 'NONE',  ( 7.364013710877980401, 8.620379413226322285, -1.199719254218452047 ) ) ;
#17334 =( NAMED_UNIT ( * ) SI_UNIT ( $, .STERADIAN. ) SOLID_ANGLE_UNIT ( ) );
#17335 = CARTESIAN_POINT ( 'NONE',  ( 10.10176665042273392, 1.000000000000000888, 6.279211784079129721 ) ) ;
#17336 = CARTESIAN_POINT ( 'NONE',  ( -5.422371370461663176, 8.413518134592214537, -1.199719254218446718 ) ) ;
#17337 = CARTESIAN_POINT ( 'NONE',  ( -3.305895513212903758, -0.9091400625591844475, 0.2125217450545698883 ) ) ;
#17338 = CARTESIAN_POINT ( 'NONE',  ( 0.4861908890553789941, -2.175720422541329580, -0.2624175912114696252 ) ) ;
#17339 = CARTESIAN_POINT ( 'NONE',  ( 3.701012746850603996, 7.261672604726938651, 1.040834085586084257E-14 ) ) ;
#17340 = ORIENTED_EDGE ( 'NONE', *, *, #161282, .T. ) ;
#17341 = CARTESIAN_POINT ( 'NONE',  ( -1.685698123273788429, -1.399999999999998579, 1.979500400907064916 ) ) ;
#17342 = CARTESIAN_POINT ( 'NONE',  ( 3.022498986271238586, 2.800000000000017586, -2.499999999999995115 ) ) ;
#17343 = CARTESIAN_POINT ( 'NONE',  ( 1.347985785199314668, 1.823511463271022093, 0.09156768404049858701 ) ) ;
#17344 = CARTESIAN_POINT ( 'NONE',  ( -4.731959306369413198, 5.479372931307791461, -1.199719254218446718 ) ) ;
#17345 = CARTESIAN_POINT ( 'NONE',  ( 3.217127751380299383, 1.692560603008624875, 0.3766165182450386117 ) ) ;
#17346 = CARTESIAN_POINT ( 'NONE',  ( -6.567035442730039030, 6.789466400107097677, -0.3981859287331638297 ) ) ;
#17347 = CARTESIAN_POINT ( 'NONE',  ( 6.509000000000012776, 0.5843741663743782233, 2.053293374786519188 ) ) ;
#17348 = CARTESIAN_POINT ( 'NONE',  ( 0.1331565106231363538, 0.2470099659030860484, -1.980838409567912572 ) ) ;
#17349 = CARTESIAN_POINT ( 'NONE',  ( 0.3988885142760539293, 1.602443225120395720, -1.069099046168849876 ) ) ;
#17350 = CARTESIAN_POINT ( 'NONE',  ( 4.100408672059585591, 1.951911038179511726, 0.1965976633130430695 ) ) ;
#17351 = CARTESIAN_POINT ( 'NONE',  ( -7.853197290813634268, 10.18514947741448573, 1.599625672291295375 ) ) ;
#17352 = CARTESIAN_POINT ( 'NONE',  ( 5.289652487626049115, 9.323011668872403845, 0.7998128361456462443 ) ) ;
#17353 = CARTESIAN_POINT ( 'NONE',  ( 4.987034407221377030, -1.996844880220369545, -0.7138980100366009163 ) ) ;
#17354 = CARTESIAN_POINT ( 'NONE',  ( 6.156284269057003655, 9.340026192945279249, -1.199719254218452047 ) ) ;
#17355 = CARTESIAN_POINT ( 'NONE',  ( -8.320953590485107298, 10.73086516036454618, 1.599625672291269396 ) ) ;
#17356 = CARTESIAN_POINT ( 'NONE',  ( 4.364835388595708743, 7.179726155748598515, 1.199719254218462483 ) ) ;
#17357 = CARTESIAN_POINT ( 'NONE',  ( 2.957943426865859760, -0.6537446763684885420, 1.964363857337739105 ) ) ;
#17359 = CARTESIAN_POINT ( 'NONE',  ( -1.402160292154681736E-14, 0.2593750003414224681, -1.575800808251665908 ) ) ;
#17358 = CARTESIAN_POINT ( 'NONE',  ( 2.064209525776505849, 8.524375063532966479, -2.459883114193431197 ) ) ;
#17360 = ORIENTED_EDGE ( 'NONE', *, *, #85411, .F. ) ;
#17361 = CARTESIAN_POINT ( 'NONE',  ( 2.901363961662834168, -1.135721475377445167, -1.998492394250019233 ) ) ;
#17362 = CARTESIAN_POINT ( 'NONE',  ( 8.812436659202669276, 10.34389285956704363, -1.082531754730543083 ) ) ;
#17364 = CARTESIAN_POINT ( 'NONE',  ( 1.642778471875000035, -2.326041666188709112, -2.845375778867859751 ) ) ;
#17363 = CARTESIAN_POINT ( 'NONE',  ( 4.895902868310594513, 8.725987423088758632, 0.000000000000000000 ) ) ;
#17365 = DIRECTION ( 'NONE',  ( -0.000000000000000000, 1.000000000000000000, -0.000000000000000000 ) ) ;
#17366 = DIRECTION ( 'NONE',  ( 0.000000000000000000, 0.000000000000000000, 1.000000000000000000 ) ) ;
#17367 = VERTEX_POINT ( 'NONE', #170222 ) ;
#17368 = CARTESIAN_POINT ( 'NONE',  ( -5.152983112885297217E-15, -6.594478602028688741, 10.23203630735471137 ) ) ;
#17369 = CARTESIAN_POINT ( 'NONE',  ( 3.884940529579200774, -1.786240503712609895, -0.6835825222790415934 ) ) ;
#17370 = CARTESIAN_POINT ( 'NONE',  ( -3.130644732418688569, 6.137896444317757272, -0.8662315412496863765 ) ) ;
#17371 = CARTESIAN_POINT ( 'NONE',  ( 5.368053323270940425, 0.8530656342727646058, 1.498931087277301843 ) ) ;
#17372 = CARTESIAN_POINT ( 'NONE',  ( 3.591030000661588062, 1.731995077137841843, 1.032480907900306111 ) ) ;
#17373 = CARTESIAN_POINT ( 'NONE',  ( 5.555437251493606787, -1.460316692103363456, 1.775274546321881530 ) ) ;
#17374 = DIRECTION ( 'NONE',  ( 0.000000000000000000, 0.000000000000000000, 1.000000000000000000 ) ) ;
#17375 = CARTESIAN_POINT ( 'NONE',  ( 0.3466626200071438180, 2.201290530325435757, 0.1579762268871589825 ) ) ;
#17376 = CARTESIAN_POINT ( 'NONE',  ( -4.746763178560296836, 6.631252689777363152, 1.443375672974058777 ) ) ;
#17377 = CARTESIAN_POINT ( 'NONE',  ( 6.274623264596165484, -1.681128386917314366, -0.5530667918781423387 ) ) ;
#17378 = EDGE_CURVE ( 'NONE', #82863, #33705, #209850, .T. ) ;
#17380 = CARTESIAN_POINT ( 'NONE',  ( 1.676131343691760645, -1.223425685817343789, 1.938311714834321631 ) ) ;
#17379 = CARTESIAN_POINT ( 'NONE',  ( 4.362691568547328202, 8.311833606605697256, -0.7998128361456381397 ) ) ;
#17381 = CARTESIAN_POINT ( 'NONE',  ( 6.685540632719009224, -0.7820230359689305244, 1.665195522482863399 ) ) ;
#17382 = CARTESIAN_POINT ( 'NONE',  ( -7.553827861469316396, 8.841829255582865699, -1.199719254218452047 ) ) ;
#17383 = CARTESIAN_POINT ( 'NONE',  ( 6.421842908546858908, 1.265077015623069290, -1.789241164368003068 ) ) ;
#17384 = CARTESIAN_POINT ( 'NONE',  ( -5.002032328799064231, 4.800402236545811441, -0.7998128361456362523 ) ) ;
#17385 = CARTESIAN_POINT ( 'NONE',  ( 0.6801582343749883464, -0.7447916663252535097, 1.178068619123796568 ) ) ;
#17386 = CARTESIAN_POINT ( 'NONE',  ( -0.02988540731103107514, 0.005807295984020740404, -1.726291166677936362 ) ) ;
#17387 = CARTESIAN_POINT ( 'NONE',  ( 0.6960477194701603088, -1.535568182542995208, -1.535184517522319769 ) ) ;
#17388 = CARTESIAN_POINT ( 'NONE',  ( 1.059780186608853203, 1.205045252304644210, 1.616690996016925563 ) ) ;
#17389 = CARTESIAN_POINT ( 'NONE',  ( -1.402160292154681736E-14, 0.6187500006828180465, -1.732050807568863648 ) ) ;
#17390 = CARTESIAN_POINT ( 'NONE',  ( 5.707627890916790570, -0.4656921374228146226, 1.869253615786143685 ) ) ;
#17391 = CARTESIAN_POINT ( 'NONE',  ( -1.364683531250000748, 12.10937500034139980, 0.000000000000000000 ) ) ;
#17392 = CARTESIAN_POINT ( 'NONE',  ( 2.356001076229676805, -1.649452400593539148, -1.488157709660995920 ) ) ;
#17393 = ORIENTED_EDGE ( 'NONE', *, *, #162539, .F. ) ;
#17394 = FACE_OUTER_BOUND ( 'NONE', #51817, .T. ) ;
#17395 = CARTESIAN_POINT ( 'NONE',  ( 8.378048858240820351, 11.86180853700128601, -1.199719254218446718 ) ) ;
#17396 = CYLINDRICAL_SURFACE ( 'NONE', #132382, 0.07999999999999998779 ) ;
#17397 = CARTESIAN_POINT ( 'NONE',  ( 3.791513125430877373, 7.352524219418101303, -0.3677586026353037996 ) ) ;
#17398 = CARTESIAN_POINT ( 'NONE',  ( 4.511116409865087995, -1.705632679577104849, 0.3454082310308664305 ) ) ;
#17399 = CARTESIAN_POINT ( 'NONE',  ( 3.473055881322492322, 1.772541284497713976, 0.8411618914155661875 ) ) ;
#17401 = CARTESIAN_POINT ( 'NONE',  ( -8.202319746587722449, 8.671720580548228696, 1.040834085586084257E-14 ) ) ;
#17400 = CARTESIAN_POINT ( 'NONE',  ( 4.660252114795294887, 6.460046772059735432, -1.599625672291256295 ) ) ;
#17402 = CARTESIAN_POINT ( 'NONE',  ( -5.908080316777766683, 6.002527095666024159, -0.1116623552285273685 ) ) ;
#17403 = CARTESIAN_POINT ( 'NONE',  ( 10.16199982864259788, 11.81442020729326536, 1.199719254218452047 ) ) ;
#17404 = CARTESIAN_POINT ( 'NONE',  ( 0.5552253240413919100, 1.715889405040219584, -1.144428160675447614 ) ) ;
#17405 = CARTESIAN_POINT ( 'NONE',  ( -7.802881099864745984, 9.062115023719057305, -1.199719254218446718 ) ) ;
#17406 = ADVANCED_FACE ( 'NONE', ( #106349 ), #4489, .F. ) ;
#17407 = CARTESIAN_POINT ( 'NONE',  ( -3.999292125906916073, 5.688926785023260102, 1.443375672974064550 ) ) ;
#17408 = CARTESIAN_POINT ( 'NONE',  ( 1.692605830730309791, -2.251738780704269249, -0.2206997258237669290 ) ) ;
#17409 = ORIENTED_EDGE ( 'NONE', *, *, #120455, .F. ) ;
#17410 = CARTESIAN_POINT ( 'NONE',  ( -1.402160292154681736E-14, 0.2437500006828163535, 1.732050807568877637 ) ) ;
#17411 = CARTESIAN_POINT ( 'NONE',  ( 2.706148147531197701, -0.7121320899835179574, -1.729884524348634933 ) ) ;
#17412 = CARTESIAN_POINT ( 'NONE',  ( 0.9669347054478127923, -1.691490974053434959, -0.3813910478582624441 ) ) ;
#17413 = CARTESIAN_POINT ( 'NONE',  ( 5.759372899636661991, 2.159370146098410714, -0.3733810082120898044 ) ) ;
#17414 = CARTESIAN_POINT ( 'NONE',  ( 6.545943480548680249, 0.8917086005404940563, -2.128542236993334669 ) ) ;
#17415 = CARTESIAN_POINT ( 'NONE',  ( 1.569287236123186213, 0.1524497474049029966, -2.055318472165644117 ) ) ;
#17416 = CARTESIAN_POINT ( 'NONE',  ( 3.486211078826762844, -0.3796756879693505837, -1.904310675543115394 ) ) ;
#17417 = CARTESIAN_POINT ( 'NONE',  ( -3.917943204224914933, 6.554388924028945240, -1.082531754730548412 ) ) ;
#17418 = B_SPLINE_SURFACE_WITH_KNOTS ( 'NONE', 1, 3, ( 
 ( #196729, #48369, #114482, #180479, #32098, #201576, #184272, #168041, #135552, #67304, #150742, #19643, #18575, #20697, #53222, #119353, #166985, #151803, #4435, #103044, #84653, #185340, #117218, #169099, #36963, #86788, #149664, #132385, #38045, #1243, #165910, #152857, #2304, #182138, #70504, #85716, #136620, #52159, #3377, #199451, #202646, #54295, #51093, #133445, #120433, #104114, #186407, #69444, #170162, #82513, #99846, #34821, #116151, #183216, #68380, #198385, #148600, #169, #66236, #50027, #33768, #101973, #17495, #134510, #83582, #200514, #100896, #118286, #35896, #124708, #141976, #123653, #172313, #107371, #59616, #206925, #173392, #205860, #121508, #41261, #26039, #92152, #156062, #24975, #188549, #154994, #5499, #58554, #91078, #125773, #158205, #9794, #39110, #189615, #74811, #71580, #57492, #138755, #157138, #87859, #187480, #106293, #75869, #23902, #207988, #171231, #22826, #108443, #43390, #191734, #109511, #88941, #8730, #6579, #174463, #40179, #21751, #105194, #153931, #137688, #140912, #190667, #72659, #42327, #203709, #90008, #204773, #55356, #7650, #56428, #122587, #73735, #139832, #10847, #28185, #46585, #63881, #48711, #94281, #179776, #175519, #145177, #76920, #110573, #160322, #161401, #79059, #93215, #77998, #131085, #163524, #126840, #27107, #61755, #12985, #211182, #15111, #212247, #177650, #193875, #159247, #127923, #143047, #112704, #45523, #30330, #192798, #130035, #209042, #81200, #44457, #176575, #196026, #146230, #31393, #62808, #210115, #11926, #144121, #97468, #111639, #128969, #80125, #96414, #194949, #47662, #147278, #178714, #64935, #213310, #197074, #60678, #29259, #95351, #162463, #14039, #113773, #184015, #118028, #100641, #116956, #133182, #152592, #32450, #84394, #65972, #36699, #214342, #180823, #82251, #68111, #69181, #182955, #181874, #35631, #101709, #166718, #34570, #199182, #4179, #98519, #150481, #132121, #102784 ),
 ( #164581, #85457, #167781, #70249, #168842, #119093, #198131, #134248, #19377, #16166, #2041, #17235, #151543, #148342, #49763, #50829, #20445, #18308, #86527, #115889, #33510, #201315, #136363, #202383, #114825, #99583, #200254, #165647, #52954, #67045, #83310, #149397, #185073, #979, #3110, #135301, #51906, #24716, #89759, #204517, #38850, #9545, #188286, #103855, #90819, #173135, #5241, #169904, #121251, #139572, #156882, #141730, #187221, #58302, #54033, #23651, #21492, #203448, #104933, #39926, #172057, #186147, #170975, #75621, #42073, #71317, #120170, #154739, #106035, #155808, #108187, #8469, #56165, #72396, #37781, #6322, #87602, #205599, #138496, #123397, #137430, #74555, #153673, #174213, #55102, #22574, #140656, #206670, #124457, #7391, #88680, #122329, #73471, #190416, #57237, #189361, #25786, #41002, #107112, #91897, #157953, #29003, #97220, #31146, #179527, #125519, #163272, #94026, #43148, #76674, #60425, #127662, #96159, #113518, #95090, #143864, #78799, #14854, #178460, #144923, #177389, #92959, #12726, #211991, #63632, #193624, #210929, #10598, #207738, #80944, #159005, #176326, #142789, #59362, #62555, #191480, #77743, #162211, #128718, #129786, #209857, #208795, #45266, #126585, #111386, #192546, #195767, #44199, #110320, #27933, #47406, #109261, #160065, #175269, #11669, #13796, #79870, #61495, #26854, #161138, #194690, #46332, #112447, #30069, #145979, #131870, #115629, #19124, #717, #164329, #15919, #82002, #100388, #85203, #181624, #117778, #51656, #34313, #18050, #200006, #197878, #66782, #84137, #83060, #151287, #183769, #35379, #16980, #1795, #68928, #167526, #149136, #101454, #33253, #2858, #135048, #201061, #214095, #196825, #102524, #65722, #148089, #52702, #132922, #32195, #118833, #150225, #184819, #116695, #67852, #49509, #36449, #168586, #99337, #165386, #20186, #147036, #213058, #134000, #64688, #130833, #198927, #50573, #180573 ) ),
 .UNSPECIFIED., .F., .T., .F.,
 ( 2, 2 ),
 ( 4, 2, 2, 2, 2, 2, 2, 2, 2, 2, 2, 2, 2, 2, 2, 2, 2, 2, 2, 2, 2, 2, 2, 2, 2, 2, 2, 2, 2, 2, 2, 2, 2, 2, 2, 2, 2, 2, 2, 2, 2, 2, 2, 2, 2, 2, 2, 2, 2, 2, 2, 2, 2, 2, 2, 2, 2, 2, 2, 2, 2, 2, 2, 2, 2, 2, 2, 2, 2, 2, 2, 2, 2, 2, 2, 2, 2, 2, 2, 2, 2, 2, 2, 2, 2, 2, 2, 2, 2, 2, 2, 2, 2, 2, 2, 2, 2, 2, 2, 2, 2, 2, 2, 2, 2, 2, 2, 2, 2, 2, 2, 4 ),
 ( 0.000000000000000000, 1.000000000000000000 ),
 ( 0.0003185708494972700616, 0.0004481554763622086794, 0.0005777401032271472971, 0.0007073247300920859149, 0.0008369093569570245326, 0.0009017016703894938957, 0.0009664939838219631504, 0.001031286297254432405, 0.001096078610686901768, 0.001225663237551840277, 0.001290455550984309641, 0.001322851707700544322, 0.001355247864416779004, 0.001420040177849248367, 0.001484832491281717730, 0.001614417118146656239, 0.001679209431579125385, 0.001744001745011594749, 0.001808794058444064112, 0.001873586371876533475, 0.001938378685309002621, 0.002003170998741471767, 0.002067963312173941130, 0.002132755625606410493, 0.002197547939038879856, 0.002229944095755114538, 0.002262340252471349220, 0.002391924879336287946, 0.002521509506201226672, 0.002586301819633696035, 0.002651094133066165398, 0.002715886446498634761, 0.002780678759931104124, 0.002910263386796042417, 0.002975055700228511346, 0.003039848013660980709, 0.003104640327093450072, 0.003169432640525919435, 0.003299017267390858162, 0.003428601894255796888, 0.003493394207688266251, 0.003558186521120735614, 0.003622978834553204977, 0.003687771147985673906, 0.003817355774850612199, 0.003946940401715550925, 0.003979336558431785173, 0.004011732715148020288, 0.004076525028580489651, 0.004141317342012959014, 0.004206109655445428377, 0.004270901968877897741, 0.004335694282310367104, 0.004400486595742836467, 0.004465278909175305830, 0.004594863536040244556, 0.004659655849472713919, 0.004724448162905183282, 0.004789240476337652645, 0.004854032789770122008, 0.004918825103202591371, 0.004983617416635060735, 0.005048409730067530098, 0.005113202043499999461, 0.005177994356932468824, 0.005210390513648703939, 0.005242786670364938187, 0.005372371297229876913, 0.005501955924094814772, 0.005566748237527284135, 0.005631540550959752631, 0.005696332864392221994, 0.005761125177824691357, 0.005890709804689630083, 0.005955502118122099446, 0.006020294431554568809, 0.006085086744987038172, 0.006149879058419507535, 0.006214671371851976898, 0.006279463685284446262, 0.006409048312149384988, 0.006473840625581854351, 0.006506236782298089466, 0.006538632939014323714, 0.006603425252446793077, 0.006668217565879262440, 0.006797802192744201166, 0.006862594506176670529, 0.006927386819609139892, 0.006992179133041609256, 0.007056971446474078619, 0.007121763759906547982, 0.007186556073339017345, 0.007251348386771486708, 0.007316140700203956071, 0.007380933013636425434, 0.007445725327068894797, 0.007510517640501363293, 0.007575309953933832656, 0.007704894580798770515, 0.007769686894231239878, 0.007834479207663709241, 0.007866875364379945224, 0.007899271521096179471, 0.007964063834528647967, 0.008093648461393586693, 0.008158440774826056924, 0.008223233088258525419, 0.008288025401690993915, 0.008352817715123464146, 0.008482402341988402872, 0.008611986968853341598 ),
 .UNSPECIFIED. ) ;
#17419 = CARTESIAN_POINT ( 'NONE',  ( 6.151601556293980089, 0.5431611868166182910, -1.789914130245950474 ) ) ;
#17420 = CARTESIAN_POINT ( 'NONE',  ( 0.7500000000000005551, 4.270513119278528127E-14, 2.052068128417952497 ) ) ;
#17421 = CARTESIAN_POINT ( 'NONE',  ( 4.038955833855768063, 7.541343398062151593, 0.4257906834902285276 ) ) ;
#17422 = CARTESIAN_POINT ( 'NONE',  ( 6.714220164357198151, -1.617572894677368422, -1.203167480739217643 ) ) ;
#17423 = CARTESIAN_POINT ( 'NONE',  ( 2.943528747942701695, 6.448217615992859919, 0.000000000000000000 ) ) ;
#17424 = CARTESIAN_POINT ( 'NONE',  ( -0.6801582343750368631, 1.682291667008048552, 1.178068619123803451 ) ) ;
#17425 = CARTESIAN_POINT ( 'NONE',  ( 4.781875055470904634, 1.674888562130649960, -1.122497055794105192 ) ) ;
#17426 = CARTESIAN_POINT ( 'NONE',  ( -4.744990574658554117, 4.638169879964154418, 1.214306433183764966E-14 ) ) ;
#17427 = CARTESIAN_POINT ( 'NONE',  ( 7.584896871841365851, 10.93646455286856956, -1.199719254218446718 ) ) ;
#17428 = CARTESIAN_POINT ( 'NONE',  ( 5.727393547130178675, 5.646656991265468939, 0.000000000000000000 ) ) ;
#17430 = SURFACE_STYLE_FILL_AREA ( #47863 ) ;
#17429 = CARTESIAN_POINT ( 'NONE',  ( 2.385134503015675200, 1.669401249834654433, -0.7394980648879890817 ) ) ;
#17431 = CARTESIAN_POINT ( 'NONE',  ( 6.661184041422462343, -7.645986912801310709, -6.773376349081635439 ) ) ;
#17432 = CARTESIAN_POINT ( 'NONE',  ( -1.225000000000016076, 1.812500000682795598, -2.081668171172168513E-14 ) ) ;
#17433 = ORIENTED_EDGE ( 'NONE', *, *, #118416, .F. ) ;
#17434 = CARTESIAN_POINT ( 'NONE',  ( -4.434925645001610128, 8.188180662561590495, 0.7216878364870338292 ) ) ;
#17435 = CARTESIAN_POINT ( 'NONE',  ( -1.271070482941953461, 8.436788551174030815, 10.93994114196923739 ) ) ;
#17436 = CARTESIAN_POINT ( 'NONE',  ( -7.808606406466886973, 11.19745900993164511, 1.199719254218453823 ) ) ;
#17437 = CARTESIAN_POINT ( 'NONE',  ( 6.621752733038558603, -0.4373435798001067965, 1.978785184894470639 ) ) ;
#17438 = CARTESIAN_POINT ( 'NONE',  ( 0.5047332052380922862, -2.104974169346077506, -0.2554120829242333968 ) ) ;
#17439 = ORIENTED_EDGE ( 'NONE', *, *, #154446, .F. ) ;
#17440 = CARTESIAN_POINT ( 'NONE',  ( -6.668631453075260396, 8.873432343378178544, -1.599625672291271394 ) ) ;
#17441 = CARTESIAN_POINT ( 'NONE',  ( 6.017121246366603060, 5.914396297049491658, 1.040834085586084257E-14 ) ) ;
#17442 = AXIS2_PLACEMENT_3D ( 'NONE', #29341, #96499, #10929 ) ;
#17443 = CARTESIAN_POINT ( 'NONE',  ( 5.998915433584960155, 1.686223865786851128, -1.184587077384538167 ) ) ;
#17444 = CARTESIAN_POINT ( 'NONE',  ( 5.063125043234593115, -1.117834493326537393, 1.678003986596336761 ) ) ;
#17445 = ORIENTED_EDGE ( 'NONE', *, *, #35088, .F. ) ;
#17446 = ORIENTED_EDGE ( 'NONE', *, *, #140681, .F. ) ;
#17447 = CARTESIAN_POINT ( 'NONE',  ( 2.892933200463445154, 6.441114558253461908, 0.3893011784570130640 ) ) ;
#17448 = CARTESIAN_POINT ( 'NONE',  ( -0.2108831679770924727, 4.091978752061476321, -2.452067053820900178 ) ) ;
#17451 = ORIENTED_EDGE ( 'NONE', *, *, #129734, .F. ) ;
#17450 = CARTESIAN_POINT ( 'NONE',  ( 1.499999999999990896, 5.275000000000022560, 1.214306433183764966E-14 ) ) ;
#17449 = CARTESIAN_POINT ( 'NONE',  ( -5.498713818794216834, 8.572860667638675380, -1.199719254218452047 ) ) ;
#17452 = CARTESIAN_POINT ( 'NONE',  ( 5.057296774772758852, 7.978757421411086348, 1.172581024337983724 ) ) ;
#17453 = CARTESIAN_POINT ( 'NONE',  ( 5.677111188754776272, -0.9039728708103295096, -1.802140534545144890 ) ) ;
#17454 = CARTESIAN_POINT ( 'NONE',  ( 4.945164379994194448, 0.5744887182440976403, -1.749284230371531024 ) ) ;
#17455 = CARTESIAN_POINT ( 'NONE',  ( -0.9657642407454779532, -4.140281660848668999, -0.3272472668956744601 ) ) ;
#17456 = CARTESIAN_POINT ( 'NONE',  ( 3.159088808783340419, -1.747439373373047333, 1.507377025801335702 ) ) ;
#17457 = CARTESIAN_POINT ( 'NONE',  ( 7.828907357248368726, 8.098423103070084395, 0.7998128361456281477 ) ) ;
#17458 = CARTESIAN_POINT ( 'NONE',  ( 4.921240491056324551, -0.1114908479964340365, 2.158860929761210912 ) ) ;
#17459 = CARTESIAN_POINT ( 'NONE',  ( 8.067265095331215718, 9.370563018429956870, 1.199719254218462483 ) ) ;
#17460 = CARTESIAN_POINT ( 'NONE',  ( 0.6088030852571654217, -0.2837962540496056785, 1.921085339388538982 ) ) ;
#17461 = CARTESIAN_POINT ( 'NONE',  ( -3.411848212133334446, 7.132240014130862171, 0.7998128361456341429 ) ) ;
#17462 = EDGE_LOOP ( 'NONE', ( #99648, #51992, #11358, #213136 ) ) ;
#17463 = AXIS2_PLACEMENT_3D ( 'NONE', #62159, #128317, #194280 ) ;
#17464 = CARTESIAN_POINT ( 'NONE',  ( 2.617062827300069117, 0.3852370113777958682, -0.1797355214283801461 ) ) ;
#17465 = CARTESIAN_POINT ( 'NONE',  ( -4.980641328173854632, 6.904110530993182948, 1.599625672291263179 ) ) ;
#17466 = CARTESIAN_POINT ( 'NONE',  ( 3.959713429720784106, 1.856571849420919795, -0.2284545790810637578 ) ) ;
#17469 = CARTESIAN_POINT ( 'NONE',  ( -5.152980901645737077, 8.169505597632108262, -1.199719254218453823 ) ) ;
#17468 = CARTESIAN_POINT ( 'NONE',  ( 1.499999999999987566, -0.6937499993171849511, 0.000000000000000000 ) ) ;
#17467 = CARTESIAN_POINT ( 'NONE',  ( 0.8614045922798494459, -1.509235727096858826, -1.174430983434850972 ) ) ;
#17470 = CARTESIAN_POINT ( 'NONE',  ( 2.350463684150871035, 2.206416367115513477, 0.05273732197710182673 ) ) ;
#17471 = CARTESIAN_POINT ( 'NONE',  ( -5.586852281741751192, 6.234037913494448802, 1.005928974618113481 ) ) ;
#17472 = CARTESIAN_POINT ( 'NONE',  ( 3.344057444064992168, 7.053150784717805877, 1.040834085586084257E-14 ) ) ;
#17473 = CARTESIAN_POINT ( 'NONE',  ( 7.065207446052794715, 9.336104335185329006, -1.443375672974064550 ) ) ;
#17474 = CARTESIAN_POINT ( 'NONE',  ( -4.029797971759847997, 5.724516938518342535, -1.599625672291256295 ) ) ;
#17475 = CARTESIAN_POINT ( 'NONE',  ( -6.577113915960836721, 8.766661883411348555, -1.443375672974066548 ) ) ;
#17476 = CARTESIAN_POINT ( 'NONE',  ( 1.018749824907847934, 1.819822117139553885, 0.7584178161138422913 ) ) ;
#17477 = CARTESIAN_POINT ( 'NONE',  ( 0.2535066641492569883, -1.850528970283831010, 1.378429844982787422 ) ) ;
#17478 = CARTESIAN_POINT ( 'NONE',  ( 1.310910670669521272, -1.548711629584406113, 1.204245502051364936 ) ) ;
#17479 = CARTESIAN_POINT ( 'NONE',  ( 4.434473652564925317, -1.191674006009019404, 1.683292407194038054 ) ) ;
#17480 = CARTESIAN_POINT ( 'NONE',  ( 6.155038550924150087, 7.243595066575396757, 1.082531754730558626 ) ) ;
#17481 = CARTESIAN_POINT ( 'NONE',  ( 5.169401708560450004, 9.252995436621013425, 0.000000000000000000 ) ) ;
#17482 = ORIENTED_EDGE ( 'NONE', *, *, #207043, .F. ) ;
#17483 = CARTESIAN_POINT ( 'NONE',  ( -1.364683531250012516, 4.551041667008082214, -0.7879004041258300672 ) ) ;
#17484 = DIRECTION ( 'NONE',  ( -1.000000000000000000, 0.000000000000000000, 0.000000000000000000 ) ) ;
#17485 = CARTESIAN_POINT ( 'NONE',  ( 5.138177029454852551, 5.096887410559856946, 0.7216878364870317197 ) ) ;
#17486 = CARTESIAN_POINT ( 'NONE',  ( 0.4444779246538512751, -1.024716592377757696, 1.914062593285012603 ) ) ;
#17488 = CARTESIAN_POINT ( 'NONE',  ( 6.040549724581927293, -1.551790349881351450, 0.9907606852931831742 ) ) ;
#17487 = CARTESIAN_POINT ( 'NONE',  ( 2.679285714285720044, -0.4970443252110337551, -0.09999999999999592548 ) ) ;
#17489 = CARTESIAN_POINT ( 'NONE',  ( -5.181866634007240791, 6.340624232048664766, 1.284222742053082733 ) ) ;
#17490 = DIRECTION ( 'NONE',  ( -1.276756478318932585E-15, 1.000000000000000000, -1.665334536937738262E-16 ) ) ;
#17491 = CARTESIAN_POINT ( 'NONE',  ( 1.616246341788161622, 1.260175398906153266, -1.382505567627971388 ) ) ;
#17492 = CARTESIAN_POINT ( 'NONE',  ( 5.167319818800252484, 0.2175342549677051207, -2.150644138106901693 ) ) ;
#17493 = CARTESIAN_POINT ( 'NONE',  ( -5.747036748294815922, 6.247280920146251582, 1.064921034751656226 ) ) ;
#17494 = CARTESIAN_POINT ( 'NONE',  ( -0.02264175331115596268, 2.007280006360371960, -2.503048469261221598 ) ) ;
#17495 = CARTESIAN_POINT ( 'NONE',  ( 6.489313741793890422, 6.842916442627623219, -0.5960428994750706089 ) ) ;
#17496 = CARTESIAN_POINT ( 'NONE',  ( -1.364683531249997417, 5.071875000341417916, 1.214306433183764966E-14 ) ) ;
#17497 = CARTESIAN_POINT ( 'NONE',  ( 1.559083858985313320, -1.614856622157490706, 1.023943737511850083 ) ) ;
#17498 = CARTESIAN_POINT ( 'NONE',  ( 2.500565701108145689, 1.422975883020457077, -1.052153950563482265 ) ) ;
#17499 = CARTESIAN_POINT ( 'NONE',  ( 1.084454188491505988, -1.212558158303609135, 1.478703618145213783 ) ) ;
#17501 = CARTESIAN_POINT ( 'NONE',  ( 4.903869178324737454, -1.028422014321051403, -1.615943446245589943 ) ) ;
#17500 = CARTESIAN_POINT ( 'NONE',  ( 3.105163759955598124, -3.206389149015671514, 1.164969029660678723 ) ) ;
#17502 = CARTESIAN_POINT ( 'NONE',  ( 5.090277013941287620, 1.014100869069594291, -1.688273828314874825 ) ) ;
#17503 = CARTESIAN_POINT ( 'NONE',  ( 1.301209403646291118, -0.3165094942152619772, -2.096747597609450953 ) ) ;
#17504 = CARTESIAN_POINT ( 'NONE',  ( -1.326716514427061987E-15, 2.999999999999988454, -1.225000000000003864 ) ) ;
#17505 = CARTESIAN_POINT ( 'NONE',  ( 3.608139902456270143, -0.7572706533398064765, -1.710698989992056607 ) ) ;
#17507 = VERTEX_POINT ( 'NONE', #107428 ) ;
#17506 = CARTESIAN_POINT ( 'NONE',  ( 0.1701549220758866166, -1.195335944658926230, 1.380069390326914336 ) ) ;
#17509 = CARTESIAN_POINT ( 'NONE',  ( 4.851297196472967421, 8.072458764906237150, -0.9094135686919021522 ) ) ;
#17508 = CARTESIAN_POINT ( 'NONE',  ( 3.035963658818414235, -1.482449291622448095, -1.634993338104336891 ) ) ;
#17510 = EDGE_CURVE ( 'NONE', #106638, #92178, #25033, .T. ) ;
#17511 = CARTESIAN_POINT ( 'NONE',  ( 1.364683531249990311, 4.926041667008083991, 0.7879004041258500513 ) ) ;
#17512 = CARTESIAN_POINT ( 'NONE',  ( 1.715356188534086224, -1.767971037936959089, -1.062312629515406170 ) ) ;
#17513 = CARTESIAN_POINT ( 'NONE',  ( 4.937140493670735708, 8.911747675924535983, -0.7998128361456281477 ) ) ;
#17514 = CARTESIAN_POINT ( 'NONE',  ( -9.612894607289142357, 11.17379744904754801, -1.199719254218441611 ) ) ;
#17515 = DIRECTION ( 'NONE',  ( -3.330669073875479482E-16, 3.330669073875479482E-16, 1.000000000000000000 ) ) ;
#17516 = CARTESIAN_POINT ( 'NONE',  ( 0.000000000000000000, 6.999999999999999112, 0.000000000000000000 ) ) ;
#17517 = CARTESIAN_POINT ( 'NONE',  ( 6.381121926128928479, -1.751337275642101510, -0.7685668267764720341 ) ) ;
#17518 = VERTEX_POINT ( 'NONE', #171291 ) ;
#17519 = CARTESIAN_POINT ( 'NONE',  ( 4.123533666479628046, 0.2564666318346648377, -2.054367117340555549 ) ) ;
#17520 = CARTESIAN_POINT ( 'NONE',  ( -1.364683531250000748, -0.9281249996585805295, 0.000000000000000000 ) ) ;
#17521 = CARTESIAN_POINT ( 'NONE',  ( 1.915512222264357467, -0.2666219456287990952, 2.145042957367573777 ) ) ;
#17522 = CARTESIAN_POINT ( 'NONE',  ( -5.962047440371475382, 7.122956488241998230, -1.095284208787988822 ) ) ;
#17523 = CARTESIAN_POINT ( 'NONE',  ( 2.420574729456357765, -0.7750317791199374806, -1.865254733019072297 ) ) ;
#17524 = CYLINDRICAL_SURFACE ( 'NONE', #4335, 2.250000000000006661 ) ;
#17525 = ORIENTED_EDGE ( 'NONE', *, *, #5141, .T. ) ;
#17527 = CARTESIAN_POINT ( 'NONE',  ( 8.920901888111997025, 10.47043562662792304, 1.082531754730549967 ) ) ;
#17526 = CARTESIAN_POINT ( 'NONE',  ( 1.737499999999999378, -3.266666666666667496, -3.009438278150925683 ) ) ;
#17528 = CARTESIAN_POINT ( 'NONE',  ( 6.679064532090532857, -0.9478974852125362505, -1.779352858464311016 ) ) ;
#17529 = CARTESIAN_POINT ( 'NONE',  ( 0.7785302072789467287, -0.4946362931835950327, -1.954778448132548752 ) ) ;
#17530 = CARTESIAN_POINT ( 'NONE',  ( 5.056268342064010213, -1.587557771011731678, 1.511049258477934032 ) ) ;
#17531 = CARTESIAN_POINT ( 'NONE',  ( 0.7499999999999902300, 3.514583334016149863, 1.299038105676669330 ) ) ;
#17532 = CARTESIAN_POINT ( 'NONE',  ( 3.920094060441734030, -1.906919942518231936, 0.1457910263855527466 ) ) ;
#17533 = CARTESIAN_POINT ( 'NONE',  ( -4.741601036477307574, 6.554953847355395880, 1.599625672291267398 ) ) ;
#17534 = CARTESIAN_POINT ( 'NONE',  ( 3.158686601859607368, 6.628958768904106513, -0.7216878364870267237 ) ) ;
#17536 = CARTESIAN_POINT ( 'NONE',  ( 2.319935610374638468, 0.9480221781073931986, -1.779637559903464394 ) ) ;
#17535 = CARTESIAN_POINT ( 'NONE',  ( 4.296393142825893463, -0.4330127018922214077, -4.470011852588159584 ) ) ;
#17537 = CARTESIAN_POINT ( 'NONE',  ( 0.6823417656249934904, 13.00520833367473017, 1.181850606188764807 ) ) ;
#17539 = CARTESIAN_POINT ( 'NONE',  ( -4.522526758610270647, 7.433975764090723359, -1.199719254218453823 ) ) ;
#17538 = CARTESIAN_POINT ( 'NONE',  ( 0.4160993436025617886, -1.233022138464324291, -1.932370275504050827 ) ) ;
#17540 = CARTESIAN_POINT ( 'NONE',  ( 4.436358534413815669, 1.691719876958649227, 0.3350348670820638142 ) ) ;
#17541 = CARTESIAN_POINT ( 'NONE',  ( -0.1399997263889612154, 1.357298622859518078, -2.254419820505838334 ) ) ;
#17542 = CARTESIAN_POINT ( 'NONE',  ( 5.196852952739813070, 4.957416621151553571, -0.7998128361456221525 ) ) ;
#17543 = CARTESIAN_POINT ( 'NONE',  ( 11.86145016429273014, 11.00587408513255028, 1.099999999999996536 ) ) ;
#17544 = CARTESIAN_POINT ( 'NONE',  ( 0.8890225878602634468, 0.1407106197201784259, 1.956863499422318631 ) ) ;
#17545 =( BOUNDED_SURFACE ( )  B_SPLINE_SURFACE ( 3, 2, ( 
 ( #90002, #51356, #156055 ),
 ( #7643, #183471, #68635 ),
 ( #134759, #73728, #210107 ),
 ( #209035, #43383, #12978 ),
 ( #141969, #175511, #174456 ),
 ( #91070, #189608, #10840 ) ),
 .UNSPECIFIED., .F., .F., .F. ) 
 B_SPLINE_SURFACE_WITH_KNOTS ( ( 4, 2, 4 ),
 ( 3, 3 ),
 ( 0.000000000000000000, 0.0003766365702389427796, 0.0007532731404778855592 ),
 ( 0.000000000000000000, 1.000000000000000000 ),
 .UNSPECIFIED. ) 
 GEOMETRIC_REPRESENTATION_ITEM ( )  RATIONAL_B_SPLINE_SURFACE ( (
 ( 1.000000000000000000, 0.7452309222762957264, 1.000000000000000000),
 ( 1.000000000000000000, 0.7451892422671814176, 1.000000000000000000),
 ( 1.000000000000000000, 0.7429606254238495522, 1.000000000000000000),
 ( 1.000000000000000000, 0.7311462761265991039, 1.000000000000000000),
 ( 1.000000000000000000, 0.7212257702791110558, 1.000000000000000000),
 ( 1.000000000000000000, 0.7071067811865475727, 1.000000000000000000) ) ) 
 REPRESENTATION_ITEM ( '' )  SURFACE ( )  );
#17546 = CARTESIAN_POINT ( 'NONE',  ( -1.123270288250339366, 3.283552654332833054, 0.7749999999993804067 ) ) ;
#17547 = CARTESIAN_POINT ( 'NONE',  ( 3.669453130792974971, 7.432779085900453886, 1.040834085586084257E-14 ) ) ;
#17548 = CARTESIAN_POINT ( 'NONE',  ( 0.07516593201273896740, 4.087024598281757015, -2.598925129725014660 ) ) ;
#17549 = CARTESIAN_POINT ( 'NONE',  ( 0.4267348894952603944, -1.354911996285239395, 1.565345633960463889 ) ) ;
#17550 = ORIENTED_EDGE ( 'NONE', *, *, #204483, .T. ) ;
#17551 = CARTESIAN_POINT ( 'NONE',  ( 3.984856247070994506, -1.691632632888851351, -0.6484230535298250997 ) ) ;
#17552 = ORIENTED_EDGE ( 'NONE', *, *, #10791, .F. ) ;
#17553 = CARTESIAN_POINT ( 'NONE',  ( 7.205232291019763480, 7.370802192470005565, -0.7998128361456341429 ) ) ;
#17554 = CARTESIAN_POINT ( 'NONE',  ( 1.664652168048566030E-16, -4.500000000000003553, 1.359291649810836722 ) ) ;
#17555 = CARTESIAN_POINT ( 'NONE',  ( 4.547391301494094762, -1.654308909395687310, 0.7384720232115218330 ) ) ;
#17556 = CARTESIAN_POINT ( 'NONE',  ( 5.343321937117211817, 9.247976336696488886, 0.000000000000000000 ) ) ;
#17557 = FACE_OUTER_BOUND ( 'NONE', #140145, .T. ) ;
#17559 = CARTESIAN_POINT ( 'NONE',  ( 5.298667053604809496, 6.361919491657284986, -1.123377533431538566 ) ) ;
#17558 = B_SPLINE_CURVE_WITH_KNOTS ( 'NONE', 3,
 ( #11514, #94932, #128566, #61344, #212905 ),
 .UNSPECIFIED., .F., .F.,
 ( 4, 1, 4 ),
 ( 0.000000000000000000, 3.079525422856393096E-06, 6.159050845712786192E-06 ),
 .UNSPECIFIED. ) ;
#17561 = CARTESIAN_POINT ( 'NONE',  ( 8.594979316059474073, 12.11489407112305372, 1.199719254218450271 ) ) ;
#17560 = CARTESIAN_POINT ( 'NONE',  ( 6.531710587413017244, 1.780498168465095787, -0.5416703039235416517 ) ) ;
#17562 = CARTESIAN_POINT ( 'NONE',  ( 4.024928501738918030, -1.664925135935046763, 0.9472863605698205181 ) ) ;
#17563 = CARTESIAN_POINT ( 'NONE',  ( 1.500000000000035971, 7.750000000000000000, 10.86128356754324109 ) ) ;
#17564 = CIRCLE ( 'NONE', #57048, 8.049999999999993605 ) ;
#17565 = EDGE_CURVE ( 'NONE', #211004, #54861, #70560, .T. ) ;
#17566 = CARTESIAN_POINT ( 'NONE',  ( 9.499607930503637832, -9.902952869712851935, -0.08630915044579903772 ) ) ;
#17567 = CARTESIAN_POINT ( 'NONE',  ( 11.33772463945037146, 13.39999999999998259, 3.599999999999999201 ) ) ;
#17568 = CARTESIAN_POINT ( 'NONE',  ( 5.829642864196157070, 8.784705193995428374, 1.082531754730558626 ) ) ;
#17570 = CARTESIAN_POINT ( 'NONE',  ( 5.331313699870084299, -1.671001674814942994, -1.300292098898154780 ) ) ;
#17569 = CARTESIAN_POINT ( 'NONE',  ( -10.00555417720528872, 10.77549408293541866, 0.7216878364870438212 ) ) ;
#17571 = CARTESIAN_POINT ( 'NONE',  ( 1.217891636700708435, -2.108894920778502602, 0.4742063263511315796 ) ) ;
#17572 = CARTESIAN_POINT ( 'NONE',  ( -4.423703259808839938, 8.383013913077441259, 0.7998128361456352531 ) ) ;
#17573 = CARTESIAN_POINT ( 'NONE',  ( 5.388439706788500594, 5.251210844200210559, 0.7998128361456352531 ) ) ;
#17574 = CARTESIAN_POINT ( 'NONE',  ( 1.201864610381056853, -1.825762228264395048, -0.004348209057210283834 ) ) ;
#17575 = CARTESIAN_POINT ( 'NONE',  ( -3.602716132929368875, 5.226254793216122074, 1.599625672291267398 ) ) ;
#17576 = CARTESIAN_POINT ( 'NONE',  ( 3.926616521958687045, 1.733384925006593136, 0.5729815612169064654 ) ) ;
#17577 = CARTESIAN_POINT ( 'NONE',  ( -4.183485216215332869, 3.563207579971354289, 2.499999999999998668 ) ) ;
#17578 = CARTESIAN_POINT ( 'NONE',  ( 2.004032382285144021, -0.8144628449315849394, 1.730399521388835460 ) ) ;
#17579 = EDGE_LOOP ( 'NONE', ( #26005, #112210, #5682 ) ) ;
#17580 = CARTESIAN_POINT ( 'NONE',  ( 2.330458462945466547, -1.214122947426389709, 1.550707797581540204 ) ) ;
#17581 = CARTESIAN_POINT ( 'NONE',  ( 4.880387366230515944, -0.2415804104359954019, -1.926931144411721641 ) ) ;
#17582 = CARTESIAN_POINT ( 'NONE',  ( -5.002032328799064231, 4.800402236545811441, -0.7998128361456362523 ) ) ;
#17584 = CARTESIAN_POINT ( 'NONE',  ( 5.361630242575341931, -1.673063676233761621, -1.302930760576012092 ) ) ;
#17583 = CARTESIAN_POINT ( 'NONE',  ( 6.668631453075247073, 8.873432343378178544, -1.599625672291281386 ) ) ;
#17585 = CARTESIAN_POINT ( 'NONE',  ( 0.002323312721274023267, -7.217450603046065893, 9.500350659417536647 ) ) ;
#17586 = CARTESIAN_POINT ( 'NONE',  ( 3.123589223026546957, -0.3706944625661895976, 1.875830702792554483 ) ) ;
#17587 = CARTESIAN_POINT ( 'NONE',  ( 5.756168354352870331, 6.246635012430203027, 1.018728318139457523 ) ) ;
#17588 = CARTESIAN_POINT ( 'NONE',  ( 0.2331563151865486683, 0.2490001740663889407, -1.980811336351681273 ) ) ;
#17589 = CARTESIAN_POINT ( 'NONE',  ( -5.600986303897101948, 14.48156060235217701, 10.62204783317221235 ) ) ;
#17590 = CARTESIAN_POINT ( 'NONE',  ( 3.555981428534177091, 7.370671776590375757, 0.7998128361456271485 ) ) ;
#17591 = CARTESIAN_POINT ( 'NONE',  ( 3.310162060030825248, 7.013606170011280838, -0.7998128361456291469 ) ) ;
#17592 = AXIS2_PLACEMENT_3D ( 'NONE', #58066, #123172, #15694 ) ;
#17593 = CARTESIAN_POINT ( 'NONE',  ( 0.000000000000000000, -9.063431457505059186, 0.000000000000000000 ) ) ;
#17594 = CARTESIAN_POINT ( 'NONE',  ( 5.004447790439923160, -0.6182884515001166870, -1.717943145347331502 ) ) ;
#17595 = CARTESIAN_POINT ( 'NONE',  ( 10.99945475518247129, -9.908704762181759662, -0.1095286008944305889 ) ) ;
#17596 = CARTESIAN_POINT ( 'NONE',  ( -8.026063749610047537, 11.34719622697832264, -1.082531754730543971 ) ) ;
#17597 =( BOUNDED_SURFACE ( )  B_SPLINE_SURFACE ( 3, 2, ( 
 ( #55691, #105538, #171572 ),
 ( #23169, #167319, #18906 ),
 ( #89285, #84990, #151081 ),
 ( #52494, #53561, #134840 ),
 ( #118624, #119694, #9081 ),
 ( #43744, #59963, #142322 ),
 ( #143392, #206202, #157486 ),
 ( #42680, #12267, #176922 ) ),
 .UNSPECIFIED., .F., .F., .T. ) 
 B_SPLINE_SURFACE_WITH_KNOTS ( ( 4, 2, 2, 4 ),
 ( 3, 3 ),
 ( 5.421010862427522170E-20, 0.0004401918256850920631, 0.0006602877385276380946, 0.0008803836513701841261 ),
 ( 0.000000000000000000, 1.000000000000000000 ),
 .UNSPECIFIED. ) 
 GEOMETRIC_REPRESENTATION_ITEM ( )  RATIONAL_B_SPLINE_SURFACE ( (
 ( 1.000000000000000000, 0.6787756258918233865, 1.000000000000000000),
 ( 1.000000000000000000, 0.6284487096100427328, 1.000000000000000000),
 ( 1.000000000000000000, 0.5704014816683798950, 1.000000000000000000),
 ( 1.000000000000000000, 0.4882303283130677296, 1.000000000000000000),
 ( 1.000000000000000000, 0.4617370933884979434, 1.000000000000000000),
 ( 1.000000000000000000, 0.4222438920367950765, 1.000000000000000000),
 ( 1.000000000000000000, 0.4105126989450126884, 1.000000000000000000),
 ( 1.000000000000000000, 0.4127341956164993220, 1.000000000000000000) ) ) 
 REPRESENTATION_ITEM ( '' )  SURFACE ( )  );
#17598 = CARTESIAN_POINT ( 'NONE',  ( -6.617491849531519144, 6.756558277422160863, -0.006230766683231955816 ) ) ;
#17599 = CARTESIAN_POINT ( 'NONE',  ( -5.939880696118548187, 6.102484698325975288, 0.000000000000000000 ) ) ;
#17600 = CARTESIAN_POINT ( 'NONE',  ( 5.875831987524620992, 1.115552982110395330, 1.501486808359139946 ) ) ;
#17601 = CARTESIAN_POINT ( 'NONE',  ( 8.437251666405968464, 8.737881787095446384, 1.040834085586084257E-14 ) ) ;
#17602 = CARTESIAN_POINT ( 'NONE',  ( -4.436542580169821726, 6.199052314996659874, 1.599625672291267175 ) ) ;
#17603 = AXIS2_PLACEMENT_3D ( 'NONE', #196348, #163856, #51161 ) ;
#17604 = CARTESIAN_POINT ( 'NONE',  ( 4.355193658487811703, 6.104145239700998538, -1.599625672291255185 ) ) ;
#17605 = CARTESIAN_POINT ( 'NONE',  ( -1.364683531250014514, 10.15104166700806587, -0.7879004041258335089 ) ) ;
#17606 = CARTESIAN_POINT ( 'NONE',  ( -6.423865854776591000, 6.388931673527803667, 1.040834085586084257E-14 ) ) ;
#17607 = CARTESIAN_POINT ( 'NONE',  ( -3.973948422136970748, 6.690004688251493192, -1.082531754730546636 ) ) ;
#17608 = CARTESIAN_POINT ( 'NONE',  ( -4.042302355168801320, 7.867769847672247074, 0.7998128361456341429 ) ) ;
#17609 = CARTESIAN_POINT ( 'NONE',  ( 6.473493066963706966, -0.2743099562094972743, 2.153646047958713172 ) ) ;
#17610 = CARTESIAN_POINT ( 'NONE',  ( 1.107202915679715405, -0.04781017987004822223, 2.116844178444466706 ) ) ;
#17611 = CARTESIAN_POINT ( 'NONE',  ( 8.052653171512838881, 11.48218023581863001, -1.199719254218446718 ) ) ;
#17612 = CARTESIAN_POINT ( 'NONE',  ( -6.177789192036478916, 5.326704385441258793, 2.499999999999775735 ) ) ;
#17613 = CARTESIAN_POINT ( 'NONE',  ( 5.928598010555855780, -1.317819122799672504, 1.596621505246295314 ) ) ;
#17615 = CARTESIAN_POINT ( 'NONE',  ( 4.513260471453858003, 7.001907027245110271, -1.160773635454902530 ) ) ;
#17614 = CARTESIAN_POINT ( 'NONE',  ( 1.540310226958538475, -1.555040833713853710, 0.9856339240054690087 ) ) ;
#17616 = CARTESIAN_POINT ( 'NONE',  ( 5.450014563013511726, 8.341805509282339770, -1.082531754730543083 ) ) ;
#17618 = FILL_AREA_STYLE ('',( #169228 ) ) ;
#17617 = CARTESIAN_POINT ( 'NONE',  ( 3.475000000000000533, -3.354166666666667851, 2.006292185433948827 ) ) ;
#17619 = CARTESIAN_POINT ( 'NONE',  ( 1.377341666110833529, 2.116387791839238641, -0.8810097948994728423 ) ) ;
#17621 = CARTESIAN_POINT ( 'NONE',  ( -1.387358672536802340, 7.315968950354509559, 4.254625267136455058 ) ) ;
#17620 = DIRECTION ( 'NONE',  ( 1.000000000000000000, 0.000000000000000000, 0.000000000000000000 ) ) ;
#17622 = CARTESIAN_POINT ( 'NONE',  ( 2.461071540317420592, -1.587761714688111780, 1.065645112462119570 ) ) ;
#17623 = ORIENTED_EDGE ( 'NONE', *, *, #138938, .T. ) ;
#17624 = CARTESIAN_POINT ( 'NONE',  ( 6.100805936025112786, 10.06143132543056673, 1.040834085586084257E-14 ) ) ;
#17625 = CARTESIAN_POINT ( 'NONE',  ( 0.07056460990086978191, 0.7743322593966313061, 1.858523817361916963 ) ) ;
#17626 = CARTESIAN_POINT ( 'NONE',  ( 1.481223165768187355, -0.05357505548480785695, 1.961209554040027170 ) ) ;
#17627 = CARTESIAN_POINT ( 'NONE',  ( 3.929058411375439874, -1.000000000000000888, -0.7500000000000006661 ) ) ;
#17629 = FACE_OUTER_BOUND ( 'NONE', #135883, .T. ) ;
#17628 = CARTESIAN_POINT ( 'NONE',  ( -8.311311860377216476, 9.655284244316948872, -1.199719254218446718 ) ) ;
#17631 = CARTESIAN_POINT ( 'NONE',  ( 1.938023551401172773, 1.750023271871611996, 0.2632672158595899536 ) ) ;
#17630 = CARTESIAN_POINT ( 'NONE',  ( 4.048837805470763662, -1.738144455908509078, -1.161405209330027555 ) ) ;
#17632 = CARTESIAN_POINT ( 'NONE',  ( 4.008199524592567897, 7.584238231759597326, 0.2402771892247856922 ) ) ;
#17633 = ADVANCED_FACE ( 'NONE', ( #156126 ), #188606, .T. ) ;
#17635 = CARTESIAN_POINT ( 'NONE',  ( 4.927800006241752406, 1.181458742244513971, -1.964204249851936090 ) ) ;
#17634 = CARTESIAN_POINT ( 'NONE',  ( -11.13976883071979174, 5.784892963039250269, 4.476295437483729600 ) ) ;
#17636 = CARTESIAN_POINT ( 'NONE',  ( 3.222313301838835020, 0.04370593061932443596, 1.739952058630070519 ) ) ;
#17637 = CARTESIAN_POINT ( 'NONE',  ( 3.029357257649615054, 5.621668336311468117, -1.199719254218446718 ) ) ;
#17638 = CARTESIAN_POINT ( 'NONE',  ( 5.737035277238070385, 6.722237907313067140, -1.199719254218452047 ) ) ;
#17639 = CARTESIAN_POINT ( 'NONE',  ( 3.567500862290486019, 1.367785175758473581, -1.065411925293987760 ) ) ;
#17640 = CARTESIAN_POINT ( 'NONE',  ( -6.775324078527193983, 8.927630729746953264, -1.599625672291263179 ) ) ;
#17641 = CARTESIAN_POINT ( 'NONE',  ( 4.088457082891777894, 1.164728776245987918, -1.832164736925721682 ) ) ;
#17642 = CARTESIAN_POINT ( 'NONE',  ( 5.332434488876471868, 5.115595079977664383, 0.7998128361456341429 ) ) ;
#17643 = CARTESIAN_POINT ( 'NONE',  ( 5.454314652423888354, -1.275559214091715354, 1.561879324423600668 ) ) ;
#17644 = CARTESIAN_POINT ( 'NONE',  ( 1.000000000000000666, -5.752119711681284071E-14, -2.052068128417952053 ) ) ;
#17645 = VECTOR ( 'NONE', #125725, 1000.000000000000000 ) ;
#17646 = CARTESIAN_POINT ( 'NONE',  ( 1.499999999999989120, 4.785416667349486453, 0.8660254037844524744 ) ) ;
#17647 = CARTESIAN_POINT ( 'NONE',  ( 2.256748493264736588, -1.490592131378381646, 1.220310119380305203 ) ) ;
#17648 = CARTESIAN_POINT ( 'NONE',  ( -1.364683531250014514, 15.08854166700806587, -0.7879004041258335089 ) ) ;
#17649 = CARTESIAN_POINT ( 'NONE',  ( 5.361676289133297857, -1.751401506552331400, -1.366425036640180446 ) ) ;
#17650 = ORIENTED_EDGE ( 'NONE', *, *, #14127, .T. ) ;
#17652 = STYLED_ITEM ( 'NONE', ( #131077 ), #56893 ) ;
#17651 = CARTESIAN_POINT ( 'NONE',  ( -0.2108831679770959699, 2.036692374882024037, -2.313561348563981657 ) ) ;
#17653 = CARTESIAN_POINT ( 'NONE',  ( -1.500000000000013101, 2.170833333333357373, 0.8660254037844403729 ) ) ;
#17654 = CARTESIAN_POINT ( 'NONE',  ( 6.856673000209174695, 9.022537805042615489, 1.599625672291281386 ) ) ;
#17655 = CARTESIAN_POINT ( 'NONE',  ( 3.484082288587588838, 7.008587070086755411, -0.7216878364870267237 ) ) ;
#17656 = CARTESIAN_POINT ( 'NONE',  ( 3.285556943750000514, -1.363541666188708978, 1.896917185911906722 ) ) ;
#17657 = CARTESIAN_POINT ( 'NONE',  ( 1.875925780897500950, 0.3759573520328520768, -2.189106109952672519 ) ) ;
#17658 = CARTESIAN_POINT ( 'NONE',  ( 6.707479306934847507, -1.574971382793718178, -1.169550641929931079 ) ) ;
#17659 = CARTESIAN_POINT ( 'NONE',  ( 7.429504990608736037, 11.61158022244479682, -0.7216878364870267237 ) ) ;
#17660 = PLANE ( 'NONE',  #194342 ) ;
#17661 = CARTESIAN_POINT ( 'NONE',  ( 4.016958651398847557, 7.908478536599129249, -0.7998128361456362523 ) ) ;
#17662 = CARTESIAN_POINT ( 'NONE',  ( -0.06968618116158857567, -1.560424145883563929, -1.276814929289785239 ) ) ;
#17663 = CARTESIAN_POINT ( 'NONE',  ( 4.035635273026453085, 1.943268055400270811, -0.6920256600186375229 ) ) ;
#17664 = CARTESIAN_POINT ( 'NONE',  ( -5.742041750587549842, 6.657802449562273850, 1.199719254218450271 ) ) ;
#17665 = CARTESIAN_POINT ( 'NONE',  ( 0.7499999999999902300, 4.597916667349482012, -1.299038105676658228 ) ) ;
#17666 = CARTESIAN_POINT ( 'NONE',  ( -1.364683531250014514, 0.03020833367475737191, 0.7879004041258379498 ) ) ;
#17667 = CARTESIAN_POINT ( 'NONE',  ( 6.221928862670094595, -1.039020359566013907, -1.555222851818117924 ) ) ;
#17668 = CARTESIAN_POINT ( 'NONE',  ( 5.027816288645148290, -1.483603310789272323, 0.8976219912088311270 ) ) ;
#17669 = CARTESIAN_POINT ( 'NONE',  ( 4.352889007613729433, 0.3757914745146764823, -1.699215345876355476 ) ) ;
#17670 = CARTESIAN_POINT ( 'NONE',  ( 5.009901455449552010, 5.803638771901306725, -1.199719254218452047 ) ) ;
#17671 = CARTESIAN_POINT ( 'NONE',  ( 1.751946580633024331, 2.285858364093972028, -0.1737669427509143383 ) ) ;
#17672 = CARTESIAN_POINT ( 'NONE',  ( 1.364683531249990311, 5.676041667008088432, 0.7879004041258500513 ) ) ;
#17673 = CARTESIAN_POINT ( 'NONE',  ( 5.530836773642837656, -1.889722758269284375, 0.8948517497979097124 ) ) ;
#17674 = CARTESIAN_POINT ( 'NONE',  ( 0.3922017905241963476, 1.532332584989907653, -1.020347975915262939 ) ) ;
#17675 = CARTESIAN_POINT ( 'NONE',  ( 1.786647480846655257E-05, -9.954793286625724491, 11.00029511060568588 ) ) ;
#17676 = CARTESIAN_POINT ( 'NONE',  ( 1.371720446232262081, -0.2986288616722633793, -1.994071132515719658 ) ) ;
#17677 = CARTESIAN_POINT ( 'NONE',  ( 0.09403522832084068583, -2.191061582759439297, -0.04926842934906834615 ) ) ;
#17678 = CARTESIAN_POINT ( 'NONE',  ( 8.353377556026709172, 13.12787966248234284, -8.539254890958119404 ) ) ;
#17679 = CARTESIAN_POINT ( 'NONE',  ( -6.364663046611467756, 9.512858423433634414, 1.199719254218452047 ) ) ;
#17680 = CARTESIAN_POINT ( 'NONE',  ( 3.655894977179307226, 7.416961240017848844, -0.7998128361456291469 ) ) ;
#17681 = CARTESIAN_POINT ( 'NONE',  ( -1.360316468750040642, 2.161458333674780352, 0.7853790794158861388 ) ) ;
#17682 = CARTESIAN_POINT ( 'NONE',  ( 3.756581929197760683, 2.110411401290826383, 0.2062832702387565331 ) ) ;
#17683 = CARTESIAN_POINT ( 'NONE',  ( 0.6823417656249882723, -0.4072916663252490466, 1.181850606188755259 ) ) ;
#17684 = CARTESIAN_POINT ( 'NONE',  ( 5.637271085457097541, -1.648663388651723460, 0.7845467231081537651 ) ) ;
#17685 = ORIENTED_EDGE ( 'NONE', *, *, #82075, .F. ) ;
#17686 = CARTESIAN_POINT ( 'NONE',  ( -6.607619761813764647, 8.802252036906432764, 1.599625672291269396 ) ) ;
#17687 = CARTESIAN_POINT ( 'NONE',  ( 2.272459710430874580, 5.681424495331688362, -0.3682267578792697282 ) ) ;
#17688 = CARTESIAN_POINT ( 'NONE',  ( -3.475000000000000533, -3.135416665710750284, -2.006292185433948827 ) ) ;
#17689 = CARTESIAN_POINT ( 'NONE',  ( -6.663996196316808174, 7.733415969579778171, -1.199719254218446718 ) ) ;
#17690 = CARTESIAN_POINT ( 'NONE',  ( 3.533467377359212680, -0.1442520194480846618, 2.014668725452229303 ) ) ;
#17691 = CARTESIAN_POINT ( 'NONE',  ( 0.1652458694026041341, -1.881425287724652673, -0.9463707761560661291 ) ) ;
#17692 = CARTESIAN_POINT ( 'NONE',  ( 10.05353459973327368, 11.68787744023238417, -1.199719254218440723 ) ) ;
#17693 = CARTESIAN_POINT ( 'NONE',  ( 3.643253357272932647, 1.684219189441754416, -0.7917782423425399063 ) ) ;
#17694 = CARTESIAN_POINT ( 'NONE',  ( 9.053093885623066939, 11.58502883802551153, -1.599625672291262513 ) ) ;
#17695 = CARTESIAN_POINT ( 'NONE',  ( 2.373851744317274193, 1.000000000000000888, -11.76285798163019969 ) ) ;
#17696 = CARTESIAN_POINT ( 'NONE',  ( -2.266184231778562541, 5.795632037050281404, 1.040834085586084257E-14 ) ) ;
#17697 = CARTESIAN_POINT ( 'NONE',  ( -7.212047647465563038, 10.50147379109678880, -1.199719254218446718 ) ) ;
#17698 = CARTESIAN_POINT ( 'NONE',  ( 0.3214396764580421118, -0.1044536432763705502, 2.159311484102262479 ) ) ;
#17700 = CARTESIAN_POINT ( 'NONE',  ( -4.670247306389155639, 7.079074041166477649, 1.395957953274113983 ) ) ;
#17699 = CARTESIAN_POINT ( 'NONE',  ( -7.598418745816086783, 7.829519723065708092, 0.000000000000000000 ) ) ;
#17701 = CARTESIAN_POINT ( 'NONE',  ( -1.402160292154681736E-14, -0.9281249996585830830, 1.575800808251672791 ) ) ;
#17702 = CARTESIAN_POINT ( 'NONE',  ( 1.159081676615776990, -0.4145447896758222561, -1.683414020171439818 ) ) ;
#17703 = CARTESIAN_POINT ( 'NONE',  ( 1.552286559517775499, -1.491368903747305019, -0.8966978864634599367 ) ) ;
#17705 = CARTESIAN_POINT ( 'NONE',  ( 8.026063749610047537, 10.38682701267698150, -1.443375672974057666 ) ) ;
#17704 = CARTESIAN_POINT ( 'NONE',  ( 6.621674845842873580, -2.240319515690874397, 0.5532079777821105049 ) ) ;
#17706 = CARTESIAN_POINT ( 'NONE',  ( -10.57232049882948388, 5.599334429189661400, -4.968988939937085014 ) ) ;
#17707 = CARTESIAN_POINT ( 'NONE',  ( 1.932957488262206480, 0.1987776095667900533, 2.051143708757536821 ) ) ;
#17708 = CARTESIAN_POINT ( 'NONE',  ( 0.2278875137335881207, -1.799627942332830965, -0.9090566646320766830 ) ) ;
#17709 = CARTESIAN_POINT ( 'NONE',  ( 0.003079562121058774214, 7.078201604703558303, -2.121336893758704711 ) ) ;
#17710 = CARTESIAN_POINT ( 'NONE',  ( -5.906512197408906317, 6.919960980845699439, -1.199719254218453823 ) ) ;
#17711 = VECTOR ( 'NONE', #30583, 1000.000000000000000 ) ;
#17712 = CARTESIAN_POINT ( 'NONE',  ( 6.315307248462690204, -0.2269180964024133385, 1.856785020699961875 ) ) ;
#17714 = CARTESIAN_POINT ( 'NONE',  ( -7.431277594066160397, 7.842447745931541370, -0.7216878364870338292 ) ) ;
#17713 = CARTESIAN_POINT ( 'NONE',  ( 4.693567934957057375, 1.782326746607498791, -0.6936623114904352239 ) ) ;
#17715 = CARTESIAN_POINT ( 'NONE',  ( 6.340462157465731607, 2.182225300935904055, 0.3281612982340698093 ) ) ;
#17716 = CARTESIAN_POINT ( 'NONE',  ( -6.577113915960828727, 9.727031097712693253, -1.082531754730549967 ) ) ;
#17717 = CARTESIAN_POINT ( 'NONE',  ( 3.973948422136968084, 5.729635473950147606, -1.443375672974068769 ) ) ;
#17718 = CARTESIAN_POINT ( 'NONE',  ( -4.787437638956939523, 5.718337012605431369, -1.082531754730549967 ) ) ;
#17719 = CARTESIAN_POINT ( 'NONE',  ( 6.463548717370299457, -1.702720583769131490, -1.263627255760652046 ) ) ;
#17720 = VERTEX_POINT ( 'NONE', #169158 ) ;
#17721 = CARTESIAN_POINT ( 'NONE',  ( 3.979734726549417623, 2.174020839304124042, -0.7740601867209749853 ) ) ;
#17722 = CARTESIAN_POINT ( 'NONE',  ( 4.387127823891323608, 0.09410986116351567621, 1.959716250186482434 ) ) ;
#17723 = CARTESIAN_POINT ( 'NONE',  ( 2.219515905360454067, 0.3404028402014187549, -1.931851785523025944 ) ) ;
#17724 = CARTESIAN_POINT ( 'NONE',  ( 10.08456733046637765, 10.65975006183261087, 0.000000000000000000 ) ) ;
#17725 = CARTESIAN_POINT ( 'NONE',  ( 6.729185404178087637, -6.864242587301018439, 6.701130199342134830 ) ) ;
#17726 = ORIENTED_EDGE ( 'NONE', *, *, #99278, .F. ) ;
#17727 = CARTESIAN_POINT ( 'NONE',  ( 0.6380961361360514283, 2.114605634092497688, -0.1105060169243020224 ) ) ;
#17728 = CARTESIAN_POINT ( 'NONE',  ( -5.708146366553361162, 6.618257834855742594, -1.199719254218446718 ) ) ;
#17729 = CARTESIAN_POINT ( 'NONE',  ( 0.1285073612291263989, -1.684675954457705682, 0.7431698939026829542 ) ) ;
#17730 = CARTESIAN_POINT ( 'NONE',  ( 4.733362013637422372, 0.006437197247223526778, -2.171239809022653677 ) ) ;
#17731 = CARTESIAN_POINT ( 'NONE',  ( -0.2349500406733201208, 2.568208434401662021, 1.989585655505116568 ) ) ;
#17732 = CARTESIAN_POINT ( 'NONE',  ( 2.004293344102888508, -0.9022931611136343344, 1.919180038594799687 ) ) ;
#17733 = CARTESIAN_POINT ( 'NONE',  ( -0.7499999999999972244, 3.639583334016149863, -1.299038105676652011 ) ) ;
#17734 = CARTESIAN_POINT ( 'NONE',  ( 8.530051201292206287, 13.10347683481629488, 0.000000000000000000 ) ) ;
#17735 = CARTESIAN_POINT ( 'NONE',  ( 11.89942855770814312, 11.29999999999999893, -0.7000000000000009548 ) ) ;
#17736 = CARTESIAN_POINT ( 'NONE',  ( 6.212391540903618115, 7.031971956796816414, -1.022972206104319826 ) ) ;
#17737 = CARTESIAN_POINT ( 'NONE',  ( 2.108734400483037952, 1.529077776457531401, -1.381789073784354560 ) ) ;
#17738 = AXIS2_PLACEMENT_3D ( 'NONE', #106614, #187797, #189939 ) ;
#17740 = CARTESIAN_POINT ( 'NONE',  ( 6.509000000000010999, 0.004788705324892603143, 2.000274819378269786 ) ) ;
#17739 = CARTESIAN_POINT ( 'NONE',  ( -7.167456763118792651, 11.51378332361394818, 0.000000000000000000 ) ) ;
#17741 = CARTESIAN_POINT ( 'NONE',  ( 1.364683531249986537, 2.405208333674752286, -0.7879004041258239610 ) ) ;
#17742 = CARTESIAN_POINT ( 'NONE',  ( 0.07735805125223117751, 5.721077998510399887, -2.682987299736539377 ) ) ;
#17743 = CARTESIAN_POINT ( 'NONE',  ( 10.59781858645781405, 11.29999999999997762, 3.302687032930892830 ) ) ;
#17744 = VERTEX_POINT ( 'NONE', #137748 ) ;
#17745 = CARTESIAN_POINT ( 'NONE',  ( 4.213462193461685601, 1.537813053725526569, 1.136448645172025262 ) ) ;
#17746 = CARTESIAN_POINT ( 'NONE',  ( -1.737500000000000266, -1.108333333333332726, -3.009438278150923907 ) ) ;
#17747 = CARTESIAN_POINT ( 'NONE',  ( 1.142281600899584193, 0.9165754381605104584, -2.068608644781688710 ) ) ;
#17748 = CARTESIAN_POINT ( 'NONE',  ( -2.656508033273816238, 5.186677574539687363, -1.199719254218446718 ) ) ;
#17749 = CARTESIAN_POINT ( 'NONE',  ( 0.7909136568654427935, -0.04542554662571558072, -1.811195533156365611 ) ) ;
#17750 = EDGE_CURVE ( 'NONE', #147564, #48301, #172628, .T. ) ;
#17751 = CARTESIAN_POINT ( 'NONE',  ( 2.202218669689899322, 1.248139960717888908, -1.453441320886917243 ) ) ;
#17752 = CARTESIAN_POINT ( 'NONE',  ( 3.613788337741298040, 0.5058112091442801272, -2.007490274132675445 ) ) ;
#17753 = CARTESIAN_POINT ( 'NONE',  ( -1.201851678989727383E-14, 0.8843750003414173610, 1.575800808251672791 ) ) ;
#17754 = AXIS2_PLACEMENT_3D ( 'NONE', #134311, #187281, #38907 ) ;
#17755 = CARTESIAN_POINT ( 'NONE',  ( 0.5847652604651293329, -0.2391135408384200411, -1.956842742423828829 ) ) ;
#17756 = CARTESIAN_POINT ( 'NONE',  ( 5.215425455482871619, -0.2808245750387359796, 1.905809792320038998 ) ) ;
#17758 = CARTESIAN_POINT ( 'NONE',  ( 6.272547281004660746, 6.891683285556123195, -0.7655605874731727933 ) ) ;
#17757 = CARTESIAN_POINT ( 'NONE',  ( 0.4875218067809834466, -0.2886260216827610803, -2.289518885299694606 ) ) ;
#17759 = EDGE_CURVE ( 'NONE', #130236, #56668, #75055, .T. ) ;
#17760 = CARTESIAN_POINT ( 'NONE',  ( 1.364683531249986537, 1.905208333674750287, -0.7879004041258239610 ) ) ;
#17761 = CARTESIAN_POINT ( 'NONE',  ( 5.090308526370699305, 1.063348096890677441, -1.767349029039886110 ) ) ;
#17762 = CARTESIAN_POINT ( 'NONE',  ( -5.052384799386910430, 9.046199365926717917, 1.214306433183764966E-14 ) ) ;
#17763 = CARTESIAN_POINT ( 'NONE',  ( 9.088043039861931405, 9.497138389460751284, 1.040834085586084257E-14 ) ) ;
#17764 = CARTESIAN_POINT ( 'NONE',  ( 5.203632029546647608, 4.965325544092860532, 1.040834085586084257E-14 ) ) ;
#17766 = CARTESIAN_POINT ( 'NONE',  ( -1.201851678989727383E-14, 3.587500000000020339, -1.732050807568863648 ) ) ;
#17765 = CARTESIAN_POINT ( 'NONE',  ( 5.473694172853372564, 2.030421858957079273, -0.5587401243299906506 ) ) ;
#17767 = CARTESIAN_POINT ( 'NONE',  ( 0.8366658991775147713, -1.206067806592339142, 1.805196218089277549 ) ) ;
#17768 = CARTESIAN_POINT ( 'NONE',  ( -1.364683531250000748, 2.321875000341422357, 1.214306433183764966E-14 ) ) ;
#17769 = CARTESIAN_POINT ( 'NONE',  ( 5.061884429210019576, 2.138887713127162638, -0.3115965683029159883 ) ) ;
#17770 = CARTESIAN_POINT ( 'NONE',  ( 5.742833863956755103, 1.946992082993486584, 0.5367204025522700483 ) ) ;
#17771 = CYLINDRICAL_SURFACE ( 'NONE', #108194, 0.4000000000000001332 ) ;
#17772 = EDGE_CURVE ( 'NONE', #97632, #77820, #13107, .T. ) ;
#17775 = CARTESIAN_POINT ( 'NONE',  ( 4.528060117284222308, 8.226561203566173930, 0.7216878364870438212 ) ) ;
#17774 = CARTESIAN_POINT ( 'NONE',  ( 3.285556943750000514, -1.363541666188709423, 1.896917185911906500 ) ) ;
#17773 = CARTESIAN_POINT ( 'NONE',  ( -5.973258884348944697, 14.55272284716803455, -10.36629430815492903 ) ) ;
#17776 = CARTESIAN_POINT ( 'NONE',  ( -5.926849427829407269, 6.943687749669614995, -1.199719254218453823 ) ) ;
#17777 = CARTESIAN_POINT ( 'NONE',  ( 3.081267818761534549, 1.592661989535900657, 1.236799713577160231 ) ) ;
#17778 = CARTESIAN_POINT ( 'NONE',  ( -7.181014916732457287, 11.52960116949655678, -0.7998128361456291469 ) ) ;
#17780 = LINE ( 'NONE', #31942, #77910 ) ;
#17779 = CARTESIAN_POINT ( 'NONE',  ( -2.252626078164912560, 5.779814191167667481, 0.7998128361456341429 ) ) ;
#17781 = CARTESIAN_POINT ( 'NONE',  ( -1.364683531250010295, 3.780208333674750953, 0.7879004041258379498 ) ) ;
#17783 = CARTESIAN_POINT ( 'NONE',  ( -1.364683531250000748, 8.359375000341396245, 0.000000000000000000 ) ) ;
#17782 = CARTESIAN_POINT ( 'NONE',  ( 4.786082296487640164, -1.021991182799499409, 1.904868704497929333 ) ) ;
#17784 = FILL_AREA_STYLE_COLOUR ( '', #197141 ) ;
#17785 = CARTESIAN_POINT ( 'NONE',  ( 1.854049621773927514, 4.999999999999997335, 0.7500000000000006661 ) ) ;
#17787 = CARTESIAN_POINT ( 'NONE',  ( 5.870720304489429608, -0.2986452421533461465, -1.994069804803912049 ) ) ;
#17786 = CARTESIAN_POINT ( 'NONE',  ( -8.310784975052689205, 8.798263347090697906, -0.7216878364870267237 ) ) ;
#17788 = CARTESIAN_POINT ( 'NONE',  ( -0.7500000000000215383, 5.691666666666685082, 1.299038105676671107 ) ) ;
#17789 = CARTESIAN_POINT ( 'NONE',  ( 0.2051046121598932848, -0.4657588872633237065, 1.660747436093058083 ) ) ;
#17790 = CARTESIAN_POINT ( 'NONE',  ( 5.032011289327418702, 5.899709921417326974, 1.199719254218452935 ) ) ;
#17792 = CARTESIAN_POINT ( 'NONE',  ( 7.503511670520385479, 7.718794801887437274, 0.7998128361456281477 ) ) ;
#17791 = CARTESIAN_POINT ( 'NONE',  ( 8.026063749610047537, 10.38682701267698150, -1.443375672974057666 ) ) ;
#17793 = CARTESIAN_POINT ( 'NONE',  ( -11.86239285000045918, 13.87999999999998302, 1.812080536912751061 ) ) ;
#17794 = CARTESIAN_POINT ( 'NONE',  ( 6.046149701670225696, 1.868418987705861234, 0.09211505606019491921 ) ) ;
#17795 = CARTESIAN_POINT ( 'NONE',  ( -0.005209864377695229073, -1.953240142932886725, -0.4869125064202137199 ) ) ;
#17796 = CARTESIAN_POINT ( 'NONE',  ( 6.539320575229257138, 4.699150603835311912, 2.459441311396874497 ) ) ;
#17797 = AXIS2_PLACEMENT_3D ( 'NONE', #148285, #17179, #33449 ) ;
#17798 = B_SPLINE_CURVE_WITH_KNOTS ( 'NONE', 3,
 ( #202185, #87413, #102590, #20252 ),
 .UNSPECIFIED., .F., .F.,
 ( 4, 4 ),
 ( 8.516827915682558025E-05, 0.0002597075693988114926 ),
 .UNSPECIFIED. ) ;
#17799 = CARTESIAN_POINT ( 'NONE',  ( -5.424670858799220063, 9.342883411992149334, 0.000000000000000000 ) ) ;
#17800 = ORIENTED_EDGE ( 'NONE', *, *, #171627, .T. ) ;
#17802 = CARTESIAN_POINT ( 'NONE',  ( 8.392133896734652154, 12.73464727959172293, 0.7216878364870438212 ) ) ;
#17801 = CIRCLE ( 'NONE', #104275, 6.961139734775127152 ) ;
#17805 = EDGE_CURVE ( 'NONE', #80335, #137341, #82775, .T. ) ;
#17804 = CARTESIAN_POINT ( 'NONE',  ( 1.317982704262925298, 0.9913799330133238330, -1.755781447868165035 ) ) ;
#17803 = CARTESIAN_POINT ( 'NONE',  ( 1.787894333202539654, 2.028250040683087008, -0.6185522307536188702 ) ) ;
#17806 = CARTESIAN_POINT ( 'NONE',  ( 2.232397805642115873, 1.180933449141470026, -1.373882015996011452 ) ) ;
#17807 = CARTESIAN_POINT ( 'NONE',  ( 7.038618024149998043, 8.240751112043669835, -1.199719254218452047 ) ) ;
#17808 = CARTESIAN_POINT ( 'NONE',  ( 6.016527291255574283, 1.455332790597754000, -1.598591904487467463 ) ) ;
#17809 = CARTESIAN_POINT ( 'NONE',  ( 6.775324078527185989, 8.927630729746953264, -1.599625672291262513 ) ) ;
#17811 = CARTESIAN_POINT ( 'NONE',  ( 0.09280537598354164641, 1.668161973260675834, 0.9417010505823987243 ) ) ;
#17810 = CARTESIAN_POINT ( 'NONE',  ( -5.311043488251275591, 7.219303374425030562, -1.599625672291256295 ) ) ;
#17812 = DIRECTION ( 'NONE',  ( 0.6507913734559640506, -0.7592566023653004592, 0.000000000000000000 ) ) ;
#17813 = CARTESIAN_POINT ( 'NONE',  ( 5.246642258364164313, 8.104537820524768676, -1.082531754730549078 ) ) ;
#17814 = EDGE_CURVE ( 'NONE', #67975, #189420, #118890, .T. ) ;
#17815 = B_SPLINE_CURVE_WITH_KNOTS ( 'NONE', 3,
 ( #71482, #41165, #25946, #158109, #203611, #106196 ),
 .UNSPECIFIED., .F., .F.,
 ( 4, 2, 4 ),
 ( 0.000000000000000000, 0.0003144386176887254184, 0.0006288772353774508368 ),
 .UNSPECIFIED. ) ;
#17816 = CARTESIAN_POINT ( 'NONE',  ( 1.364683531249986537, 0.6760416670080884316, 0.7879004041258500513 ) ) ;
#17817 = CARTESIAN_POINT ( 'NONE',  ( 3.307826292054301121, 4.882216645528547616, -1.443375672974057666 ) ) ;
#17818 = CARTESIAN_POINT ( 'NONE',  ( -8.136864746495904299, 12.64475930422059768, -0.7998128361456281477 ) ) ;
#17819 = CARTESIAN_POINT ( 'NONE',  ( 3.959979445722985325, 2.145676688911036578, -0.2621329562078680842 ) ) ;
#17820 = EDGE_CURVE ( 'NONE', #31261, #73128, #51875, .T. ) ;
#17821 = CARTESIAN_POINT ( 'NONE',  ( -7.119440060951841787, 7.478637290631501067, 0.000000000000000000 ) ) ;
#17822 = CARTESIAN_POINT ( 'NONE',  ( 5.885648082108199119, 6.999582529615296700, 1.082531754730549967 ) ) ;
#17823 = CARTESIAN_POINT ( 'NONE',  ( 2.197662576721173266, 1.936918166296027977, -0.8637449004969056654 ) ) ;
#17824 = CARTESIAN_POINT ( 'NONE',  ( 6.686557121163758666, -1.791048715316777562, -0.3524728914669760793 ) ) ;
#17825 = CARTESIAN_POINT ( 'NONE',  ( 2.811746400649973499, -1.950408978035414354, 0.2857507918755904930 ) ) ;
#17826 = CARTESIAN_POINT ( 'NONE',  ( 5.695548698317931091, 1.764485844685494742, -0.7379451211212140205 ) ) ;
#17827 = ORIENTED_EDGE ( 'NONE', *, *, #2718, .F. ) ;
#17828 = CARTESIAN_POINT ( 'NONE',  ( 9.586610838029429260, -7.161464053357567749, -0.003376046620571135446 ) ) ;
#17829 = CARTESIAN_POINT ( 'NONE',  ( 5.547300264688804994, 1.737891114709901208, -0.9267001309954668864 ) ) ;
#17830 = CARTESIAN_POINT ( 'NONE',  ( 1.025216207372595223, -1.231406509999972254, -1.501593997598904995 ) ) ;
#17831 = ORIENTED_EDGE ( 'NONE', *, *, #194419, .F. ) ;
#17832 = CARTESIAN_POINT ( 'NONE',  ( -3.122120512896910505, 6.864500708346841229, 0.7998128361456352531 ) ) ;
#17834 = CARTESIAN_POINT ( 'NONE',  ( 5.854088466050551887, 10.05179665369283981, 0.7998128361456341429 ) ) ;
#17833 = CARTESIAN_POINT ( 'NONE',  ( -5.614485009834902840, 9.564333254867113610, 0.7216878364870267237 ) ) ;
#17835 = CARTESIAN_POINT ( 'NONE',  ( 5.621827251160867789, 9.710548892996357040, 1.040834085586084257E-14 ) ) ;
#17837 = CARTESIAN_POINT ( 'NONE',  ( 5.573810548549551491, 6.635772073796838200, -1.082531754730548412 ) ) ;
#17836 = CARTESIAN_POINT ( 'NONE',  ( 7.644099680006512187, 7.812537802962739697, 1.040834085586084257E-14 ) ) ;
#17839 = ORIENTED_EDGE ( 'NONE', *, *, #9224, .F. ) ;
#17838 = CARTESIAN_POINT ( 'NONE',  ( 5.742805640131908973, 1.844151595126357179, 0.5056804652876015771 ) ) ;
#17840 = CARTESIAN_POINT ( 'NONE',  ( 2.754729969050898841, 0.7443088323898851000, 2.077706851784946185 ) ) ;
#17841 = CARTESIAN_POINT ( 'NONE',  ( 1.993488836774780060, 1.919990754028239488, -1.087721427556323617 ) ) ;
#17842 = CARTESIAN_POINT ( 'NONE',  ( 0.3999999999999825362, 3.248764396332278981, -0.4641653677813217804 ) ) ;
#17843 = CARTESIAN_POINT ( 'NONE',  ( 0.6449871831117168774, 0.1410837285014763798, 1.907147727228817757 ) ) ;
#17844 = CARTESIAN_POINT ( 'NONE',  ( -0.08011318657386623521, 15.51804218995383167, 11.99973258272403775 ) ) ;
#17845 = CARTESIAN_POINT ( 'NONE',  ( 11.48243876534946217, 13.79999999999999893, -3.200000000000001510 ) ) ;
#17846 = CARTESIAN_POINT ( 'NONE',  ( 3.596198176508007105, 0.9334358170956689182, -1.848091447891623051 ) ) ;
#17847 = CARTESIAN_POINT ( 'NONE',  ( -5.762378981008047241, 6.681529218386182301, 1.199719254218450271 ) ) ;
#17848 = CARTESIAN_POINT ( 'NONE',  ( -6.423141557142870717, 6.808251908967412724, 0.4733936187572094223 ) ) ;
#17850 = CARTESIAN_POINT ( 'NONE',  ( 1.727627455807039691, -2.035446057602477321, 0.7283451284763039490 ) ) ;
#17849 = CARTESIAN_POINT ( 'NONE',  ( -2.578021764892882040, 6.159442492350315490, 0.7998128361456341429 ) ) ;
#17851 = CARTESIAN_POINT ( 'NONE',  ( 3.439196427729715566, -1.660734982795486481, -1.430121640581414111 ) ) ;
#17852 = CARTESIAN_POINT ( 'NONE',  ( 0.000000000000000000, 3.480000000000000426, -2.000000000000000000 ) ) ;
#17853 = FACE_OUTER_BOUND ( 'NONE', #68438, .T. ) ;
#17854 = CARTESIAN_POINT ( 'NONE',  ( 0.3728355200474325337, -6.583727468838304731, 9.609247538823966650 ) ) ;
#17855 = CARTESIAN_POINT ( 'NONE',  ( -0.6823417656250039265, 14.88020833367473195, -1.181850606188755259 ) ) ;
#17856 = CARTESIAN_POINT ( 'NONE',  ( -4.685224601974262271, 7.623789914682047808, -1.199719254218453823 ) ) ;
#17857 = UNCERTAINTY_MEASURE_WITH_UNIT (LENGTH_MEASURE( 1.000000000000000082E-05 ), #202827, 'distance_accuracy_value', 'NONE');
#17858 = CARTESIAN_POINT ( 'NONE',  ( 6.504571816962987363, -1.679391772619584833, 0.4319377402999846627 ) ) ;
#17859 = CIRCLE ( 'NONE', #76645, 0.08000000000000020983 ) ;
#17860 = CARTESIAN_POINT ( 'NONE',  ( -9.490344339885973923, 12.09515436799890331, -1.443375672974059665 ) ) ;
#17861 = CARTESIAN_POINT ( 'NONE',  ( 3.221598570378156001, 0.3083542414583049784, -2.047064864394084971 ) ) ;
#17862 = CARTESIAN_POINT ( 'NONE',  ( 5.870749427052773584, -0.3112397890362226249, -2.094129459642315005 ) ) ;
#17863 = CARTESIAN_POINT ( 'NONE',  ( 5.449487677688982679, 8.445153826357429949, -1.199719254218446718 ) ) ;
#17864 = CARTESIAN_POINT ( 'NONE',  ( -1.364683531249997417, 5.009375000341425022, 1.214306433183764966E-14 ) ) ;
#17865 = CARTESIAN_POINT ( 'NONE',  ( 3.256658344530354299, -0.5673638227334516504, -1.885978461452636479 ) ) ;
#17866 = CARTESIAN_POINT ( 'NONE',  ( 1.336036003918249948, -1.064896177285217016, -1.588262137521757822 ) ) ;
#17867 = CARTESIAN_POINT ( 'NONE',  ( 6.439416457043729558, 0.8834936782941483768, -2.115358923741214259 ) ) ;
#17868 = CARTESIAN_POINT ( 'NONE',  ( 2.894927146036041510, 1.565677646668685696, -0.9388022922067614795 ) ) ;
#17869 = CARTESIAN_POINT ( 'NONE',  ( 3.054329744828568227, 6.785411478933790264, 0.000000000000000000 ) ) ;
#17870 = CARTESIAN_POINT ( 'NONE',  ( 3.972175818679561043, 7.578029521860726092, -0.7216878364870197293 ) ) ;
#17871 = CARTESIAN_POINT ( 'NONE',  ( -5.994676475536691029, 10.14553965476814845, 0.7998128361456481317 ) ) ;
#17872 = VERTEX_POINT ( 'NONE', #167721 ) ;
#17873 = ORIENTED_EDGE ( 'NONE', *, *, #6374, .F. ) ;
#17874 = CARTESIAN_POINT ( 'NONE',  ( 3.568611400213494989, 0.7284950617309441379, 1.876934371664749301 ) ) ;
#17875 = CARTESIAN_POINT ( 'NONE',  ( 4.135565103414404753, 1.848670044762780407, -0.6568835154602686854 ) ) ;
#17876 = CARTESIAN_POINT ( 'NONE',  ( -6.509886312855995172, 10.74661779830734254, -0.7998128361456291469 ) ) ;
#17877 = EDGE_CURVE ( 'NONE', #194213, #170139, #3054, .T. ) ;
#17878 = CARTESIAN_POINT ( 'NONE',  ( -5.117312914154178216, 8.057616602233474978, -1.199719254218452047 ) ) ;
#17880 = CARTESIAN_POINT ( 'NONE',  ( 5.805463146582474643, -0.4265672176911333713, 1.717519531449087866 ) ) ;
#17879 = CARTESIAN_POINT ( 'NONE',  ( 0.4157161284131759005, -1.121801286243618190, -1.764121917367883263 ) ) ;
#17881 = CARTESIAN_POINT ( 'NONE',  ( 11.00020965659335204, -5.765528217051488546, 0.01167607004708704974 ) ) ;
#17882 = CARTESIAN_POINT ( 'NONE',  ( 2.308753661914957345, 1.958203289975643191, 0.9839491227633669901 ) ) ;
#17883 = CARTESIAN_POINT ( 'NONE',  ( 6.562468561866369399, -1.594522334811569131, -0.6977961348336658709 ) ) ;
#17884 = AXIS2_PLACEMENT_3D ( 'NONE', #96585, #77096, #30504 ) ;
#17885 = CARTESIAN_POINT ( 'NONE',  ( 6.089583550832340819, 10.25626457594641749, 1.040834085586084257E-14 ) ) ;
#17886 = CARTESIAN_POINT ( 'NONE',  ( -15.75000000000000000, 10.90000000000000036, -1.100000000000002087 ) ) ;
#17887 = CARTESIAN_POINT ( 'NONE',  ( 0.5215560022201523038, -0.9183498723843477318, -1.459886522650925000 ) ) ;
#17888 = CARTESIAN_POINT ( 'NONE',  ( 1.019433853822170777, 2.295598214472119203, -0.1149376033552674814 ) ) ;
#17889 = CARTESIAN_POINT ( 'NONE',  ( 0.8201894534925309177, 1.301127354658284663, -1.763390660798454634 ) ) ;
#17890 = CARTESIAN_POINT ( 'NONE',  ( 3.369938178094655346, 2.153121441420174698, -0.4834393813165636100 ) ) ;
#17891 = CARTESIAN_POINT ( 'NONE',  ( 0.7257146478014552260, 0.2145687282662836204, -2.160472036209131197 ) ) ;
#17892 = PLANE ( 'NONE',  #138005 ) ;
#17893 = CARTESIAN_POINT ( 'NONE',  ( 2.817688460867060485, -1.425471633543059724, -1.565750481055405263 ) ) ;
#17894 = CARTESIAN_POINT ( 'NONE',  ( 6.620655732516651071, 1.241313378043694238, 2.288056600130850882 ) ) ;
#17895 = CARTESIAN_POINT ( 'NONE',  ( 5.403319659429405952, 1.574929826682970990, 1.109050863186450853 ) ) ;
#17896 = VERTEX_POINT ( 'NONE', #168782 ) ;
#17898 = CARTESIAN_POINT ( 'NONE',  ( 0.7499999999999902300, 5.566666666666685082, -1.299038105676658228 ) ) ;
#17897 = CARTESIAN_POINT ( 'NONE',  ( 2.085838899777220590, -0.9763249575661275825, 2.074189754910108263 ) ) ;
#17899 = CARTESIAN_POINT ( 'NONE',  ( 3.225950485047770933, 5.851027101609320269, 1.199719254218450271 ) ) ;
#17900 = CARTESIAN_POINT ( 'NONE',  ( 5.192936529234042808, 6.017179691316550283, -1.199719254218452047 ) ) ;
#17901 = MECHANICAL_DESIGN_GEOMETRIC_PRESENTATION_REPRESENTATION (  '', ( #52108 ), #45637 ) ;
#17902 = CARTESIAN_POINT ( 'NONE',  ( 4.617978872065289231, -0.5927926152728602016, 2.140694073679518805 ) ) ;
#17903 = CARTESIAN_POINT ( 'NONE',  ( -8.378575743565381373, 8.877352577022161739, 0.7216878364870438212 ) ) ;
#17904 = CARTESIAN_POINT ( 'NONE',  ( 0.4382560683119269829, -7.666862915010147717, -10.99126615174920296 ) ) ;
#17905 = CARTESIAN_POINT ( 'NONE',  ( 5.666945020832177882, 6.674152614801420746, 1.082531754730558626 ) ) ;
#17906 = CARTESIAN_POINT ( 'NONE',  ( -8.975134502122321223, 9.573337795338607847, 1.040834085586084257E-14 ) ) ;
#17907 = CARTESIAN_POINT ( 'NONE',  ( 4.692530564105613422, 7.528350520548263702, -1.082531754730548412 ) ) ;
#17908 = ORIENTED_EDGE ( 'NONE', *, *, #48845, .T. ) ;
#17909 = CARTESIAN_POINT ( 'NONE',  ( 3.305314717767214638, 1.277042846462652204, -1.560500556308255238 ) ) ;
#17911 = CARTESIAN_POINT ( 'NONE',  ( 0.5849265108320426121, 1.972682758258193392, 0.6021488627185996867 ) ) ;
#17910 = CARTESIAN_POINT ( 'NONE',  ( 6.612626235163189925, 8.737816579155630592, -1.599625672291262513 ) ) ;
#17912 = FACE_OUTER_BOUND ( 'NONE', #99877, .T. ) ;
#17913 = CARTESIAN_POINT ( 'NONE',  ( 6.360183458142179447, 6.592837920686898556, -0.7216878364870458196 ) ) ;
#17914 = DIRECTION ( 'NONE',  ( -6.938893903907222067E-15, -1.000000000000000000, 0.000000000000000000 ) ) ;
#17915 = CARTESIAN_POINT ( 'NONE',  ( -1.364683531249997417, 3.759375000341423689, 1.214306433183764966E-14 ) ) ;
#17916 = CARTESIAN_POINT ( 'NONE',  ( 3.591891977137162684, -2.188917585555647527, -0.1077332384093188100 ) ) ;
#17917 = CARTESIAN_POINT ( 'NONE',  ( 1.389296306420295224, -0.7283806465635984662, -1.880434191983325398 ) ) ;
#17918 = CARTESIAN_POINT ( 'NONE',  ( 1.276629239279066574, 1.701104413791530767, -0.7050613402737049284 ) ) ;
#17919 = CARTESIAN_POINT ( 'NONE',  ( 4.950848118218736715, -1.935628577297190400, -1.227853487085520001 ) ) ;
#17920 = CARTESIAN_POINT ( 'NONE',  ( 4.611176429654996412, -1.805050139478355353, 0.3618648703537508671 ) ) ;
#17921 = EDGE_CURVE ( 'NONE', #125480, #146898, #157946, .T. ) ;
#17922 = CARTESIAN_POINT ( 'NONE',  ( 7.313733799568044702, 10.62010763521636214, 1.199719254218460707 ) ) ;
#17923 =( NAMED_UNIT ( * ) SI_UNIT ( $, .STERADIAN. ) SOLID_ANGLE_UNIT ( ) );
#17924 = CARTESIAN_POINT ( 'NONE',  ( 4.436427218767265757, 1.790408935156896586, 0.3557191534368231434 ) ) ;
#17925 = CARTESIAN_POINT ( 'NONE',  ( 4.412732527109735514, -1.242725882911545510, -1.587838301257207041 ) ) ;
#17926 = CARTESIAN_POINT ( 'NONE',  ( -8.178592977541617515, 10.56477777859713463, 1.599625672291295375 ) ) ;
#17928 = CARTESIAN_POINT ( 'NONE',  ( -5.433785704026946384, 9.561443431331920095, 0.000000000000000000 ) ) ;
#17927 = CARTESIAN_POINT ( 'NONE',  ( 5.137693465899466183, -1.596169073733178845, -1.603756505840604918 ) ) ;
#17929 = CARTESIAN_POINT ( 'NONE',  ( 0.04767123857605212733, -1.629476508726154016, -1.334019646271035198 ) ) ;
#17930 = CARTESIAN_POINT ( 'NONE',  ( 4.668459276380106715, -0.8822503692092443783, -1.873099891353036561 ) ) ;
#17931 = CARTESIAN_POINT ( 'NONE',  ( 10.06423010004587759, 10.63602329300870153, 0.000000000000000000 ) ) ;
#17932 = CARTESIAN_POINT ( 'NONE',  ( -3.755786496842897795E-14, 2.109375000341444206, -1.570758158831810247 ) ) ;
#17933 = PRODUCT_CONTEXT ( 'NONE', #38036, 'mechanical' ) ;
#17935 = CARTESIAN_POINT ( 'NONE',  ( 2.332535780611888043, 1.868688736674573247, 0.4679572130895108817 ) ) ;
#17934 = CARTESIAN_POINT ( 'NONE',  ( -9.501566725078754772, 9.979582688880366703, -0.7998128361456291469 ) ) ;
#17936 = CARTESIAN_POINT ( 'NONE',  ( 0.000000000000000000, 0.000000000000000000, 0.000000000000000000 ) ) ;
#17937 = CARTESIAN_POINT ( 'NONE',  ( 0.5198876536083548716, 1.948639688611382148, -0.2852860490613322031 ) ) ;
#17938 = CARTESIAN_POINT ( 'NONE',  ( 6.770317605177710085, 8.992066187497757213, 1.599625672291268286 ) ) ;
#17939 = CARTESIAN_POINT ( 'NONE',  ( 5.786614514570532997, 6.041473168147688533, -0.5398422057949890940 ) ) ;
#17940 = CARTESIAN_POINT ( 'NONE',  ( -2.103486388414573138, 5.605817886458954291, 1.040834085586084257E-14 ) ) ;
#17942 = CARTESIAN_POINT ( 'NONE',  ( 1.494693441997055894, -1.183060725354843079, 1.879997432091018217 ) ) ;
#17941 = CARTESIAN_POINT ( 'NONE',  ( 0.5980879788009090259, 1.428637019467562830, 1.567290143595565066 ) ) ;
#17943 = CARTESIAN_POINT ( 'NONE',  ( 3.733512407637301855, -1.946585179706640467, 0.8041552576890409476 ) ) ;
#17944 = CARTESIAN_POINT ( 'NONE',  ( -5.250750630242457362, 9.347902511916677426, 0.000000000000000000 ) ) ;
#17945 = CARTESIAN_POINT ( 'NONE',  ( 7.070740804726770357, 8.207951346058097286, 1.199719254218462483 ) ) ;
#17946 = CARTESIAN_POINT ( 'NONE',  ( 3.016010921186715432, 1.952665002612500533, -0.1895750030070641190 ) ) ;
#17947 = CARTESIAN_POINT ( 'NONE',  ( 6.043183783389218355, 8.073467052085995022, 1.599625672291267398 ) ) ;
#17948 = CARTESIAN_POINT ( 'NONE',  ( -4.167783244592077274, 7.418453011031667543, -0.7534271236282058526 ) ) ;
#17949 = CARTESIAN_POINT ( 'NONE',  ( 3.147464216666835402, 6.823792019419957278, -0.7998128361456291469 ) ) ;
#17950 = CARTESIAN_POINT ( 'NONE',  ( -4.638297949650955765, 8.425448351319163365, 0.7216878364870267237 ) ) ;
#17951 = CARTESIAN_POINT ( 'NONE',  ( -8.514157279702036618, 9.035531035848267223, -0.7216878364870278340 ) ) ;
#17952 = AXIS2_PLACEMENT_3D ( 'NONE', #170064, #50998, #153834 ) ;
#17953 = CARTESIAN_POINT ( 'NONE',  ( 1.072698285844303934, 0.8645715524648779349, 1.936551149067309741 ) ) ;
#17954 = CARTESIAN_POINT ( 'NONE',  ( -7.259464905474441565, 7.434073576000447048, -0.7998128361456362523 ) ) ;
#17956 = CARTESIAN_POINT ( 'NONE',  ( 4.650807877244386823, -0.4278111053654386486, -1.914496481071884970 ) ) ;
#17955 = CARTESIAN_POINT ( 'NONE',  ( 1.224999999999971001, 1.354166666666710483, 0.7072540797572898219 ) ) ;
#17957 = CARTESIAN_POINT ( 'NONE',  ( 3.573254463033649131, 0.05508235185803719847, -2.161170636208443963 ) ) ;
#17958 = CARTESIAN_POINT ( 'NONE',  ( 1.452429406588066740, -1.579491434881035827, -0.9459884711465746943 ) ) ;
#17959 = AXIS2_PLACEMENT_3D ( 'NONE', #192873, #160394, #110647 ) ;
#17960 = CARTESIAN_POINT ( 'NONE',  ( -4.072711641797504001, 7.543564457389225986, 0.4874124537386469447 ) ) ;
#17961 = CARTESIAN_POINT ( 'NONE',  ( 0.6823417656249864960, -1.011458332991911568, -1.181850606188749264 ) ) ;
#17962 = CARTESIAN_POINT ( 'NONE',  ( 4.593551391122507432, -1.740074876368927104, -0.03866795590094784102 ) ) ;
#17963 = CARTESIAN_POINT ( 'NONE',  ( -9.898321827452971178, 16.00000000001253753, -7.924999999985292476 ) ) ;
#17964 = CARTESIAN_POINT ( 'NONE',  ( 5.843201017809841247, 5.919415396974013532, 1.040834085586084257E-14 ) ) ;
#17965 = CARTESIAN_POINT ( 'NONE',  ( -10.99318506637795956, 6.209869560752310669, 6.173358988436974393 ) ) ;
#17966 = CARTESIAN_POINT ( 'NONE',  ( 2.307699607974790901, -0.4742087202370263155, 2.108885336910087283 ) ) ;
#17967 = ADVANCED_FACE ( 'NONE', ( #1985 ), #120176, .F. ) ;
#17968 = CARTESIAN_POINT ( 'NONE',  ( 4.815779736370030761, -1.620933320526974031, 1.198678058543983571 ) ) ;
#17969 = DIRECTION ( 'NONE',  ( -0.000000000000000000, 1.000000000000000000, -0.000000000000000000 ) ) ;
#17970 = CARTESIAN_POINT ( 'NONE',  ( 1.692469166403000491, -2.151312531270420436, -0.2117842694067117448 ) ) ;
#17971 = CARTESIAN_POINT ( 'NONE',  ( 3.907068546088189986, 1.690197745946390162, 1.014639218175046764 ) ) ;
#17972 = CARTESIAN_POINT ( 'NONE',  ( -6.580325463743616154, 6.773331238431972601, 0.4807764197584866728 ) ) ;
#17973 = CARTESIAN_POINT ( 'NONE',  ( 3.948723843360758323, -1.616405859212793894, -1.076207510925797139 ) ) ;
#17976 = ORIENTED_EDGE ( 'NONE', *, *, #188508, .F. ) ;
#17975 = CARTESIAN_POINT ( 'NONE',  ( -3.283337425626721373, -0.1112512837626866702, -0.1207467602163218856 ) ) ;
#17974 = CARTESIAN_POINT ( 'NONE',  ( -9.531018800282611281, 12.14260790512831889, 1.443375672974076540 ) ) ;
#17977 = CARTESIAN_POINT ( 'NONE',  ( -7.795011973214244883, 8.058878488363559356, 0.7998128361456341429 ) ) ;
#17978 = CARTESIAN_POINT ( 'NONE',  ( 9.858406733136194415E-16, 3.000000000000002665, -8.050000000000000711 ) ) ;
#17979 = CARTESIAN_POINT ( 'NONE',  ( -5.666381855868691808, 5.575476684793721383, 0.000000000000000000 ) ) ;
#17980 = CARTESIAN_POINT ( 'NONE',  ( -5.550083779947821760, 7.568460058062819407, -1.599625672291271394 ) ) ;
#17981 = CARTESIAN_POINT ( 'NONE',  ( -9.449669878600623463, 11.08733161553131197, -1.082531754730537976 ) ) ;
#17982 = CARTESIAN_POINT ( 'NONE',  ( 0.2357703454196959370, -2.016519153289020760, 0.8967723332334791575 ) ) ;
#17983 = CARTESIAN_POINT ( 'NONE',  ( -3.285556943749998737, -3.930208332855377407, 1.896917185911908499 ) ) ;
#17984 = CARTESIAN_POINT ( 'NONE',  ( 5.172687041346638814, 1.355624813549320740, -1.418227474788292364 ) ) ;
#17985 = CARTESIAN_POINT ( 'NONE',  ( 1.389296306420295224, -0.7283806465635984662, -1.880434191983325398 ) ) ;
#17986 = ORIENTED_EDGE ( 'NONE', *, *, #201940, .T. ) ;
#17987 = CARTESIAN_POINT ( 'NONE',  ( 3.889952640533121286, -2.111394073168832097, 0.1598612332101984890 ) ) ;
#17988 = CARTESIAN_POINT ( 'NONE',  ( 1.499999999999987121, 3.327083334016150751, -0.8660254037844262731 ) ) ;
#17990 = CARTESIAN_POINT ( 'NONE',  ( -5.799137018343247796, 7.788745826199009237, -1.599625672291256295 ) ) ;
#17989 = CARTESIAN_POINT ( 'NONE',  ( 9.499668754385638181, -7.246166700194470067, 0.07933194154488365513 ) ) ;
#17991 = CARTESIAN_POINT ( 'NONE',  ( 4.206863059814883066, -0.3125640686512491384, 1.814249101404527220 ) ) ;
#17992 = ORIENTED_EDGE ( 'NONE', *, *, #38172, .F. ) ;
#17993 = UNCERTAINTY_MEASURE_WITH_UNIT (LENGTH_MEASURE( 1.000000000000000082E-05 ), #71744, 'distance_accuracy_value', 'NONE');
#17994 = CARTESIAN_POINT ( 'NONE',  ( -7.648771216403934758, 12.07531685244661723, -0.7998128361456291469 ) ) ;
#17995 = CARTESIAN_POINT ( 'NONE',  ( 0.4205683736966560615, 3.129384673317399113, 0.4296503687815094175 ) ) ;
#17996 = CARTESIAN_POINT ( 'NONE',  ( 4.640951271726033056, 2.030106984047326701, 0.6129599860185754867 ) ) ;
#17997 = CARTESIAN_POINT ( 'NONE',  ( 11.55950211276791251, 13.87999999999998302, 3.221476510067114329 ) ) ;
#17998 = CARTESIAN_POINT ( 'NONE',  ( 6.471319392424407901, 6.444294134116939077, 0.7998128361456341429 ) ) ;
#17999 = EDGE_CURVE ( 'NONE', #141519, #119587, #87926, .T. ) ;
#18000 = CARTESIAN_POINT ( 'NONE',  ( 5.993449436079309578, 1.557461279572001756, 1.349564693925601189 ) ) ;
#18001 = AXIS2_PLACEMENT_3D ( 'NONE', #25821, #44234, #23691 ) ;
#18003 = CARTESIAN_POINT ( 'NONE',  ( 2.858754248528099229, 0.2676582106064147593, -1.821554178878769470 ) ) ;
#18002 = CARTESIAN_POINT ( 'NONE',  ( 1.222862307070234911, -1.680409034227359211, -0.8001750615637763797 ) ) ;
#18004 = CARTESIAN_POINT ( 'NONE',  ( 7.910292558569346433, 11.31609285405122556, -1.199719254218446718 ) ) ;
#18005 = DIRECTION ( 'NONE',  ( 0.000000000000000000, -1.000000000000000000, -0.000000000000000000 ) ) ;
#18006 = CARTESIAN_POINT ( 'NONE',  ( 3.673896439623290266, 4.156855427197417185, 1.000000000000011324 ) ) ;
#18007 = CARTESIAN_POINT ( 'NONE',  ( -1.162044386198238935E-15, 2.625000000682799151, 1.224999999999985656 ) ) ;
#18008 = CARTESIAN_POINT ( 'NONE',  ( 1.664966938652842954, -1.558911317520403239, 1.562347339584921002 ) ) ;
#18009 = CARTESIAN_POINT ( 'NONE',  ( 5.413438844936455219, -0.3396298981525199823, 2.236681904191807568 ) ) ;
#18010 = CARTESIAN_POINT ( 'NONE',  ( 3.573454097414618946, 1.463926983822515293, 1.387100322000796027 ) ) ;
#18011 = CARTESIAN_POINT ( 'NONE',  ( -7.456621297836087514, 9.722477485607340597, 1.443375672974090751 ) ) ;
#18012 = CARTESIAN_POINT ( 'NONE',  ( 4.359482725938978120, -1.404519563743265920, -1.144221460762798737 ) ) ;
#18013 = CARTESIAN_POINT ( 'NONE',  ( 5.260912935490944520, -0.05370519216219872549, -1.915158585242337397 ) ) ;
#18014 = CARTESIAN_POINT ( 'NONE',  ( -0.6823417656250212460, 5.113541667008086655, 1.181850606188767472 ) ) ;
#18015 = CARTESIAN_POINT ( 'NONE',  ( 3.748864756286158340, -1.612500686720008236, 1.134000162313458793 ) ) ;
#18016 = CARTESIAN_POINT ( 'NONE',  ( 5.278141497218024725, -1.038406966791558528, 1.555765341417144842 ) ) ;
#18017 = CARTESIAN_POINT ( 'NONE',  ( 4.422197255734514165, 0.8761312318771010688, 1.641894029917531084 ) ) ;
#18018 = DIRECTION ( 'NONE',  ( -1.000000000000000000, -3.451266460341925773E-31, -8.638326563840809144E-31 ) ) ;
#18019 = AXIS2_PLACEMENT_3D ( 'NONE', #395, #38012, #104084 ) ;
#18020 = CARTESIAN_POINT ( 'NONE',  ( 5.383597848809928088, 1.190821987996647513, 1.309499010278234898 ) ) ;
#18021 = CARTESIAN_POINT ( 'NONE',  ( -0.2234322562767385167, -0.4468160588090731022, -1.973564571300358228 ) ) ;
#18023 = CARTESIAN_POINT ( 'NONE',  ( 2.174573150871310201, -1.294977634586411908, 1.660803824364719405 ) ) ;
#18022 = CARTESIAN_POINT ( 'NONE',  ( -10.10098813738111545, 11.74323990082152491, -1.199719254218441611 ) ) ;
#18024 = CARTESIAN_POINT ( 'NONE',  ( 10.26082332744404368, 10.86538205830655279, -0.7998128361456281477 ) ) ;
#18026 = CARTESIAN_POINT ( 'NONE',  ( -8.455481356417053007, 13.01647868246193518, 0.7998128361456341429 ) ) ;
#18025 = DIRECTION ( 'NONE',  ( -1.000000000000000000, 0.000000000000000000, 0.000000000000000000 ) ) ;
#18027 = CARTESIAN_POINT ( 'NONE',  ( 3.199588043238619228, 1.915454767000431602, -0.9102714984489732597 ) ) ;
#18028 = DIRECTION ( 'NONE',  ( 0.5005768354468328463, -0.8656921114426504582, 6.106226635438361958E-16 ) ) ;
#18029 = CARTESIAN_POINT ( 'NONE',  ( 2.250265822158686646, 0.9482326530925830887, -1.783330763309778577 ) ) ;
#18030 = CARTESIAN_POINT ( 'NONE',  ( -1.364683531250014514, 1.988541667008086655, -0.7879004041258289570 ) ) ;
#18031 = CARTESIAN_POINT ( 'NONE',  ( 6.620655732516649294, 0.5971256128398574337, 1.879834161342401666 ) ) ;
#18032 = CARTESIAN_POINT ( 'NONE',  ( 3.337278367258157630, 7.045241861776501580, 0.7998128361456341429 ) ) ;
#18033 = VERTEX_POINT ( 'NONE', #59299 ) ;
#18034 = EDGE_CURVE ( 'NONE', #103348, #179825, #128429, .T. ) ;
#18035 = CARTESIAN_POINT ( 'NONE',  ( 1.915512222264357467, -0.2666219456287990952, 2.145042957367573777 ) ) ;
#18036 = CARTESIAN_POINT ( 'NONE',  ( 6.890000000000010338, 2.965158640989657979, 2.452917560796507246 ) ) ;
#18039 = CARTESIAN_POINT ( 'NONE',  ( 2.901081683644319842, 5.368050483351580304, 1.082531754730548412 ) ) ;
#18038 = CARTESIAN_POINT ( 'NONE',  ( 3.834746474454188013E-15, 13.09375000068279959, 1.500000000000001554 ) ) ;
#18037 = CARTESIAN_POINT ( 'NONE',  ( 4.085803189671889157, 5.860132702740892263, -1.599625672291273171 ) ) ;
#18040 = CARTESIAN_POINT ( 'NONE',  ( 8.541273586484978253, 12.90864358430044589, 0.000000000000000000 ) ) ;
#18041 = CARTESIAN_POINT ( 'NONE',  ( -8.103009739378183696, -6.700000000000007283, 7.439168848973805481 ) ) ;
#18042 = CARTESIAN_POINT ( 'NONE',  ( -7.131225611108100715, 9.342849184424693476, 1.443375672974078761 ) ) ;
#18043 = CARTESIAN_POINT ( 'NONE',  ( 1.312353134292881141, 1.468346937154514364, -1.627112938194043235 ) ) ;
#18044 = FACE_OUTER_BOUND ( 'NONE', #77963, .T. ) ;
#18046 = CARTESIAN_POINT ( 'NONE',  ( 0.6823417656249969321, 12.27604166700806054, -1.181850606188757036 ) ) ;
#18045 = CARTESIAN_POINT ( 'NONE',  ( 1.833286743572108968, 0.2227676567047157941, 2.251508545315301646 ) ) ;
#18047 = CARTESIAN_POINT ( 'NONE',  ( -8.833300774503376473, 10.26427131079744193, 1.199719254218462483 ) ) ;
#18048 = CARTESIAN_POINT ( 'NONE',  ( -5.273758565591545988, 6.215435083687305351, 1.082531754730546636 ) ) ;
#18049 = CARTESIAN_POINT ( 'NONE',  ( 0.6823417656249882723, 2.238541667008084435, -1.181850606188749264 ) ) ;
#18050 = CARTESIAN_POINT ( 'NONE',  ( 4.646267551848549004, 8.309382712783076386, 0.4446711254955729165 ) ) ;
#18051 = AXIS2_PLACEMENT_3D ( 'NONE', #147015, #48446, #180553 ) ;
#18052 = CARTESIAN_POINT ( 'NONE',  ( -1.500000000000008216, 10.99999999999999645, 3.469446951953614189E-15 ) ) ;
#18053 = CARTESIAN_POINT ( 'NONE',  ( 4.927462483923885195, 4.713404084191450849, -0.7998128361456481317 ) ) ;
#18054 = ADVANCED_FACE ( 'NONE', ( #162152 ), #60635, .F. ) ;
#18055 = CARTESIAN_POINT ( 'NONE',  ( 3.620126565017945275, 1.124893713931356842, -1.366185836280229715 ) ) ;
#18056 = CARTESIAN_POINT ( 'NONE',  ( 6.211994372536747022, -2.190858219723303080, 0.2640275128017176565 ) ) ;
#18057 = ORIENTED_EDGE ( 'NONE', *, *, #193087, .F. ) ;
#18058 = CARTESIAN_POINT ( 'NONE',  ( -6.473091995881817162, 6.516638514809040217, 0.7998128361456281477 ) ) ;
#18059 = CARTESIAN_POINT ( 'NONE',  ( 5.589470316598125876, -0.4871849528341637980, 1.956566939648955339 ) ) ;
#18060 = EDGE_LOOP ( 'NONE', ( #148558, #78337, #41757, #56181 ) ) ;
#18061 = CARTESIAN_POINT ( 'NONE',  ( 2.008475284031425723, 1.387998011844304491, -1.254312187223500796 ) ) ;
#18062 = CARTESIAN_POINT ( 'NONE',  ( 2.413015750098276513, -1.603085927076562500, 1.310038033242977518 ) ) ;
#18063 = CARTESIAN_POINT ( 'NONE',  ( -6.224601922005509991, 10.27613631906616476, 0.7216878364870267237 ) ) ;
#18064 = CARTESIAN_POINT ( 'NONE',  ( 2.250135261179100343, 0.8981609309555339538, -1.688322754368525747 ) ) ;
#18065 = CARTESIAN_POINT ( 'NONE',  ( -5.639168051347689392, 7.169606540874463363, 1.217459232585948570 ) ) ;
#18066 = CARTESIAN_POINT ( 'NONE',  ( -10.22593938286385296, 3.000029897349846930, -7.498676971688964521 ) ) ;
#18067 = CARTESIAN_POINT ( 'NONE',  ( 0.4362825330288246928, -6.085430761754772711, 10.10516068267232548 ) ) ;
#18068 = EDGE_CURVE ( 'NONE', #85365, #116525, #109609, .T. ) ;
#18069 = CARTESIAN_POINT ( 'NONE',  ( -0.6823417656249969321, 4.780208333674755394, -1.181850606188749264 ) ) ;
#18070 = CARTESIAN_POINT ( 'NONE',  ( 0.07037084582631887575, 0.7337836260858083826, 1.766209603411242668 ) ) ;
#18071 = CARTESIAN_POINT ( 'NONE',  ( 4.584065335196252811, 8.362176967788721882, 0.7216878364870328300 ) ) ;
#18072 = CARTESIAN_POINT ( 'NONE',  ( 1.152704166800899932, -0.4732522875653189520, -1.903817266927515961 ) ) ;
#18073 = ADVANCED_FACE ( 'NONE', ( #146392 ), #16111, .T. ) ;
#18074 = CARTESIAN_POINT ( 'NONE',  ( 0.2630457479233569984, -2.015603748724136945, -0.05229424383911692592 ) ) ;
#18075 = CARTESIAN_POINT ( 'NONE',  ( -5.496904935697871863, 5.377753611261092637, 0.7998128361456281477 ) ) ;
#18076 = CARTESIAN_POINT ( 'NONE',  ( 5.010073305087408002, -0.7609581946756528437, 1.979555329295646260 ) ) ;
#18077 = CARTESIAN_POINT ( 'NONE',  ( 9.043452155515161905, 10.50944792197790889, 1.199719254218453823 ) ) ;
#18078 = CARTESIAN_POINT ( 'NONE',  ( 6.591095686763909001, 1.716256228956919871, -0.9697327587238188107 ) ) ;
#18079 = CARTESIAN_POINT ( 'NONE',  ( -1.364683531249997417, 2.509375000341422357, 1.214306433183764966E-14 ) ) ;
#18080 = CARTESIAN_POINT ( 'NONE',  ( 1.511978199970403836, -0.6742157057700901568, 1.897102442587648374 ) ) ;
#18082 = CARTESIAN_POINT ( 'NONE',  ( 1.230240178466317724, 2.114980979692267393, 0.09988113581482771508 ) ) ;
#18081 = CARTESIAN_POINT ( 'NONE',  ( -7.551528373131759508, 7.912463978182924684, 1.040834085586084257E-14 ) ) ;
#18083 = CARTESIAN_POINT ( 'NONE',  ( 9.442551103936683177, 11.02991041777048231, 7.411286945868026166 ) ) ;
#18084 = CARTESIAN_POINT ( 'NONE',  ( 2.699741690289765295, -1.532448122638006671, -1.392287113214360827 ) ) ;
#18085 = CARTESIAN_POINT ( 'NONE',  ( 3.203469434578891661, 6.959407783642502565, -0.7998128361456362523 ) ) ;
#18086 = CARTESIAN_POINT ( 'NONE',  ( 4.655245641445829641, 6.524482229810530498, 1.599625672291269396 ) ) ;
#18087 = ORIENTED_EDGE ( 'NONE', *, *, #57719, .T. ) ;
#18089 = CARTESIAN_POINT ( 'NONE',  ( 3.357615597678655917, 7.068968630600412695, 0.7998128361456321445 ) ) ;
#18088 = CARTESIAN_POINT ( 'NONE',  ( 5.402318495819277366, 1.583515501651384438, -1.365094957383119700 ) ) ;
#18092 = ORIENTED_EDGE ( 'NONE', *, *, #211296, .F. ) ;
#18091 = CARTESIAN_POINT ( 'NONE',  ( 2.631291878999729938, -0.1756591012599724722, 1.802909387868474766 ) ) ;
#18090 = CARTESIAN_POINT ( 'NONE',  ( 4.524309061075334704, 1.122661849025725189, -1.439470297551891154 ) ) ;
#18093 = CARTESIAN_POINT ( 'NONE',  ( 8.809047120577066181, 11.30030761213851953, 1.599625672291281386 ) ) ;
#18094 = DIRECTION ( 'NONE',  ( 0.000000000000000000, -1.000000000000000000, 0.000000000000000000 ) ) ;
#18095 = CARTESIAN_POINT ( 'NONE',  ( 9.992730418911948576, 9.901705038286040761, 5.020517729075291591 ) ) ;
#18096 = CARTESIAN_POINT ( 'NONE',  ( 5.473716482686670659, 2.128106746890707335, -0.5837492795209007213 ) ) ;
#18097 = CARTESIAN_POINT ( 'NONE',  ( -1.364683531250010740, 8.942708333674731946, 0.7879004041258445001 ) ) ;
#18098 = ORIENTED_EDGE ( 'NONE', *, *, #91149, .F. ) ;
#18099 = CARTESIAN_POINT ( 'NONE',  ( 3.686107007616833631, 1.064666855108999721, 1.588282736317746302 ) ) ;
#18100 = CARTESIAN_POINT ( 'NONE',  ( -3.436101866059630527, 6.096203712789787232, 1.199719254218462483 ) ) ;
#18101 = VECTOR ( 'NONE', #204232, 1000.000000000000000 ) ;
#18102 = CARTESIAN_POINT ( 'NONE',  ( 8.444030743212801227, 8.745790710036752458, 0.7998128361456462443 ) ) ;
#18103 = AXIS2_PLACEMENT_3D ( 'NONE', #4931, #105708, #185836 ) ;
#18104 = CARTESIAN_POINT ( 'NONE',  ( -1.360316468750038865, 0.4427083336747321130, 0.7853790794158700406 ) ) ;
#18105 = CARTESIAN_POINT ( 'NONE',  ( 3.782361668088245921, 6.396210465202840645, -1.082531754730548412 ) ) ;
#18106 = CARTESIAN_POINT ( 'NONE',  ( 7.704073495075588696, 14.42981585874038153, -9.201162189417628312 ) ) ;
#18107 = CARTESIAN_POINT ( 'NONE',  ( -0.1237769027084348328, -0.1346504581853508187, -1.811164470923332104 ) ) ;
#18108 = VERTEX_POINT ( 'NONE', #62973 ) ;
#18109 = CARTESIAN_POINT ( 'NONE',  ( -11.86239285000045918, 12.22000000000000064, -1.812080536912752837 ) ) ;
#18110 = CARTESIAN_POINT ( 'NONE',  ( 3.883945074633635031, -0.9243716352356041721, 1.626130415258054018 ) ) ;
#18111 = CARTESIAN_POINT ( 'NONE',  ( 5.671053392266061977, 9.838255734277600695, 0.7998128361456331437 ) ) ;
#18112 = DIRECTION ( 'NONE',  ( -1.000000000000000000, 0.000000000000000000, 1.224646799147352961E-16 ) ) ;
#18113 =( BOUNDED_CURVE ( )  B_SPLINE_CURVE ( 2, ( #200103, #51753, #120014, #117876, #19225, #85303, #152446, #151389, #2959 ),
 .UNSPECIFIED., .F., .T. ) 
 B_SPLINE_CURVE_WITH_KNOTS ( ( 3, 2, 2, 2, 3 ),
 ( 0.5267857142857143016, 0.5297619047619047672, 0.5357142857142856984, 0.5416666666666666297, 0.5446428571428572063 ),
 .UNSPECIFIED. ) 
 CURVE ( )  GEOMETRIC_REPRESENTATION_ITEM ( )  RATIONAL_B_SPLINE_CURVE ( ( 0.9330127018922194093, 0.9330127018922194093, 1.000000000000000000, 0.8660254037844387076, 1.000000000000000000, 0.8660254037844387076, 1.000000000000000000, 0.9330127018922180770, 0.9330127018922194093 ) ) 
 REPRESENTATION_ITEM ( '' )  );
#18114 = CARTESIAN_POINT ( 'NONE',  ( -7.537970219518089543, 8.857015346601659900, -1.082531754730543971 ) ) ;
#18115 = CARTESIAN_POINT ( 'NONE',  ( 5.671388329218120639, 5.511041227042920099, 1.040834085586084257E-14 ) ) ;
#18116 = CARTESIAN_POINT ( 'NONE',  ( 6.455931442665615805, -0.7031469350025701948, 1.947301169641938223 ) ) ;
#18117 = CARTESIAN_POINT ( 'NONE',  ( 2.689077551358230789, 1.704951624378052033, 1.076298511635757738 ) ) ;
#18118 = CARTESIAN_POINT ( 'NONE',  ( -9.643927338022246332, 10.14567007064778004, -0.7998128361456291469 ) ) ;
#18119 = CARTESIAN_POINT ( 'NONE',  ( 5.505492895601038938, 8.580769590579979678, -1.199719254218452047 ) ) ;
#18120 = DIRECTION ( 'NONE',  ( -0.9999980456341538426, 0.000000000000000000, -0.001977050295941298105 ) ) ;
#18121 = CARTESIAN_POINT ( 'NONE',  ( 2.713028398602938651, -0.2137989841624072795, 2.180988865010752509 ) ) ;
#18122 = CARTESIAN_POINT ( 'NONE',  ( 6.164658409365946667, -1.287482145768016117, 1.294691480910937553 ) ) ;
#18123 = CARTESIAN_POINT ( 'NONE',  ( -4.460796234096120472, 5.163016013655583158, 1.199719254218462483 ) ) ;
#18124 = CARTESIAN_POINT ( 'NONE',  ( 4.909461021924254709, 5.860697626067345567, 1.082531754730549078 ) ) ;
#18125 = CARTESIAN_POINT ( 'NONE',  ( 8.289920859751990889, 11.75899253876431416, 1.199719254218450271 ) ) ;
#18126 = CARTESIAN_POINT ( 'NONE',  ( 3.032219910950674890, 6.689340329417765574, 0.7998128361456321445 ) ) ;
#18127 = CARTESIAN_POINT ( 'NONE',  ( 5.045042558060919724, 8.899983727797476263, -0.7216878364870458196 ) ) ;
#18128 = ORIENTED_EDGE ( 'NONE', *, *, #51352, .F. ) ;
#18130 = CARTESIAN_POINT ( 'NONE',  ( 0.2936080233231981862, 1.877589464902774674, -0.7265071302150533095 ) ) ;
#18129 = CARTESIAN_POINT ( 'NONE',  ( 3.843160323004328305, 0.6166970922517557296, -1.735048075492843456 ) ) ;
#18131 = CARTESIAN_POINT ( 'NONE',  ( 3.603114471349005754, 1.037088744013005659, -2.051189238963199379 ) ) ;
#18133 = CARTESIAN_POINT ( 'NONE',  ( 1.182201811662712210, 1.114302846955270709, -1.490276101724023583 ) ) ;
#18132 = CARTESIAN_POINT ( 'NONE',  ( 2.846849069189655967, 5.304779099821139710, -1.082531754730543083 ) ) ;
#18134 = CARTESIAN_POINT ( 'NONE',  ( 0.000000000000000000, -0.4374999999999981126, -4.012584370867899430 ) ) ;
#18135 = CARTESIAN_POINT ( 'NONE',  ( -4.120788623549732854, 6.895004929861607401, -1.199719254218452047 ) ) ;
#18136 = CARTESIAN_POINT ( 'NONE',  ( -0.4000000000000322742, 3.950000000000009059, 1.007084189318363077 ) ) ;
#18137 = CARTESIAN_POINT ( 'NONE',  ( 4.675980034926481288, 1.890745994642643479, -0.2862527531290667837 ) ) ;
#18138 = CARTESIAN_POINT ( 'NONE',  ( -7.160677686311960777, 11.50587440067263678, -0.7998128361456291469 ) ) ;
#18139 = MANIFOLD_SOLID_BREP ( 'Fillet1', #25706 ) ;
#18140 = CARTESIAN_POINT ( 'NONE',  ( 6.467812791377033577, 6.763347601114057639, -0.2696018389747659172 ) ) ;
#18141 = CARTESIAN_POINT ( 'NONE',  ( -6.617788377246193399, 8.814115421577600529, -1.443375672974066548 ) ) ;
#18143 = CARTESIAN_POINT ( 'NONE',  ( 2.219420098953532428, -1.815089452277141691, 0.4520615115926190919 ) ) ;
#18142 = CARTESIAN_POINT ( 'NONE',  ( 3.421503388043937832, -1.247306758965301521, -1.677755357943153447 ) ) ;
#18144 = CARTESIAN_POINT ( 'NONE',  ( 6.914295153289432783, 10.05013286460426691, -1.082531754730537976 ) ) ;
#18145 = CARTESIAN_POINT ( 'NONE',  ( -6.650326532587143902, -8.038658175288281527, -6.784185045882105136 ) ) ;
#18146 = CARTESIAN_POINT ( 'NONE',  ( 5.864778394761136049, 0.1288883805774850844, -1.836796581567698539 ) ) ;
#18147 = AXIS2_PLACEMENT_3D ( 'NONE', #49844, #43737, #149480 ) ;
#18148 = CARTESIAN_POINT ( 'NONE',  ( 3.358669367883368118, 4.941533567329135401, -1.599625672291262513 ) ) ;
#18150 = CARTESIAN_POINT ( 'NONE',  ( 3.655894977179307226, 7.416961240017848844, -0.7998128361456291469 ) ) ;
#18149 = CARTESIAN_POINT ( 'NONE',  ( 1.278248824818062671E-15, 1.062499999999996003, 1.224999999999968781 ) ) ;
#18151 = CARTESIAN_POINT ( 'NONE',  ( 3.387030231456603424, 1.558874866368621159, -0.7386201850746020314 ) ) ;
#18152 = CARTESIAN_POINT ( 'NONE',  ( -7.711890448074853133, 7.891627032375787998, -0.7998128361456291469 ) ) ;
#18153 = CARTESIAN_POINT ( 'NONE',  ( 6.410767893487317792, 1.638320036227768783, -1.478771730184471389 ) ) ;
#18154 = CARTESIAN_POINT ( 'NONE',  ( 6.983263157960391432, 4.691677264508577139, 2.616375093613742209 ) ) ;
#18155 = DIRECTION ( 'NONE',  ( 0.000000000000000000, -1.000000000000000000, 0.000000000000000000 ) ) ;
#18156 = CARTESIAN_POINT ( 'NONE',  ( 5.278266929526361118, -1.155484533919543422, -1.837868763204909994 ) ) ;
#18157 = CARTESIAN_POINT ( 'NONE',  ( 2.842213963582499670, 1.811911227886909614, 0.2232855069103783507 ) ) ;
#18158 = DIRECTION ( 'NONE',  ( 0.000000000000000000, 0.000000000000000000, -1.000000000000000000 ) ) ;
#18159 = CARTESIAN_POINT ( 'NONE',  ( 6.069547426979996274, 1.461697874074740389, 1.532048495917796016 ) ) ;
#18160 = EDGE_LOOP ( 'NONE', ( #178324, #187270, #20793, #194947 ) ) ;
#18162 = CARTESIAN_POINT ( 'NONE',  ( -1.364683531250012516, 2.092708333674750953, 0.7879004041258379498 ) ) ;
#18161 = CARTESIAN_POINT ( 'NONE',  ( 6.093372230586791893, -0.7761969640797984349, 2.157113249652943932 ) ) ;
#18163 = CARTESIAN_POINT ( 'NONE',  ( 9.399880572976245574, 9.860948844760784482, 0.7998128361456462443 ) ) ;
#18164 = CARTESIAN_POINT ( 'NONE',  ( 1.172698094321134477, 0.8626872041959359194, 1.937259058979395654 ) ) ;
#18165 = CARTESIAN_POINT ( 'NONE',  ( -3.456965981804629884, 6.976951378839947537, 1.040834085586084257E-14 ) ) ;
#18166 = DIRECTION ( 'NONE',  ( 0.6507913734559640506, -0.7592566023653004592, 0.000000000000000000 ) ) ;
#18167 = AXIS2_PLACEMENT_3D ( 'NONE', #155773, #125487, #206637 ) ;
#18168 = CARTESIAN_POINT ( 'NONE',  ( -5.056828107772852299, 7.883087978168217269, -1.082531754730548412 ) ) ;
#18169 = VECTOR ( 'NONE', #151795, 1000.000000000000000 ) ;
#18170 = CARTESIAN_POINT ( 'NONE',  ( 6.842638762948665132, -2.127444276778973631, -0.4322993451541176091 ) ) ;
#18172 = CARTESIAN_POINT ( 'NONE',  ( 0.7500000000000006661, 12.69791666734946389, -1.299038105676657340 ) ) ;
#18171 = CARTESIAN_POINT ( 'NONE',  ( 6.883263157960350043, 2.968548739964393945, 2.406833999121655854 ) ) ;
#18174 = VERTEX_POINT ( 'NONE', #199348 ) ;
#18173 = CARTESIAN_POINT ( 'NONE',  ( 1.612303553688280600, -0.7442547213242669546, 2.093046284049724370 ) ) ;
#18175 = CARTESIAN_POINT ( 'NONE',  ( 6.604150280000163242, -0.1430408514614608939, 1.983920101186954721 ) ) ;
#18177 = CARTESIAN_POINT ( 'NONE',  ( 4.100476343641854093, 2.052162271747024924, 0.2072667206600986300 ) ) ;
#18176 = CARTESIAN_POINT ( 'NONE',  ( 3.011882680530176604, 6.665613560593854459, 0.7998128361456341429 ) ) ;
#18179 = CARTESIAN_POINT ( 'NONE',  ( -3.475000000000000533, -3.179166666666664476, -2.006292185433948827 ) ) ;
#18178 = CARTESIAN_POINT ( 'NONE',  ( 5.722423353419669567, 8.833855124701747386, 1.199719254218451159 ) ) ;
#18180 = CARTESIAN_POINT ( 'NONE',  ( 7.686546744304875389, 7.932335721302671949, 0.7998128361456291469 ) ) ;
#18181 = CARTESIAN_POINT ( 'NONE',  ( 1.642778471875000035, -4.163541666188708135, -2.845375778867859751 ) ) ;
#18182 = PRESENTATION_STYLE_ASSIGNMENT (( #149271 ) ) ;
#18183 = CARTESIAN_POINT ( 'NONE',  ( -0.02340959012393610192, -0.1578203421408593821, -2.056509962333047614 ) ) ;
#18184 = CARTESIAN_POINT ( 'NONE',  ( 4.412732527109735514, -1.242725882911545510, -1.587838301257207041 ) ) ;
#18185 = CARTESIAN_POINT ( 'NONE',  ( 4.335397732480402055, 0.7831895168094182846, -1.666506522714307437 ) ) ;
#18186 = CARTESIAN_POINT ( 'NONE',  ( 3.493197133815315603, 7.227147089426516402, -0.7998128361456291469 ) ) ;
#18187 =( NAMED_UNIT ( * ) SI_UNIT ( $, .STERADIAN. ) SOLID_ANGLE_UNIT ( ) );
#18188 = CARTESIAN_POINT ( 'NONE',  ( 1.166562959395722077, -1.556812811267356711, -0.7427251802107991407 ) ) ;
#18189 = CARTESIAN_POINT ( 'NONE',  ( 0.2336117360935245635, 0.6279853779636718203, -1.916355031878452797 ) ) ;
#18190 = CARTESIAN_POINT ( 'NONE',  ( 1.372188323541504218, -0.3435771540031757332, -2.272792483656468576 ) ) ;
#18191 = CARTESIAN_POINT ( 'NONE',  ( -6.749261541504576911, 6.768559974710451677, 1.040834085586084257E-14 ) ) ;
#18192 = CARTESIAN_POINT ( 'NONE',  ( 0.9314073880264511773, 0.1673361042086803641, 2.256242939573564144 ) ) ;
#18193 = CARTESIAN_POINT ( 'NONE',  ( 3.580784747083717523, -2.029690618531124091, -0.5617794247858574064 ) ) ;
#18194 = CARTESIAN_POINT ( 'NONE',  ( -4.285259070371116863, 7.157163461145040095, 1.199719254218452935 ) ) ;
#18195 = CARTESIAN_POINT ( 'NONE',  ( 4.950698647284403009, 8.927565521807144577, 1.040834085586084257E-14 ) ) ;
#18196 = CARTESIAN_POINT ( 'NONE',  ( 4.706088717274896638, 7.544168365912456764, 1.082531754730548412 ) ) ;
#18197 = CARTESIAN_POINT ( 'NONE',  ( 0.000000000000000000, 2.344942989059404237, -2.501676308668091764 ) ) ;
#18198 = CARTESIAN_POINT ( 'NONE',  ( -5.738125327081750271, 7.717565519727259904, 1.599625672291269396 ) ) ;
#18199 = CARTESIAN_POINT ( 'NONE',  ( 1.499999999999989120, 1.525000000000019451, 0.000000000000000000 ) ) ;
#18201 = EDGE_CURVE ( 'NONE', #123242, #196200, #9399, .T. ) ;
#18200 = PRESENTATION_LAYER_ASSIGNMENT (  '', '', ( #35529 ) ) ;
#18202 = CARTESIAN_POINT ( 'NONE',  ( -4.243865776277440993, 4.909930479533815451, -1.199719254218446718 ) ) ;
#18203 = CARTESIAN_POINT ( 'NONE',  ( 5.010122972300034228, -0.7987708819462059351, 2.073016528135694703 ) ) ;
#18204 = CARTESIAN_POINT ( 'NONE',  ( 4.031328258368102269, -1.510625130563835627, -1.587819133214096734 ) ) ;
#18205 = CARTESIAN_POINT ( 'NONE',  ( -5.494078562035765501, 7.432844293840273231, -1.599625672291256295 ) ) ;
#18206 = CARTESIAN_POINT ( 'NONE',  ( 6.773846765317306229, -7.246166700180828535, -6.773846765317331986 ) ) ;
#18207 =( BOUNDED_SURFACE ( )  B_SPLINE_SURFACE ( 3, 2, ( 
 ( #210225, #48819, #195059 ),
 ( #145290, #161512, #78104 ),
 ( #113889, #192909, #213415 ),
 ( #144231, #44565, #131194 ) ),
 .UNSPECIFIED., .F., .F., .F. ) 
 B_SPLINE_SURFACE_WITH_KNOTS ( ( 4, 4 ),
 ( 3, 3 ),
 ( 3.059570999471135089, 3.223614307708988491 ),
 ( 0.000000000000000000, 1.000000000000000000 ),
 .UNSPECIFIED. ) 
 GEOMETRIC_REPRESENTATION_ITEM ( )  RATIONAL_B_SPLINE_SURFACE ( (
 ( 1.000000000000000000, 0.6179932349766422695, 1.000000000000000000),
 ( 1.000000000000000000, 0.6282795510881240553, 1.000000000000000000),
 ( 1.000000000000000000, 0.6282795510880839762, 1.000000000000000000),
 ( 1.000000000000000000, 0.6179932349765423494, 1.000000000000000000) ) ) 
 REPRESENTATION_ITEM ( '' )  SURFACE ( )  );
#18208 = CARTESIAN_POINT ( 'NONE',  ( 1.364683531249988535, 3.113541667008083991, 0.7879004041258500513 ) ) ;
#18209 = CARTESIAN_POINT ( 'NONE',  ( 6.609999999999971010, 7.629137130509032971, 2.879999999999991456 ) ) ;
#18210 = CARTESIAN_POINT ( 'NONE',  ( -4.392478581147607031, 7.108013530438723748, 1.082531754730560403 ) ) ;
#18211 = CARTESIAN_POINT ( 'NONE',  ( 5.502226937873657242, -0.9515977829631333540, 1.895136135177949877 ) ) ;
#18212 = CARTESIAN_POINT ( 'NONE',  ( -6.292392690518202159, 9.394856334696294553, -1.082531754730549967 ) ) ;
#18213 = ORIENTED_EDGE ( 'NONE', *, *, #202175, .T. ) ;
#18215 = CARTESIAN_POINT ( 'NONE',  ( 6.262596564776618635, -1.532251275270900326, 1.525113613579494709 ) ) ;
#18214 = CARTESIAN_POINT ( 'NONE',  ( -4.990809943606273613, 7.876343129965691858, -1.082531754730549967 ) ) ;
#18216 = CARTESIAN_POINT ( 'NONE',  ( 6.518772930072240790, 6.499656594706071822, -0.7998128361456281477 ) ) ;
#18217 = CARTESIAN_POINT ( 'NONE',  ( 5.952668924537682038, -1.582617586749142102, -0.9407850039931386910 ) ) ;
#18218 = CARTESIAN_POINT ( 'NONE',  ( -0.6823417656250212460, 2.363541667008084435, 1.181850606188767472 ) ) ;
#18219 = CARTESIAN_POINT ( 'NONE',  ( 1.294060738426667134, 1.423250580516822072, -1.001416416642088469 ) ) ;
#18220 = CARTESIAN_POINT ( 'NONE',  ( 4.356247428692526569, 3.976710176429713250, 0.7998128361456341429 ) ) ;
#18222 = EDGE_CURVE ( 'NONE', #119302, #322, #213252, .T. ) ;
#18221 = CARTESIAN_POINT ( 'NONE',  ( -9.578206920975032901, -9.954640969533237183, 0.1671882237015447359 ) ) ;
#18223 = CARTESIAN_POINT ( 'NONE',  ( -0.3617947196724534131, 3.196405949189511819, 2.034416336090804744 ) ) ;
#18224 = CARTESIAN_POINT ( 'NONE',  ( 8.868625083907582862, 12.79269056714098163, -8.084906220447308556 ) ) ;
#18225 = CARTESIAN_POINT ( 'NONE',  ( 4.803692121107413726, -0.5798474923815257753, 2.082409481564663434 ) ) ;
#18226 = EDGE_CURVE ( 'NONE', #38381, #22501, #165399, .T. ) ;
#18227 = CARTESIAN_POINT ( 'NONE',  ( -3.541704441667874903, 5.155074486744371853, -1.599625672291256295 ) ) ;
#18228 = CARTESIAN_POINT ( 'NONE',  ( -7.009202228140751778, 9.200488570962775725, -1.443375672974058777 ) ) ;
#18229 = CARTESIAN_POINT ( 'NONE',  ( 4.627887939457571598, -1.327398817707679868, -1.706084338546076662 ) ) ;
#18230 = CARTESIAN_POINT ( 'NONE',  ( -0.6823417656250003738, 2.717708333674753618, -1.181850606188749264 ) ) ;
#18231 = CARTESIAN_POINT ( 'NONE',  ( 5.852796007109359877, -1.555770171409420977, 1.210649060634989560 ) ) ;
#18232 = CARTESIAN_POINT ( 'NONE',  ( 4.657415279524609986, -0.3804069660688877974, -1.691394979786196684 ) ) ;
#18234 = CARTESIAN_POINT ( 'NONE',  ( 1.927518781310177509, -1.434474475899261581, -1.656937093973806396 ) ) ;
#18233 = CARTESIAN_POINT ( 'NONE',  ( 0.6801582343749744686, -0.7760416663252778235, 1.178068619123799898 ) ) ;
#18235 = CARTESIAN_POINT ( 'NONE',  ( 1.659631924955577098, -1.980043282969433882, -1.184870857304116898 ) ) ;
#18236 = CARTESIAN_POINT ( 'NONE',  ( 5.307911771147946212, -2.051258671218537444, 0.1976249854395220606 ) ) ;
#18237 = CARTESIAN_POINT ( 'NONE',  ( 0.05839466612742905127, -1.734069842965625385, -0.8743347890363247776 ) ) ;
#18238 = CARTESIAN_POINT ( 'NONE',  ( -7.334597914868741242, 8.619747657844088806, -1.082531754730543083 ) ) ;
#18239 = CARTESIAN_POINT ( 'NONE',  ( -5.679940009482361774, 5.591294530676332641, 0.7998128361456281477 ) ) ;
#18240 = DIRECTION ( 'NONE',  ( 7.387867266669436732E-31, -1.000000000000000000, -8.546850786086424434E-32 ) ) ;
#18241 = CARTESIAN_POINT ( 'NONE',  ( 3.322626870553476941, -0.8629183168706102691, -1.937285153019531414 ) ) ;
#18242 = DIRECTION ( 'NONE',  ( -0.6507913734559641616, -0.7592566023653004592, 0.000000000000000000 ) ) ;
#18243 = CARTESIAN_POINT ( 'NONE',  ( 1.512342498431101134, -1.897697209584522815, 0.6819976561535444626 ) ) ;
#18244 = CARTESIAN_POINT ( 'NONE',  ( -5.856759170979136897, 9.776710099543576504, 0.000000000000000000 ) ) ;
#18245 = CARTESIAN_POINT ( 'NONE',  ( 4.471826267013489620, 2.141383520707430321, -0.5327586567505787629 ) ) ;
#18246 = CARTESIAN_POINT ( 'NONE',  ( -3.285556943750000070, -1.946874999522042682, 0.000000000000000000 ) ) ;
#18247 = CARTESIAN_POINT ( 'NONE',  ( 1.832617572280154539, -1.765004919984759058, -0.5899526775028116621 ) ) ;
#18248 = CARTESIAN_POINT ( 'NONE',  ( -0.02880301295727759683, -0.006976478922920535501, -2.273770288744044521 ) ) ;
#18249 = CARTESIAN_POINT ( 'NONE',  ( 1.355808955840426748E-16, 3.500000000000003109, 2.025000000000006573 ) ) ;
#18250 = CARTESIAN_POINT ( 'NONE',  ( 1.579999999999989413, 6.280000000000042881, -2.499999999999995115 ) ) ;
#18252 = CARTESIAN_POINT ( 'NONE',  ( 6.925078400183578786, 0.5640289027524867382, 2.196098379985710114 ) ) ;
#18251 = CARTESIAN_POINT ( 'NONE',  ( -4.603205931398525408, 8.475712490939976362, -0.2800714110085516517 ) ) ;
#18253 = CARTESIAN_POINT ( 'NONE',  ( 1.452308200714679032, 8.721976639181708180, -2.576600914284014276 ) ) ;
#18254 = ORIENTED_EDGE ( 'NONE', *, *, #21174, .F. ) ;
#18255 = CARTESIAN_POINT ( 'NONE',  ( 3.748945967280458369, -1.685778541264292274, 1.185220002557571206 ) ) ;
#18256 = CARTESIAN_POINT ( 'NONE',  ( 1.360316468749953600, 1.786458333674746601, -0.7853790794159161148 ) ) ;
#18257 = UNCERTAINTY_MEASURE_WITH_UNIT (LENGTH_MEASURE( 1.000000000000000082E-05 ), #42147, 'distance_accuracy_value', 'NONE');
#18258 = CARTESIAN_POINT ( 'NONE',  ( -6.043183783389232566, 8.073467052085995022, 1.599625672291269396 ) ) ;
#18259 = CARTESIAN_POINT ( 'NONE',  ( 2.473312253293189489, -1.758384921082667862, -0.9933899200572825494 ) ) ;
#18260 = CARTESIAN_POINT ( 'NONE',  ( -1.402160292154681736E-14, -1.037499999999977662, 1.732050807568877637 ) ) ;
#18261 = CARTESIAN_POINT ( 'NONE',  ( 2.737856954955798727, 5.281584649835344258, 1.199719254218452047 ) ) ;
#18262 = CARTESIAN_POINT ( 'NONE',  ( 1.498976495884283056, 1.685333290510768744, -1.185852821821014702 ) ) ;
#18264 = CARTESIAN_POINT ( 'NONE',  ( -1.402160292154681736E-14, 13.42187500034140157, 1.575800808251682339 ) ) ;
#18263 = LINE ( 'NONE', #84347, #90355 ) ;
#18265 = CARTESIAN_POINT ( 'NONE',  ( 6.144869935491714230, 8.192100896205568361, -1.599625672291262513 ) ) ;
#18266 = AXIS2_PLACEMENT_3D ( 'NONE', #164196, #60551, #182550 ) ;
#18267 = CARTESIAN_POINT ( 'NONE',  ( -0.1408020194049781904, -0.005144001661201018025, -2.100147592658160089 ) ) ;
#18268 = CARTESIAN_POINT ( 'NONE',  ( 0.9898993202219902310, -0.4452471680344311511, -1.786356756097874587 ) ) ;
#18269 = AXIS2_PLACEMENT_3D ( 'NONE', #199734, #84933, #212789 ) ;
#18270 = CARTESIAN_POINT ( 'NONE',  ( 5.777994779145079640, 1.311685685134782231, 1.774619457157788904 ) ) ;
#18271 = CARTESIAN_POINT ( 'NONE',  ( 5.013482942003290255, 9.071090208970993274, -0.7998128361456481317 ) ) ;
#18272 = CARTESIAN_POINT ( 'NONE',  ( 1.827627302340195437, -2.036028831988645926, 0.7264203155534704193 ) ) ;
#18273 = CARTESIAN_POINT ( 'NONE',  ( -5.097502569058221411, 6.009803087731781623, -1.082531754730544860 ) ) ;
#18274 = CARTESIAN_POINT ( 'NONE',  ( 2.009000277268524481, 0.004839059525654776373, 2.016708403978189956 ) ) ;
#18275 = LINE ( 'NONE', #120136, #687 ) ;
#18276 = CARTESIAN_POINT ( 'NONE',  ( 0.1100172516835694753, 7.047065462479300990, 3.945011421254984718 ) ) ;
#18277 = CARTESIAN_POINT ( 'NONE',  ( 4.891463287051191600, 1.460324016362057886, 1.324601213698357149 ) ) ;
#18278 = CARTESIAN_POINT ( 'NONE',  ( 3.186732694495420848, 1.586669336078951664, -1.244385354607212335 ) ) ;
#18280 = CARTESIAN_POINT ( 'NONE',  ( 10.20892648096591770, 11.01276177065614981, -0.7216878364870257245 ) ) ;
#18279 = CARTESIAN_POINT ( 'NONE',  ( 1.364683531249986537, 1.905208333674750287, -0.7879004041258239610 ) ) ;
#18282 = CARTESIAN_POINT ( 'NONE',  ( 6.639294477394681593, -1.882217795646949687, 0.9450163710809048601 ) ) ;
#18281 = CARTESIAN_POINT ( 'NONE',  ( -8.227100285394159940, 8.492705175914988303, 0.7998128361456602331 ) ) ;
#18283 = CARTESIAN_POINT ( 'NONE',  ( 5.705552448923417508, -1.629793913574303588, -1.276656259598766940 ) ) ;
#18284 = CARTESIAN_POINT ( 'NONE',  ( 6.174848896020108668, 9.291408581077091000, 1.199719254218460707 ) ) ;
#18285 = CARTESIAN_POINT ( 'NONE',  ( -7.877450944739929461, 9.149113176073413456, 1.199719254218462483 ) ) ;
#18286 = CARTESIAN_POINT ( 'NONE',  ( -1.448804818547335449, 8.711467014680348342, 2.592604518246293122 ) ) ;
#18287 = CARTESIAN_POINT ( 'NONE',  ( 5.801037524829370184, -0.3003419868748377630, -1.997221587554024458 ) ) ;
#18288 = CARTESIAN_POINT ( 'NONE',  ( -0.7500000000000006661, -1.110416665983847473, -1.299038105676652011 ) ) ;
#18289 = CARTESIAN_POINT ( 'NONE',  ( 0.7958482667242804398, -1.455889974409400045, -1.461266501696573794 ) ) ;
#18290 = CARTESIAN_POINT ( 'NONE',  ( 7.700668062882064291, 10.00719871149432549, -1.443375672974057666 ) ) ;
#18291 = EDGE_CURVE ( 'NONE', #106, #136049, #85403, .T. ) ;
#18292 = CARTESIAN_POINT ( 'NONE',  ( 7.028976294042106332, 7.165170195996068969, 0.000000000000000000 ) ) ;
#18293 = CARTESIAN_POINT ( 'NONE',  ( 4.875038752565570732, 7.845239757038595663, -1.199719254218452047 ) ) ;
#18294 = CARTESIAN_POINT ( 'NONE',  ( 0.6823417656249882723, 0.7385416670080829915, -1.181850606188749264 ) ) ;
#18296 = CARTESIAN_POINT ( 'NONE',  ( 9.533882584321561993, 4.462909869062322343, -7.287958590253622582 ) ) ;
#18295 = CARTESIAN_POINT ( 'NONE',  ( 4.179656494762836516, 8.098292687190454586, -0.7998128361456362523 ) ) ;
#18297 = CARTESIAN_POINT ( 'NONE',  ( 6.358410854684775515, 8.441231968597481483, -1.443375672974058777 ) ) ;
#18298 = CARTESIAN_POINT ( 'NONE',  ( 2.576841123524225452, 1.419588041764899611, -1.642854796848471244 ) ) ;
#18299 = CARTESIAN_POINT ( 'NONE',  ( -1.848071122224620888, 8.944961669792201420, -0.7749999999999996891 ) ) ;
#18301 = CARTESIAN_POINT ( 'NONE',  ( 2.542321706073047416, -1.529623444112483632, 1.024600984555257277 ) ) ;
#18300 = CARTESIAN_POINT ( 'NONE',  ( -5.273758566035884776, 5.255065869904374409, 0.000000000000000000 ) ) ;
#18302 = CARTESIAN_POINT ( 'NONE',  ( -1.201851678989727383E-14, 3.821875000341423689, 1.575800808251672791 ) ) ;
#18303 = CARTESIAN_POINT ( 'NONE',  ( 4.423480980095358284, -1.348712413769267426, -1.727291790683552541 ) ) ;
#18304 = LINE ( 'NONE', #179773, #32426 ) ;
#18305 = CARTESIAN_POINT ( 'NONE',  ( 4.469752058069711431, 2.195618827641317772, -0.5456854893412068641 ) ) ;
#18306 = CARTESIAN_POINT ( 'NONE',  ( -5.752737250900127997, 5.605948302338584099, 0.000000000000000000 ) ) ;
#18307 = CARTESIAN_POINT ( 'NONE',  ( -6.007394967034264788, 6.077829431587280062, -0.6506939886842719734 ) ) ;
#18308 = CARTESIAN_POINT ( 'NONE',  ( 5.410124943364367667, 7.538760657221164507, -1.247639402986647550 ) ) ;
#18309 = VECTOR ( 'NONE', #20813, 1000.000000000000000 ) ;
#18310 = CARTESIAN_POINT ( 'NONE',  ( -4.462041952228942954, 8.219816354326809460, -0.7216878364870338292 ) ) ;
#18311 = CARTESIAN_POINT ( 'NONE',  ( 4.421367491832268293, 7.211993602896056288, 1.082531754730549078 ) ) ;
#18312 = EDGE_CURVE ( 'NONE', #46131, #158010, #140792, .T. ) ;
#18313 = CARTESIAN_POINT ( 'NONE',  ( 0.1800360811037614583, -1.714963048871451790, -0.4369287763777151556 ) ) ;
#18314 = CARTESIAN_POINT ( 'NONE',  ( 3.615888430654935259, -0.5820857220382947839, 1.927115488332105553 ) ) ;
#18315 = B_SPLINE_CURVE_WITH_KNOTS ( 'NONE', 3,
 ( #411, #131576, #181332, #113216, #179221, #78503, #212760, #130539, #196530, #48173, #81707, #114286, #170409, #119603, #183461, #116395 ),
 .UNSPECIFIED., .F., .F.,
 ( 4, 3, 3, 3, 3, 4 ),
 ( 0.000000000000000000, 3.031394987250921340E-05, 4.925505422167386496E-05, 6.478297760331552379E-05, 8.039662739264234889E-05, 9.445464058994319236E-05 ),
 .UNSPECIFIED. ) ;
#18316 = CARTESIAN_POINT ( 'NONE',  ( 7.633404179693907388, 8.864391950186421454, -1.199719254218441611 ) ) ;
#18317 = CARTESIAN_POINT ( 'NONE',  ( 3.522586592847714471, 1.337535325648725459, -1.626654721158872885 ) ) ;
#18318 = CARTESIAN_POINT ( 'NONE',  ( 0.6849900193761117029, 1.566649212177973149, 1.102054418794357948 ) ) ;
#18320 = CARTESIAN_POINT ( 'NONE',  ( -1.402160292154681736E-14, 2.087500000000021227, -1.732050807568863648 ) ) ;
#18319 = CARTESIAN_POINT ( 'NONE',  ( -1.364683531250010295, 11.88020833367473017, 0.7879004041258445001 ) ) ;
#18321 = CARTESIAN_POINT ( 'NONE',  ( 2.295301284060722313, -1.760697607696968037, 0.8827641120334356328 ) ) ;
#18322 = CARTESIAN_POINT ( 'NONE',  ( 0.8834254411415434216, 1.253375741028007084, 1.388844808110502038 ) ) ;
#18323 = CARTESIAN_POINT ( 'NONE',  ( 0.6253529088778920775, 0.1960189665039281104, -1.952063659030291998 ) ) ;
#18325 = ORIENTED_EDGE ( 'NONE', *, *, #43314, .T. ) ;
#18324 = CARTESIAN_POINT ( 'NONE',  ( 6.451413702892147661, -1.613775625804831693, 0.8233398690262339059 ) ) ;
#18326 = CARTESIAN_POINT ( 'NONE',  ( 6.480434237652124452, 8.583592582059388576, 1.443375672974076540 ) ) ;
#18327 = CARTESIAN_POINT ( 'NONE',  ( 0.6823417656249899377, 0.9052083336747520637, 1.181850606188755259 ) ) ;
#18328 = CARTESIAN_POINT ( 'NONE',  ( 5.541831131927607679, 0.7570117910807551143, -1.710825945835430462 ) ) ;
#18329 = CARTESIAN_POINT ( 'NONE',  ( 10.56588178375152864, 11.22128359066528169, -0.7998128361456281477 ) ) ;
#18330 = CARTESIAN_POINT ( 'NONE',  ( 0.6823417656249899377, 2.842708333674753618, 1.181850606188765695 ) ) ;
#18331 = AXIS2_PLACEMENT_3D ( 'NONE', #204435, #183938, #153590 ) ;
#18332 = CARTESIAN_POINT ( 'NONE',  ( 5.436411051413860385, -1.154718516627372127, 1.718110687276501958 ) ) ;
#18333 = CIRCLE ( 'NONE', #139433, 11.00000000000000000 ) ;
#18334 =( NAMED_UNIT ( * ) SI_UNIT ( $, .STERADIAN. ) SOLID_ANGLE_UNIT ( ) );
#18335 = CARTESIAN_POINT ( 'NONE',  ( -4.462041952228957165, 5.338708711422782471, -1.082531754730549967 ) ) ;
#18336 = FILL_AREA_STYLE ('',( #51930 ) ) ;
#18337 = CARTESIAN_POINT ( 'NONE',  ( 1.499999999999985123, 0.5458333333333577064, -0.8660254037844253849 ) ) ;
#18338 = CARTESIAN_POINT ( 'NONE',  ( 6.100279051144945619, 9.204410428722734849, -1.199719254218440723 ) ) ;
#18339 = CARTESIAN_POINT ( 'NONE',  ( -6.367525699912501835, 10.58053041653993098, -0.7998128361456291469 ) ) ;
#18340 = CARTESIAN_POINT ( 'NONE',  ( 6.017840079619279692, 8.114175741012878973, -1.599625672291281386 ) ) ;
#18341 = EDGE_CURVE ( 'NONE', #183115, #179040, #70, .T. ) ;
#18342 = CARTESIAN_POINT ( 'NONE',  ( 0.6823417656249882723, 0.6760416670080898749, -1.181850606188749264 ) ) ;
#18343 = CARTESIAN_POINT ( 'NONE',  ( -1.500000000000013101, 2.629166666666687746, -0.8660254037844313801 ) ) ;
#18345 = CARTESIAN_POINT ( 'NONE',  ( 3.337278367258157630, 7.045241861776501580, 0.7998128361456341429 ) ) ;
#18344 = CARTESIAN_POINT ( 'NONE',  ( 5.652778587040098834, -0.4750822840141955550, -1.903360745478323679 ) ) ;
#18346 = ADVANCED_FACE ( 'NONE', ( #34725 ), #88979, .T. ) ;
#18347 = CARTESIAN_POINT ( 'NONE',  ( 2.847029653296664353, -1.038834691150035461, 1.727737368502464621 ) ) ;
#18348 = CARTESIAN_POINT ( 'NONE',  ( 2.799894175352398484, -0.9483327596419667271, -1.664474063330185105 ) ) ;
#18349 = CARTESIAN_POINT ( 'NONE',  ( -1.499999999999997780, 4.431250000682819490, 1.214306433183764966E-14 ) ) ;
#18350 = CIRCLE ( 'NONE', #129010, 0.08000000000000020983 ) ;
#18351 = CARTESIAN_POINT ( 'NONE',  ( 0.9607770615731696662, -1.983481723135366304, -0.9323335341336475013 ) ) ;
#18352 = CARTESIAN_POINT ( 'NONE',  ( 0.2335667940003049725, 0.6933325534057503958, -2.235178663643789143 ) ) ;
#18353 = CARTESIAN_POINT ( 'NONE',  ( 3.655401173194738007, 0.4573680094964555076, -1.813624142381641491 ) ) ;
#18354 = CARTESIAN_POINT ( 'NONE',  ( -1.402160292154681736E-14, -1.256249999317182953, 1.732050807568877637 ) ) ;
#18355 = CARTESIAN_POINT ( 'NONE',  ( -6.561256274009600986, 9.742217188731485678, -1.199719254218440723 ) ) ;
#18357 = CARTESIAN_POINT ( 'NONE',  ( 4.165693581912960575, 1.384238758890417031, 1.602101081018918904 ) ) ;
#18356 = CARTESIAN_POINT ( 'NONE',  ( -5.436456409399874623, 5.444880020495701523, 0.000000000000000000 ) ) ;
#18358 = DIRECTION ( 'NONE',  ( -9.577770318032057676E-19, 0.9998511425080263137, 0.01725377713413180428 ) ) ;
#18359 = CARTESIAN_POINT ( 'NONE',  ( 5.723117673755029777, -1.870111591731966616, -0.8886290660751752224 ) ) ;
#18361 = CARTESIAN_POINT ( 'NONE',  ( 6.620655732516659064, 2.000981103421325180, 2.575746817850287140 ) ) ;
#18360 = CARTESIAN_POINT ( 'NONE',  ( 2.261376066768826743, 2.049819659885134371, -0.4107522398083974791 ) ) ;
#18363 = EDGE_LOOP ( 'NONE', ( #199280, #6005, #5034, #141782 ) ) ;
#18362 = CARTESIAN_POINT ( 'NONE',  ( 0.9204217893557011809, 1.591181625417271039, 0.6660807200309772913 ) ) ;
#18364 = CARTESIAN_POINT ( 'NONE',  ( 7.935599982700328958, 8.152621489438862667, 0.7998128361456481317 ) ) ;
#18365 = CIRCLE ( 'NONE', #115391, 0.8300000000000008482 ) ;
#18366 = CARTESIAN_POINT ( 'NONE',  ( 8.937284900545680699, 14.72974997456996604, 8.011501044423479101 ) ) ;
#18367 = CARTESIAN_POINT ( 'NONE',  ( -11.01135777277261951, 13.50625186781170584, 1.399999999999998579 ) ) ;
#18368 = CARTESIAN_POINT ( 'NONE',  ( -9.979842676043658045, 5.589819607760296627, 5.978770845575332338 ) ) ;
#18369 = CARTESIAN_POINT ( 'NONE',  ( 6.548225005276093746, 9.623051025255367819, -1.082531754730537976 ) ) ;
#18370 = FACE_OUTER_BOUND ( 'NONE', #201264, .T. ) ;
#18372 = CARTESIAN_POINT ( 'NONE',  ( 0.1174177504974990710, -0.4853618992130321885, 1.745175170155540245 ) ) ;
#18371 = CARTESIAN_POINT ( 'NONE',  ( 5.657495238652423097, 9.822437888394988548, 0.000000000000000000 ) ) ;
#18373 = CARTESIAN_POINT ( 'NONE',  ( -8.355902744723985975, 8.642974711799791265, 1.040834085586084257E-14 ) ) ;
#18374 = CARTESIAN_POINT ( 'NONE',  ( 5.366329872910639232, 5.155139694684188534, 1.040834085586084257E-14 ) ) ;
#18375 = CARTESIAN_POINT ( 'NONE',  ( -5.615968211774352348, 7.384814024763004525, 1.238619054342107839 ) ) ;
#18376 = CARTESIAN_POINT ( 'NONE',  ( 6.176621499477501054, 9.363752961769195693, -1.199719254218452047 ) ) ;
#18377 = CARTESIAN_POINT ( 'NONE',  ( -11.44779963594995564, 10.89999999999999147, 3.600000000000075140 ) ) ;
#18378 = CARTESIAN_POINT ( 'NONE',  ( 9.571693261567961741, 11.22969222899322617, 1.082531754730548412 ) ) ;
#18379 = EDGE_LOOP ( 'NONE', ( #118238, #22959, #162068, #139156 ) ) ;
#18380 = CARTESIAN_POINT ( 'NONE',  ( 0.2279634046833027561, 1.910523547013969869, 0.1400250592105151126 ) ) ;
#18381 = CARTESIAN_POINT ( 'NONE',  ( 0.4871770963560326240, -1.998059126451703138, -0.7104936405118513765 ) ) ;
#18382 = CARTESIAN_POINT ( 'NONE',  ( -1.930226670627066099, 8.999999999999998224, 0.7750000000000013545 ) ) ;
#18383 = EDGE_CURVE ( 'NONE', #25559, #122127, #16330, .T. ) ;
#18384 = DIRECTION ( 'NONE',  ( 0.000000000000000000, 0.000000000000000000, -1.000000000000000000 ) ) ;
#18385 = CARTESIAN_POINT ( 'NONE',  ( -1.510809298642995957, 8.679800937805021377, -2.538927604451439723 ) ) ;
#18386 = CARTESIAN_POINT ( 'NONE',  ( -4.365362273920257330, 6.116008624372160973, 1.443375672974064550 ) ) ;
#18387 = CARTESIAN_POINT ( 'NONE',  ( 8.270110514656021650, 11.63191745286530576, 1.082531754730557072 ) ) ;
#18388 = CARTESIAN_POINT ( 'NONE',  ( 4.522284192717240359, 0.9245163773116799044, 1.738918859443546516 ) ) ;
#18389 = CARTESIAN_POINT ( 'NONE',  ( 1.102369588802411426, -0.9501182663193027400, 1.895776817140030213 ) ) ;
#18390 = CARTESIAN_POINT ( 'NONE',  ( -6.392833124043511894, 7.417059051927569868, 1.199719254218450271 ) ) ;
#18391 = CARTESIAN_POINT ( 'NONE',  ( -11.77320363351223342, 8.651382856832046997, 2.094678198626021892 ) ) ;
#18392 = CARTESIAN_POINT ( 'NONE',  ( 4.082413651490639062, 7.776916670132135501, 0.000000000000000000 ) ) ;
#18393 = CARTESIAN_POINT ( 'NONE',  ( 6.316381784907312280, 2.043361914081378128, 0.7923855730916644635 ) ) ;
#18394 = CARTESIAN_POINT ( 'NONE',  ( 0.000000000000000000, 3.400000000000000355, 0.000000000000000000 ) ) ;
#18395 = CARTESIAN_POINT ( 'NONE',  ( 4.788067677947292822, -0.9085903742032475083, 1.698673095886160000 ) ) ;
#18396 = CARTESIAN_POINT ( 'NONE',  ( -6.021792782764022078, 10.17717534653336209, -0.7998128361456291469 ) ) ;
#18397 = CARTESIAN_POINT ( 'NONE',  ( -0.1409997244346088141, -0.002808977843308038680, -2.000147647483838220 ) ) ;
#18398 = CARTESIAN_POINT ( 'NONE',  ( 1.295869073816724226, 1.673045085319382119, 1.439284050222865652 ) ) ;
#18399 = PLANE ( 'NONE',  #62028 ) ;
#18400 =( BOUNDED_CURVE ( )  B_SPLINE_CURVE ( 2, ( #34627, #117011, #98578 ),
 .UNSPECIFIED., .F., .T. ) 
 B_SPLINE_CURVE_WITH_KNOTS ( ( 3, 3 ),
 ( 0.000000000000000000, 0.004310887476439823583 ),
 .UNSPECIFIED. ) 
 CURVE ( )  GEOMETRIC_REPRESENTATION_ITEM ( )  RATIONAL_B_SPLINE_CURVE ( ( 1.000000000000000000, 0.9306940709215905105, 0.9330929566528951558 ) ) 
 REPRESENTATION_ITEM ( '' )  );
#18401 = VERTEX_POINT ( 'NONE', #166883 ) ;
#18402 = CARTESIAN_POINT ( 'NONE',  ( 4.312902262922978736, 5.164712407232485702, -1.082531754730548412 ) ) ;
#18403 = ORIENTED_EDGE ( 'NONE', *, *, #91003, .F. ) ;
#18404 = CARTESIAN_POINT ( 'NONE',  ( 6.666861335811934630, 1.461617314166022474, -1.320220550599479070 ) ) ;
#18405 = CARTESIAN_POINT ( 'NONE',  ( 0.4154419552040686248, -1.039972057064937783, -1.639973222157356636 ) ) ;
#18406 = CARTESIAN_POINT ( 'NONE',  ( 6.802148291397191571, -2.057678525504004430, 1.024270743344313672 ) ) ;
#18408 = CARTESIAN_POINT ( 'NONE',  ( 4.856225966575771658, -1.860502807761035715, -0.04838197303517684927 ) ) ;
#18407 = CARTESIAN_POINT ( 'NONE',  ( -5.824109505522200081, 8.952488968821326054, -1.199719254218452047 ) ) ;
#18409 = CARTESIAN_POINT ( 'NONE',  ( 6.339319342841494453, 9.553567112360518365, -1.199719254218452047 ) ) ;
#18410 = DIRECTION ( 'NONE',  ( 1.000000000000000000, 0.000000000000000000, 0.000000000000000000 ) ) ;
#18411 = FACE_OUTER_BOUND ( 'NONE', #115151, .T. ) ;
#18412 = CARTESIAN_POINT ( 'NONE',  ( -5.018489415352746619, 9.006654751220198207, 0.7998128361456481317 ) ) ;
#18413 = CARTESIAN_POINT ( 'NONE',  ( -3.246376473470825363, -0.8887487162375362626, 0.5058895364790267912 ) ) ;
#18414 = CARTESIAN_POINT ( 'NONE',  ( 0.2577194443907256383, 2.166829308800602316, -0.3276212646995610989 ) ) ;
#18415 = ADVANCED_FACE ( 'NONE', ( #165811, #17394 ), #83478, .F. ) ;
#18416 = CARTESIAN_POINT ( 'NONE',  ( 4.012850279964918165, 7.625483060026979842, -0.7216878364870197293 ) ) ;
#18417 = ORIENTED_EDGE ( 'NONE', *, *, #18478, .F. ) ;
#18418 = CARTESIAN_POINT ( 'NONE',  ( 3.649297074908570321E-15, -6.789018801444764277E-15, 0.2598076211376221800 ) ) ;
#18419 = FACE_OUTER_BOUND ( 'NONE', #147294, .T. ) ;
#18420 = CARTESIAN_POINT ( 'NONE',  ( 0.7678472254676466102, 0.8974085622692473674, 1.589837017038860045 ) ) ;
#18421 = CARTESIAN_POINT ( 'NONE',  ( -3.867100128395853709, 5.534702787927018974, -1.599625672291256295 ) ) ;
#18422 = MECHANICAL_DESIGN_GEOMETRIC_PRESENTATION_REPRESENTATION (  '', ( #15000 ), #21955 ) ;
#18423 = CARTESIAN_POINT ( 'NONE',  ( 3.234723362560991244, 1.734343004352358664, -0.003563068559135627086 ) ) ;
#18424 = LINE ( 'NONE', #167886, #192563 ) ;
#18425 = DIRECTION ( 'NONE',  ( -1.000000000000000000, 0.000000000000000000, 0.000000000000000000 ) ) ;
#18426 = CARTESIAN_POINT ( 'NONE',  ( -1.225000000000042277, 0.2291666666666811181, -0.7072540797573237947 ) ) ;
#18427 = AXIS2_PLACEMENT_3D ( 'NONE', #196777, #114532, #65675 ) ;
#18428 = CARTESIAN_POINT ( 'NONE',  ( 6.639283661800273961, -1.628176093627232479, 0.8261057939347238310 ) ) ;
#18429 = CARTESIAN_POINT ( 'NONE',  ( 4.065250617491710905, 1.680331827152386159, 1.012218702928203706 ) ) ;
#18430 = CARTESIAN_POINT ( 'NONE',  ( -8.585337585951595685, 11.03931315507545108, -1.599625672291263179 ) ) ;
#18431 = CARTESIAN_POINT ( 'NONE',  ( 5.829115978871627135, 8.888053511070525659, 1.199719254218462483 ) ) ;
#18432 = CARTESIAN_POINT ( 'NONE',  ( 5.197945112634200449, 1.424400718755761908, 1.570990128125760554 ) ) ;
#18433 = CARTESIAN_POINT ( 'NONE',  ( 7.503511670520385479, 7.718794801887437274, 0.7998128361456281477 ) ) ;
#18434 = CARTESIAN_POINT ( 'NONE',  ( -8.109748439268576803, 12.61312361245537517, 0.7998128361456481317 ) ) ;
#18435 = CARTESIAN_POINT ( 'NONE',  ( -1.115562610750309283E-14, 9.843750000682801371, 1.500000000000001554 ) ) ;
#18436 = CARTESIAN_POINT ( 'NONE',  ( 2.834898843300116766, -1.979765732921334731, -0.6052725283285932401 ) ) ;
#18438 = CARTESIAN_POINT ( 'NONE',  ( -0.6823417656250003738, 0.2802083336747515641, -1.181850606188749264 ) ) ;
#18437 = CARTESIAN_POINT ( 'NONE',  ( 11.86145016429272836, 19.00000000000000000, -1.180000000000002158 ) ) ;
#18439 = EDGE_LOOP ( 'NONE', ( #45940, #191936, #63009, #118299 ) ) ;
#18440 = CARTESIAN_POINT ( 'NONE',  ( 3.182589804937531852, 1.813683736837278460, 1.412227471172630588 ) ) ;
#18441 = CARTESIAN_POINT ( 'NONE',  ( 8.432808358020025707, 9.900993174853955026, 1.082531754730558626 ) ) ;
#18443 = CARTESIAN_POINT ( 'NONE',  ( -3.285556943750000514, -2.938541666188710266, -1.896917185911906500 ) ) ;
#18442 = CARTESIAN_POINT ( 'NONE',  ( 3.902768115887398803, 5.646591783325653147, -1.599625672291269396 ) ) ;
#18444 = CARTESIAN_POINT ( 'NONE',  ( 0.6125000000000071498, 1.583333333333325488, 1.060881119635915359 ) ) ;
#18445 = CARTESIAN_POINT ( 'NONE',  ( 0.000000000000000000, 0.000000000000000000, -6.123233995736775897E-17 ) ) ;
#18446 = VERTEX_POINT ( 'NONE', #85618 ) ;
#18447 = DIRECTION ( 'NONE',  ( 0.000000000000000000, 1.000000000000000000, 0.000000000000000000 ) ) ;
#18448 = CARTESIAN_POINT ( 'NONE',  ( 4.570513122935188299, 0.7371126809179430195, 1.764830652192488580 ) ) ;
#18449 = DIRECTION ( 'NONE',  ( 5.578174157656880098E-15, 1.000000000000000000, -7.437565543542506798E-15 ) ) ;
#18450 = CARTESIAN_POINT ( 'NONE',  ( 5.315364200056264643, -0.2495996188201006494, 1.706489999720143480 ) ) ;
#18451 = CARTESIAN_POINT ( 'NONE',  ( 3.028530041973789277, 0.4946322284519070744, 1.954779462066410956 ) ) ;
#18452 = CARTESIAN_POINT ( 'NONE',  ( 5.186298777384058312, 1.878100352198919465, 1.325219426413627000 ) ) ;
#18453 = CARTESIAN_POINT ( 'NONE',  ( 11.41381675112453387, 10.19999999999998153, 3.704697986577180746 ) ) ;
#18454 = CARTESIAN_POINT ( 'NONE',  ( 0.5048604690408053930, -0.7474223562033958101, -2.076596198196341003 ) ) ;
#18455 = CARTESIAN_POINT ( 'NONE',  ( -5.316205630334263965, 7.295602216847000498, -1.443375672974066548 ) ) ;
#18456 = CARTESIAN_POINT ( 'NONE',  ( 5.817594836490700416, -1.726241941513080747, 0.3891773745644273030 ) ) ;
#18458 = CARTESIAN_POINT ( 'NONE',  ( 2.080407636089614432, -2.248563537884174846, -0.4446712507181517782 ) ) ;
#18457 = CARTESIAN_POINT ( 'NONE',  ( 4.538947565524982686, 8.517465603079630299, 0.000000000000000000 ) ) ;
#18459 = CARTESIAN_POINT ( 'NONE',  ( 0.3568325553494673397, 1.722114113718915984, -0.2502821355834724537 ) ) ;
#18460 = CARTESIAN_POINT ( 'NONE',  ( 0.5727794709109834681, 4.245899076361618008, 0.3117576387476162503 ) ) ;
#18461 = CARTESIAN_POINT ( 'NONE',  ( -3.332271893908731464, 7.109677319527304640, -0.7998128361456481317 ) ) ;
#18462 = CARTESIAN_POINT ( 'NONE',  ( -1.151774525698488676E-14, -0.7656249996585936524, 1.570758158831776052 ) ) ;
#18463 = CARTESIAN_POINT ( 'NONE',  ( 3.963590886093793397, 7.315322400670926761, -0.9154733054410202353 ) ) ;
#18464 = CARTESIAN_POINT ( 'NONE',  ( 0.1862956123577602652, -1.336862347539343965, -1.711682565949741885 ) ) ;
#18465 = CARTESIAN_POINT ( 'NONE',  ( 1.217982839071569012, 0.9896824804975331569, -1.756856037137774162 ) ) ;
#18466 = CARTESIAN_POINT ( 'NONE',  ( 0.7499999999999885647, 0.5979166673494851203, -1.299038105676652899 ) ) ;
#18467 = CARTESIAN_POINT ( 'NONE',  ( 5.162690889178682241, -1.394081347390314640, 1.329872870702011545 ) ) ;
#18468 = CARTESIAN_POINT ( 'NONE',  ( -1.364683531250014514, 11.83854166700806587, -0.7879004041258335089 ) ) ;
#18469 = CARTESIAN_POINT ( 'NONE',  ( 2.637233524875877588, 2.093239256532848369, 0.7440790952397638991 ) ) ;
#18470 = VERTEX_POINT ( 'NONE', #1145 ) ;
#18472 = CARTESIAN_POINT ( 'NONE',  ( -1.203907071533418582, 3.243479746939698316, 0.7750000000000100142 ) ) ;
#18471 = CARTESIAN_POINT ( 'NONE',  ( 1.284279953904119864, 3.046639714193936754, -0.7749999999999910294 ) ) ;
#18473 = DIRECTION ( 'NONE',  ( -0.6483454320283799088, 0.000000000000000000, 0.7613463080411786432 ) ) ;
#18474 = CARTESIAN_POINT ( 'NONE',  ( 10.22692794340986921, 10.82583744360002243, 0.000000000000000000 ) ) ;
#18475 = CARTESIAN_POINT ( 'NONE',  ( 1.500000000000018430, 5.285416667349480235, 0.8660254037844364872 ) ) ;
#18476 = CARTESIAN_POINT ( 'NONE',  ( 4.317713577401066871, 1.066398661528572989, -1.375396103214795218 ) ) ;
#18478 = EDGE_CURVE ( 'NONE', #157271, #9317, #147398, .T. ) ;
#18477 = CARTESIAN_POINT ( 'NONE',  ( 2.400770673373255448, 0.4268909467371252431, 1.914702609522442867 ) ) ;
#18480 = CARTESIAN_POINT ( 'NONE',  ( -7.402388683381436074, 7.738467673474211495, 0.7216878364870317197 ) ) ;
#18479 = CARTESIAN_POINT ( 'NONE',  ( 5.281064527722868718, 6.119995689553514140, 1.199719254218462483 ) ) ;
#18481 = CARTESIAN_POINT ( 'NONE',  ( -5.826669560333386677, 6.051347404617407832, -0.4878656478981869826 ) ) ;
#18482 = CARTESIAN_POINT ( 'NONE',  ( -11.41267819554182950, 3.038492715500534569, 3.708203932499423594 ) ) ;
#18483 = VECTOR ( 'NONE', #54291, 1000.000000000000000 ) ;
#18484 = CIRCLE ( 'NONE', #184541, 12.00000000000000178 ) ;
#18485 = CARTESIAN_POINT ( 'NONE',  ( 0.4673242579315056155, 1.793762616230053508, 1.018268840648499207 ) ) ;
#18486 = CARTESIAN_POINT ( 'NONE',  ( -6.723954117373590833, 9.932031339322813679, -1.199719254218440723 ) ) ;
#18487 = CARTESIAN_POINT ( 'NONE',  ( -5.233084104750526322, 5.207612331738130429, 0.000000000000000000 ) ) ;
#18488 = CARTESIAN_POINT ( 'NONE',  ( 1.042281785820580176, 0.9147803334835495903, -2.069518175336809929 ) ) ;
#18489 = ORIENTED_EDGE ( 'NONE', *, *, #125962, .F. ) ;
#18490 = CARTESIAN_POINT ( 'NONE',  ( -1.500000000000013101, 0.4520833340161533598, 0.8660254037844403729 ) ) ;
#18491 = CARTESIAN_POINT ( 'NONE',  ( 2.688565094423268853, -0.3157439183511835945, -1.843535313746543336 ) ) ;
#18492 = CARTESIAN_POINT ( 'NONE',  ( 0.9142546942676577082, -1.099255453910731983, -1.341178637715144673 ) ) ;
#18493 = AXIS2_PLACEMENT_3D ( 'NONE', #159435, #40374, #173591 ) ;
#18494 = CARTESIAN_POINT ( 'NONE',  ( 5.021103811603734535, -2.081066139062941023, 0.6872292908843835590 ) ) ;
#18495 = CARTESIAN_POINT ( 'NONE',  ( 5.403480793235289070, 1.882684667239397758, 1.334102933689439663 ) ) ;
#18496 = CARTESIAN_POINT ( 'NONE',  ( 1.815377929200719720, -0.2531822047686766441, 2.045215655110666830 ) ) ;
#18497 = CARTESIAN_POINT ( 'NONE',  ( 3.117060223387691398, -1.871409496450952226, 0.5184039432134399661 ) ) ;
#18498 = CARTESIAN_POINT ( 'NONE',  ( -5.056828107772866510, 5.962349549565537643, -1.082531754730543971 ) ) ;
#18499 = CARTESIAN_POINT ( 'NONE',  ( 5.536355731483205922, 1.842701317132239724, 0.3206550288221421963 ) ) ;
#18500 = CARTESIAN_POINT ( 'NONE',  ( 1.593750000000000666, -1.895863743164122983, -0.7852924748298991675 ) ) ;
#18501 = CARTESIAN_POINT ( 'NONE',  ( 4.018854549923576158, 7.569224129587659888, 0.3183394790292719545 ) ) ;
#18502 = CARTESIAN_POINT ( 'NONE',  ( 0.1922019376490837483, -1.058930769078871403, -1.372993611190379104 ) ) ;
#18503 = ADVANCED_FACE ( 'NONE', ( #135452 ), #53118, .F. ) ;
#18504 = CARTESIAN_POINT ( 'NONE',  ( -1.360316468750042862, 1.869791667008058544, -0.7853790794158961308 ) ) ;
#18506 = CARTESIAN_POINT ( 'NONE',  ( 4.254529844270301453, 1.955172953530256219, -0.4926405443339901269 ) ) ;
#18505 = AXIS2_PLACEMENT_3D ( 'NONE', #212000, #128727, #63640 ) ;
#18507 = CARTESIAN_POINT ( 'NONE',  ( -3.253593677155282471, 6.739683690082376444, 1.040834085586084257E-14 ) ) ;
#18508 = CARTESIAN_POINT ( 'NONE',  ( 8.910733272679570049, 11.41894145625809820, -1.599625672291255185 ) ) ;
#18509 = CARTESIAN_POINT ( 'NONE',  ( 3.691562964670865199, 7.528850235416478576, -0.7998128361456362523 ) ) ;
#18511 = CARTESIAN_POINT ( 'NONE',  ( -0.1021852871783679312, 7.053056311350174745, -4.037408415133499240 ) ) ;
#18510 = CARTESIAN_POINT ( 'NONE',  ( 1.857752496991037061, 1.820901040755190214, -0.1330985588276211995 ) ) ;
#18512 = CARTESIAN_POINT ( 'NONE',  ( -6.459533842268148973, 6.500820668926428958, 0.000000000000000000 ) ) ;
#18513 = CARTESIAN_POINT ( 'NONE',  ( 11.41267819554178864, 3.038492715500545227, -3.708203932499494204 ) ) ;
#18514 = CARTESIAN_POINT ( 'NONE',  ( -10.19097401674926395, 4.476076320095182304, 5.708917106338025960 ) ) ;
#18515 = ORIENTED_EDGE ( 'NONE', *, *, #29848, .T. ) ;
#18516 = CARTESIAN_POINT ( 'NONE',  ( -5.817857313595549584, 6.920493299683823096, 1.082531754730549078 ) ) ;
#18517 = DIRECTION ( 'NONE',  ( 0.000000000000000000, 0.000000000000000000, 1.000000000000000000 ) ) ;
#18518 = CARTESIAN_POINT ( 'NONE',  ( -8.971744963941075568, 11.49012176272984931, 1.599625672291269396 ) ) ;
#18519 = CARTESIAN_POINT ( 'NONE',  ( 0.1057309665696047341, 1.499486454312322525, 1.353398366655131246 ) ) ;
#18521 = VERTEX_POINT ( 'NONE', #86686 ) ;
#18520 = CARTESIAN_POINT ( 'NONE',  ( 0.5750489506927083383, -1.533040007955801531, 1.465245631482835043 ) ) ;
#18522 = CARTESIAN_POINT ( 'NONE',  ( -7.449279056065764237, 7.655523418356991350, 0.7998128361456341429 ) ) ;
#18523 = CARTESIAN_POINT ( 'NONE',  ( 5.301401758143367893, 6.143722458377430584, 1.199719254218462483 ) ) ;
#18524 = CARTESIAN_POINT ( 'NONE',  ( 4.944241404475337553, 2.055231674695843669, 0.1536075889326995458 ) ) ;
#18525 = CARTESIAN_POINT ( 'NONE',  ( 5.520157785563180930, -1.821743191724470634, 0.8647220171385737730 ) ) ;
#18526 = VERTEX_POINT ( 'NONE', #152754 ) ;
#18527 = EDGE_LOOP ( 'NONE', ( #115810, #120348, #16272, #37605, #57249, #150496 ) ) ;
#18528 = CARTESIAN_POINT ( 'NONE',  ( 4.749309608864116683, 4.887773556708002509, -0.7920672577798372194 ) ) ;
#18529 = CARTESIAN_POINT ( 'NONE',  ( 1.394453263437886604E-15, -1.268749999044084253, 3.474999999999999645 ) ) ;
#18531 = VERTEX_POINT ( 'NONE', #126474 ) ;
#18530 = CARTESIAN_POINT ( 'NONE',  ( -7.117104292530948229, 7.267986194233038155, -0.7998128361456362523 ) ) ;
#18532 = CARTESIAN_POINT ( 'NONE',  ( 4.601164721245145195, 8.482418317249249995, 0.1585857521721554253 ) ) ;
#18533 = CARTESIAN_POINT ( 'NONE',  ( 4.745470142856022200, -1.954873481938533608, -0.4925652823710227612 ) ) ;
#18534 = CARTESIAN_POINT ( 'NONE',  ( 4.488128036367874607, -0.4058819498431766037, -1.795677737744493019 ) ) ;
#18535 = CARTESIAN_POINT ( 'NONE',  ( 0.07661050522433666965, 0.7707917844542893082, -1.796988219766264550 ) ) ;
#18536 = CARTESIAN_POINT ( 'NONE',  ( 2.122082200655984074, -2.237848761721575208, 0.5630162806932179631 ) ) ;
#18537 = CARTESIAN_POINT ( 'NONE',  ( 5.885121196783658526, 9.023669275293071834, 1.199719254218452047 ) ) ;
#18538 = CARTESIAN_POINT ( 'NONE',  ( 5.255217470067075070, -1.823004960263453489, -1.161262906855420329 ) ) ;
#18539 = CARTESIAN_POINT ( 'NONE',  ( 7.609150525767641504, 9.900428251527500834, -1.599625672291262513 ) ) ;
#18540 = CARTESIAN_POINT ( 'NONE',  ( 0.2748124788713289246, 1.811699325429259488, -0.6999492020843509632 ) ) ;
#18541 = CARTESIAN_POINT ( 'NONE',  ( -4.086893239515592136, 6.855460315155083251, 1.199719254218464037 ) ) ;
#18542 = CARTESIAN_POINT ( 'NONE',  ( 3.884340333706528092, -0.1737987063687232436, 2.291882653078499477 ) ) ;
#18543 = CARTESIAN_POINT ( 'NONE',  ( -9.380156870149196635, 15.46908192400845827, -7.484187822904944554 ) ) ;
#18544 = CARTESIAN_POINT ( 'NONE',  ( -6.154475385960665790, 6.144919136567696505, 0.000000000000000000 ) ) ;
#18545 = CARTESIAN_POINT ( 'NONE',  ( 3.678450976403758066, -1.802590750232490491, -0.4997190347926713794 ) ) ;
#18548 = CARTESIAN_POINT ( 'NONE',  ( -6.394605727500880299, 7.489403432619674561, -1.199719254218452047 ) ) ;
#18547 = CARTESIAN_POINT ( 'NONE',  ( -1.402160292154681736E-14, -0.7562499993171803991, 1.732050807568877637 ) ) ;
#18546 = CARTESIAN_POINT ( 'NONE',  ( 0.8086807686161383568, -0.4671638426185490967, -1.854305266343849734 ) ) ;
#18549 = CARTESIAN_POINT ( 'NONE',  ( 2.789901687333019797, 1.561178712900921584, 1.560079944692857046 ) ) ;
#18550 = CARTESIAN_POINT ( 'NONE',  ( -11.97929049433705373, 9.719999999999998863, 0.7046979865771783036 ) ) ;
#18551 = CARTESIAN_POINT ( 'NONE',  ( 5.366329872910639232, 5.155139694684188534, 1.040834085586084257E-14 ) ) ;
#18552 = CARTESIAN_POINT ( 'NONE',  ( 7.471952054462754234, 8.850270497362297206, 1.082531754730549078 ) ) ;
#18553 = CARTESIAN_POINT ( 'NONE',  ( -5.122283107864663343, 4.870418468797203637, 0.000000000000000000 ) ) ;
#18554 = CARTESIAN_POINT ( 'NONE',  ( -8.041394506236766659, 8.554250810130591631, -0.7216878364870338292 ) ) ;
#18555 = CARTESIAN_POINT ( 'NONE',  ( 6.825078400183526739, -0.0002198122173602961866, 1.955566246027613531 ) ) ;
#18556 = CARTESIAN_POINT ( 'NONE',  ( 0.4293363604773897113, 2.209526777583595170, 0.6654907822973181730 ) ) ;
#18557 = CARTESIAN_POINT ( 'NONE',  ( 1.082386330805637398, 1.171445227557347923, -1.573568114121715933 ) ) ;
#18558 = CARTESIAN_POINT ( 'NONE',  ( 3.959878945198321620, -0.6033026367360559972, 1.972334540003743530 ) ) ;
#18559 = CARTESIAN_POINT ( 'NONE',  ( 5.666945020832170776, 7.634521829102760115, 1.443375672974062551 ) ) ;
#18560 = EDGE_CURVE ( 'NONE', #18526, #210539, #142283, .T. ) ;
#18561 = CARTESIAN_POINT ( 'NONE',  ( 4.681308178468477799, 8.683552984847038303, 0.000000000000000000 ) ) ;
#18562 = ORIENTED_EDGE ( 'NONE', *, *, #16828, .T. ) ;
#18563 = CARTESIAN_POINT ( 'NONE',  ( 8.256552360598020002, 8.734991963560254646, -0.7216878364870267237 ) ) ;
#18564 = CARTESIAN_POINT ( 'NONE',  ( 0.6823417656249917140, 4.155208333674755394, 1.181850606188765695 ) ) ;
#18565 = CARTESIAN_POINT ( 'NONE',  ( 0.000000000000000000, 3.481548657788671619, 0.000000000000000000 ) ) ;
#18566 = CARTESIAN_POINT ( 'NONE',  ( 3.172244755473273781, 6.644776614786712443, 0.000000000000000000 ) ) ;
#18567 = CARTESIAN_POINT ( 'NONE',  ( 6.074718851800529507, 1.462630930118626660, -1.604749943717192373 ) ) ;
#18569 = DIRECTION ( 'NONE',  ( 0.000000000000000000, 0.000000000000000000, 1.000000000000000000 ) ) ;
#18568 = CARTESIAN_POINT ( 'NONE',  ( 9.483599735403714703, -9.201296717416477478, -0.5591315121169913027 ) ) ;
#18570 = CARTESIAN_POINT ( 'NONE',  ( 5.583956936972517937, 6.169539715420659931, -0.8775874851904285068 ) ) ;
#18571 = DIRECTION ( 'NONE',  ( 0.5994789404140892231, -9.687429098727955365E-15, 0.8003905296791066215 ) ) ;
#18572 = CARTESIAN_POINT ( 'NONE',  ( 1.598681293450100904, 1.532267803987485077, -1.072633048482305007 ) ) ;
#18573 = CARTESIAN_POINT ( 'NONE',  ( -5.998154408198820953, 6.083692137903044639, 0.6724663025347333845 ) ) ;
#18574 = CARTESIAN_POINT ( 'NONE',  ( -10.90726532705803820, -6.287979527546282199, 0.008173644115966051740 ) ) ;
#18575 = CARTESIAN_POINT ( 'NONE',  ( 5.316739912341137853, 7.735632174496787528, -1.307268462668280673 ) ) ;
#18576 = CARTESIAN_POINT ( 'NONE',  ( 0.6823417656249899377, 4.738541667008086655, -1.181850606188754593 ) ) ;
#18577 = CARTESIAN_POINT ( 'NONE',  ( 0.8735180803765253410, 0.3724630581584260636, -1.875478908130092215 ) ) ;
#18578 = AXIS2_PLACEMENT_3D ( 'NONE', #90085, #109592, #188628 ) ;
#18579 = CARTESIAN_POINT ( 'NONE',  ( 3.045496301383675330, 0.6385914081092295413, -1.650799995714345325 ) ) ;
#18580 = CARTESIAN_POINT ( 'NONE',  ( 0.2582720099171370021, 1.907150531373353664, 0.1405958444523764117 ) ) ;
#18582 = CARTESIAN_POINT ( 'NONE',  ( 4.446842608676645270, -1.712983832262956696, -0.8575701973691277624 ) ) ;
#18581 = DIRECTION ( 'NONE',  ( 0.000000000000000000, 0.000000000000000000, 1.000000000000000000 ) ) ;
#18583 = CARTESIAN_POINT ( 'NONE',  ( -2.974907306228248061, 6.692710208982554754, 0.008677196802416714538 ) ) ;
#18584 = CARTESIAN_POINT ( 'NONE',  ( 5.881302004902690506, -0.04997076178031189392, 1.969097942535046331 ) ) ;
#18585 = CARTESIAN_POINT ( 'NONE',  ( 0.6332531790259123827, 1.961634380476449335, 0.8060562103610890983 ) ) ;
#18586 = CARTESIAN_POINT ( 'NONE',  ( 2.393657244693859543, -0.2279079664470242961, -0.4206872822309609128 ) ) ;
#18587 = CARTESIAN_POINT ( 'NONE',  ( 4.205816867194319464, -1.865656749788859647, 0.1373567816406878750 ) ) ;
#18589 = ORIENTED_EDGE ( 'NONE', *, *, #125125, .F. ) ;
#18588 = CARTESIAN_POINT ( 'NONE',  ( 0.8733498553583609603, 1.760202786292342170, -0.4843115980177821744 ) ) ;
#18591 = CARTESIAN_POINT ( 'NONE',  ( 4.743613802917549194, 8.193193991156523026, -0.7244234545457691743 ) ) ;
#18590 = CARTESIAN_POINT ( 'NONE',  ( 3.563272299071856164, -1.946135509614330239, -1.040604674307284316 ) ) ;
#18592 = CARTESIAN_POINT ( 'NONE',  ( -1.364683531250010295, 4.342708333674753618, 0.7879004041258379498 ) ) ;
#18593 = CARTESIAN_POINT ( 'NONE',  ( 0.9419289695592079070, 1.383825781391546883, 1.529776408950918265 ) ) ;
#18594 = CARTESIAN_POINT ( 'NONE',  ( 7.949158136313996259, 8.168439335321471262, 1.040834085586084257E-14 ) ) ;
#18595 = CARTESIAN_POINT ( 'NONE',  ( -10.15235809853472126, 10.73883929124566983, -0.7998128361456291469 ) ) ;
#18596 = CARTESIAN_POINT ( 'NONE',  ( 1.445377862185226014, 8.715816065047345518, 2.588769565374623660 ) ) ;
#18597 = CARTESIAN_POINT ( 'NONE',  ( -3.424195918967509300, -0.02093306995252190369, -0.4190893571287980235 ) ) ;
#18598 = CIRCLE ( 'NONE', #188047, 8.500000000000000000 ) ;
#18599 = CARTESIAN_POINT ( 'NONE',  ( 6.831329296439236032, 9.063246493969506545, -1.599625672291267398 ) ) ;
#18600 = EDGE_LOOP ( 'NONE', ( #207545, #73144, #119964, #103176 ) ) ;
#18601 = CARTESIAN_POINT ( 'NONE',  ( 2.699741690289765295, -1.532448122638006671, -1.392287113214360827 ) ) ;
#18602 = CARTESIAN_POINT ( 'NONE',  ( -1.201851678989727383E-14, 3.837500000000021227, -1.732050807568863648 ) ) ;
#18603 = CARTESIAN_POINT ( 'NONE',  ( 1.054251131370760319, 2.159144779032458050, -0.1049546803274861440 ) ) ;
#18604 = CARTESIAN_POINT ( 'NONE',  ( -6.405493493895330737, 6.819705373682535487, -0.5214928506756879578 ) ) ;
#18605 = CARTESIAN_POINT ( 'NONE',  ( 1.875654870896212190, 0.3429857902390308078, -1.990162865174507800 ) ) ;
#18606 = CYLINDRICAL_SURFACE ( 'NONE', #160072, 1.500000000000000222 ) ;
#18607 = EDGE_CURVE ( 'NONE', #59046, #140877, #213402, .T. ) ;
#18609 = CARTESIAN_POINT ( 'NONE',  ( 9.246297574839983824, 9.889694713509232571, 0.7216878364870438212 ) ) ;
#18608 = CARTESIAN_POINT ( 'NONE',  ( 2.665787487727776295, -3.982249430249628297, -2.473491247225932721 ) ) ;
#18610 = CARTESIAN_POINT ( 'NONE',  ( 6.415388720371407949, 0.6297814698452592896, 1.915305867393565897 ) ) ;
#18611 = CARTESIAN_POINT ( 'NONE',  ( 0.7609543035823238544, -0.05432987398422234326, -2.015980609757315190 ) ) ;
#18612 = DIRECTION ( 'NONE',  ( 0.000000000000000000, 0.000000000000000000, 1.000000000000000000 ) ) ;
#18613 = CARTESIAN_POINT ( 'NONE',  ( 5.355090213057959403, 0.4282289882464126451, -2.149144931432686256 ) ) ;
#18614 = CARTESIAN_POINT ( 'NONE',  ( -1.500000000000011324, 3.202083334016150307, 0.8660254037844403729 ) ) ;
#18615 = CARTESIAN_POINT ( 'NONE',  ( 3.164218664783400747, 1.912571728330178855, -0.004505864839042527346 ) ) ;
#18616 = CARTESIAN_POINT ( 'NONE',  ( -5.752737250900127997, 5.605948302338584099, 0.000000000000000000 ) ) ;
#18617 = EDGE_CURVE ( 'NONE', #212186, #201589, #173103, .T. ) ;
#18618 = CARTESIAN_POINT ( 'NONE',  ( 4.975479186090860928, 4.907073259968533385, 0.7216878364870317197 ) ) ;
#18620 = CARTESIAN_POINT ( 'NONE',  ( 1.300407892936685572, 1.352140309104767013, -1.496066053310755262 ) ) ;
#18619 = CARTESIAN_POINT ( 'NONE',  ( -5.346851039111044201, 6.199209027673978412, 7.500000000000000000 ) ) ;
#18621 = CARTESIAN_POINT ( 'NONE',  ( -1.402160292154681736E-14, 11.73437500034140335, 1.575800808251682339 ) ) ;
#18623 = CARTESIAN_POINT ( 'NONE',  ( -3.983063267364693960, 7.868933921892603323, -0.7998128361456481317 ) ) ;
#18622 = CARTESIAN_POINT ( 'NONE',  ( 0.1876184131640425135, 1.704306722208508873, 1.533282888375518960 ) ) ;
#18624 = CARTESIAN_POINT ( 'NONE',  ( 4.366008003732903653, 0.8140541678068600184, 1.520548270592293028 ) ) ;
#18625 = CARTESIAN_POINT ( 'NONE',  ( -0.1405533004718494683, 0.2440837993472090295, -1.754028569132993542 ) ) ;
#18626 = CARTESIAN_POINT ( 'NONE',  ( 3.388648328411762556, 6.040841252200647382, 1.199719254218462483 ) ) ;
#18627 = CARTESIAN_POINT ( 'NONE',  ( 4.137366913483981889, 8.820714063342464328, -0.7750000000000000222 ) ) ;
#18628 = CARTESIAN_POINT ( 'NONE',  ( 1.574581288703358339, 1.320057194528483135, -1.451483715152704246 ) ) ;
#18629 = DIRECTION ( 'NONE',  ( 1.000000000000000000, -8.267061968666011278E-31, -1.224646799147343593E-16 ) ) ;
#18630 = CARTESIAN_POINT ( 'NONE',  ( 6.017121246366603060, 5.914396297049491658, 1.040834085586084257E-14 ) ) ;
#18631 = CARTESIAN_POINT ( 'NONE',  ( 0.1755611466353447780, 0.6788741266964171128, -2.325051092042058620 ) ) ;
#18632 = CARTESIAN_POINT ( 'NONE',  ( 7.334597915313080918, 9.580116872663850813, 1.040834085586084257E-14 ) ) ;
#18633 = VERTEX_POINT ( 'NONE', #208686 ) ;
#18634 = CARTESIAN_POINT ( 'NONE',  ( 4.160681542540445754, 0.4872625442002316287, 1.744618836514327587 ) ) ;
#18635 = ORIENTED_EDGE ( 'NONE', *, *, #167207, .T. ) ;
#18636 = CARTESIAN_POINT ( 'NONE',  ( 5.020262018810099924, 9.078999131912302900, 0.7998128361456331437 ) ) ;
#18637 = DIRECTION ( 'NONE',  ( 0.000000000000000000, 1.000000000000000000, 0.000000000000000000 ) ) ;
#18638 = CARTESIAN_POINT ( 'NONE',  ( 5.039644362999008642, -1.718302384056184851, 0.5736564087924463928 ) ) ;
#18639 = CARTESIAN_POINT ( 'NONE',  ( 6.495764994278797388, 8.671754808115688107, 1.443375672974063439 ) ) ;
#18640 = PRESENTATION_STYLE_ASSIGNMENT (( #84719 ) ) ;
#18641 = CARTESIAN_POINT ( 'NONE',  ( 4.731797659388218946, 6.802130194288283249, -1.238660871931380303 ) ) ;
#18643 = CARTESIAN_POINT ( 'NONE',  ( 8.204655514564224816, 12.72384853363364066, 1.040834085586084257E-14 ) ) ;
#18642 = CARTESIAN_POINT ( 'NONE',  ( 5.881279174647062291, -0.04503291608629880066, 1.860690090596372137 ) ) ;
#18644 = CARTESIAN_POINT ( 'NONE',  ( 3.778834734487185099, 1.616410871901182711, -1.027684692424314594 ) ) ;
#18645 = AXIS2_PLACEMENT_3D ( 'NONE', #138656, #190572, #90978 ) ;
#18646 = CARTESIAN_POINT ( 'NONE',  ( 5.289089323106923146, 6.303597310780433283, -1.082531754730548412 ) ) ;
#18647 = CARTESIAN_POINT ( 'NONE',  ( -11.83627402213341107, 4.942735150756283780, -4.855302456647772935 ) ) ;
#18648 = ADVANCED_FACE ( 'NONE', ( #190306 ), #9437, .F. ) ;
#18649 = CARTESIAN_POINT ( 'NONE',  ( 4.839897650398541806, 8.590371658866210680, 1.040834085586084257E-14 ) ) ;
#18650 = B_SPLINE_CURVE_WITH_KNOTS ( 'NONE', 3,
 ( #152052, #185594, #186666, #4686 ),
 .UNSPECIFIED., .F., .F.,
 ( 4, 4 ),
 ( 0.000000000000000000, 0.0004044236633723155756 ),
 .UNSPECIFIED. ) ;
#18651 = CARTESIAN_POINT ( 'NONE',  ( -9.978437869977950569, 11.70422760547153906, -1.082531754730539753 ) ) ;
#18652 = CARTESIAN_POINT ( 'NONE',  ( 0.6378455412261313517, -1.529572671500577297, -1.527792216034072670 ) ) ;
#18653 = CARTESIAN_POINT ( 'NONE',  ( -4.437261413422502798, 8.398831758960053406, 0.000000000000000000 ) ) ;
#18654 = CARTESIAN_POINT ( 'NONE',  ( 5.041653019435334393, 6.975290837464928728, -1.599625672291269396 ) ) ;
#18655 = CARTESIAN_POINT ( 'NONE',  ( 0.4459769555512117511, 1.820297760642339391, 0.1397589855641478973 ) ) ;
#18656 = CARTESIAN_POINT ( 'NONE',  ( -5.915435094264120508, 5.795762452929912101, 0.000000000000000000 ) ) ;
#18657 = CARTESIAN_POINT ( 'NONE',  ( 3.979382468966369935, 1.719079831940514502, -0.6148086763930470378 ) ) ;
#18658 = CARTESIAN_POINT ( 'NONE',  ( 9.897453898556438645, 12.56651866558563313, 7.888353118025118071 ) ) ;
#18659 = CARTESIAN_POINT ( 'NONE',  ( 2.285291272251275707, 0.09004542135446562401, -1.910373438827176251 ) ) ;
#18660 = VERTEX_POINT ( 'NONE', #111278 ) ;
#18661 = CARTESIAN_POINT ( 'NONE',  ( 2.154690271565715687, -0.5224902820043091367, -1.898924457017936662 ) ) ;
#18662 = CARTESIAN_POINT ( 'NONE',  ( 4.774914120469089696, 1.810774457899359202, -0.7023516835302608952 ) ) ;
#18663 = CARTESIAN_POINT ( 'NONE',  ( -7.370792787684826486, 8.628288336167626582, -1.199719254218452047 ) ) ;
#18665 = CARTESIAN_POINT ( 'NONE',  ( 4.324552338190708056, -0.9094542848507057853, -1.915842285305848769 ) ) ;
#18664 = CARTESIAN_POINT ( 'NONE',  ( 7.289443866002793371, 8.533381260871966134, 1.199719254218452047 ) ) ;
#18666 = CARTESIAN_POINT ( 'NONE',  ( 6.776593369755653740, -7.026643280347737885, 6.796618584847460731 ) ) ;
#18667 = CARTESIAN_POINT ( 'NONE',  ( 8.289920859751990889, 11.75899253876431416, 1.199719254218450271 ) ) ;
#18668 = CARTESIAN_POINT ( 'NONE',  ( 6.025359521845701671, 6.071890788804434891, 0.5399204162177869692 ) ) ;
#18669 = CARTESIAN_POINT ( 'NONE',  ( -1.115562610750309283E-14, 8.343750000682796042, 1.500000000000001554 ) ) ;
#18670 = EDGE_LOOP ( 'NONE', ( #43333, #56028, #35683, #20544 ) ) ;
#18671 = CARTESIAN_POINT ( 'NONE',  ( 0.6823417656249969321, 13.02604166700806232, -1.181850606188757036 ) ) ;
#18672 = CARTESIAN_POINT ( 'NONE',  ( 3.379725431556547477, 7.165039780116438273, -1.734723475976807094E-15 ) ) ;
#18673 = CARTESIAN_POINT ( 'NONE',  ( 3.499976210622149253, 7.235056012367825140, 0.7998128361456321445 ) ) ;
#18674 = CARTESIAN_POINT ( 'NONE',  ( 5.224688093219824303, 7.188831756880171397, -1.599625672291283607 ) ) ;
#18675 = CARTESIAN_POINT ( 'NONE',  ( 11.96533679318060095, 12.34753988812994763, -0.9151144679398871551 ) ) ;
#18676 = CARTESIAN_POINT ( 'NONE',  ( 5.443921307256319508, 0.7362202147598860824, -1.670853202368662860 ) ) ;
#18677 = CARTESIAN_POINT ( 'NONE',  ( 0.2212536527127808295, -1.848710500310095872, -0.9322282823912150240 ) ) ;
#18678 = CARTESIAN_POINT ( 'NONE',  ( -7.361714222540411967, 11.53249099303175385, 0.000000000000000000 ) ) ;
#18679 = CARTESIAN_POINT ( 'NONE',  ( -4.912146588114373991, 8.123387011080156483, 1.048141424314027237 ) ) ;
#18680 = CARTESIAN_POINT ( 'NONE',  ( 6.925078400183546812, 3.702220002068328242, 2.370079373711677206 ) ) ;
#18681 = CARTESIAN_POINT ( 'NONE',  ( 5.805500895539822181, -0.4530025297027094888, 1.814837910242727226 ) ) ;
#18682 = CARTESIAN_POINT ( 'NONE',  ( 5.940443861082012944, 10.08226827123770697, 0.7998128361456462443 ) ) ;
#18683 = CARTESIAN_POINT ( 'NONE',  ( 3.527879399192564325, -1.148099800794393444, -1.546878348965428973 ) ) ;
#18684 = CARTESIAN_POINT ( 'NONE',  ( 0.6823417656249934904, 9.505208333674728394, 1.181850606188764807 ) ) ;
#18685 = CARTESIAN_POINT ( 'NONE',  ( -5.708146366553361162, 6.618257834855742594, -1.199719254218446718 ) ) ;
#18686 = CARTESIAN_POINT ( 'NONE',  ( 2.347533153460546806, 5.890539112345938300, 0.000000000000000000 ) ) ;
#18687 = CARTESIAN_POINT ( 'NONE',  ( -8.093291352714894415, 8.406871097780989288, -0.7998128361456362523 ) ) ;
#18688 = CARTESIAN_POINT ( 'NONE',  ( 1.265409400557556907, 1.954659568096604350, -0.8140754496198910894 ) ) ;
#18689 = VECTOR ( 'NONE', #44044, 1000.000000000000000 ) ;
#18690 = CARTESIAN_POINT ( 'NONE',  ( 7.391166297744269365, 11.77477778067701664, 1.040834085586084257E-14 ) ) ;
#18691 = CARTESIAN_POINT ( 'NONE',  ( -4.010620668045727477, 3.846206254399771929, 2.500000000000000444 ) ) ;
#18692 = CARTESIAN_POINT ( 'NONE',  ( 6.192251260771239885, 1.025525066348543568, -1.798363755310352197 ) ) ;
#18694 = CARTESIAN_POINT ( 'NONE',  ( 4.007117460063951420, 7.817974094756804604, -0.2064290434495383852 ) ) ;
#18693 = CARTESIAN_POINT ( 'NONE',  ( 2.050122339901743196, -1.422379512129726908, 1.169167124061460949 ) ) ;
#18695 = CARTESIAN_POINT ( 'NONE',  ( 4.839897650398541806, 8.590371658866210680, 1.040834085586084257E-14 ) ) ;
#18697 = CARTESIAN_POINT ( 'NONE',  ( 0.4267829560204765005, 6.608306969908364081, 3.280653110164307495 ) ) ;
#18696 = CARTESIAN_POINT ( 'NONE',  ( 4.923019175537949543, 4.916146257648610352, 0.000000000000000000 ) ) ;
#18698 = CARTESIAN_POINT ( 'NONE',  ( 1.799181239640806007, 1.907565883177517740, 1.270813247315852879 ) ) ;
#18699 = CARTESIAN_POINT ( 'NONE',  ( -0.02319159430949970652, 0.003959926571647092407, -1.810968101872318714 ) ) ;
#18700 = ORIENTED_EDGE ( 'NONE', *, *, #181594, .F. ) ;
#18701 = CARTESIAN_POINT ( 'NONE',  ( 7.524412065460039933, 10.76193592880331984, -1.082531754730537976 ) ) ;
#18702 = CARTESIAN_POINT ( 'NONE',  ( 1.160403428290600392, 2.011073784072180182, 0.09471770850632241223 ) ) ;
#18703 = CARTESIAN_POINT ( 'NONE',  ( 1.463640819124707004, -0.4818986642843925972, 1.901505326443528876 ) ) ;
#18704 = CARTESIAN_POINT ( 'NONE',  ( -11.04536101718726293, 12.69999999999999929, -1.100000000000000311 ) ) ;
#18706 = CARTESIAN_POINT ( 'NONE',  ( -10.97260011637327182, 3.256560822415822454, -6.404599650317903681 ) ) ;
#18705 = CARTESIAN_POINT ( 'NONE',  ( -7.720478407978036195, 11.09464301169468037, -1.199719254218446718 ) ) ;
#18707 = CARTESIAN_POINT ( 'NONE',  ( 1.469576158976824144E-15, 19.00000000000000000, 12.00000000000000178 ) ) ;
#18709 = CARTESIAN_POINT ( 'NONE',  ( 1.832500204630353124, 0.1694391671427826207, 1.761704050274701894 ) ) ;
#18708 = CARTESIAN_POINT ( 'NONE',  ( 3.996100316046395484, -0.6559638842641742906, -1.985124821949519891 ) ) ;
#18711 = CARTESIAN_POINT ( 'NONE',  ( 5.859400655334408015, 2.259312458388713196, -0.3864819027975390786 ) ) ;
#18710 = CARTESIAN_POINT ( 'NONE',  ( -11.99967559429689778, 8.028203318877215722, 0.5374089444583232122 ) ) ;
#18712 = CARTESIAN_POINT ( 'NONE',  ( 2.835604015501072439, 1.727201357243525637, 0.2126739171897980840 ) ) ;
#18713 = CARTESIAN_POINT ( 'NONE',  ( 2.703961570921634028, 5.242040035128820108, -1.199719254218446718 ) ) ;
#18714 = CARTESIAN_POINT ( 'NONE',  ( 5.845500506147374153, 6.848780674373954547, 1.199719254218453823 ) ) ;
#18715 = CARTESIAN_POINT ( 'NONE',  ( 3.391645568799035892, 0.04004947218742663240, 1.733546134666413607 ) ) ;
#18716 = CARTESIAN_POINT ( 'NONE',  ( 3.490846471615864921, 2.117612208401131735, 0.4786232489656114253 ) ) ;
#18717 = CARTESIAN_POINT ( 'NONE',  ( 4.822949958159288286, 6.649860922651058992, -1.599625672291256295 ) ) ;
#18718 = CARTESIAN_POINT ( 'NONE',  ( 4.839077477813122918, -1.706110771555340744, -1.074664961451990308 ) ) ;
#18719 = CARTESIAN_POINT ( 'NONE',  ( 0.4687500000003047007, 0.7852924748224731077, -1.895863743164100335 ) ) ;
#18720 = CARTESIAN_POINT ( 'NONE',  ( -0.7499999999999972244, 3.889583334016149863, -1.299038105676652011 ) ) ;
#18721 = CARTESIAN_POINT ( 'NONE',  ( 1.817283056450700318, -0.2383884500203499179, 1.911531453543861225 ) ) ;
#18722 = CARTESIAN_POINT ( 'NONE',  ( -0.6823417656250039265, 15.06770833367473195, -1.181850606188755259 ) ) ;
#18723 = CARTESIAN_POINT ( 'NONE',  ( 6.064703480017706205, 0.6958612881963457397, 2.109637055116654558 ) ) ;
#18724 = ORIENTED_EDGE ( 'NONE', *, *, #15602, .T. ) ;
#18725 = CARTESIAN_POINT ( 'NONE',  ( -0.1110810684433038154, 7.629137130509058728, -2.396956819904518809 ) ) ;
#18726 = CARTESIAN_POINT ( 'NONE',  ( -1.500000000000013101, 1.920833333333356263, 0.8660254037844403729 ) ) ;
#18727 = CARTESIAN_POINT ( 'NONE',  ( 6.636879889089462026, 7.701780277814560982, -1.199719254218446718 ) ) ;
#18728 = CARTESIAN_POINT ( 'NONE',  ( 5.816084710138150093, 5.887779704690372817, -0.7216878364870257245 ) ) ;
#18729 = CARTESIAN_POINT ( 'NONE',  ( 0.000000000000000000, -1.596874999522041705, -3.793834371823813445 ) ) ;
#18730 = CARTESIAN_POINT ( 'NONE',  ( 0.5752228765869402682, -1.604835199033414872, 1.536031695938171460 ) ) ;
#18732 = ADVANCED_FACE ( 'NONE', ( #41964 ), #178319, .F. ) ;
#18731 = CARTESIAN_POINT ( 'NONE',  ( 5.758247127753066685, -1.962046631956643195, -0.001586170976335121285 ) ) ;
#18733 = CARTESIAN_POINT ( 'NONE',  ( 8.595506201384008449, 11.05117653974661529, 1.443375672974076540 ) ) ;
#18734 = CARTESIAN_POINT ( 'NONE',  ( -9.499606442108966320, 7.849261790823902629, 0.08647222121513364890 ) ) ;
#18735 = CARTESIAN_POINT ( 'NONE',  ( 6.432949606591497727, 0.2122621168692347127, 2.252429721023613496 ) ) ;
#18736 = CARTESIAN_POINT ( 'NONE',  ( 4.041212305325117882, 6.872442235258051646, -1.199719254218448494 ) ) ;
#18737 = CARTESIAN_POINT ( 'NONE',  ( -3.824808732831001201, 7.476377598362539345, 0.7216878364870338292 ) ) ;
#18738 = CARTESIAN_POINT ( 'NONE',  ( 4.246570442813556667, -2.039787899008322469, -0.3057716575347816934 ) ) ;
#18739 = CARTESIAN_POINT ( 'NONE',  ( -4.066556009095094737, 6.831733546331167695, 1.199719254218464037 ) ) ;
#18740 = CARTESIAN_POINT ( 'NONE',  ( -1.500000000000013101, 3.910416667349482012, -0.8660254037844313801 ) ) ;
#18741 = CARTESIAN_POINT ( 'NONE',  ( -1.364683531250000748, -0.4906249996585801409, 0.000000000000000000 ) ) ;
#18742 = CARTESIAN_POINT ( 'NONE',  ( 6.028550586359523678, 1.802609027081774951, 0.4991829554215552744 ) ) ;
#18743 = CARTESIAN_POINT ( 'NONE',  ( 4.816919938037654170, 0.8852131329995099884, -1.491020713638806949 ) ) ;
#18744 = CARTESIAN_POINT ( 'NONE',  ( 4.528681460942417303, -1.588859801488880175, 0.7108448094420779517 ) ) ;
#18745 = CARTESIAN_POINT ( 'NONE',  ( 10.50720586046655391, 11.36075438007358507, 0.7216878364870438212 ) ) ;
#18746 = CARTESIAN_POINT ( 'NONE',  ( 1.962814135067984411, -2.097685689255949448, -0.9248770880663819138 ) ) ;
#18747 = CARTESIAN_POINT ( 'NONE',  ( 0.6823417656249917140, 3.655208333674754506, 1.181850606188765695 ) ) ;
#18748 = CARTESIAN_POINT ( 'NONE',  ( 5.671452434703694756, 1.246268910035509991, 1.678523727997438986 ) ) ;
#18749 = CARTESIAN_POINT ( 'NONE',  ( 0.2867153840934755782, 1.362228626754984573, 1.238794746348782505 ) ) ;
#18750 = CARTESIAN_POINT ( 'NONE',  ( 1.499999999999990896, 5.056250000682820378, 1.214306433183764966E-14 ) ) ;
#18751 =( NAMED_UNIT ( * ) SI_UNIT ( $, .STERADIAN. ) SOLID_ANGLE_UNIT ( ) );
#18752 = CARTESIAN_POINT ( 'NONE',  ( 1.301407962653992501, 1.352153127569672098, -1.496052916918483522 ) ) ;
#18753 = CARTESIAN_POINT ( 'NONE',  ( -0.02900071798685524560, -0.004641455105012376459, -2.173770343569726649 ) ) ;
#18754 = CARTESIAN_POINT ( 'NONE',  ( 8.213514019010339950, 13.37925768050776298, -8.583069077171659345 ) ) ;
#18755 = CARTESIAN_POINT ( 'NONE',  ( -7.527801604085656351, 9.805521176231838609, 1.599625672291295375 ) ) ;
#18756 = CARTESIAN_POINT ( 'NONE',  ( 5.819474248763732760, 7.812472595022922128, -1.599625672291262513 ) ) ;
#18757 = CARTESIAN_POINT ( 'NONE',  ( 3.563236855010095017, -1.732559338849114505, 1.222301536229251084 ) ) ;
#18758 = CARTESIAN_POINT ( 'NONE',  ( 0.6823417656249882723, -0.6572916663252492686, 1.181850606188755259 ) ) ;
#18759 = CARTESIAN_POINT ( 'NONE',  ( 5.496661139185262002, -0.4475443406098400523, -1.769863040007889410 ) ) ;
#18760 = EDGE_LOOP ( 'NONE', ( #130636, #200012, #80742, #66766 ) ) ;
#18761 = CARTESIAN_POINT ( 'NONE',  ( -5.271087860662956537, 9.371629280740593870, 0.000000000000000000 ) ) ;
#18762 = CARTESIAN_POINT ( 'NONE',  ( 2.273078772964581606, 5.704048046545305617, -0.2041365465368546461 ) ) ;
#18763 = CARTESIAN_POINT ( 'NONE',  ( 7.810905894804431426, 8.285347430126213553, 0.000000000000000000 ) ) ;
#18764 = CARTESIAN_POINT ( 'NONE',  ( 3.285556943750000514, -1.101041666188710355, 1.896917185911906500 ) ) ;
#18765 = CARTESIAN_POINT ( 'NONE',  ( -5.368138756007025947, 8.350246751061767725, 1.199719254218452047 ) ) ;
#18766 = CARTESIAN_POINT ( 'NONE',  ( 3.480727363932310414, -1.353466037422011992, 1.499425228245174102 ) ) ;
#18767 = CARTESIAN_POINT ( 'NONE',  ( 6.317417574511640765, -0.2763070477263400715, 2.189352377801502936 ) ) ;
#18768 = CARTESIAN_POINT ( 'NONE',  ( -4.065465959251405081, 5.836405933916976707, -1.599625672291271394 ) ) ;
#18769 = CARTESIAN_POINT ( 'NONE',  ( 3.801460577334394575, -1.406423387113703960, -1.218697170607488944 ) ) ;
#18770 = CARTESIAN_POINT ( 'NONE',  ( 10.07778825365955733, 10.65184113889131012, -0.7998128361456281477 ) ) ;
#18771 = CARTESIAN_POINT ( 'NONE',  ( -9.768463870713130603, 4.463474924597734095, -6.895317384053313070 ) ) ;
#18772 = CARTESIAN_POINT ( 'NONE',  ( -4.440459003675619520, 5.139289244831666714, 1.199719254218462483 ) ) ;
#18773 = CARTESIAN_POINT ( 'NONE',  ( -6.672584156219988571, 10.93643194889866521, -0.7998128361456291469 ) ) ;
#18775 = CARTESIAN_POINT ( 'NONE',  ( -4.645415345243833372, 7.101964347008438594, 1.385782282575825919 ) ) ;
#18774 = CARTESIAN_POINT ( 'NONE',  ( -7.923814432544069142, 8.209148024248356990, 0.000000000000000000 ) ) ;
#18776 = CARTESIAN_POINT ( 'NONE',  ( -1.402160292154681736E-14, -0.3031249996585801965, -1.575800808251665908 ) ) ;
#18777 = CARTESIAN_POINT ( 'NONE',  ( 1.563399581876812716, 1.420944641023152322, -0.9932112465018216874 ) ) ;
#18778 = CARTESIAN_POINT ( 'NONE',  ( 1.200653373194009443, -0.4260525342448440722, 1.687239105062097400 ) ) ;
#18780 = CARTESIAN_POINT ( 'NONE',  ( 8.948018195339340508, 9.541702104091804415, -0.7216878364870197293 ) ) ;
#18779 = CARTESIAN_POINT ( 'NONE',  ( 0.09532371275382427178, -0.5158531520006398585, -2.257940698305866967 ) ) ;
#18781 = CARTESIAN_POINT ( 'NONE',  ( 4.415115299905642665, 5.179997933758551554, -1.199719254218450271 ) ) ;
#18782 = CARTESIAN_POINT ( 'NONE',  ( 0.8782832160191712534, -1.147062573054495216, 1.711818785435960111 ) ) ;
#18783 = CARTESIAN_POINT ( 'NONE',  ( 4.306686350635271054, 8.176217842383143974, -0.7998128361456221525 ) ) ;
#18784 = CARTESIAN_POINT ( 'NONE',  ( 6.884150280000160826, -0.1566355309425542519, 2.263600626914013869 ) ) ;
#18785 = CARTESIAN_POINT ( 'NONE',  ( -1.225000000000033396, 1.000000000000021760, -2.775557561562891351E-14 ) ) ;
#18787 = AXIS2_PLACEMENT_3D ( 'NONE', #2410, #169209, #70611 ) ;
#18786 = CARTESIAN_POINT ( 'NONE',  ( -5.098748287191073203, 8.106234214101666780, 1.199719254218452935 ) ) ;
#18788 = CARTESIAN_POINT ( 'NONE',  ( 0.3386658216258168763, 0.3346604457750371187, 1.942702894000091662 ) ) ;
#18789 = CIRCLE ( 'NONE', #139908, 6.959052028703005099 ) ;
#18791 = CARTESIAN_POINT ( 'NONE',  ( -5.316205630334251531, 9.216340645449683677, -0.7216878364870338292 ) ) ;
#18790 = CARTESIAN_POINT ( 'NONE',  ( 4.992401499097729456, -1.057410677138232780, 1.593263788312593743 ) ) ;
#18792 = CARTESIAN_POINT ( 'NONE',  ( 6.147136880733683917, -1.866598994669689926, 1.177069016086537356 ) ) ;
#18793 = CARTESIAN_POINT ( 'NONE',  ( 0.6124999999999707345, 1.895833334016133742, 1.060881119635880721 ) ) ;
#18794 = CARTESIAN_POINT ( 'NONE',  ( -6.640718169120819248, -6.363025497629810623, -7.257245574616625561 ) ) ;
#18795 = CARTESIAN_POINT ( 'NONE',  ( 4.217995187182922656, 6.014356699837137832, 1.443375672974058777 ) ) ;
#18796 = CARTESIAN_POINT ( 'NONE',  ( -7.553827861469316396, 8.841829255582865699, -1.199719254218452047 ) ) ;
#18797 = CARTESIAN_POINT ( 'NONE',  ( 6.410795937096152919, -0.5649949523399040441, -2.043744576961013859 ) ) ;
#18798 = ORIENTED_EDGE ( 'NONE', *, *, #28769, .T. ) ;
#18799 = CARTESIAN_POINT ( 'NONE',  ( 3.452467797911736636, 2.307758715189492271, 0.002325993833134780940 ) ) ;
#18800 = CARTESIAN_POINT ( 'NONE',  ( 4.932062528313536198, 1.127988425013145779, 1.604980062286972542 ) ) ;
#18801 = CARTESIAN_POINT ( 'NONE',  ( 0.7429250141685154185, -0.2344385519315282107, -1.947609053799495005 ) ) ;
#18802 = CARTESIAN_POINT ( 'NONE',  ( 4.202664430556261266, 4.005456045178151570, 0.7216878364870317197 ) ) ;
#18803 = CARTESIAN_POINT ( 'NONE',  ( -1.626862140677534470E-15, 1.125000000682806034, 1.224999999999975886 ) ) ;
#18804 = CARTESIAN_POINT ( 'NONE',  ( 0.1107727185766090999, 2.028241449780379568, 0.6078911015285259900 ) ) ;
#18805 = CARTESIAN_POINT ( 'NONE',  ( -3.588104209110990706, 7.337872010604796991, 1.040834085586084257E-14 ) ) ;
#18806 = CARTESIAN_POINT ( 'NONE',  ( -2.788906526875773208E-15, 8.687500000000000000, -1.499999999999998446 ) ) ;
#18807 = CARTESIAN_POINT ( 'NONE',  ( 2.870184708472456325, -2.148041568373111776, 0.3144570722862209955 ) ) ;
#18808 = CARTESIAN_POINT ( 'NONE',  ( 9.577100139991578942, 12.68281731961604564, -7.233471777081839527 ) ) ;
#18809 = CARTESIAN_POINT ( 'NONE',  ( 0.1762450972803019933, 2.096614079038420897, -0.3174041833761130360 ) ) ;
#18810 = CARTESIAN_POINT ( 'NONE',  ( -0.7499999999999972244, 3.389583334016149863, -1.299038105676652011 ) ) ;
#18811 = CARTESIAN_POINT ( 'NONE',  ( 8.971744963941056028, 11.49012176272984931, 1.599625672291281386 ) ) ;
#18812 = CARTESIAN_POINT ( 'NONE',  ( 11.94105721839855505, 13.52698343341124421, -1.187919402540330127 ) ) ;
#18813 = CARTESIAN_POINT ( 'NONE',  ( 6.509182584184366682, 6.829728176725765820, 0.5468608461018635847 ) ) ;
#18814 = CARTESIAN_POINT ( 'NONE',  ( 2.266935757080061897, -1.882882732336080167, -0.8380483592859179209 ) ) ;
#18816 = DIRECTION ( 'NONE',  ( -0.6483454320283799088, 0.000000000000000000, 0.7613463080411786432 ) ) ;
#18815 = CARTESIAN_POINT ( 'NONE',  ( -10.00321840878439339, 10.56484298653695397, 1.040834085586084257E-14 ) ) ;
#18817 = CARTESIAN_POINT ( 'NONE',  ( -1.402160292154681736E-14, 2.446875000341416584, -1.575800808251660134 ) ) ;
#18818 = CARTESIAN_POINT ( 'NONE',  ( 0.07775346131142897577, 1.984126704040774181, -2.702190870904349840 ) ) ;
#18819 =( BOUNDED_CURVE ( )  B_SPLINE_CURVE ( 2, ( #24188, #205075, #23117, #71867, #168333, #69736, #170455 ),
 .UNSPECIFIED., .F., .T. ) 
 B_SPLINE_CURVE_WITH_KNOTS ( ( 3, 2, 2, 3 ),
 ( 0.3784226669537131271, 0.3809523809523809312, 0.3869047619047619180, 0.3894344759034296666 ),
 .UNSPECIFIED. ) 
 CURVE ( )  GEOMETRIC_REPRESENTATION_ITEM ( )  RATIONAL_B_SPLINE_CURVE ( ( 0.9345202395942608931, 0.9430618748659213013, 1.000000000000000000, 0.8660254037844387076, 1.000000000000000000, 0.9430618748659225226, 0.9345202395942613371 ) ) 
 REPRESENTATION_ITEM ( '' )  );
#18820 = CARTESIAN_POINT ( 'NONE',  ( 10.56536251450128994, 11.25961062549474612, 3.404319718479180690 ) ) ;
#18821 = ORIENTED_EDGE ( 'NONE', *, *, #137465, .T. ) ;
#18822 = CARTESIAN_POINT ( 'NONE',  ( 4.635362334195573197, -0.09024504784891505815, 1.910265517452471862 ) ) ;
#18823 = CARTESIAN_POINT ( 'NONE',  ( -1.772826578343107640, 3.949999999999974420, 0.4499999999999487188 ) ) ;
#18825 = AXIS2_PLACEMENT_3D ( 'NONE', #109823, #99627, #210433 ) ;
#18824 = CARTESIAN_POINT ( 'NONE',  ( 1.124742813458483814, 1.347236035482470839, -1.817372803150618221 ) ) ;
#18826 = CARTESIAN_POINT ( 'NONE',  ( -2.117044542028253318, 5.621635732341564662, -0.7998128361456281477 ) ) ;
#18827 = CARTESIAN_POINT ( 'NONE',  ( 1.212835290986268300, 1.479965279312319693, -1.044435387019273742 ) ) ;
#18828 = CARTESIAN_POINT ( 'NONE',  ( 0.3740639818887542267, -1.901581053304630675, -0.2314239742453021165 ) ) ;
#18829 = CARTESIAN_POINT ( 'NONE',  ( 1.662640112210824306, -0.7432673875312334477, -1.932532381715674097 ) ) ;
#18830 = CARTESIAN_POINT ( 'NONE',  ( 1.364683531249986537, 0.1760416670080860446, 0.7879004041258500513 ) ) ;
#18831 = CARTESIAN_POINT ( 'NONE',  ( 0.6726557866889815163, -1.855577277548149828, -0.6663020492489196700 ) ) ;
#18832 = CARTESIAN_POINT ( 'NONE',  ( 5.953728026056397837, 0.5566793334266966209, -1.844321365346488273 ) ) ;
#18834 = CARTESIAN_POINT ( 'NONE',  ( 6.467812791377033577, 6.763347601114057639, -0.2696018389747659172 ) ) ;
#18833 = CARTESIAN_POINT ( 'NONE',  ( 0.2062968637084483525, -0.6088960595307371104, 2.225859948526871079 ) ) ;
#18835 = CARTESIAN_POINT ( 'NONE',  ( -1.364683531250012516, 1.780208333674757615, 0.7879004041258379498 ) ) ;
#18836 = CARTESIAN_POINT ( 'NONE',  ( 4.000476411064065374, 2.052455503700638229, 0.2052804401120340017 ) ) ;
#18837 = CARTESIAN_POINT ( 'NONE',  ( -4.903245109636583443, 8.872203061218007392, -0.7998128361456281477 ) ) ;
#18838 = CARTESIAN_POINT ( 'NONE',  ( 6.903072767652295383, 11.20533532890304684, 1.040834085586084257E-14 ) ) ;
#18839 = DIRECTION ( 'NONE',  ( 0.000000000000000000, -1.000000000000000000, 0.000000000000000000 ) ) ;
#18840 = CARTESIAN_POINT ( 'NONE',  ( 5.843727902690005749, 6.776436293681846301, -1.199719254218445830 ) ) ;
#18843 = CARTESIAN_POINT ( 'NONE',  ( 1.499999999999989120, 3.254166666666690855, 0.8660254037844524744 ) ) ;
#18842 = AXIS2_PLACEMENT_3D ( 'NONE', #69117, #65911, #51842 ) ;
#18841 = CARTESIAN_POINT ( 'NONE',  ( 5.631892205062830392, -1.333580992396019571, -1.629923671128389762 ) ) ;
#18844 = CARTESIAN_POINT ( 'NONE',  ( 1.223348113247175961, -1.962646724111057672, -0.9287667758015824004 ) ) ;
#18845 = CARTESIAN_POINT ( 'NONE',  ( 1.364683531249988757, 1.946875000341415030, 0.000000000000000000 ) ) ;
#18846 = CARTESIAN_POINT ( 'NONE',  ( 4.833375328034618335, -1.978455579520097762, 0.8711445904842631816 ) ) ;
#18847 = CARTESIAN_POINT ( 'NONE',  ( 5.725262222419306823, 1.782257655895511661, 0.9500345275383536015 ) ) ;
#18848 = DIRECTION ( 'NONE',  ( -5.578564026256490882E-16, -1.000000000000000000, -9.066213480720158442E-32 ) ) ;
#18849 = VECTOR ( 'NONE', #45045, 1000.000000000000000 ) ;
#18852 = CARTESIAN_POINT ( 'NONE',  ( 4.853455804012203778, 8.606189504748821051, 0.7216878364870438212 ) ) ;
#18851 = CARTESIAN_POINT ( 'NONE',  ( -3.285556943750000514, -1.538541666188708357, -1.896917185911906500 ) ) ;
#18850 = CARTESIAN_POINT ( 'NONE',  ( 8.039058738260216330, 8.343599714250547805, -0.7998128361456341429 ) ) ;
#18853 = CARTESIAN_POINT ( 'NONE',  ( -6.981522756394290319, 7.109807735406931783, 0.7998128361456341429 ) ) ;
#18854 = CARTESIAN_POINT ( 'NONE',  ( 3.872279980006509970, -1.995268062538615883, -0.2910826752766728642 ) ) ;
#18855 = CARTESIAN_POINT ( 'NONE',  ( -6.991200766141138168, 11.30815132714001159, 0.7998128361456481317 ) ) ;
#18857 = PRESENTATION_STYLE_ASSIGNMENT (( #133737 ) ) ;
#18856 = CARTESIAN_POINT ( 'NONE',  ( -4.060830702492950195, 4.696389560118578999, -1.199719254218452047 ) ) ;
#18859 = CARTESIAN_POINT ( 'NONE',  ( -1.364683531250000748, 8.609375000341396245, 0.000000000000000000 ) ) ;
#18858 = CARTESIAN_POINT ( 'NONE',  ( 5.084929678302336775, -0.2608814864752464491, -2.145832476913120068 ) ) ;
#18860 = CARTESIAN_POINT ( 'NONE',  ( 7.228805602686604992, -7.003075417673639613, 7.884707905546937567 ) ) ;
#18861 = EDGE_CURVE ( 'NONE', #96467, #97798, #95943, .T. ) ;
#18863 = CARTESIAN_POINT ( 'NONE',  ( 4.587517648402447357, -0.5350702435001615243, 1.944077497823355483 ) ) ;
#18862 = CARTESIAN_POINT ( 'NONE',  ( -7.998947441938374148, 8.434452891790657603, 1.040834085586084257E-14 ) ) ;
#18864 = CARTESIAN_POINT ( 'NONE',  ( 0.7499999999999920064, 4.733333333333352932, 1.299038105676669330 ) ) ;
#18865 = CARTESIAN_POINT ( 'NONE',  ( 0.5215560022201523038, -0.9183498723843477318, -1.459886522650925000 ) ) ;
#18866 = CARTESIAN_POINT ( 'NONE',  ( 6.886615681098613884, 6.999082814228660077, 0.000000000000000000 ) ) ;
#18868 = CARTESIAN_POINT ( 'NONE',  ( 7.354371980770088690, 7.544798497178720531, 0.000000000000000000 ) ) ;
#18867 = CARTESIAN_POINT ( 'NONE',  ( 7.117667457494414762, 11.24776976714476184, 1.040834085586084257E-14 ) ) ;
#18869 = CARTESIAN_POINT ( 'NONE',  ( -11.63630038494604690, 8.312388184584818873, 2.945693487284683165 ) ) ;
#18870 = CARTESIAN_POINT ( 'NONE',  ( 5.114452126850835612, 1.290914414355217366, -1.353902443742838191 ) ) ;
#18871 = CARTESIAN_POINT ( 'NONE',  ( 6.533470335063485734, -0.1341179537190802518, 1.982235210812468340 ) ) ;
#18872 = CARTESIAN_POINT ( 'NONE',  ( -4.243057018770354460, 3.980691995439412878, 0.4872899543362524954 ) ) ;
#18873 = CARTESIAN_POINT ( 'NONE',  ( 4.514501963226220660, 4.369266499959774563, -0.7216878364870197293 ) ) ;
#18874 =( BOUNDED_SURFACE ( )  B_SPLINE_SURFACE ( 3, 1, ( 
 ( #27392, #112989 ),
 ( #93492, #179001 ),
 ( #30616, #96705 ),
 ( #128200, #159532 ),
 ( #95635, #79353 ),
 ( #162754, #14327 ),
 ( #145471, #211466 ) ),
 .UNSPECIFIED., .T., .F., .T. ) 
 B_SPLINE_SURFACE_WITH_KNOTS ( ( 4, 3, 4 ),
 ( 2, 2 ),
 ( 0.000000000000000000, 0.5000000000000000000, 1.000000000000000000 ),
 ( 0.000000000000000000, 1.000000000000000000 ),
 .UNSPECIFIED. ) 
 GEOMETRIC_REPRESENTATION_ITEM ( )  RATIONAL_B_SPLINE_SURFACE ( (
 ( 1.000000000000000000, 1.000000000000000000),
 ( 0.3333333333333333703, 0.3333333333333333703),
 ( 0.3333333333333333703, 0.3333333333333333703),
 ( 1.000000000000000000, 1.000000000000000000),
 ( 0.3333333333333333703, 0.3333333333333333703),
 ( 0.3333333333333333703, 0.3333333333333333703),
 ( 1.000000000000000000, 1.000000000000000000) ) ) 
 REPRESENTATION_ITEM ( '' )  SURFACE ( )  );
#18875 = CARTESIAN_POINT ( 'NONE',  ( -6.333067150914850174, 8.481940657524365434, 1.443375672974064550 ) ) ;
#18876 = ORIENTED_EDGE ( 'NONE', *, *, #195623, .T. ) ;
#18878 = CARTESIAN_POINT ( 'NONE',  ( 0.5797041155359907716, -0.7231210598357665775, 1.882482590253447663 ) ) ;
#18877 = CARTESIAN_POINT ( 'NONE',  ( 1.858217301831434964, 0.8087058978607818416, -1.960417502992222838 ) ) ;
#18879 = CARTESIAN_POINT ( 'NONE',  ( 1.371055822538247870, -1.554752094505476467, -0.9295159999406394924 ) ) ;
#18880 = CARTESIAN_POINT ( 'NONE',  ( 7.147083253059300922, 8.367293879104554577, 1.199719254218452935 ) ) ;
#18881 = CARTESIAN_POINT ( 'NONE',  ( 6.034075718726629844, 1.069613854859407631, -1.878468107683453514 ) ) ;
#18882 = CARTESIAN_POINT ( 'NONE',  ( 6.089583550832340819, 10.25626457594641749, 1.040834085586084257E-14 ) ) ;
#18884 = CARTESIAN_POINT ( 'NONE',  ( -0.1005721928965920831, -1.878210221491773524, 0.3762452260359094303 ) ) ;
#18883 = CARTESIAN_POINT ( 'NONE',  ( -4.218558352146454915, 8.073401844146177453, 1.040834085586084257E-14 ) ) ;
#18885 = LINE ( 'NONE', #21007, #142339 ) ;
#18886 = PRESENTATION_STYLE_ASSIGNMENT (( #487 ) ) ;
#18887 = EDGE_CURVE ( 'NONE', #92086, #207114, #85215, .T. ) ;
#18888 = CARTESIAN_POINT ( 'NONE',  ( 6.439759776366775768, 7.575769829591800786, 1.082531754730558626 ) ) ;
#18889 = CARTESIAN_POINT ( 'NONE',  ( -1.402160292154681736E-14, -0.9906249996585834161, -1.575800808251665908 ) ) ;
#18890 = CARTESIAN_POINT ( 'NONE',  ( 2.738383840280328663, 5.178236332760252303, 1.082531754730548412 ) ) ;
#18891 = CARTESIAN_POINT ( 'NONE',  ( -9.622536337397040285, 12.24937836509514710, 1.599625672291281386 ) ) ;
#18892 = CARTESIAN_POINT ( 'NONE',  ( 3.731458613173586514, -1.998165266068991253, 0.8252760040215676440 ) ) ;
#18893 = CARTESIAN_POINT ( 'NONE',  ( -6.794044374223859428, 7.099008989448849505, 0.000000000000000000 ) ) ;
#18894 = CARTESIAN_POINT ( 'NONE',  ( 5.072158865288222351, 8.931619419562697004, 0.7216878364870317197 ) ) ;
#18895 = CARTESIAN_POINT ( 'NONE',  ( 2.180079139336263516, 2.078761533942363737, -0.4183221158333137457 ) ) ;
#18896 = CARTESIAN_POINT ( 'NONE',  ( 0.000000000000000000, 8.500000000000000000, 0.000000000000000000 ) ) ;
#18897 = CARTESIAN_POINT ( 'NONE',  ( 2.003138245156708130, 1.636809484843353868, 1.098402624201348488 ) ) ;
#18898 = CARTESIAN_POINT ( 'NONE',  ( 4.922078805074791674, -1.902621863305080430, 0.1933406509087298719 ) ) ;
#18899 = ORIENTED_EDGE ( 'NONE', *, *, #157376, .F. ) ;
#18900 = CARTESIAN_POINT ( 'NONE',  ( 9.499801640457391727, -7.008739397177219388, 0.06269018847620325130 ) ) ;
#18901 = CARTESIAN_POINT ( 'NONE',  ( 6.391062254520311292, 0.1913994329204322109, 1.960204640275018395 ) ) ;
#18902 = CARTESIAN_POINT ( 'NONE',  ( 1.745936028080337765, 0.6089015219087092756, 1.844080840262368071 ) ) ;
#18903 = VERTEX_POINT ( 'NONE', #76565 ) ;
#18904 = CARTESIAN_POINT ( 'NONE',  ( -5.255720823952942489, 6.160704378480398979, -1.199719254218453823 ) ) ;
#18906 = CARTESIAN_POINT ( 'NONE',  ( 6.672971353126269989, -7.009934032700107842, -6.761775799041030766 ) ) ;
#18905 = CARTESIAN_POINT ( 'NONE',  ( -7.946487431385463651, 8.443525889470736345, 0.7216878364870317197 ) ) ;
#18908 = CARTESIAN_POINT ( 'NONE',  ( 6.333067150914820864, 6.561202228921677815, 0.7216878364870328300 ) ) ;
#18907 = CARTESIAN_POINT ( 'NONE',  ( 7.793239369756836510, 7.986534107671458216, 0.7998128361456341429 ) ) ;
#18910 = ORIENTED_EDGE ( 'NONE', *, *, #52547, .F. ) ;
#18909 = CARTESIAN_POINT ( 'NONE',  ( 4.916621234345090130, -0.6478637630910142331, -1.799314785492410529 ) ) ;
#18911 = CARTESIAN_POINT ( 'NONE',  ( 3.844505992619148937, 2.196175933995975438, 0.2170506636963928093 ) ) ;
#18912 = CARTESIAN_POINT ( 'NONE',  ( 2.520803682403276902, 1.441976459853638204, -1.670562425240495363 ) ) ;
#18913 = CARTESIAN_POINT ( 'NONE',  ( 11.78331023100045627, 13.88000000000000078, -1.800000000000001155 ) ) ;
#18914 = CARTESIAN_POINT ( 'NONE',  ( 0.1527893875182678718, 0.3269112364552365091, 1.883972597190447518 ) ) ;
#18915 = CARTESIAN_POINT ( 'NONE',  ( -1.850000000000000089, 2.265195232789710231E-16, 0.5999999999999969802 ) ) ;
#18916 = DIRECTION ( 'NONE',  ( 0.000000000000000000, -1.000000000000000000, 0.000000000000000000 ) ) ;
#18917 = CARTESIAN_POINT ( 'NONE',  ( -0.5341596719058562259, 6.871489935936940796, 3.795319914582534704 ) ) ;
#18918 = CARTESIAN_POINT ( 'NONE',  ( 3.033707436314789785, 1.966763487489433970, -0.6469820378900912328 ) ) ;
#18919 = CARTESIAN_POINT ( 'NONE',  ( -5.382750679825375251, 6.238629533673094585, -1.199719254218446718 ) ) ;
#18920 = CARTESIAN_POINT ( 'NONE',  ( -5.394899524673852476, 7.567224757263017132, 1.245178244268474010 ) ) ;
#18922 = CARTESIAN_POINT ( 'NONE',  ( 2.114359756454447847, -1.018641858927371135, -1.906637348776268004 ) ) ;
#18921 = CARTESIAN_POINT ( 'NONE',  ( -5.278201874421821316, 5.052323696447222900, 0.7998128361456341429 ) ) ;
#18923 = CARTESIAN_POINT ( 'NONE',  ( 3.509492838045696672, -2.158849082856160173, 0.3763758916049686487 ) ) ;
#18924 = CARTESIAN_POINT ( 'NONE',  ( 0.02755585400013305097, 7.629137130509076492, -2.789001785468494976 ) ) ;
#18925 = CARTESIAN_POINT ( 'NONE',  ( 3.770576118376306241, 6.452737000530752276, 1.082531754730549078 ) ) ;
#18926 = CARTESIAN_POINT ( 'NONE',  ( -1.225000000000044276, 1.083333334016145066, 0.7072540797572517413 ) ) ;
#18927 = CARTESIAN_POINT ( 'NONE',  ( 0.6823417656249969321, 13.83854166700806942, -1.181850606188757036 ) ) ;
#18928 = CARTESIAN_POINT ( 'NONE',  ( -5.061990249855848667, 6.999017606288844284, -1.599625672291271394 ) ) ;
#18930 = CARTESIAN_POINT ( 'NONE',  ( 5.484916526786003388, -1.734343006517705676, 0.008455456694493946809 ) ) ;
#18929 = AXIS2_PLACEMENT_3D ( 'NONE', #178318, #51231, #193483 ) ;
#18931 = CARTESIAN_POINT ( 'NONE',  ( -8.514157279702017078, 12.87700789305364069, -0.7216878364870267237 ) ) ;
#18932 = CARTESIAN_POINT ( 'NONE',  ( 3.573154620739454224, 1.869565233029608198, 0.8895530118792621677 ) ) ;
#18933 = CARTESIAN_POINT ( 'NONE',  ( 5.062167955004798436, -1.175237403299607797, 1.760913580352542862 ) ) ;
#18934 = VECTOR ( 'NONE', #202463, 1000.000000000000000 ) ;
#18935 = CARTESIAN_POINT ( 'NONE',  ( 6.419949431270806528, 7.448694743692793274, 1.199719254218462483 ) ) ;
#18936 = CARTESIAN_POINT ( 'NONE',  ( 1.364683531249990311, 4.134375000341417028, 1.214306433183764966E-14 ) ) ;
#18937 = CARTESIAN_POINT ( 'NONE',  ( 2.535944157116743369, 1.207843060446149197, 1.555523554018751309 ) ) ;
#18938 = CARTESIAN_POINT ( 'NONE',  ( 1.019614524654769872, -0.4619345408787678964, 1.855657206939323789 ) ) ;
#18939 = CARTESIAN_POINT ( 'NONE',  ( 5.209026396049201146, -0.3404489335739938061, 2.266724491853837620 ) ) ;
#18940 = CARTESIAN_POINT ( 'NONE',  ( 3.035583632137848653, -1.226507576337819483, -1.352503160878690380 ) ) ;
#18941 = B_SPLINE_CURVE_WITH_KNOTS ( 'NONE', 1,
 ( #202880, #21987 ),
 .UNSPECIFIED., .F., .F.,
 ( 2, 2 ),
 ( 0.000000000000000000, 0.9297416518164913768 ),
 .UNSPECIFIED. ) ;
#18942 = CARTESIAN_POINT ( 'NONE',  ( 6.048345925472166762, 10.07050432311064903, 0.7216878364870317197 ) ) ;
#18943 = CARTESIAN_POINT ( 'NONE',  ( 4.161989969270883272, 7.799479364217271282, 0.7216878364870317197 ) ) ;
#18944 = CARTESIAN_POINT ( 'NONE',  ( -6.775324078527193983, 8.927630729746953264, -1.599625672291263179 ) ) ;
#18945 = ORIENTED_EDGE ( 'NONE', *, *, #67226, .F. ) ;
#18946 = CARTESIAN_POINT ( 'NONE',  ( 3.744393049878576463, 1.073438034848249290, -1.702967747733853843 ) ) ;
#18947 = VECTOR ( 'NONE', #81634, 1000.000000000000000 ) ;
#18948 = CARTESIAN_POINT ( 'NONE',  ( 4.434394140398959294, -1.132915509570767476, 1.601352629973289199 ) ) ;
#18949 = CARTESIAN_POINT ( 'NONE',  ( -6.832419346282942563, 10.05857410638369487, 1.199719254218453823 ) ) ;
#18950 = CARTESIAN_POINT ( 'NONE',  ( -6.437424008390261854, 6.404749519410410485, 0.7998128361456341429 ) ) ;
#18951 = CARTESIAN_POINT ( 'NONE',  ( 0.1753634416057498202, 0.7014533214223102053, -2.226873008360684913 ) ) ;
#18953 = CARTESIAN_POINT ( 'NONE',  ( 5.682415782506053503, -1.727394229680437876, -0.3844701117694647174 ) ) ;
#18952 = CARTESIAN_POINT ( 'NONE',  ( 0.2399332258718233080, 2.085444179493881389, 0.1495565104911322774 ) ) ;
#18954 = CARTESIAN_POINT ( 'NONE',  ( 10.97093617010649780, -5.223179855898941959, -0.3663205537283247826 ) ) ;
#18955 = CARTESIAN_POINT ( 'NONE',  ( 2.414256260463796711, 1.430409426244143134, -1.660321623440104810 ) ) ;
#18956 = CARTESIAN_POINT ( 'NONE',  ( 6.650362500428334656, -1.339898832705511911, 1.110426912289312451 ) ) ;
#18957 = CARTESIAN_POINT ( 'NONE',  ( 7.019370843573166319, 9.212351955633947043, 1.599625672291281386 ) ) ;
#18958 = CARTESIAN_POINT ( 'NONE',  ( 0.1335669894368343991, 7.629137130509040965, -2.753547149787978654 ) ) ;
#18959 = CARTESIAN_POINT ( 'NONE',  ( 0.7149654600043838792, -0.2576282674517544335, 1.705390864826474839 ) ) ;
#18960 = CARTESIAN_POINT ( 'NONE',  ( 1.054597461939084768, 2.025951976169305890, -1.085350914182762638 ) ) ;
#18961 = CARTESIAN_POINT ( 'NONE',  ( 0.5389544483674936215, -1.876709678404146153, 1.131566444868239874 ) ) ;
#18962 = CARTESIAN_POINT ( 'NONE',  ( 2.491098823239074278, -0.3784457004711218042, -2.174036671264235387 ) ) ;
#18963 = FACE_OUTER_BOUND ( 'NONE', #25327, .T. ) ;
#18964 = CARTESIAN_POINT ( 'NONE',  ( 6.883263157960365142, -0.007059606330772279746, 2.153658854459541416 ) ) ;
#18965 = CARTESIAN_POINT ( 'NONE',  ( 0.7499999999999902300, 3.983333333333352488, 1.299038105676669330 ) ) ;
#18966 = CARTESIAN_POINT ( 'NONE',  ( 1.622414240495053672, 2.095119945234637182, 0.3050691438145485268 ) ) ;
#18967 = AXIS2_PLACEMENT_3D ( 'NONE', #44218, #41025, #107134 ) ;
#18968 = CARTESIAN_POINT ( 'NONE',  ( 6.620655732516647518, 3.684600858287550906, 2.687722323901103660 ) ) ;
#18969 = CARTESIAN_POINT ( 'NONE',  ( 5.350583055395741638, 0.5590458624239265095, 1.843501136262601037 ) ) ;
#18970 = EDGE_LOOP ( 'NONE', ( #148266, #98534, #188231, #16913, #112394 ) ) ;
#18972 = CARTESIAN_POINT ( 'NONE',  ( -1.001543065824772872E-14, 5.212500000000019895, 1.732050807568877637 ) ) ;
#18971 = CARTESIAN_POINT ( 'NONE',  ( 1.435548669473255323, -1.664339209632224481, -1.576619915386682447 ) ) ;
#18973 = CARTESIAN_POINT ( 'NONE',  ( 4.844340958784499662, 4.546152628203684820, 0.7998128361456341429 ) ) ;
#18974 = CARTESIAN_POINT ( 'NONE',  ( 5.198661835836162481, 8.152523677529138979, 1.199719254218462483 ) ) ;
#18975 = CARTESIAN_POINT ( 'NONE',  ( 5.162811894357514753, 0.6434298260243781487, 2.126049117748362249 ) ) ;
#18976 = CARTESIAN_POINT ( 'NONE',  ( -7.619319141200077361, 9.912291636198670375, 1.443375672974090751 ) ) ;
#18978 = EDGE_CURVE ( 'NONE', #8679, #93531, #28898, .T. ) ;
#18977 = FACE_OUTER_BOUND ( 'NONE', #208314, .T. ) ;
#18979 = CARTESIAN_POINT ( 'NONE',  ( 6.507550544879468823, 6.694489845221929691, -0.7216878364870257245 ) ) ;
#18980 = CARTESIAN_POINT ( 'NONE',  ( -8.229436053370685400, 10.62409470039771442, 1.443375672974090751 ) ) ;
#18981 = CARTESIAN_POINT ( 'NONE',  ( 5.397554552016216256, 7.390509292142662723, 1.443375672974065660 ) ) ;
#18982 = AXIS2_PLACEMENT_3D ( 'NONE', #16721, #148882, #151030 ) ;
#18983 = ORIENTED_EDGE ( 'NONE', *, *, #122619, .F. ) ;
#18984 = CARTESIAN_POINT ( 'NONE',  ( 2.901017702322743919, -0.9963018188003970321, -1.753030416019534021 ) ) ;
#18986 = CARTESIAN_POINT ( 'NONE',  ( 1.270463096138880088, -0.9239429406890822261, -1.844087381150324001 ) ) ;
#18985 = CARTESIAN_POINT ( 'NONE',  ( 6.805303039055573322, 10.02693841461847057, 1.199719254218460707 ) ) ;
#18987 = DIRECTION ( 'NONE',  ( 0.000000000000000000, 0.000000000000000000, 1.000000000000000000 ) ) ;
#18988 = CARTESIAN_POINT ( 'NONE',  ( 6.007671464186834065, 7.141943142040370063, 1.082531754730549967 ) ) ;
#18989 = CARTESIAN_POINT ( 'NONE',  ( -3.947104627881229622, 8.980740528189222971, 0.7749999999999996891 ) ) ;
#18990 = CARTESIAN_POINT ( 'NONE',  ( -1.364683531250010295, 4.030208333674751842, 0.7879004041258379498 ) ) ;
#18991 = CARTESIAN_POINT ( 'NONE',  ( 4.013774469618203611, -1.125877316280783358, -1.879984707117538845 ) ) ;
#18992 = CARTESIAN_POINT ( 'NONE',  ( 1.336564801266389990, 0.5826540126645517459, -1.930418273149013153 ) ) ;
#18993 = CARTESIAN_POINT ( 'NONE',  ( 1.135996871135702024, 0.3593859243370273182, 1.805655672011026391 ) ) ;
#18994 = CARTESIAN_POINT ( 'NONE',  ( 5.443040390997877509, -1.805468894110316080, -1.412473186189531438 ) ) ;
#18995 = CARTESIAN_POINT ( 'NONE',  ( 2.976309490518674217, -0.1360139883382974202, -1.836174483004118674 ) ) ;
#18997 = EDGE_CURVE ( 'NONE', #155561, #12134, #69849, .T. ) ;
#18996 = COLOUR_RGB ( '', 0.31764706, 0.68627451, 0.89019608) ;
#18998 = CARTESIAN_POINT ( 'NONE',  ( 8.259941899223605333, 10.65968485389279508, -1.599625672291268286 ) ) ;
#18999 = CARTESIAN_POINT ( 'NONE',  ( 3.803562306130504389, -0.5304149723801485639, 1.746809896627635084 ) ) ;
#19000 = CARTESIAN_POINT ( 'NONE',  ( 4.904922738988922504, -1.081064280317966420, -1.701948707654332704 ) ) ;
#19001 = CARTESIAN_POINT ( 'NONE',  ( -7.343712760096452463, 11.71941532008788833, -0.7998128361456291469 ) ) ;
#19003 = CARTESIAN_POINT ( 'NONE',  ( -7.632314129850253259, 7.869064337772231355, 0.7998128361456341429 ) ) ;
#19002 = CARTESIAN_POINT ( 'NONE',  ( 4.381858629716777642, 1.474804143916402355, 1.715883708886431158 ) ) ;
#19004 = CARTESIAN_POINT ( 'NONE',  ( 6.405314555823123257, 1.748765893162683271, 1.173091541056320297 ) ) ;
#19005 = CARTESIAN_POINT ( 'NONE',  ( -1.997444822565112910, 3.480956003829108081, -0.4000000000000817901 ) ) ;
#19006 = CARTESIAN_POINT ( 'NONE',  ( 3.437997351728830697, 1.311287738946330439, 1.602184970737066116 ) ) ;
#19007 = CARTESIAN_POINT ( 'NONE',  ( 10.05353459973327368, 11.68787744023238417, -1.199719254218440723 ) ) ;
#19008 = CARTESIAN_POINT ( 'NONE',  ( 0.6801582343749761339, 1.838541667008058988, -1.178068619123876282 ) ) ;
#19009 = SHAPE_DEFINITION_REPRESENTATION ( #47232, #211717 ) ;
#19011 = CARTESIAN_POINT ( 'NONE',  ( 1.682126184939515934, -1.031041751839639087, 1.627202258603721363 ) ) ;
#19010 = CARTESIAN_POINT ( 'NONE',  ( -7.181014916732457287, 11.52960116949655678, -0.7998128361456291469 ) ) ;
#19012 = UNCERTAINTY_MEASURE_WITH_UNIT (LENGTH_MEASURE( 1.000000000000000082E-05 ), #20529, 'distance_accuracy_value', 'NONE');
#19013 = CARTESIAN_POINT ( 'NONE',  ( 0.000000000000000000, 0.06547992991065912372, -3.399419719642636561 ) ) ;
#19014 = CARTESIAN_POINT ( 'NONE',  ( 6.912958093653829295, -1.524444945649571004, 1.246696689375533795 ) ) ;
#19015 = CARTESIAN_POINT ( 'NONE',  ( 4.923019175093585886, 5.876515471431535076, -1.082531754730548412 ) ) ;
#19016 = CARTESIAN_POINT ( 'NONE',  ( 5.892130686423356245, 5.977214202646935703, -0.03562020706840245132 ) ) ;
#19017 = CARTESIAN_POINT ( 'NONE',  ( -4.790108344329849110, 4.482881244673243337, 0.7998128361456341429 ) ) ;
#19018 = CARTESIAN_POINT ( 'NONE',  ( 1.459560619642571000, -1.873223059428649639, 1.193793739728800762 ) ) ;
#19019 = CARTESIAN_POINT ( 'NONE',  ( 3.258910125681306891, -1.595695288142566337, 1.374458643164514937 ) ) ;
#19020 = CARTESIAN_POINT ( 'NONE',  ( -5.264308783856126439, 9.363720357799287797, -0.7998128361456362523 ) ) ;
#19021 = CARTESIAN_POINT ( 'NONE',  ( 5.587931867126699537, 9.671004278289832001, -0.7998128361456291469 ) ) ;
#19022 = CARTESIAN_POINT ( 'NONE',  ( 0.6603357414211168397, -0.6217855776655777378, -1.754263843975149006 ) ) ;
#19023 = CARTESIAN_POINT ( 'NONE',  ( 5.452350330990040739, 9.512825819463730070, 0.7998128361456462443 ) ) ;
#19024 = CARTESIAN_POINT ( 'NONE',  ( 4.310602774141044868, 7.116454772218158809, -1.199719254218452047 ) ) ;
#19025 = CARTESIAN_POINT ( 'NONE',  ( -6.970300371201519241, 7.304640985922785212, 0.7216878364870317197 ) ) ;
#19026 = CARTESIAN_POINT ( 'NONE',  ( -7.321039761699444703, 10.52466824108257804, 1.082531754730549967 ) ) ;
#19027 = CARTESIAN_POINT ( 'NONE',  ( 0.9848172835694012361, -1.340914915981223476, 1.642866500755429948 ) ) ;
#19028 = CARTESIAN_POINT ( 'NONE',  ( -6.261886844665283114, 8.398896966899865646, 1.599625672291269396 ) ) ;
#19030 = CARTESIAN_POINT ( 'NONE',  ( 4.703538834289092030, -1.515240342570793430, -1.246145567450624991 ) ) ;
#19029 = CARTESIAN_POINT ( 'NONE',  ( -0.6125000000000089262, 1.041666666666662966, 1.060881119635898040 ) ) ;
#19031 = CARTESIAN_POINT ( 'NONE',  ( 3.327187652246216931, 0.05129554954072869377, 2.161254785723889515 ) ) ;
#19032 = CARTESIAN_POINT ( 'NONE',  ( 1.944624168438695566, -1.479605912621816399, -1.095697124569312564 ) ) ;
#19033 = CARTESIAN_POINT ( 'NONE',  ( -4.053570677780473197, 7.570253647979210854, -0.4034679714342986889 ) ) ;
#19034 = EDGE_CURVE ( 'NONE', #59141, #16779, #45477, .T. ) ;
#19035 = CARTESIAN_POINT ( 'NONE',  ( -1.364683531250014514, -0.9489583329919112353, -0.7879004041258359514 ) ) ;
#19036 = B_SPLINE_CURVE_WITH_KNOTS ( 'NONE', 3,
 ( #144977, #17043, #132987, #210982, #131929, #100449 ),
 .UNSPECIFIED., .F., .F.,
 ( 4, 2, 4 ),
 ( 0.001877801214402442754, 0.002190719108449961511, 0.002503637002497480051 ),
 .UNSPECIFIED. ) ;
#19037 = CARTESIAN_POINT ( 'NONE',  ( 4.786887925959832479, 1.292461281945065599, 1.165648420485969394 ) ) ;
#19038 = CARTESIAN_POINT ( 'NONE',  ( -3.501245407923943898, 16.00000000000493117, -11.28115623562582748 ) ) ;
#19039 = CARTESIAN_POINT ( 'NONE',  ( 6.670248388243460447, 6.884303995813253252, -0.7216878364870257245 ) ) ;
#19040 = CARTESIAN_POINT ( 'NONE',  ( -10.05286969158539812, 5.876479340494690895, 5.831501649199077875 ) ) ;
#19041 = CARTESIAN_POINT ( 'NONE',  ( 2.219795081190904629, -2.096929600374438429, 0.5247480557022954351 ) ) ;
#19042 = CARTESIAN_POINT ( 'NONE',  ( 3.567732365556259833, 1.591074578583808075, -1.238131541301431549 ) ) ;
#19043 = CARTESIAN_POINT ( 'NONE',  ( -0.4170821662629279336, 3.033599471985628959, -0.4170821662629279336 ) ) ;
#19044 = CARTESIAN_POINT ( 'NONE',  ( 0.8136072859011161951, -0.3160970183575459447, 2.138355382504661506 ) ) ;
#19045 = CARTESIAN_POINT ( 'NONE',  ( 3.168780698033875076, -1.820990468880798296, -0.7558852700480926945 ) ) ;
#19046 = ADVANCED_FACE ( 'NONE', ( #100279 ), #144822, .T. ) ;
#19047 = CARTESIAN_POINT ( 'NONE',  ( -0.08058608058608696112, -9.999999999999994671, 10.99970480893081870 ) ) ;
#19048 = CARTESIAN_POINT ( 'NONE',  ( 3.280740747204694774, 1.754465757641409995, -0.8330476171748876224 ) ) ;
#19050 = ORIENTED_EDGE ( 'NONE', *, *, #117783, .T. ) ;
#19049 = CARTESIAN_POINT ( 'NONE',  ( -8.771762197917311710, 13.17754696430482042, 0.7216878364870317197 ) ) ;
#19052 = EDGE_CURVE ( 'NONE', #210292, #17872, #80252, .T. ) ;
#19051 = CARTESIAN_POINT ( 'NONE',  ( -5.438229012412903352, 6.477593614970734492, -1.082531754730549967 ) ) ;
#19053 = CARTESIAN_POINT ( 'NONE',  ( -0.2106854629475037044, 2.877407191259284680, -2.485613835449883346 ) ) ;
#19054 = CARTESIAN_POINT ( 'NONE',  ( 4.712340909201580885, 7.655425606447271214, -1.199719254218452047 ) ) ;
#19055 = CARTESIAN_POINT ( 'NONE',  ( -5.490125858891038213, 5.369844688319787451, -0.7998128361456362523 ) ) ;
#19057 = EDGE_LOOP ( 'NONE', ( #189662, #16217, #33632, #103582 ) ) ;
#19056 = CARTESIAN_POINT ( 'NONE',  ( -4.769436176957319695, 8.786368983084006601, 0.7998128361456281477 ) ) ;
#19058 = CARTESIAN_POINT ( 'NONE',  ( -9.124274191872636663, 11.66807252865000244, -1.443375672974058777 ) ) ;
#19059 = CARTESIAN_POINT ( 'NONE',  ( 0.07755575628183573877, -0.002876890934064984650, -2.188974970840869005 ) ) ;
#19060 = CARTESIAN_POINT ( 'NONE',  ( 3.285556943750000514, -2.763541666188707335, 1.896917185911906500 ) ) ;
#19061 = CARTESIAN_POINT ( 'NONE',  ( 4.645332984504850771, 1.754159843842403976, -0.8783796436172899291 ) ) ;
#19062 = CARTESIAN_POINT ( 'NONE',  ( 2.215470409936692420, 1.956561601830292485, 0.4872017847364697452 ) ) ;
#19063 = ORIENTED_EDGE ( 'NONE', *, *, #192235, .F. ) ;
#19064 = CARTESIAN_POINT ( 'NONE',  ( 3.766910327102332978, -0.2117226681838789426, -2.106763584193247940 ) ) ;
#19065 = CARTESIAN_POINT ( 'NONE',  ( -1.500000000000011324, 3.202083334016150307, 0.8660254037844403729 ) ) ;
#19067 = CARTESIAN_POINT ( 'NONE',  ( -5.392392409933270514, 7.314210449720692786, 1.599625672291269396 ) ) ;
#19066 = CARTESIAN_POINT ( 'NONE',  ( 0.07479286986305545837, 0.7422478802248284602, -1.939684878352589070 ) ) ;
#19068 = CARTESIAN_POINT ( 'NONE',  ( 3.380630241506640932, 1.664009615612583204, -0.7882418170854917916 ) ) ;
#19069 = VERTEX_POINT ( 'NONE', #79766 ) ;
#19070 = CARTESIAN_POINT ( 'NONE',  ( -8.483651433849100698, 10.92067931095586886, 1.599625672291269396 ) ) ;
#19071 = CARTESIAN_POINT ( 'NONE',  ( 0.3000000002817697631, 3.198312376128888967, 0.5146719259195579044 ) ) ;
#19073 = AXIS2_PLACEMENT_3D ( 'NONE', #123548, #92046, #174360 ) ;
#19072 = CARTESIAN_POINT ( 'NONE',  ( 4.781546299372162245, 0.2051969522943071500, -2.110614603223801122 ) ) ;
#19074 = CARTESIAN_POINT ( 'NONE',  ( 6.825078400183545391, 0.005516643811322498661, 1.755566376062764000 ) ) ;
#19075 = CARTESIAN_POINT ( 'NONE',  ( 7.935599982700328958, 8.152621489438862667, 0.7998128361456481317 ) ) ;
#19076 = CARTESIAN_POINT ( 'NONE',  ( 5.940714679333914283, 0.3976391751681263576, 2.021873298595587176 ) ) ;
#19078 = CARTESIAN_POINT ( 'NONE',  ( 2.524749765808989466, -1.717266272480859834, 0.6646640004178904215 ) ) ;
#19077 = CARTESIAN_POINT ( 'NONE',  ( 1.310759002261387529, -1.470036769156491063, 1.141183394468782364 ) ) ;
#19079 = CARTESIAN_POINT ( 'NONE',  ( 7.886038904643079661, 12.35212915539230139, -0.7998128361456352531 ) ) ;
#19080 = PRESENTATION_STYLE_ASSIGNMENT (( #4937 ) ) ;
#19081 = CYLINDRICAL_SURFACE ( 'NONE', #1016, 0.3999999999999997446 ) ;
#19082 = CARTESIAN_POINT ( 'NONE',  ( 10.99574878476024153, -7.889012432655408524, -0.3098035853330123324 ) ) ;
#19083 = CARTESIAN_POINT ( 'NONE',  ( 2.754729969050898841, 0.7443088323898851000, 2.077706851784946185 ) ) ;
#19084 = CARTESIAN_POINT ( 'NONE',  ( 4.921284695982240720, -0.1178685990214298068, 2.259476483347002240 ) ) ;
#19085 = CARTESIAN_POINT ( 'NONE',  ( 3.520720487665735643, 0.3006478860226591276, 1.993893439002386581 ) ) ;
#19086 = CARTESIAN_POINT ( 'NONE',  ( -6.887178846062109727, 10.01849717283904262, -1.082531754730537976 ) ) ;
#19087 = CARTESIAN_POINT ( 'NONE',  ( 5.115404481452859642, 1.485474843905653985, 1.036646722175238011 ) ) ;
#19088 = CARTESIAN_POINT ( 'NONE',  ( 4.715990674440117658, 0.9792849278024118309, -1.646335200727979897 ) ) ;
#19089 = CARTESIAN_POINT ( 'NONE',  ( 1.364683531249990311, 5.176041667008085767, 0.7879004041258500513 ) ) ;
#19090 = CARTESIAN_POINT ( 'NONE',  ( 4.293796034307355569, -0.7555264168055545460, 1.821139111365249308 ) ) ;
#19091 = CARTESIAN_POINT ( 'NONE',  ( 5.418772907935071714, 1.728844841293469159, 0.7149302089985640762 ) ) ;
#19092 = CARTESIAN_POINT ( 'NONE',  ( 4.896841239116665356, 0.3175000240179836619, 1.833586397851859839 ) ) ;
#19093 = CARTESIAN_POINT ( 'NONE',  ( -1.001543065824772872E-14, 5.571875000341416140, 1.575800808251672791 ) ) ;
#19094 = AXIS2_PLACEMENT_3D ( 'NONE', #93354, #144268, #177789 ) ;
#19095 = CARTESIAN_POINT ( 'NONE',  ( 0.7082206942033396624, 1.197301205363930254, -1.622488844446705381 ) ) ;
#19097 = CARTESIAN_POINT ( 'NONE',  ( 1.242952776902699785, 0.4124841525564198474, 2.065099357090140586 ) ) ;
#19096 = CARTESIAN_POINT ( 'NONE',  ( -10.66756793585402363, 11.33991743478486391, 0.7998128361456462443 ) ) ;
#19098 = CIRCLE ( 'NONE', #188725, 0.7499999999999997780 ) ;
#19099 = CARTESIAN_POINT ( 'NONE',  ( 8.563946585326370098, 13.14302144952281814, 0.7998128361456462443 ) ) ;
#19101 = CARTESIAN_POINT ( 'NONE',  ( -9.480175724453545172, 12.08329098332774265, 1.599625672291281386 ) ) ;
#19100 = CARTESIAN_POINT ( 'NONE',  ( 1.403499169903295263, 7.376709478543810761, -4.304123474983216902 ) ) ;
#19102 = CARTESIAN_POINT ( 'NONE',  ( 3.392942708002244068, -2.044739723715986113, -0.5619712599038150236 ) ) ;
#19103 = CARTESIAN_POINT ( 'NONE',  ( -4.955918092712652268, 4.886086657537050293, 0.4932186882876873901 ) ) ;
#19104 = CARTESIAN_POINT ( 'NONE',  ( 1.845969175824228925, -1.322618866652914393, -1.526557775719493915 ) ) ;
#19105 = CARTESIAN_POINT ( 'NONE',  ( -1.364683531250000748, 1.759375000341421913, 0.000000000000000000 ) ) ;
#19106 = CARTESIAN_POINT ( 'NONE',  ( -2.304522924643024773, 5.632434478818063361, 0.7216878364870317197 ) ) ;
#19107 = CARTESIAN_POINT ( 'NONE',  ( 4.009460741339333723, 5.700790169694431420, -1.599625672291256295 ) ) ;
#19108 = VERTEX_POINT ( 'NONE', #50469 ) ;
#19109 = CARTESIAN_POINT ( 'NONE',  ( 2.108864864398530159, 1.603267699958549342, -1.450045708023157687 ) ) ;
#19110 = CARTESIAN_POINT ( 'NONE',  ( 6.890000000000009450, -0.01081285896028030651, 2.279840171838913854 ) ) ;
#19112 = CARTESIAN_POINT ( 'NONE',  ( 4.094037528094967016, 3.811616672697253350, -2.445516385416635963 ) ) ;
#19111 = CARTESIAN_POINT ( 'NONE',  ( 3.223806664999388172, 6.983134552466421674, -0.7998128361456362523 ) ) ;
#19113 = PLANE ( 'NONE',  #48041 ) ;
#19114 = CARTESIAN_POINT ( 'NONE',  ( -2.282425430171015623, 5.569261388197155327, -0.5172846513131660329 ) ) ;
#19115 = CARTESIAN_POINT ( 'NONE',  ( -6.832946231607472498, 9.955225789308602913, 1.082531754730549967 ) ) ;
#19116 = CARTESIAN_POINT ( 'NONE',  ( 1.452940684028160234, -1.882004992133184285, -1.122693704575933316 ) ) ;
#19117 = CARTESIAN_POINT ( 'NONE',  ( 4.151089631643987587, 2.978105173886053336, 0.7750000000000117906 ) ) ;
#19119 = CARTESIAN_POINT ( 'NONE',  ( 0.6823417656249969321, 12.02604166700806054, -1.181850606188757036 ) ) ;
#19118 = CARTESIAN_POINT ( 'NONE',  ( 1.112636518468415270, -1.019398372879092962, -2.019907345245135932 ) ) ;
#19120 = CARTESIAN_POINT ( 'NONE',  ( -9.345647958521597687, 9.797677461230342999, 0.7998128361456462443 ) ) ;
#19121 = EDGE_CURVE ( 'NONE', #115058, #96370, #211809, .T. ) ;
#19122 = CARTESIAN_POINT ( 'NONE',  ( -4.894130264408866893, 6.732904613275549899, -1.443375672974051449 ) ) ;
#19123 = CARTESIAN_POINT ( 'NONE',  ( -1.364683531250014514, 2.051041667008086655, -0.7879004041258289570 ) ) ;
#19124 = CARTESIAN_POINT ( 'NONE',  ( 4.771497086726927073, 8.161215468402982509, 0.7801120568680236511 ) ) ;
#19125 = CARTESIAN_POINT ( 'NONE',  ( 0.7500000000000006661, 9.166666666666669627, -1.299038105676657340 ) ) ;
#19126 = CARTESIAN_POINT ( 'NONE',  ( 3.879312468746206832, 1.623315624747388775, -0.5835212994509741957 ) ) ;
#19127 = CARTESIAN_POINT ( 'NONE',  ( 5.415556014015861841, 5.282846535965431300, -0.7998128361456481317 ) ) ;
#19128 = CARTESIAN_POINT ( 'NONE',  ( 1.563349520526525538, 1.744638119327382553, -0.2959517217632592900 ) ) ;
#19130 = AXIS2_PLACEMENT_3D ( 'NONE', #195268, #29569, #13304 ) ;
#19129 = CARTESIAN_POINT ( 'NONE',  ( 4.999154358079874960, 1.837129776665728187, -1.222328095618854693 ) ) ;
#19131 = ORIENTED_EDGE ( 'NONE', *, *, #151247, .T. ) ;
#19132 = CARTESIAN_POINT ( 'NONE',  ( 4.429947715222688487, -1.979980911821906497, 0.3981057063161990706 ) ) ;
#19133 = CARTESIAN_POINT ( 'NONE',  ( -6.017840079619296567, 8.114175741012878973, -1.599625672291271394 ) ) ;
#19134 = CARTESIAN_POINT ( 'NONE',  ( 4.728138764314923748, 2.011206665557175199, 0.1455158850461671372 ) ) ;
#19136 = ORIENTED_EDGE ( 'NONE', *, *, #189421, .T. ) ;
#19135 = CARTESIAN_POINT ( 'NONE',  ( 4.570457401048643398, 0.6997940171077315918, 1.671178544893426654 ) ) ;
#19137 = CARTESIAN_POINT ( 'NONE',  ( 2.553401164250346245, 0.5009360343536627402, -1.802255699741683870 ) ) ;
#19138 = EDGE_CURVE ( 'NONE', #170509, #198869, #28463, .T. ) ;
#19139 = CARTESIAN_POINT ( 'NONE',  ( 6.621730190220365131, -1.769489810573118049, 0.4491385735008179836 ) ) ;
#19140 = CARTESIAN_POINT ( 'NONE',  ( 1.582132296805271787, 0.9858968508435607125, 1.638552900098678045 ) ) ;
#19142 = PRESENTATION_LAYER_ASSIGNMENT (  '', '', ( #88444 ) ) ;
#19141 = CARTESIAN_POINT ( 'NONE',  ( -6.132724857352506831, 6.712246147164017351, 0.7681735678050619631 ) ) ;
#19143 = CARTESIAN_POINT ( 'NONE',  ( -10.52626310920980757, 3.679096435225583939, -5.196420034295205603 ) ) ;
#19144 = B_SPLINE_CURVE_WITH_KNOTS ( 'NONE', 3,
 ( #186542, #185469, #38171, #8858, #103169, #169230, #152986, #207054, #107503, #86918, #89070, #56559, #40316, #72786, #104244, #136746 ),
 .UNSPECIFIED., .F., .F.,
 ( 4, 3, 3, 3, 3, 4 ),
 ( 0.000000000000000000, 3.357617230303705058E-05, 6.715207102180654238E-05, 0.0001007279560762661569, 0.0001343044553218104679, 0.0001562161319167434893 ),
 .UNSPECIFIED. ) ;
#19145 = CARTESIAN_POINT ( 'NONE',  ( 0.6823417656249899377, 3.488541667008085323, -1.181850606188754593 ) ) ;
#19146 = CARTESIAN_POINT ( 'NONE',  ( 0.2813230411330031600, 0.1852680230450229892, -1.903361379684164412 ) ) ;
#19147 = AXIS2_PLACEMENT_3D ( 'NONE', #2693, #15763, #131715 ) ;
#19148 = CARTESIAN_POINT ( 'NONE',  ( 5.017926250833595780, 7.907978821730911712, -1.082531754730548412 ) ) ;
#19149 = CARTESIAN_POINT ( 'NONE',  ( 2.119516022818414669, 0.3384452847540948550, -1.932298432780136244 ) ) ;
#19150 = EDGE_CURVE ( 'NONE', #183272, #133306, #131766, .T. ) ;
#19151 = DIRECTION ( 'NONE',  ( 0.000000000000000000, 0.000000000000000000, -1.000000000000000000 ) ) ;
#19152 = CARTESIAN_POINT ( 'NONE',  ( -4.634908411025374875, 6.500755460986618495, 1.599625672291263179 ) ) ;
#19153 = CARTESIAN_POINT ( 'NONE',  ( 5.291314375706784645, -0.05428322906628547939, -2.120082430678168706 ) ) ;
#19155 = CARTESIAN_POINT ( 'NONE',  ( -11.69380381030441107, 8.410673437356566140, -1.083569014401829955 ) ) ;
#19154 = CARTESIAN_POINT ( 'NONE',  ( 8.062294901620731480, 12.55776115186623620, 1.040834085586084257E-14 ) ) ;
#19156 = CARTESIAN_POINT ( 'NONE',  ( 6.819606788702130551, -1.912791534441590668, 0.4766558377571166183 ) ) ;
#19157 = CARTESIAN_POINT ( 'NONE',  ( 0.6823417656249899377, 2.592708333674753618, 1.181850606188767472 ) ) ;
#19158 = CARTESIAN_POINT ( 'NONE',  ( 0.5451820649361303062, 0.1524121550021810545, 2.007518037476815564 ) ) ;
#19159 = ORIENTED_EDGE ( 'NONE', *, *, #90678, .T. ) ;
#19160 = CARTESIAN_POINT ( 'NONE',  ( 1.124788838837559535, 0.4171406989393853793, 2.075574515046583191 ) ) ;
#19161 = CARTESIAN_POINT ( 'NONE',  ( 11.35739107624612210, 7.533900434079529695, -3.740981627317509606 ) ) ;
#19162 = CARTESIAN_POINT ( 'NONE',  ( 2.734898984476673789, -1.980466496001157317, -0.6033880717724803278 ) ) ;
#19163 = CARTESIAN_POINT ( 'NONE',  ( 5.225741863424510747, 5.061396693608882558, 0.7998128361456352531 ) ) ;
#19164 = CARTESIAN_POINT ( 'NONE',  ( 3.898851692381625877, 6.706354853490643642, -1.199719254218452047 ) ) ;
#19165 = ORIENTED_EDGE ( 'NONE', *, *, #33910, .F. ) ;
#19167 = CARTESIAN_POINT ( 'NONE',  ( 5.691725559638619814, 5.534767995866836543, 1.040834085586084257E-14 ) ) ;
#19166 = CARTESIAN_POINT ( 'NONE',  ( 4.822261998019022222, 2.000437409348213347, 0.6074620046824655839 ) ) ;
#19170 = ORIENTED_EDGE ( 'NONE', *, *, #210167, .T. ) ;
#19169 = CARTESIAN_POINT ( 'NONE',  ( 2.965264322261091934, -1.482184020574893069, -1.041122702216127571 ) ) ;
#19168 = CARTESIAN_POINT ( 'NONE',  ( 2.537895388257872753, 0.8626947210231518115, -1.608888323311054691 ) ) ;
#19171 = CARTESIAN_POINT ( 'NONE',  ( 6.164705905600973423, -1.563586322211576674, 1.557672334054376773 ) ) ;
#19172 = CARTESIAN_POINT ( 'NONE',  ( 9.270933768482571224, 13.53532804777227661, 6.807664277187561730 ) ) ;
#19173 = CARTESIAN_POINT ( 'NONE',  ( 5.631908123138919642, -1.395923778694251105, -1.709176034821748624 ) ) ;
#19174 = CARTESIAN_POINT ( 'NONE',  ( -1.364683531250014514, 9.151041667008062319, -0.7879004041258335089 ) ) ;
#19175 = VERTEX_POINT ( 'NONE', #194584 ) ;
#19176 = CARTESIAN_POINT ( 'NONE',  ( 4.125576785117724299, -0.3237648511281773778, 1.884507068624697190 ) ) ;
#19177 = CARTESIAN_POINT ( 'NONE',  ( -3.541704441667874903, 5.155074486744371853, -1.599625672291256295 ) ) ;
#19178 = CARTESIAN_POINT ( 'NONE',  ( 7.259501185113382604, 10.55683625168592243, -1.199719254218441611 ) ) ;
#19179 = CARTESIAN_POINT ( 'NONE',  ( 5.881320641815352523, -0.05461762546566178989, 2.069818975884097689 ) ) ;
#19180 = CARTESIAN_POINT ( 'NONE',  ( 1.360316468749987573, 0.2760416670081234369, 0.7853790794158700406 ) ) ;
#19181 = CARTESIAN_POINT ( 'NONE',  ( 5.463572716182829581, 6.436884926043849653, 1.082531754730560403 ) ) ;
#19182 = CARTESIAN_POINT ( 'NONE',  ( 6.620655732516649294, -0.002413161512292843602, 2.173887093218459743 ) ) ;
#19183 = CARTESIAN_POINT ( 'NONE',  ( -6.326802395788107880, 6.950450678040672514, 0.9045734915664763731 ) ) ;
#19184 = CARTESIAN_POINT ( 'NONE',  ( -9.477100695693458476, -6.554910290221380720, 0.2834499523633453588 ) ) ;
#19185 = ORIENTED_EDGE ( 'NONE', *, *, #166507, .F. ) ;
#19186 = CARTESIAN_POINT ( 'NONE',  ( -3.474999999999997868, -2.070833333333331971, 2.006292185433951047 ) ) ;
#19187 = ADVANCED_FACE ( 'NONE', ( #146937 ), #182583, .F. ) ;
#19188 = CARTESIAN_POINT ( 'NONE',  ( 3.462029368274913477, 0.8381641302350505418, 1.672297462726477946 ) ) ;
#19189 = CARTESIAN_POINT ( 'NONE',  ( 1.499999999999993117, 10.85416666666666785, 0.8660254037844408170 ) ) ;
#19190 = CARTESIAN_POINT ( 'NONE',  ( -7.876924059859742755, 8.292092279365579799, 1.040834085586084257E-14 ) ) ;
#19191 = CARTESIAN_POINT ( 'NONE',  ( 3.923105346307896202, 5.670318552149568703, -1.599625672291269396 ) ) ;
#19192 = CARTESIAN_POINT ( 'NONE',  ( 4.364835388595708743, 7.179726155748598515, 1.199719254218462483 ) ) ;
#19193 = CARTESIAN_POINT ( 'NONE',  ( 6.977413707831522593, -0.1558467299303326059, 2.036386162850227333 ) ) ;
#19194 = CARTESIAN_POINT ( 'NONE',  ( 0.9312678054614745848, -1.591333336790928366, -1.238303555203337458 ) ) ;
#19195 = CARTESIAN_POINT ( 'NONE',  ( -9.809487834687324437, 11.40315621434539395, 1.199719254218462483 ) ) ;
#19196 = CARTESIAN_POINT ( 'NONE',  ( 6.692885107001518286, 7.837396042037102717, -1.199719254218452047 ) ) ;
#19197 = CARTESIAN_POINT ( 'NONE',  ( -15.75000000000000000, 11.29999999999998117, 3.199999999999997957 ) ) ;
#19198 = CARTESIAN_POINT ( 'NONE',  ( 1.218978173989828884, -0.05078841826402366588, 2.191026318449231791 ) ) ;
#19199 = CARTESIAN_POINT ( 'NONE',  ( 6.111906964637446649, -1.811269838261083232, 0.2284818145076653595 ) ) ;
#19200 = CARTESIAN_POINT ( 'NONE',  ( -4.322352044658376968, 3.937165561723182883, 0.7998128361456341429 ) ) ;
#19201 = CARTESIAN_POINT ( 'NONE',  ( 4.421367491832268293, 7.211993602896056288, 1.082531754730549078 ) ) ;
#19202 = CARTESIAN_POINT ( 'NONE',  ( 10.26082332744404368, 10.86538205830655279, -0.7998128361456281477 ) ) ;
#19203 = CARTESIAN_POINT ( 'NONE',  ( 5.054492339796319733, 4.791329239384148231, -0.7998128361456211532 ) ) ;
#19204 = CARTESIAN_POINT ( 'NONE',  ( 6.048345925472166762, 10.07050432311064903, 0.7216878364870317197 ) ) ;
#19205 = ORIENTED_EDGE ( 'NONE', *, *, #213637, .T. ) ;
#19207 = CARTESIAN_POINT ( 'NONE',  ( 0.3287710483851979393, 1.386612999538240576, -1.459627859818838802 ) ) ;
#19206 = CARTESIAN_POINT ( 'NONE',  ( 3.702549152423353807, 1.581054339307564449, 0.9433870219286569769 ) ) ;
#19208 = CARTESIAN_POINT ( 'NONE',  ( 2.847332689139534523, -1.183592279326161290, 1.970102427710369808 ) ) ;
#19210 = CARTESIAN_POINT ( 'NONE',  ( 0.6196752394443981737, 1.841814893205738102, -0.2651871859581377833 ) ) ;
#19209 = CARTESIAN_POINT ( 'NONE',  ( -0.1290005225502918740, 6.946858002156244716, -2.769053915224591211 ) ) ;
#19211 = CARTESIAN_POINT ( 'NONE',  ( 1.737500000000001155, -0.5833333333333314830, 3.009438278150922130 ) ) ;
#19212 = CARTESIAN_POINT ( 'NONE',  ( -5.427341564172148303, 5.226320001155936090, 0.000000000000000000 ) ) ;
#19213 = DIRECTION ( 'NONE',  ( -1.000000000000000000, 0.000000000000000000, -5.551115123125765446E-17 ) ) ;
#19214 = CARTESIAN_POINT ( 'NONE',  ( 4.359561026920276916, -1.481784043772149229, -1.208992945495937610 ) ) ;
#19215 = CARTESIAN_POINT ( 'NONE',  ( -8.350932551013499960, 11.83017284523606172, -1.199719254218446718 ) ) ;
#19216 = MANIFOLD_SOLID_BREP ( 'Fillet3', #122762 ) ;
#19217 = CARTESIAN_POINT ( 'NONE',  ( 6.292946923374557855, 6.878031543426355476, -0.7329977330566839200 ) ) ;
#19218 = CARTESIAN_POINT ( 'NONE',  ( -5.587368702607575344, 8.572328348800551723, 1.082531754730550855 ) ) ;
#19220 = CARTESIAN_POINT ( 'NONE',  ( 2.360033908006432757, 0.7977434165707707470, 1.692156362554583460 ) ) ;
#19219 = CARTESIAN_POINT ( 'NONE',  ( 3.333613130510120648, 0.9378223671878234136, -1.868666107883134142 ) ) ;
#19221 = CARTESIAN_POINT ( 'NONE',  ( 8.270110514656037637, 8.750809809961280550, 0.7216878364870458196 ) ) ;
#19222 = CARTESIAN_POINT ( 'NONE',  ( -1.364683531249997417, 5.821875000341418804, 1.214306433183764966E-14 ) ) ;
#19223 = CARTESIAN_POINT ( 'NONE',  ( 3.245385237338119566, 1.740626721681370670, -0.003331538806947489072 ) ) ;
#19224 = CARTESIAN_POINT ( 'NONE',  ( 3.551346171775753735, 6.230655402791975384, 1.199719254218462483 ) ) ;
#19226 = CARTESIAN_POINT ( 'NONE',  ( 4.680589345215795838, 6.483773540883647435, -1.599625672291256295 ) ) ;
#19225 = CARTESIAN_POINT ( 'NONE',  ( -1.500000000000008216, 11.53125000068279427, 3.469446951953614189E-15 ) ) ;
#19227 = CARTESIAN_POINT ( 'NONE',  ( 4.002375702155434922, -0.5437682074083802775, -1.636994321040524447 ) ) ;
#19228 = CARTESIAN_POINT ( 'NONE',  ( -7.497822643557261024, 8.706213491360317747, -1.199719254218446718 ) ) ;
#19229 = CARTESIAN_POINT ( 'NONE',  ( 3.931328349035985603, -1.512150646884598215, -1.586510368271301541 ) ) ;
#19230 = CARTESIAN_POINT ( 'NONE',  ( -1.426546532658534927, 7.396047039057213723, 4.272878514717270093 ) ) ;
#19231 = CARTESIAN_POINT ( 'NONE',  ( 9.579253414572376002, -9.994362535427860905, -0.1002978391578448342 ) ) ;
#19232 = CARTESIAN_POINT ( 'NONE',  ( 3.590846382830733763, 2.117060681034032221, 0.4805534470472500042 ) ) ;
#19233 = CARTESIAN_POINT ( 'NONE',  ( 2.437895498511342574, 0.8609710149188254391, -1.609920059450341778 ) ) ;
#19234 = DIRECTION ( 'NONE',  ( -0.000000000000000000, -1.000000000000000000, -0.000000000000000000 ) ) ;
#19235 = CARTESIAN_POINT ( 'NONE',  ( 5.102788515576859751, 1.957488760995762300, 0.8075332785216599030 ) ) ;
#19236 = EDGE_CURVE ( 'NONE', #214357, #6682, #162749, .T. ) ;
#19237 = VERTEX_POINT ( 'NONE', #29966 ) ;
#19239 = CARTESIAN_POINT ( 'NONE',  ( -0.6823417656250212460, 2.613541667008084879, 1.181850606188767472 ) ) ;
#19238 = CARTESIAN_POINT ( 'NONE',  ( 5.425394459833968064, -1.452027641166652172, -1.773832485185691032 ) ) ;
#19240 = CARTESIAN_POINT ( 'NONE',  ( 9.378489572351044856, 11.96465713920816043, -1.599625672291262513 ) ) ;
#19241 = CARTESIAN_POINT ( 'NONE',  ( 1.330900338397854155, 1.421537331630345014, -1.573617108223644312 ) ) ;
#19242 = CARTESIAN_POINT ( 'NONE',  ( -5.612712406377534435, 5.650512016969639895, 0.7216878364870317197 ) ) ;
#19243 = CARTESIAN_POINT ( 'NONE',  ( 0.000000000000000000, 0.000000000000000000, 0.000000000000000000 ) ) ;
#19244 = CARTESIAN_POINT ( 'NONE',  ( -4.378920427089552092, 8.052564898339037214, 0.7216878364870317197 ) ) ;
#19245 = CARTESIAN_POINT ( 'NONE',  ( -1.402160292154681736E-14, 12.09375000068279782, 1.732050807568881190 ) ) ;
#19248 = VERTEX_POINT ( 'NONE', #67739 ) ;
#19247 = CARTESIAN_POINT ( 'NONE',  ( 1.436510670779034937, -1.237796341723711002, -1.844280071174006164 ) ) ;
#19246 = TOROIDAL_SURFACE ( 'NONE', #168011, 3.970406073902761790, 0.08000000000000000167 ) ;
#19249 = CARTESIAN_POINT ( 'NONE',  ( 5.889296118903345700, -0.7283762112263308941, -1.880435897373772258 ) ) ;
#19251 = CARTESIAN_POINT ( 'NONE',  ( 3.907127581704954888, -1.689070986467123836, 1.183507789072274496 ) ) ;
#19250 = CARTESIAN_POINT ( 'NONE',  ( 5.522248639467795428, 5.337044922334209573, -0.7998128361456231517 ) ) ;
#19253 = CARTESIAN_POINT ( 'NONE',  ( -0.2409995289980003397, 2.873648158547074338, -2.488896373646624749 ) ) ;
#19252 = CARTESIAN_POINT ( 'NONE',  ( 6.475954649182838807, 7.584310507915338562, 1.199719254218452047 ) ) ;
#19254 = CARTESIAN_POINT ( 'NONE',  ( 5.691390622686558487, 9.861982503101517139, 0.7998128361456341429 ) ) ;
#19255 = CARTESIAN_POINT ( 'NONE',  ( -1.642778471875000035, -1.917708332855375897, -2.845375778867859751 ) ) ;
#19256 = CARTESIAN_POINT ( 'NONE',  ( 0.4981332788140432899, -0.7063641614380437028, -1.967824727186429978 ) ) ;
#19257 = CARTESIAN_POINT ( 'NONE',  ( 4.693982515131527755, 1.755768268644173791, 0.9914009648221073778 ) ) ;
#19258 = CARTESIAN_POINT ( 'NONE',  ( 4.124425300631988200, 0.09459923933386081563, 1.838956108544815171 ) ) ;
#19259 = EDGE_CURVE ( 'NONE', #23806, #16236, #47544, .T. ) ;
#19260 = CARTESIAN_POINT ( 'NONE',  ( 5.307127064745490230, 8.279066444590018392, -1.199719254218452935 ) ) ;
#19261 = CARTESIAN_POINT ( 'NONE',  ( 1.236830563851202491, -1.561790747969876714, 0.7321873917187391445 ) ) ;
#19262 = CARTESIAN_POINT ( 'NONE',  ( 0.5148617154710419808, 0.1531739628206352510, 2.010800830040265996 ) ) ;
#19263 = CARTESIAN_POINT ( 'NONE',  ( 1.249136956142880894, 2.263619502511230230, -0.3993902815438779563 ) ) ;
#19264 = CARTESIAN_POINT ( 'NONE',  ( -6.033542053281340856, 6.997886136038390603, -1.199719254218446718 ) ) ;
#19265 = CARTESIAN_POINT ( 'NONE',  ( 1.405971756114566595, -0.5497231165422427068, 2.194469222715933476 ) ) ;
#19266 = CARTESIAN_POINT ( 'NONE',  ( 3.299542427861827498, 1.660325518240006071, 1.295591914420061830 ) ) ;
#19267 = CARTESIAN_POINT ( 'NONE',  ( -3.800028193580205382, 7.655393002477360653, -0.7998128361456481317 ) ) ;
#19268 = CARTESIAN_POINT ( 'NONE',  ( 7.076466111328892694, 10.34329533227067799, -1.199719254218441611 ) ) ;
#19269 = CARTESIAN_POINT ( 'NONE',  ( 6.007671464186825183, 8.102312356341712984, 1.443375672974064550 ) ) ;
#19270 = CARTESIAN_POINT ( 'NONE',  ( 6.625000595499368039, -2.052053476427456502, 3.646059517245236328E-13 ) ) ;
#19271 = CARTESIAN_POINT ( 'NONE',  ( -4.225337428953291230, 8.081310767087481750, 0.7998128361456341429 ) ) ;
#19272 = CARTESIAN_POINT ( 'NONE',  ( 6.114364089638782751, 9.116879957011832403, 1.082531754730558626 ) ) ;
#19273 = CARTESIAN_POINT ( 'NONE',  ( 5.061713581663421557, 6.751138122384800155, 1.419579013000639378 ) ) ;
#19274 = CARTESIAN_POINT ( 'NONE',  ( -5.298539104842322267, 5.076050465271134016, 0.7998128361456341429 ) ) ;
#19275 = CARTESIAN_POINT ( 'NONE',  ( 5.150715375432683985, 2.188637957643671417, 0.3792565894785212000 ) ) ;
#19276 = CARTESIAN_POINT ( 'NONE',  ( 3.082162360440068749, -2.159116730143955998, -0.3741398933536920213 ) ) ;
#19277 = CARTESIAN_POINT ( 'NONE',  ( -5.545448523189368650, 6.428443684264421698, -1.199719254218446718 ) ) ;
#19278 = FACE_OUTER_BOUND ( 'NONE', #13587, .T. ) ;
#19279 = CARTESIAN_POINT ( 'NONE',  ( 5.564887814092526419, 1.486691789297951871, -1.280227714881218892 ) ) ;
#19280 = CARTESIAN_POINT ( 'NONE',  ( 1.364683531249988535, 2.113541667008087099, 0.7879004041258500513 ) ) ;
#19281 = CARTESIAN_POINT ( 'NONE',  ( 6.890000000000008562, 1.260399741928097672, 2.114076522472335462 ) ) ;
#19283 = CARTESIAN_POINT ( 'NONE',  ( -5.585596099150199834, 5.618876325204420930, -0.7216878364870207285 ) ) ;
#19282 =( GEOMETRIC_REPRESENTATION_CONTEXT ( 3 ) GLOBAL_UNCERTAINTY_ASSIGNED_CONTEXT ( ( #84284 ) ) GLOBAL_UNIT_ASSIGNED_CONTEXT ( ( #8436, #60392, #174183 ) ) REPRESENTATION_CONTEXT ( 'NONE', 'WORKASPACE' ) );
#19284 = CARTESIAN_POINT ( 'NONE',  ( 4.693665235656380830, 1.977662049654808740, -0.7657889336421249693 ) ) ;
#19285 = CARTESIAN_POINT ( 'NONE',  ( -7.132998214565509087, 7.494455136514109661, 0.7216878364870317197 ) ) ;
#19286 = ORIENTED_EDGE ( 'NONE', *, *, #182418, .T. ) ;
#19288 = CARTESIAN_POINT ( 'NONE',  ( 6.649309733611729278, -1.732918351142084035, -1.292073167451508686 ) ) ;
#19287 = CARTESIAN_POINT ( 'NONE',  ( -6.482206841109545259, 6.735198534148810090, 0.7216878364870257245 ) ) ;
#19289 = CARTESIAN_POINT ( 'NONE',  ( 6.179819089730593795, 6.104210447640811665, 1.040834085586084257E-14 ) ) ;
#19290 = CARTESIAN_POINT ( 'NONE',  ( 4.774869596704574448, 1.716175909155163382, -0.6674964387535023969 ) ) ;
#19291 = DIRECTION ( 'NONE',  ( 1.000000000000000000, 0.000000000000000000, 0.000000000000000000 ) ) ;
#19292 = CARTESIAN_POINT ( 'NONE',  ( -1.201851678989727383E-14, 3.384375000341421469, 1.575800808251672791 ) ) ;
#19293 = CARTESIAN_POINT ( 'NONE',  ( 1.171013094284451439, 1.035884637911354877, 1.398405216058955514 ) ) ;
#19294 = CARTESIAN_POINT ( 'NONE',  ( 11.33772465723237666, 12.59131699265169502, 3.600000000000073364 ) ) ;
#19295 = CARTESIAN_POINT ( 'NONE',  ( -0.3031628594467480897, 3.278079808138081752, 2.050209013101042643 ) ) ;
#19296 = CARTESIAN_POINT ( 'NONE',  ( -0.4423565646247712979, 3.073250980203129146, 0.4181372721655218783 ) ) ;
#19297 = CARTESIAN_POINT ( 'NONE',  ( 5.717692609583751029, -2.109997883074541392, 0.4692839721026839661 ) ) ;
#19298 = CARTESIAN_POINT ( 'NONE',  ( -2.611917148927046295, 6.198987107056845858, 1.040834085586084257E-14 ) ) ;
#19299 = AXIS2_PLACEMENT_3D ( 'NONE', #141920, #189557, #140853 ) ;
#19300 = CARTESIAN_POINT ( 'NONE',  ( -6.521108698048772467, 9.591415333490143524, -1.082531754730537976 ) ) ;
#19301 = TOROIDAL_SURFACE ( 'NONE', #119576, 0.05000000000000000278, 0.05000000000000000278 ) ;
#19302 = CARTESIAN_POINT ( 'NONE',  ( 4.610339536224768331, -0.9213992672730475508, -1.955631277330005968 ) ) ;
#19303 = CARTESIAN_POINT ( 'NONE',  ( 1.364683531249988535, 3.113541667008083991, 0.7879004041258500513 ) ) ;
#19304 = CARTESIAN_POINT ( 'NONE',  ( 5.360604507329317592, -1.429826957936894960, 1.357393395290319660 ) ) ;
#19305 = CARTESIAN_POINT ( 'NONE',  ( 3.655360161107966022, -0.3364991752431121808, -1.700650080047048318 ) ) ;
#19306 = EDGE_CURVE ( 'NONE', #73220, #64997, #37227, .T. ) ;
#19307 = CARTESIAN_POINT ( 'NONE',  ( 0.8904706703079521279, -0.5376514911656914419, -2.124458794526106864 ) ) ;
#19308 = CARTESIAN_POINT ( 'NONE',  ( 2.134188411380482098, -1.507708438093162018, -1.747028958505469909 ) ) ;
#19309 = CARTESIAN_POINT ( 'NONE',  ( 5.149710871190182893, 0.6505453885284390170, -1.955453191944044766 ) ) ;
#19310 = CARTESIAN_POINT ( 'NONE',  ( 6.392136499528294102, -0.5222240449473265489, -1.870457282704639290 ) ) ;
#19311 = CARTESIAN_POINT ( 'NONE',  ( -7.253248993186740989, 9.485209796849769504, 1.443375672974090751 ) ) ;
#19312 = VECTOR ( 'NONE', #139927, 1000.000000000000114 ) ;
#19314 = EDGE_CURVE ( 'NONE', #138623, #175932, #78589, .T. ) ;
#19313 = CARTESIAN_POINT ( 'NONE',  ( -4.281342646865346602, 8.216926531310035031, 0.7998128361456352531 ) ) ;
#19315 = CARTESIAN_POINT ( 'NONE',  ( -9.367496996949647325, 15.51845925588232333, 7.500000000809289524 ) ) ;
#19316 = FILL_AREA_STYLE_COLOUR ( '', #60442 ) ;
#19317 = CARTESIAN_POINT ( 'NONE',  ( 1.178361531996233280, 1.528742360773158282, 1.314995429398260196 ) ) ;
#19318 = CARTESIAN_POINT ( 'NONE',  ( -5.870317324592811303, 8.832158731124840401, -1.082531754730537976 ) ) ;
#19319 = CARTESIAN_POINT ( 'NONE',  ( 3.487540646120320442, 1.995909124301387116, -0.9416478298167814120 ) ) ;
#19320 = CARTESIAN_POINT ( 'NONE',  ( 3.285556943749998737, -1.742708332855374076, -1.896917185911906500 ) ) ;
#19321 = CARTESIAN_POINT ( 'NONE',  ( 1.287708147089029032, -1.175244795098003614, -1.442924398407473108 ) ) ;
#19322 = CARTESIAN_POINT ( 'NONE',  ( 0.000000000000000000, 1.500000000000001332, 0.000000000000000000 ) ) ;
#19323 = CARTESIAN_POINT ( 'NONE',  ( 2.713058575063114652, 3.002994061098673395, -2.500000000000000444 ) ) ;
#19325 = CARTESIAN_POINT ( 'NONE',  ( 6.925078400183590333, 2.958959781645562170, 2.496897724761244497 ) ) ;
#19324 = CARTESIAN_POINT ( 'NONE',  ( -5.696549332702473656, 7.414053552612095643, -1.332310987329322183 ) ) ;
#19326 = CARTESIAN_POINT ( 'NONE',  ( 4.540391295830774609, 8.311223921862364250, 0.5620231006616300817 ) ) ;
#19327 = VERTEX_POINT ( 'NONE', #4871 ) ;
#19328 = CARTESIAN_POINT ( 'NONE',  ( 2.975518139630950021, 1.957357868463033501, -0.6452315760040390202 ) ) ;
#19329 = CARTESIAN_POINT ( 'NONE',  ( -1.360316468749990459, 1.890625000341386475, -2.428612866367529932E-14 ) ) ;
#19330 = CARTESIAN_POINT ( 'NONE',  ( -5.799137018343247796, 7.788745826199009237, -1.599625672291256295 ) ) ;
#19331 = CARTESIAN_POINT ( 'NONE',  ( 2.666670786633594137, 0.6826474749901580985, 1.900933108274209360 ) ) ;
#19332 = CARTESIAN_POINT ( 'NONE',  ( -3.811250579217344558, 5.539821323877241355, 0.000000000000000000 ) ) ;
#19333 = CARTESIAN_POINT ( 'NONE',  ( 5.034155109375821446, 4.767602470560229122, -0.7998128361456221525 ) ) ;
#19334 = CARTESIAN_POINT ( 'NONE',  ( 2.377870294028866294, 1.267006343609432761, 1.625331576946090539 ) ) ;
#19336 = CARTESIAN_POINT ( 'NONE',  ( 1.364683531249996529, 12.96354166700806410, 0.7879004041258405033 ) ) ;
#19335 = FACE_OUTER_BOUND ( 'NONE', #210722, .T. ) ;
#19337 = CARTESIAN_POINT ( 'NONE',  ( 6.819914962873951936, 7.915321197229798322, -1.199719254218446718 ) ) ;
#19338 = CARTESIAN_POINT ( 'NONE',  ( -0.2408018239684642792, 7.629137130509051623, -2.700476273684692785 ) ) ;
#19339 = CARTESIAN_POINT ( 'NONE',  ( 5.654950187766193181, -1.741821662664808867, 1.355018943897445149 ) ) ;
#19340 = CARTESIAN_POINT ( 'NONE',  ( 5.091969210384201361, 8.098325291160362482, 1.199719254218452047 ) ) ;
#19341 = CARTESIAN_POINT ( 'NONE',  ( 1.071799524545346216, 2.083542002058445863, -0.5754571431841256635 ) ) ;
#19342 = CARTESIAN_POINT ( 'NONE',  ( -4.989037340148921196, 5.883260320670900434, 1.082531754730560403 ) ) ;
#19343 = CARTESIAN_POINT ( 'NONE',  ( 1.464077725791514517, -1.074659653367866952, 1.706114136832518779 ) ) ;
#19344 = CARTESIAN_POINT ( 'NONE',  ( 2.284880952019330280, -2.229702823797473865, 0.5573334316414603196 ) ) ;
#19345 = DIRECTION ( 'NONE',  ( 3.330669073875478989E-16, -3.540251991789410786E-16, -1.000000000000000000 ) ) ;
#19346 = CARTESIAN_POINT ( 'NONE',  ( -0.4925365349140243265, 6.683082350101194002, 3.393863156617258792 ) ) ;
#19347 = DIRECTION ( 'NONE',  ( 0.7806247497998004548, 0.000000000000000000, 0.6249999999999992228 ) ) ;
#19348 = CARTESIAN_POINT ( 'NONE',  ( 2.061206331123175861, 0.3224310286589862629, -1.842498087946140561 ) ) ;
#19349 = CARTESIAN_POINT ( 'NONE',  ( 3.274625289317079524, -0.3981104328964027994, -1.976669913042613747 ) ) ;
#19351 = CARTESIAN_POINT ( 'NONE',  ( 11.44779963594988814, 13.39999999999998614, 3.600000000000001421 ) ) ;
#19350 = CARTESIAN_POINT ( 'NONE',  ( -1.364683531250014514, 1.488541667008084435, -0.7879004041258289570 ) ) ;
#19353 = CARTESIAN_POINT ( 'NONE',  ( 4.758481774355417748, 0.8053329972168337125, 1.946216683261194236 ) ) ;
#19352 = CARTESIAN_POINT ( 'NONE',  ( -8.715193815486133033, 9.062147627688959872, 0.7998128361456462443 ) ) ;
#19354 = CARTESIAN_POINT ( 'NONE',  ( 7.969495366734495434, 8.192166104145387706, 1.040834085586084257E-14 ) ) ;
#19355 = CARTESIAN_POINT ( 'NONE',  ( -7.714753101375940503, 8.959299025482085455, 1.199719254218462483 ) ) ;
#19356 = CARTESIAN_POINT ( 'NONE',  ( -0.09872732973945111401, -6.896119493545342038, -9.497255425109710103 ) ) ;
#19357 = CARTESIAN_POINT ( 'NONE',  ( 5.607677614632407881, 1.532089292189286356, 1.316289066716142431 ) ) ;
#19358 = CARTESIAN_POINT ( 'NONE',  ( -1.500000000000015099, -0.3395833326505143801, -0.8660254037844383745 ) ) ;
#19359 = CARTESIAN_POINT ( 'NONE',  ( 0.4267248635717044158, -1.349908593859616257, 1.559510075185864153 ) ) ;
#19360 = CARTESIAN_POINT ( 'NONE',  ( 8.026063749610047537, 10.38682701267698150, -1.443375672974057666 ) ) ;
#19361 = CARTESIAN_POINT ( 'NONE',  ( 6.367489420273535039, 7.457767740854454708, -1.199719254218452047 ) ) ;
#19362 = CARTESIAN_POINT ( 'NONE',  ( 6.737475991348287785, 6.825086509519945999, -0.7998128361456481317 ) ) ;
#19363 = CARTESIAN_POINT ( 'NONE',  ( 1.364683531249988757, 0.4468750003414206917, 0.000000000000000000 ) ) ;
#19365 = CARTESIAN_POINT ( 'NONE',  ( 9.534402287735492365, 3.538071065864172304, -7.287264613139948111 ) ) ;
#19364 = CARTESIAN_POINT ( 'NONE',  ( 5.391302360089590628, 6.318882837306503575, -1.199719254218452047 ) ) ;
#19366 = CARTESIAN_POINT ( 'NONE',  ( 7.659993601596707613, 9.959745173328078849, -1.443375672974058777 ) ) ;
#19368 = DIRECTION ( 'NONE',  ( 0.000000000000000000, 1.000000000000000000, 0.000000000000000000 ) ) ;
#19367 = CARTESIAN_POINT ( 'NONE',  ( 3.262351433937484835, -2.168797558456833308, 0.1038475075719157148 ) ) ;
#19370 = CARTESIAN_POINT ( 'NONE',  ( 2.155570461979210428, 0.7887370375637430264, 1.663910549085621415 ) ) ;
#19369 = CARTESIAN_POINT ( 'NONE',  ( -4.609409038966245653, 6.400729850259146758, -1.443375672974053447 ) ) ;
#19371 = CARTESIAN_POINT ( 'NONE',  ( 0.6823417656249899377, 3.092708333674754062, 1.181850606188765695 ) ) ;
#19372 = CARTESIAN_POINT ( 'NONE',  ( 3.861010967126535576, 0.2669419790740577558, -2.175157288012785184 ) ) ;
#19373 = LINE ( 'NONE', #153669, #53298 ) ;
#19374 = CARTESIAN_POINT ( 'NONE',  ( 4.891644337148946420, 1.673267685831375307, 1.523052275532793320 ) ) ;
#19375 = CARTESIAN_POINT ( 'NONE',  ( -5.343885102080728977, 9.386283052402845328, 0.7998128361456481317 ) ) ;
#19376 = CARTESIAN_POINT ( 'NONE',  ( -0.6823417656250212460, 5.613541667008087543, 1.181850606188767472 ) ) ;
#19377 = CARTESIAN_POINT ( 'NONE',  ( 5.170590401584001405, 7.751911629329717002, -1.182414590771277085 ) ) ;
#19378 = CARTESIAN_POINT ( 'NONE',  ( 1.499999999999997113, 13.89583333333333037, -0.8660254037844378194 ) ) ;
#19379 = CARTESIAN_POINT ( 'NONE',  ( -7.092323753280154186, 7.447001598347859463, 0.7216878364870317197 ) ) ;
#19380 = CARTESIAN_POINT ( 'NONE',  ( 3.770576118376296471, 7.413106214832098750, 0.7216878364870257245 ) ) ;
#19381 = CARTESIAN_POINT ( 'NONE',  ( 4.956192180792302615, 0.6771475221719803761, 1.635265836519818716 ) ) ;
#19382 = CARTESIAN_POINT ( 'NONE',  ( 3.246742594617262334, 1.964541544574874621, 0.4388061624774098890 ) ) ;
#19383 = CARTESIAN_POINT ( 'NONE',  ( 7.793239369756836510, 7.986534107671458216, 0.7998128361456341429 ) ) ;
#19384 = CARTESIAN_POINT ( 'NONE',  ( 1.483573828499670899, 1.945989852495342065, -0.8055925053903155719 ) ) ;
#19386 = CARTESIAN_POINT ( 'NONE',  ( -1.499999999999997780, 2.150000000000019895, 1.214306433183764966E-14 ) ) ;
#19385 = CARTESIAN_POINT ( 'NONE',  ( 1.364683531250000303, 12.50520833367473195, -0.7879004041258355073 ) ) ;
#19387 = CARTESIAN_POINT ( 'NONE',  ( 1.662492070209736994, -0.7059575147525645189, -1.838877744480153620 ) ) ;
#19388 = CARTESIAN_POINT ( 'NONE',  ( 0.6724591444495706671, -1.759989063064151038, -0.6342292696241008665 ) ) ;
#19389 = CARTESIAN_POINT ( 'NONE',  ( 0.4671467121175364445, 1.705069321186868159, 0.9702857188121425391 ) ) ;
#19391 = VERTEX_POINT ( 'NONE', #119796 ) ;
#19390 = CARTESIAN_POINT ( 'NONE',  ( -0.2049973002360427898, -0.1418364932926942379, -1.881151990943498387 ) ) ;
#19392 = CARTESIAN_POINT ( 'NONE',  ( 5.829642864196157070, 8.784705193995428374, 1.082531754730558626 ) ) ;
#19393 = CARTESIAN_POINT ( 'NONE',  ( 0.6823417656249882723, 0.2385416670080825474, -1.181850606188749264 ) ) ;
#19395 = CARTESIAN_POINT ( 'NONE',  ( 5.770339134078734666, -1.185559297855027561, 1.446973003893243348 ) ) ;
#19394 = VECTOR ( 'NONE', #184475, 1000.000000000000000 ) ;
#19396 = CARTESIAN_POINT ( 'NONE',  ( 2.218730694130720771, 5.740269576461138890, 0.7998128361456462443 ) ) ;
#19397 = CARTESIAN_POINT ( 'NONE',  ( 9.132253115921068698, 1.016282880930313937, 8.222717639126729594 ) ) ;
#19398 = CARTESIAN_POINT ( 'NONE',  ( 5.120015143727554729, 2.048507142264085701, -0.2983452141967629645 ) ) ;
#19399 = CARTESIAN_POINT ( 'NONE',  ( -1.752700365193352367E-14, 2.687499999999996447, -1.414508159514589636 ) ) ;
#19400 = GEOMETRIC_CURVE_SET ( 'NONE', ( #57871, #104305, #96668, #44855, #140389, #26801, #83573, #153404, #16425, #65515, #192124, #34459 ) ) ;
#19401 = CARTESIAN_POINT ( 'NONE',  ( -5.614485009390564940, 5.722856397143323726, 0.000000000000000000 ) ) ;
#19402 = CARTESIAN_POINT ( 'NONE',  ( 2.423460580168060652, 1.405705671057797312, -11.75284646727698679 ) ) ;
#19404 = CARTESIAN_POINT ( 'NONE',  ( -1.402160292154681736E-14, 0.2125000000000202283, 1.732050807568877637 ) ) ;
#19403 = COLOUR_RGB ( '', 0.08235294, 0.09019608, 0.10196078) ;
#19405 = CARTESIAN_POINT ( 'NONE',  ( 8.925345196497941558, 9.307324238869423283, 1.040834085586084257E-14 ) ) ;
#19406 = CARTESIAN_POINT ( 'NONE',  ( -9.854078719034067291, 10.39084668182823634, 0.7998128361456462443 ) ) ;
#19407 = CARTESIAN_POINT ( 'NONE',  ( 6.180537922983273091, 8.303989891604203422, -1.599625672291281386 ) ) ;
#19408 = CARTESIAN_POINT ( 'NONE',  ( 1.364683531249988757, 1.884375000341421913, 0.000000000000000000 ) ) ;
#19409 = ORIENTED_EDGE ( 'NONE', *, *, #153621, .T. ) ;
#19410 = CARTESIAN_POINT ( 'NONE',  ( -0.7500000000000006661, 1.608333333333357373, -1.299038105676652011 ) ) ;
#19412 = CARTESIAN_POINT ( 'NONE',  ( 3.714044015139744914, 6.420469553383295391, 1.199719254218462483 ) ) ;
#19411 = CARTESIAN_POINT ( 'NONE',  ( 5.459412808053472510, 1.602871733476991079, 1.130958114227413436 ) ) ;
#19413 = CARTESIAN_POINT ( 'NONE',  ( 3.321638586175166719, -1.528507173905558014, 1.314795459203411676 ) ) ;
#19414 = CARTESIAN_POINT ( 'NONE',  ( 2.887788952342277948, -1.913322710806207194, 0.09880452340514658816 ) ) ;
#19415 = CARTESIAN_POINT ( 'NONE',  ( -1.908029163539614492, 3.237038651130966116, -0.4603255239806567367 ) ) ;
#19416 = CARTESIAN_POINT ( 'NONE',  ( 0.6443834720083198020, 0.6415979653194536780, 2.095529601600601755 ) ) ;
#19417 = CARTESIAN_POINT ( 'NONE',  ( 0.1333692844072559003, 5.722267537706915874, -2.647605121726896105 ) ) ;
#19418 = CARTESIAN_POINT ( 'NONE',  ( 3.796049943699483453, -1.868292110373217518, -0.09463876624429126694 ) ) ;
#19419 = CARTESIAN_POINT ( 'NONE',  ( 0.7499999999999885647, 0.01458333401615358182, 1.299038105676657340 ) ) ;
#19420 = CARTESIAN_POINT ( 'NONE',  ( -7.670162217029145246, 9.971608557999250166, 1.599625672291295375 ) ) ;
#19422 = CARTESIAN_POINT ( 'NONE',  ( 4.218443861432810138, 2.076744001477859314, 0.4112613105302816430 ) ) ;
#19421 = CARTESIAN_POINT ( 'NONE',  ( -5.260200412422213923, 6.199617238323108737, -1.082531754730544860 ) ) ;
#19423 = CARTESIAN_POINT ( 'NONE',  ( 6.549288556030710140, 1.803345607721940524, -1.016871928424132099 ) ) ;
#19425 = CARTESIAN_POINT ( 'NONE',  ( 6.720655732516642722, 6.033109933379183332, 2.868628414513713309 ) ) ;
#19424 = CARTESIAN_POINT ( 'NONE',  ( 1.400065306692158229, -0.7557916345088554477, -1.949536834912476646 ) ) ;
#19427 = ORIENTED_EDGE ( 'NONE', *, *, #83347, .T. ) ;
#19426 = CARTESIAN_POINT ( 'NONE',  ( 6.827182134110196365, 0.003888933837258023128, 1.810856214465895508 ) ) ;
#19428 = CARTESIAN_POINT ( 'NONE',  ( 7.884230021546724920, 9.157022099014721306, 1.199719254218462483 ) ) ;
#19429 = DIRECTION ( 'NONE',  ( 0.000000000000000000, 1.000000000000000000, 0.000000000000000000 ) ) ;
#19430 = CARTESIAN_POINT ( 'NONE',  ( -10.48284956170200921, 5.077895721165493370, 7.121295720048954614 ) ) ;
#19431 = CARTESIAN_POINT ( 'NONE',  ( 5.287316719205157334, 9.112360572473935605, 1.040834085586084257E-14 ) ) ;
#19432 = CARTESIAN_POINT ( 'NONE',  ( 1.364683531250000748, 13.31770833367473195, -0.7879004041258355073 ) ) ;
#19434 = CARTESIAN_POINT ( 'NONE',  ( 0.09988412287174981696, -0.8557525428138833545, 1.596560661436140283 ) ) ;
#19433 = CARTESIAN_POINT ( 'NONE',  ( 6.638652492546827766, 7.774124658506663010, 1.199719254218452047 ) ) ;
#19435 = CARTESIAN_POINT ( 'NONE',  ( -9.006694118179950692, 9.402231314165087284, 1.040834085586084257E-14 ) ) ;
#19436 = CARTESIAN_POINT ( 'NONE',  ( 3.493197133815315603, 7.227147089426516402, -0.7998128361456291469 ) ) ;
#19437 = CARTESIAN_POINT ( 'NONE',  ( 7.523848900940885542, 7.742521570711348389, 0.7998128361456291469 ) ) ;
#19438 = CARTESIAN_POINT ( 'NONE',  ( 0.03415196713897553082, -6.453216945989479036, 10.89423718502873939 ) ) ;
#19439 = CARTESIAN_POINT ( 'NONE',  ( 4.003835517601626925, 7.590433450137844318, -0.2001945245787856709 ) ) ;
#19440 = CARTESIAN_POINT ( 'NONE',  ( 2.849184837166184536, 6.475799410002530898, 0.7998128361456362523 ) ) ;
#19441 = ORIENTED_EDGE ( 'NONE', *, *, #159575, .T. ) ;
#19442 = EDGE_CURVE ( 'NONE', #7171, #193389, #38817, .T. ) ;
#19443 = STYLED_ITEM ( 'NONE', ( #187405 ), #146775 ) ;
#19444 = EDGE_CURVE ( 'NONE', #25653, #136464, #85545, .T. ) ;
#19445 = CARTESIAN_POINT ( 'NONE',  ( 6.609000000000036401, 0.002801690667396730238, 2.000160786441218086 ) ) ;
#19446 = CARTESIAN_POINT ( 'NONE',  ( 0.6102159345307588412, -0.7594153588383574238, 1.980023364433493915 ) ) ;
#19447 = CARTESIAN_POINT ( 'NONE',  ( 10.91804383151479740, -8.407420853759283830, -0.1905751639681655396 ) ) ;
#19448 = CARTESIAN_POINT ( 'NONE',  ( -0.1394461523060988861, 1.283499747810852520, -2.524650647122913316 ) ) ;
#19449 = CARTESIAN_POINT ( 'NONE',  ( 7.235142258280584215, -6.594478602024285152, 7.235142258280580663 ) ) ;
#19450 = CARTESIAN_POINT ( 'NONE',  ( -5.260200412422220140, 5.239248024021764039, -0.7216878364870207285 ) ) ;
#19451 = CARTESIAN_POINT ( 'NONE',  ( 8.053180056837369705, 11.37883191874353805, -1.082531754730543083 ) ) ;
#19452 = CARTESIAN_POINT ( 'NONE',  ( 3.168761922233914952, 1.429703897159577464, -1.354768240434875759 ) ) ;
#19453 = CARTESIAN_POINT ( 'NONE',  ( 0.9441710812277158693, -1.348169866081018853, -1.636719737310005973 ) ) ;
#19454 = CARTESIAN_POINT ( 'NONE',  ( -7.054319997812058318, 7.124461507069184130, 1.040834085586084257E-14 ) ) ;
#19455 = CARTESIAN_POINT ( 'NONE',  ( 0.000000000000000000, 2.880000000000021210, 1.214306433183764966E-14 ) ) ;
#19456 = CARTESIAN_POINT ( 'NONE',  ( 6.727182134110200273, 0.5640974741700152117, 2.241195997201197443 ) ) ;
#19457 = COLOUR_RGB ( '', 0.40784314, 0.44705882, 0.49803922) ;
#19458 = CARTESIAN_POINT ( 'NONE',  ( 6.298795234281088895, 1.819837665574381091, 1.220625243075368127 ) ) ;
#19459 = CARTESIAN_POINT ( 'NONE',  ( 4.322341018716207017, 3.567520274870273678, 2.444429072473035536 ) ) ;
#19460 = CARTESIAN_POINT ( 'NONE',  ( 3.821244781301834426, -0.1429285350797465659, 1.921155437072092242 ) ) ;
#19461 = CARTESIAN_POINT ( 'NONE',  ( -7.374745490829552885, 10.69128794168811680, -1.199719254218446718 ) ) ;
#19462 = CARTESIAN_POINT ( 'NONE',  ( -0.1294898018152200736, 7.629137130509059617, -2.526516153123930852 ) ) ;
#19463 = CARTESIAN_POINT ( 'NONE',  ( 1.401302286655212948, 1.802556353783949517, -1.272968949304439379 ) ) ;
#19464 = CARTESIAN_POINT ( 'NONE',  ( 5.493163732433528068, 6.391633739925519642, -1.208849031437130961 ) ) ;
#19465 = ORIENTED_EDGE ( 'NONE', *, *, #56238, .T. ) ;
#19466 = CARTESIAN_POINT ( 'NONE',  ( 4.800995793014950941, 5.734154859006458160, -1.082531754730548412 ) ) ;
#19467 = CARTESIAN_POINT ( 'NONE',  ( 6.051603174176475086, 1.488812912110796249, 1.289293616420229549 ) ) ;
#19468 = CARTESIAN_POINT ( 'NONE',  ( 0.4857531807862237594, -1.927505705540471403, -0.2366729787525098105 ) ) ;
#19469 = CARTESIAN_POINT ( 'NONE',  ( 6.046309306592402955, 2.127046199546629435, -0.8712367593181246095 ) ) ;
#19471 = CARTESIAN_POINT ( 'NONE',  ( 4.750749981963457991, -0.4049220142380467458, -1.816192249911535272 ) ) ;
#19470 = CARTESIAN_POINT ( 'NONE',  ( -7.279802135894939852, 7.457800344824362604, -0.7998128361456362523 ) ) ;
#19472 = CARTESIAN_POINT ( 'NONE',  ( 7.198453214212898743, 7.362893269528701268, 0.7998128361456291469 ) ) ;
#19473 = CARTESIAN_POINT ( 'NONE',  ( -2.862179826260718762, 6.353310540697199471, 0.000000000000000000 ) ) ;
#19474 = DIRECTION ( 'NONE',  ( 0.000000000000000000, 1.000000000000000000, 0.000000000000000000 ) ) ;
#19476 = B_SPLINE_CURVE_WITH_KNOTS ( 'NONE', 3,
 ( #68737, #184629, #85009, #51457, #34125, #17852 ),
 .UNSPECIFIED., .F., .F.,
 ( 4, 2, 4 ),
 ( 0.002871295844531347036, 0.002933344926395646882, 0.002995394008259946294 ),
 .UNSPECIFIED. ) ;
#19475 = CARTESIAN_POINT ( 'NONE',  ( -6.856673000209188906, 9.022537805042615489, 1.599625672291283607 ) ) ;
#19477 = CARTESIAN_POINT ( 'NONE',  ( -3.354001786068215196, -0.9357451212759041459, 0.07218384636315192115 ) ) ;
#19478 = CARTESIAN_POINT ( 'NONE',  ( 0.7674258922165803076, 2.110627382301712540, -0.5898035449652739848 ) ) ;
#19479 = CARTESIAN_POINT ( 'NONE',  ( 4.446711195602238931, 6.210915699667823198, -1.443375672974051449 ) ) ;
#19480 = ORIENTED_EDGE ( 'NONE', *, *, #203350, .T. ) ;
#19481 = CARTESIAN_POINT ( 'NONE',  ( 0.5773502691896124084, -2.500000000000002220, -0.9999999999999991118 ) ) ;
#19482 = DIRECTION ( 'NONE',  ( 0.000000000000000000, 0.000000000000000000, -1.000000000000000000 ) ) ;
#19483 = CARTESIAN_POINT ( 'NONE',  ( 0.4690313652776016418, 0.1822212253758948297, -1.816563760317004395 ) ) ;
#19484 = CARTESIAN_POINT ( 'NONE',  ( -4.111146893441842920, 5.819424013814012753, 1.599625672291267398 ) ) ;
#19485 =( BOUNDED_SURFACE ( )  B_SPLINE_SURFACE ( 3, 2, ( 
 ( #163, #201571, #136615 ),
 ( #38039, #104108, #119348 ),
 ( #132378, #198379, #50020 ),
 ( #116144, #140907, #73729 ),
 ( #72653, #172307, #121502 ),
 ( #27102, #109505, #175512 ) ),
 .UNSPECIFIED., .F., .F., .T. ) 
 B_SPLINE_SURFACE_WITH_KNOTS ( ( 4, 2, 4 ),
 ( 3, 3 ),
 ( 0.000000000000000000, 0.0003766365702389427254, 0.0007532731404778854507 ),
 ( 0.000000000000000000, 1.000000000000000000 ),
 .UNSPECIFIED. ) 
 GEOMETRIC_REPRESENTATION_ITEM ( )  RATIONAL_B_SPLINE_SURFACE ( (
 ( 1.000000000000000000, 0.7452309222762957264, 1.000000000000000000),
 ( 1.000000000000000000, 0.7451892422669574856, 1.000000000000000000),
 ( 1.000000000000000000, 0.7429606254241496455, 1.000000000000000000),
 ( 1.000000000000000000, 0.7311462761262990107, 1.000000000000000000),
 ( 1.000000000000000000, 0.7212257702793347658, 1.000000000000000000),
 ( 1.000000000000000000, 0.7071067811865475727, 1.000000000000000000) ) ) 
 REPRESENTATION_ITEM ( '' )  SURFACE ( )  );
#19486 = CARTESIAN_POINT ( 'NONE',  ( 2.461176475124981611, -1.659910965455011267, -0.5019686038148748475 ) ) ;
#19487 = DIRECTION ( 'NONE',  ( -3.491481338843133750E-15, -0.000000000000000000, -1.000000000000000000 ) ) ;
#19488 = CARTESIAN_POINT ( 'NONE',  ( -11.07131242353766254, 9.799999999999998934, -0.8043462106219255725 ) ) ;
#19489 = CARTESIAN_POINT ( 'NONE',  ( -5.939880696118548187, 6.102484698325975288, 0.000000000000000000 ) ) ;
#19490 = CARTESIAN_POINT ( 'NONE',  ( 6.129513044595952032, -1.717388127611047421, 0.6198453807191862674 ) ) ;
#19491 = CARTESIAN_POINT ( 'NONE',  ( 3.203904402660478379, 0.7104733393662396868, -1.828749470067204896 ) ) ;
#19492 = CARTESIAN_POINT ( 'NONE',  ( -3.880700980283063650, 7.437752890734468991, 0.4300534088077876405 ) ) ;
#19493 = CARTESIAN_POINT ( 'NONE',  ( -10.16591625214838679, 10.75465713712827487, 1.040834085586084257E-14 ) ) ;
#19494 = CARTESIAN_POINT ( 'NONE',  ( 5.286789834324991055, 8.255339675766103724, -1.199719254218452935 ) ) ;
#19495 = CARTESIAN_POINT ( 'NONE',  ( 4.969442291489525765, -1.791676405564743169, -1.133875526122554156 ) ) ;
#19496 = CARTESIAN_POINT ( 'NONE',  ( 5.345657705538078730, 9.458627433094950021, 0.7998128361456331437 ) ) ;
#19497 = CARTESIAN_POINT ( 'NONE',  ( -8.448702279610222021, 13.00856975952063088, 1.040834085586084257E-14 ) ) ;
#19498 = CARTESIAN_POINT ( 'NONE',  ( 2.817306709214098870, -1.799057772339835548, -1.024303335033532658 ) ) ;
#19500 = CARTESIAN_POINT ( 'NONE',  ( 0.6823417656249882723, 0.4052083336747516751, 1.181850606188755259 ) ) ;
#19499 = DIRECTION ( 'NONE',  ( 0.000000000000000000, -1.000000000000000000, 0.000000000000000000 ) ) ;
#19502 = ORIENTED_EDGE ( 'NONE', *, *, #99329, .T. ) ;
#19501 = CARTESIAN_POINT ( 'NONE',  ( 5.022253332556455341, -2.210719170837057934, 0.2167383629448139670 ) ) ;
#19503 = CARTESIAN_POINT ( 'NONE',  ( 2.391599454647721945, -0.8833308501894185927, -2.122370812339502422 ) ) ;
#19504 = CARTESIAN_POINT ( 'NONE',  ( 8.758204044748005401, 10.28062147603659504, 1.082531754730549967 ) ) ;
#19506 = CARTESIAN_POINT ( 'NONE',  ( 1.001543065824772753E-15, -2.821874999522044458, 3.793834371823811669 ) ) ;
#19505 = CARTESIAN_POINT ( 'NONE',  ( 6.048345925472178308, 9.110135108809304327, 1.082531754730549967 ) ) ;
#19507 = CARTESIAN_POINT ( 'NONE',  ( 0.000000000000000000, -8.327195405469542067, 10.91970695577495931 ) ) ;
#19508 = DIRECTION ( 'NONE',  ( 0.000000000000000000, -1.000000000000000000, 0.000000000000000000 ) ) ;
#19509 = DIRECTION ( 'NONE',  ( 0.000000000000000000, 0.000000000000000000, -1.000000000000000000 ) ) ;
#19510 = EDGE_CURVE ( 'NONE', #137701, #137589, #67164, .T. ) ;
#19511 = CARTESIAN_POINT ( 'NONE',  ( 4.025576834063953946, -0.3218090080209669024, 1.884953445776993863 ) ) ;
#19512 = CARTESIAN_POINT ( 'NONE',  ( -0.08896015503664653212, 7.049507384514471120, -3.948637857580538313 ) ) ;
#19513 = CARTESIAN_POINT ( 'NONE',  ( 3.662884335446520367, -1.521034750653621481, -0.8131990640867832187 ) ) ;
#19514 = CARTESIAN_POINT ( 'NONE',  ( 3.221888912838869690, 0.9023448338944944913, -1.803416113280359445 ) ) ;
#19515 = CARTESIAN_POINT ( 'NONE',  ( 3.639517500262396954, 0.8282738168534724554, 2.144427848026169592 ) ) ;
#19516 = CARTESIAN_POINT ( 'NONE',  ( -11.35569630219380777, 12.48731560708633914, -3.554478010595065296 ) ) ;
#19517 = CARTESIAN_POINT ( 'NONE',  ( 0.04788047853313340263, -1.708876078042343316, -1.396090968258607790 ) ) ;
#19518 = CARTESIAN_POINT ( 'NONE',  ( -6.807602527837528505, 7.114826835331461652, 0.7216878364870317197 ) ) ;
#19519 = VERTEX_POINT ( 'NONE', #120880 ) ;
#19520 = CARTESIAN_POINT ( 'NONE',  ( 4.516719421352251906, 1.617689212748760985, 0.7181139158070405371 ) ) ;
#19521 = CIRCLE ( 'NONE', #47244, 2.000000000000000000 ) ;
#19523 = CARTESIAN_POINT ( 'NONE',  ( 0.7094041017953250927, -0.3309814517665210509, 2.268137058596159328 ) ) ;
#19522 = CARTESIAN_POINT ( 'NONE',  ( 5.352436782344940802, 9.466536356036257871, 0.000000000000000000 ) ) ;
#19524 = CARTESIAN_POINT ( 'NONE',  ( 6.474545096729185545, -0.09562278402284159207, -1.838781726270556804 ) ) ;
#19525 = CARTESIAN_POINT ( 'NONE',  ( 0.4153311931458965045, 3.919844006742699616, -0.4999999999999988343 ) ) ;
#19526 = CARTESIAN_POINT ( 'NONE',  ( 6.650331627364351128, -1.696677047125955795, 1.386650686450926484 ) ) ;
#19527 = CARTESIAN_POINT ( 'NONE',  ( -5.503684012504701961, 5.385662534202396934, 0.000000000000000000 ) ) ;
#19528 = CARTESIAN_POINT ( 'NONE',  ( 1.360316468749955598, -0.9739583329918906074, 0.7853790794158580502 ) ) ;
#19529 = CARTESIAN_POINT ( 'NONE',  ( 0.07933194154487524519, 7.849261790823902629, 9.499668754385634628 ) ) ;
#19530 = EDGE_CURVE ( 'NONE', #61984, #211122, #102873, .T. ) ;
#19531 = CARTESIAN_POINT ( 'NONE',  ( 0.2741912710782665741, -2.129148944087058126, 0.4243047986705119068 ) ) ;
#19532 = CARTESIAN_POINT ( 'NONE',  ( 1.182827746461931229, 1.645757370610765102, -1.164989914844760444 ) ) ;
#19533 = CARTESIAN_POINT ( 'NONE',  ( 1.499999999999987121, -0.4645833326505149907, 0.8660254037844524744 ) ) ;
#19534 = CARTESIAN_POINT ( 'NONE',  ( 4.916589582839517192, 1.327171671461774061, -1.396654247447129960 ) ) ;
#19535 = CARTESIAN_POINT ( 'NONE',  ( -0.6823417656250039265, 11.56770833367473017, -1.181850606188755259 ) ) ;
#19536 = CARTESIAN_POINT ( 'NONE',  ( 1.108037262132562262, 1.686735864949813202, 1.445688421275423075 ) ) ;
#19538 = EDGE_LOOP ( 'NONE', ( #202696, #107130, #73533, #161399 ) ) ;
#19537 = CARTESIAN_POINT ( 'NONE',  ( 8.191097360950562845, 12.70803068775103739, -0.7998128361456352531 ) ) ;
#19540 = CARTESIAN_POINT ( 'NONE',  ( 0.000000000000000000, -9.006862915010128035, 0.000000000000000000 ) ) ;
#19539 = CARTESIAN_POINT ( 'NONE',  ( 0.000000000000000000, 0.000000000000000000, -0.4856446947087145194 ) ) ;
#19541 = DIRECTION ( 'NONE',  ( -0.7366372490352351976, 0.000000000000000000, 0.6762880771785058087 ) ) ;
#19542 = CARTESIAN_POINT ( 'NONE',  ( 10.07778825365955733, 10.65184113889131012, -0.7998128361456281477 ) ) ;
#19543 = DIRECTION ( 'NONE',  ( 0.000000000000000000, 0.000000000000000000, -1.000000000000000000 ) ) ;
#19544 = CARTESIAN_POINT ( 'NONE',  ( 3.821228196946160338, 7.349073440743831398, -0.5400038253845617087 ) ) ;
#19545 = CARTESIAN_POINT ( 'NONE',  ( 4.194663043249587275, 1.400965740628885126, 1.032472458625796286 ) ) ;
#19546 = CARTESIAN_POINT ( 'NONE',  ( 2.049198471137442912, 1.708465938063120637, -0.9642302061752604514 ) ) ;
#19548 = CARTESIAN_POINT ( 'NONE',  ( -1.201851678989727383E-14, 2.134375000341423689, 1.575800808251672791 ) ) ;
#19547 = CARTESIAN_POINT ( 'NONE',  ( 2.849184837166184536, 6.475799410002530898, 0.7998128361456362523 ) ) ;
#19549 = CARTESIAN_POINT ( 'NONE',  ( -5.881612045648562770, 6.018300081020916181, 0.2952277700727298781 ) ) ;
#19550 = CARTESIAN_POINT ( 'NONE',  ( -3.475000000000000533, -2.056249999044083232, 0.000000000000000000 ) ) ;
#19551 = AXIS2_PLACEMENT_3D ( 'NONE', #163546, #193898, #79081 ) ;
#19552 = CARTESIAN_POINT ( 'NONE',  ( 6.285602425426498385, -1.847771260692541162, 0.6596951833430019230 ) ) ;
#19553 = CARTESIAN_POINT ( 'NONE',  ( -6.821723845970312894, 11.11042825360738284, 0.000000000000000000 ) ) ;
#19554 = CARTESIAN_POINT ( 'NONE',  ( -3.755245360860925086, 6.364574773437617239, -1.082531754730548412 ) ) ;
#19555 = CARTESIAN_POINT ( 'NONE',  ( 5.208220363674559650, 1.197307938467083055, -1.622483861274232719 ) ) ;
#19556 = AXIS2_PLACEMENT_3D ( 'NONE', #8574, #207834, #26951 ) ;
#19557 = CARTESIAN_POINT ( 'NONE',  ( 1.323510708689378479, -0.05371019744930016770, 2.262043349595239228 ) ) ;
#19558 = ORIENTED_EDGE ( 'NONE', *, *, #130557, .T. ) ;
#19559 = CARTESIAN_POINT ( 'NONE',  ( -1.500000000000015099, -0.5895833326505155458, -0.8660254037844383745 ) ) ;
#19560 = CARTESIAN_POINT ( 'NONE',  ( 2.336979506217982117, -1.672866993182718698, 0.8370366242000035761 ) ) ;
#19561 = CARTESIAN_POINT ( 'NONE',  ( 1.107607643408299314, -0.04344470770747606292, 1.733769432050970449 ) ) ;
#19562 = B_SPLINE_CURVE_WITH_KNOTS ( 'NONE', 3,
 ( #22360, #171843, #102571, #86319, #39708, #184867, #136153, #200050, #170772, #202170, #87395, #117823, #168631, #54892, #138290, #71110, #3969, #118881, #204305, #150270, #103650, #119958, #183813, #121046, #203248, #185933, #5035, #35423, #154532, #169701, #38644, #153462, #167571, #19171, #201107, #137228, #187013, #45070, #156673, #89547, #8266, #74350, #140454, #190211, #206465, #205392, #90616, #91691, #177183, #58092, #111181, #109046, #41871, #191271, #176126, #77537, #155598, #125312, #124252, #209653, #7183, #107981, #106902, #60220, #174009, #26652, #159861, #25580, #157744, #76469, #40797, #142578, #24505, #172928, #9341, #75414, #141527, #192338, #11464, #175065, #207535, #59154, #42937, #110115, #143659, #189158, #92753, #93820, #61294, #158797, #73254, #27726, #10394, #127455, #208585, #126379, #123197, #43997, #139361, #193426, #57030, #194490, #33059, #12530, #82864, #147890, #32002, #144722, #30947, #66580, #47205, #165186, #81807, #16780, #15722, #148940, #50373, #14657, #163076, #78602, #132722, #49321, #113320, #179327, #146839, #210734, #115438, #116496, #129582, #97022, #513, #63430, #80751, #62360, #197677, #212858, #114383, #94883, #64495, #213906, #198727, #130637, #65529, #196629, #131675, #128521, #28799, #195569, #160935, #181429, #99137, #48270, #98083, #46132, #112249, #180378, #178260, #164138, #29873, #95957, #162011, #13600, #79674, #145789, #211792, #18911, #122674, #167325, #84995, #68723, #151086, #83924, #183559, #184615, #58643, #2650, #207012, #204858, #134845, #72744, #57580, #200848, #152142, #150014, #157222, #35166, #56514, #52498, #199800, #156156, #101242, #188637, #41352, #118630, #36233, #172402, #133792, #23990, #117564, #51445, #102311, #168385, #141005, #19981, #86065, #6668, #138842, #40267, #91166, #106378, #90092, #73823, #182485, #7737, #189699, #139918, #8821, #205948, #123738, #107461, #173487, #25064, #1584, #74896, #100185, #34113, #166250, #17840, #67645, #191820, #28275, #144210, #79150, #162555, #193963, #78086, #43485, #142061, #208075, #174554, #93303, #160409, #109603, #30420, #190757, #62897, #46673, #14126, #195039, #27197, #192888, #44546, #209133, #129067, #80219, #210206, #110661, #61842, #12012, #60771, #175609, #13071, #112793, #128010, #126931, #45611, #75958, #176662, #145266, #178805, #9883, #111726, #96505, #146318, #159339, #124796, #212333, #94367, #42420, #177734, #29347, #95442, #108525, #161492, #211274, #26130, #59701, #92243, #158292, #125863, #10935, #77011, #143138, #66064, #83404, #312, #181966, #15200, #149486, #134334, #67134, #198215, #47752, #167865, #19463, #49850, #82340, #35720, #117045, #165736, #18398, #132207, #115978, #113867, #184100, #213394, #166806, #179862, #148432, #85538, #63971, #33595, #183041, #51990, #199276, #99667, #180913, #200339, #101796, #17323, #1069, #48797, #133267, #50918, #151629, #196115, #34657, #81291, #118115, #163620, #130127, #84475, #150566, #2127, #131171, #31486, #97561, #197161, #147368, #114915, #65018, #32537, #98611, #164672, #16255, #68203, #100727, #187302, #154816, #203527, #137510, #189439, #5317, #23729, #87677, #21570, #121326, #185157, #89835, #24793, #103941, #153749, #41081, #37861, #55181, #53037, #172134, #38928, #88759, #69265, #71399, #205675, #138573, #105011, #120252, #139655, #107189 ),
 .UNSPECIFIED., .F., .F.,
 ( 4, 1, 1, 1, 1, 1, 1, 1, 1, 1, 1, 1, 1, 1, 1, 1, 1, 1, 1, 1, 1, 1, 1, 1, 1, 1, 1, 1, 1, 1, 1, 1, 1, 1, 1, 1, 1, 1, 1, 1, 1, 1, 1, 1, 1, 1, 1, 1, 1, 1, 1, 1, 1, 1, 1, 1, 1, 1, 1, 1, 1, 1, 1, 1, 1, 1, 1, 1, 1, 1, 1, 1, 1, 1, 1, 1, 1, 1, 1, 1, 1, 1, 1, 1, 1, 1, 1, 1, 1, 1, 1, 1, 1, 1, 1, 1, 1, 1, 1, 1, 1, 1, 1, 1, 1, 1, 1, 1, 1, 1, 1, 1, 1, 1, 1, 1, 1, 1, 1, 1, 1, 1, 1, 1, 1, 1, 1, 1, 1, 1, 1, 1, 1, 1, 1, 1, 1, 1, 1, 1, 1, 1, 1, 1, 1, 1, 1, 1, 1, 1, 1, 1, 1, 1, 1, 1, 1, 1, 1, 1, 1, 1, 1, 1, 1, 1, 1, 1, 1, 1, 1, 1, 1, 1, 1, 1, 1, 1, 1, 1, 1, 1, 1, 1, 1, 1, 1, 1, 1, 1, 1, 1, 1, 1, 1, 1, 1, 1, 1, 1, 1, 1, 1, 1, 1, 1, 1, 1, 1, 1, 1, 1, 1, 1, 1, 1, 1, 1, 1, 1, 1, 1, 1, 1, 1, 1, 1, 1, 1, 1, 1, 1, 1, 1, 1, 1, 1, 1, 1, 1, 1, 1, 1, 1, 1, 1, 1, 1, 1, 1, 1, 1, 1, 1, 1, 1, 1, 1, 1, 1, 1, 1, 1, 1, 1, 1, 1, 1, 1, 1, 1, 1, 1, 1, 1, 1, 1, 1, 1, 1, 1, 1, 1, 1, 1, 1, 1, 1, 1, 1, 1, 1, 1, 1, 1, 1, 1, 1, 1, 1, 1, 1, 1, 1, 1, 1, 1, 1, 1, 1, 1, 1, 1, 1, 1, 1, 1, 1, 1, 1, 1, 1, 1, 1, 1, 1, 1, 1, 1, 1, 1, 1, 1, 1, 1, 1, 1, 1, 1, 1, 1, 1, 1, 1, 1, 1, 1, 1, 1, 1, 1, 1, 1, 1, 1, 1, 1, 1, 1, 1, 1, 1, 1, 1, 1, 1, 1, 1, 1, 1, 1, 1, 1, 1, 1, 1, 1, 1, 1, 1, 1, 1, 1, 1, 4 ),
 ( 0.000000000000000000, 0.002599878613971510263, 0.005208762566300055921, 0.007813076245110234588, 0.01041697056762492211, 0.01302017924898362516, 0.01562522799165661294, 0.01822895742955179393, 0.02083332403451576206, 0.02343772221867868391, 0.02604143078293654281, 0.02864626161639613477, 0.03124961764961396021, 0.03385452714844047750, 0.03645799780571232912, 0.03906266225314121432, 0.04166671052383312535, 0.04427076094224517699, 0.04687542278318937439, 0.04947889361195772356, 0.05208380280015859759, 0.05468715921365963767, 0.05729198803509916865, 0.05989568673917144287, 0.06250009379223495087, 0.06510449848632135494, 0.06770819839843210397, 0.07031302545632363288, 0.07291638160390327694, 0.07552129054917994244, 0.07812475961953217751, 0.08072942239586503033, 0.08333346963797970408, 0.08593751866472883194, 0.08854217935802578821, 0.09114564884740632145, 0.09375055680876714925, 0.09635391199924973893, 0.09895873945611717570, 0.1015624370353711836, 0.1041668426700886191, 0.1067712463110160465, 0.1093749448896196713, 0.1119797708301935452, 0.1145831257515418783, 0.1171880334468678037, 0.1197915013940491491, 0.1223961628153678316, 0.1250002090321265524, 0.1276042567216372492, 0.1302089163955687523, 0.1328123846563000476, 0.1354172914881497103, 0.1380206455552074885, 0.1406254717515977581, 0.1432291683081768907, 0.1458335726268597532, 0.1484379753169847160, 0.1510416726638619811, 0.1536464975900906083, 0.1562498513865758776, 0.1588547579349887939, 0.1614582248604825021, 0.1640628850295551278, 0.1666669303230295940, 0.1692709767774011609, 0.1718756355346959253, 0.1744791026682601387, 0.1770840084736199360, 0.1796873615186004858, 0.1822921865574477218, 0.1848958821930496710, 0.1875002852981585977, 0.1901046871399069693, 0.1927083833567690418, 0.1953132073715553307, 0.1979165601445126987, 0.2005214656490191816, 0.2031249316542690642, 0.2057295906738217384, 0.2083336351460475244, 0.2109376804673406547, 0.2135423384106908962, 0.2161458045185324639, 0.2187507094003866837, 0.2213540615246011867, 0.2239588855088016361, 0.2265625803250888304, 0.2291669823190463362, 0.2317713834148095453, 0.2343750786033309830, 0.2369799018095430365, 0.2395832536602726381, 0.2421881582238437913, 0.2447916234102597566, 0.2473962813829825302, 0.2500003251359625422, 0.2526043694262022354, 0.2552090266582678346, 0.2578124918417971090, 0.2604173959030967600, 0.2630207472078238129, 0.2656255702402394725, 0.2682292643388430320, 0.2708336653240377978, 0.2734380657761767419, 0.2760417600379992398, 0.2786465825384744077, 0.2812499335682448476, 0.2838548372938197173, 0.2864583017627815864, 0.2890629587913320364, 0.2916670019270400371, 0.2942710452882197347, 0.2968757019116316509, 0.2994791662722288139, 0.3020840696158954564, 0.3046874202023847622, 0.3072922423858477359, 0.3098959358683710530, 0.3125003359471613118, 0.3151047358580104651, 0.3177084292947467969, 0.3203132511922952008, 0.3229166015023476888, 0.3255215044928377321, 0.3281249683456989308, 0.3307296245327063788, 0.3333336671530912065, 0.3359377096871765112, 0.3385423658045411677, 0.3411458294435600336, 0.3437507321724898035, 0.3463540821419661686, 0.3489589035792820537, 0.3515625965473047621, 0.3541669958220223235, 0.3567713952938928457, 0.3593750880071304721, 0.3619799094045394461, 0.3645832590960911834, 0.3671881614543835437, 0.3697916247924753486, 0.3723962802405443862, 0.3750003224475334518, 0.3776043642564660408, 0.3802090199703688222, 0.3828124829891406122, 0.3854173852062082184, 0.3880207346598750218, 0.3906255554538268782, 0.3932292480089087938, 0.3958336465818629857, 0.3984380457170473289, 0.4010417378083525053, 0.4036465588083897882, 0.4062499079826380477, 0.4088548098116001062, 0.4114582727362346981, 0.4140629275479489335, 0.4166669694434522730, 0.4192710106291533956, 0.4218756660421624782, 0.4244791285419997062, 0.4270840303500617607, 0.4296873793891050619, 0.4322921996424575197, 0.4348958918861421385, 0.4375002898596233591, 0.4401046887603987101, 0.4427083803313200949, 0.4453132010367379379, 0.4479165497948640051, 0.4505214511973463787, 0.4531249138098211726, 0.4557295680877478938, 0.4583336097736617210, 0.4609376504380365280, 0.4635423056527069874, 0.4661457677349071238, 0.4687506692368063055, 0.4713540179623986193, 0.4739588377779012651, 0.4765625298117197040, 0.4791669272880037522, 0.4817713260566358624, 0.4843750172087082362, 0.4869798377222476216, 0.4895831861654201811, 0.4921880872442612742, 0.4947915496458628049, 0.4973962034925555886, 0.5000002450707665691, 0.5026042853157074441, 0.5052089404345847523, 0.5078124022004342208, 0.5104173034990032720, 0.5130206520123070657, 0.5156254714926987726, 0.5182291634181735995, 0.5208335604995248946, 0.5234379592382720769, 0.5260416500730202838, 0.5286464704974140894, 0.5312498187267931105, 0.5338547195848227789, 0.5364581818768299204, 0.5390628353948335727, 0.5416668769672219330, 0.5442709168946127107, 0.5468755720202369552, 0.5494790335710144635, 0.5520839347690799093, 0.5546872831712518215, 0.5572921024192640793, 0.5598957943379132551, 0.5625001911265891108, 0.5651045899377058479, 0.5677082805566486812, 0.5703131009946261765, 0.5729164491113668545, 0.5755213498514099024, 0.5781248121350983649, 0.5807294654269519185, 0.5833335070953961088, 0.5859375468071157389, 0.5885422020420250089, 0.5911456634790059894, 0.5937505646793920233, 0.5963539130715860281, 0.5989587321899475514, 0.6015624242032879820, 0.6041668208015419372, 0.6067712197872831004, 0.6093749102919370220, 0.6119797308462270324, 0.6145830789514836745, 0.6171879796763642956, 0.6197914420530098445, 0.6223960952212510556, 0.6250001370876311357, 0.6276041766855571247, 0.6302088321322918407, 0.6328122935567517260, 0.6354171948622837629, 0.6380205433456558328, 0.6406253624370956690, 0.6432290546466469250, 0.6458334511567334069, 0.6484378504193577530, 0.6510415409112403351, 0.6536463616845760161, 0.6562497098795055939, 0.6588546106920506462, 0.6614580732629331550, 0.6640627264101022220, 0.6666667685763031370, 0.6692708081623160998, 0.6718754639234225667, 0.6744789254366408970, 0.6770838269501499029, 0.6796871756258610064, 0.6822919947931124218, 0.6848956873004010681, 0.6875000838245786117, 0.6901044834663523364, 0.6927081740469867022, 0.6953129951421085364, 0.6979163435278744609, 0.7005212445309179081, 0.7031247073973251327, 0.7057293606259679164, 0.7083334031938842701, 0.7109374428698714832, 0.7135420990479055536, 0.7161455607511696408, 0.7187504625754957965, 0.7213538115447158949, 0.7239586308905210377, 0.7265623237970838533, 0.7291667204376187650, 0.7317711205608201652, 0.7343748113317387638, 0.7369796328513985584, 0.7395829815291747877, 0.7421878828255610294, 0.7447913460887924941, 0.7473959995014650692, 0.7500000425730045661, 0.7526040824408628538, 0.7552087391383944803, 0.7578122011330034047, 0.7604171033709996586, 0.7630204527349119248, 0.7656252723620247114, 0.7682289657694127971, 0.7708333626285834850, 0.7734377633355060677, 0.7760414543982535607, 0.7786462764452187768, 0.7812496255161931469, 0.7838545272087811266, 0.7864579909701516769, 0.7890626446694239959, 0.7916666883465109938, 0.7942707285081521684, 0.7968753858277685120, 0.7994788482150362308, 0.8020837509695725176, 0.8046871008293766669, 0.8072919208405671121, 0.8098956148503495545, 0.8125000120304503026, 0.8151044134234068927, 0.8177081048795449281, 0.8203129275566022338, 0.8229162771219805661, 0.8255211793136476572, 0.8281246436744912343, 0.8307292977629509023, 0.8333333421475307423, 0.8359373827048843797, 0.8385420407491936956, 0.8411455036304537058, 0.8437504070044209437, 0.8463537574613370085, 0.8489585779593948889, 0.8515622726731627568, 0.8541666702765071673, 0.8567710724578335713, 0.8593747644089445581, 0.8619795878189033811, 0.8645829379799131464, 0.8671878407735589267, 0.8697913058352330085, 0.8723959604154888359, 0.8750000056095312839, 0.8776040466645483873, 0.8802087055361843548, 0.8828121690127931354, 0.8854170731091063340, 0.8880204242643787715, 0.8906252453521178447, 0.8932289408714879642, 0.8958333390004131758, 0.8984377420724726226, 0.9010414346201626179, 0.9036462588658594752, 0.9062496097237539017, 0.9088545132223035949, 0.9114579790861923048, 0.9140626342608790811, 0.9166666803663815477, 0.9192707220210388774, 0.9218753818226663732, 0.9244788459960084914, 0.9270837509176034219, 0.9296871028724987829, 0.9322919246527909820, 0.9348956210794385768, 0.9375000198362011261, 0.9401044239011964176, 0.9427081171475072408, 0.9453129423329229564, 0.9479162939871883520, 0.9505211982878988275, 0.9531246650646376661, 0.9557293209618126228, 0.9583333680330715643, 0.9609374102905526849, 0.9635420713365114853, 0.9661455366701111602, 0.9687504417289087844, 0.9713537931426093897, 0.9739586182492501187, 0.9765623229037746489, 0.9791667147516245340, 0.9817710778420317697, 0.9843748014325267581, 0.9869798465897002826, 0.9895830499482988207, 0.9921869381715581193, 0.9947912477285243416, 0.9974001254724073062, 1.000000000000000000 ),
 .UNSPECIFIED. ) ;
#19563 = EDGE_CURVE ( 'NONE', #185203, #105543, #113688, .T. ) ;
#19564 = CARTESIAN_POINT ( 'NONE',  ( 4.845371438081495619, 0.6875289519675978900, -2.081009137124201658 ) ) ;
#19565 = CARTESIAN_POINT ( 'NONE',  ( 5.983493387795983054, 2.135156284703492169, -0.8757408730279289122 ) ) ;
#19566 = CARTESIAN_POINT ( 'NONE',  ( 1.340775744366573541, 0.4011420747369342510, 2.021288966927562214 ) ) ;
#19567 = CARTESIAN_POINT ( 'NONE',  ( 3.521366475706534160, -1.157360712602263808, -1.559242563676524584 ) ) ;
#19568 = CARTESIAN_POINT ( 'NONE',  ( -4.731432421044883263, 5.582721248382882528, -1.082531754730543971 ) ) ;
#19569 = CARTESIAN_POINT ( 'NONE',  ( 5.800035319642947051, -1.870726058474009079, -0.0005997126256013226653 ) ) ;
#19570 = ADVANCED_FACE ( 'NONE', ( #152235, #153295 ), #72018, .F. ) ;
#19571 = CARTESIAN_POINT ( 'NONE',  ( 4.012968703617612931, 7.577496623363801476, 0.2782505873175616373 ) ) ;
#19572 = CARTESIAN_POINT ( 'NONE',  ( 0.4383029422423733168, 0.9912079340955775031, 1.422354019259955304 ) ) ;
#19573 = CARTESIAN_POINT ( 'NONE',  ( 4.909461021924254709, 5.860697626067345567, 1.082531754730549078 ) ) ;
#19574 = CARTESIAN_POINT ( 'NONE',  ( 1.360316468749957597, 1.265625000341379147, -5.030698080332740574E-14 ) ) ;
#19575 = CARTESIAN_POINT ( 'NONE',  ( 4.623672751230786027, 0.3474658942751900903, 1.986100912583692812 ) ) ;
#19576 = CARTESIAN_POINT ( 'NONE',  ( -4.460269348771590536, 5.266364330730674226, 1.082531754730558626 ) ) ;
#19577 = CARTESIAN_POINT ( 'NONE',  ( 8.341290820905593151, 10.75459192918846618, 1.599625672291281386 ) ) ;
#19578 = CARTESIAN_POINT ( 'NONE',  ( 3.932747076415766596, 6.745899468197171345, 1.199719254218451159 ) ) ;
#19580 = CARTESIAN_POINT ( 'NONE',  ( 7.730132016635857362, -5.756136661604687177, -7.730132016635878678 ) ) ;
#19579 = CARTESIAN_POINT ( 'NONE',  ( 1.945663734523142230, 0.6997465788082489757, -1.686465609443507763 ) ) ;
#19581 = CARTESIAN_POINT ( 'NONE',  ( -5.960744811863571968, 6.983232364376142698, 1.199719254218452935 ) ) ;
#19582 = CARTESIAN_POINT ( 'NONE',  ( -5.978219388983010418, 5.939287140093763462, -0.7998128361456361413 ) ) ;
#19583 = CARTESIAN_POINT ( 'NONE',  ( -9.811677024507259759, 4.107325997343203028, 6.339424533126782002 ) ) ;
#19584 = ORIENTED_EDGE ( 'NONE', *, *, #68379, .T. ) ;
#19585 = CARTESIAN_POINT ( 'NONE',  ( -5.438229012412899799, 7.437962829272074750, -1.443375672974066548 ) ) ;
#19586 = CARTESIAN_POINT ( 'NONE',  ( -4.060830702492950195, 4.696389560118578999, -1.199719254218452047 ) ) ;
#19587 = CARTESIAN_POINT ( 'NONE',  ( -8.611400122974211868, 13.19838391011195888, 1.040834085586084257E-14 ) ) ;
#19588 = CARTESIAN_POINT ( 'NONE',  ( 6.217445935018812264, 1.680332259792745475, 1.120195391490413472 ) ) ;
#19590 = ORIENTED_EDGE ( 'NONE', *, *, #143420, .F. ) ;
#19589 = CARTESIAN_POINT ( 'NONE',  ( 6.410783699188008278, -0.5891560598917375824, -2.141663135048486044 ) ) ;
#19591 = CARTESIAN_POINT ( 'NONE',  ( -5.749539660647037032, 8.865490816466966351, 1.199719254218454489 ) ) ;
#19592 = CARTESIAN_POINT ( 'NONE',  ( 5.331380718671758778, 7.243030143248949670, -1.599625672291256295 ) ) ;
#19593 = CARTESIAN_POINT ( 'NONE',  ( 5.541890059496114240, 0.8373154222949423797, -1.883320703650725125 ) ) ;
#19594 = CARTESIAN_POINT ( 'NONE',  ( 5.168592345394213972, 1.356298078840772803, 1.492257005506091971 ) ) ;
#19595 = ORIENTED_EDGE ( 'NONE', *, *, #112110, .T. ) ;
#19596 = ORIENTED_EDGE ( 'NONE', *, *, #214161, .T. ) ;
#19597 = CARTESIAN_POINT ( 'NONE',  ( 10.07455280567994116, 1.264806443676223857, 6.263461699855335851 ) ) ;
#19598 = CARTESIAN_POINT ( 'NONE',  ( 3.083589872104280705, 5.684939719841914929, 1.199719254218450271 ) ) ;
#19599 = PRESENTATION_LAYER_ASSIGNMENT (  '', '', ( #16170 ) ) ;
#19601 = ORIENTED_EDGE ( 'NONE', *, *, #19728, .T. ) ;
#19600 = CARTESIAN_POINT ( 'NONE',  ( -6.954406449166956605, 7.078172043641714595, -0.7998128361456362523 ) ) ;
#19602 = CARTESIAN_POINT ( 'NONE',  ( 5.004104291928844539, 8.031804922028364047, 1.127571413376940335 ) ) ;
#19603 = CARTESIAN_POINT ( 'NONE',  ( 5.395861176733054876, 0.1455124041884261754, 2.010896217931843921 ) ) ;
#19604 = CARTESIAN_POINT ( 'NONE',  ( 3.011469152984513009, -0.9080073089506625061, -1.601583425259824001 ) ) ;
#19605 = CARTESIAN_POINT ( 'NONE',  ( 0.07661050522431848975, 5.726661425590173771, -2.304854160881860903 ) ) ;
#19606 = CARTESIAN_POINT ( 'NONE',  ( 2.543975960257907953, -1.711040505396358657, -1.548661362299937228 ) ) ;
#19607 = CARTESIAN_POINT ( 'NONE',  ( 6.668631453075247073, 8.873432343378178544, -1.599625672291281386 ) ) ;
#19608 = CARTESIAN_POINT ( 'NONE',  ( 4.569695524216377258, 2.097929177840287540, -0.5203329012281321386 ) ) ;
#19609 = CARTESIAN_POINT ( 'NONE',  ( 9.271078113646423091, 9.710679308875986848, 1.040834085586084257E-14 ) ) ;
#19610 = CARTESIAN_POINT ( 'NONE',  ( 0.5209107642259405146, -1.843744896352221829, 0.6102272969235060796 ) ) ;
#19611 = CARTESIAN_POINT ( 'NONE',  ( -4.466521540698216164, 7.298359999868178960, -1.199719254218452047 ) ) ;
#19612 = STYLED_ITEM ( 'NONE', ( #135238 ), #147970 ) ;
#19613 = CARTESIAN_POINT ( 'NONE',  ( -9.434262096590540381, 15.42050698104736739, -7.415936069015691245 ) ) ;
#19614 = CARTESIAN_POINT ( 'NONE',  ( 3.168673215318769110, -1.727878594304608217, -0.7172629358194044791 ) ) ;
#19615 = CARTESIAN_POINT ( 'NONE',  ( 0.5968690581132638506, 1.641441770537595435, -1.091469919712923176 ) ) ;
#19617 = CARTESIAN_POINT ( 'NONE',  ( -5.915100157312088491, 10.12297696016459092, -0.7998128361456362523 ) ) ;
#19616 = CARTESIAN_POINT ( 'NONE',  ( 1.364683531249990311, 5.363541667008086655, 0.7879004041258500513 ) ) ;
#19618 = CARTESIAN_POINT ( 'NONE',  ( 1.260703874955213744, 0.8971468365699288849, 2.016480257658866737 ) ) ;
#19619 = CARTESIAN_POINT ( 'NONE',  ( 6.360183458142182111, 6.592837920686895004, -0.7216878364870427109 ) ) ;
#19620 = CARTESIAN_POINT ( 'NONE',  ( 4.878236342818665250, 4.585697242910212523, 1.040834085586084257E-14 ) ) ;
#19621 = CARTESIAN_POINT ( 'NONE',  ( -5.786632634934295361, 5.645492917045106473, 0.7998128361456341429 ) ) ;
#19622 = COLOUR_RGB ( '', 0.09019608, 0.27058824, 0.51372549) ;
#19623 = CARTESIAN_POINT ( 'NONE',  ( -6.685579144870156476, 9.853573864773576219, 1.082531754730549967 ) ) ;
#19624 = CARTESIAN_POINT ( 'NONE',  ( 6.754760782388981255, -1.524083220479439005, 1.250168222439652421 ) ) ;
#19625 = CARTESIAN_POINT ( 'NONE',  ( 6.358097629954328589, 2.302029506726857466, -0.1628147022267756039 ) ) ;
#19626 = CARTESIAN_POINT ( 'NONE',  ( 0.9066075625437097774, 0.5660373911110065936, 1.878450800843839419 ) ) ;
#19627 = CARTESIAN_POINT ( 'NONE',  ( 3.977431857364383205, -0.1567958407116451236, 2.056696387209145716 ) ) ;
#19628 = CARTESIAN_POINT ( 'NONE',  ( 5.585596099150174965, 7.539614753807099667, -1.443375672974057666 ) ) ;
#19629 = CARTESIAN_POINT ( 'NONE',  ( 5.936491157937257235, 8.019268665717216749, 1.599625672291268286 ) ) ;
#19630 = VERTEX_POINT ( 'NONE', #68818 ) ;
#19631 = CARTESIAN_POINT ( 'NONE',  ( 8.120970824461352322, 9.537182719035495637, -1.082531754730543083 ) ) ;
#19632 = CARTESIAN_POINT ( 'NONE',  ( -0.6823417656250212460, 4.113541667008085767, 1.181850606188767472 ) ) ;
#19633 = CARTESIAN_POINT ( 'NONE',  ( 11.84668730067608244, 12.59363775091781079, -1.400000000000002132 ) ) ;
#19634 = CARTESIAN_POINT ( 'NONE',  ( 3.334942598837264960, 6.834590765378040444, 1.214306433183764966E-14 ) ) ;
#19635 = CARTESIAN_POINT ( 'NONE',  ( 6.496539221175353873, 2.146586416477539672, 0.3252249059467678394 ) ) ;
#19637 = CARTESIAN_POINT ( 'NONE',  ( 6.093280168761200599, -0.6138376400152152357, 1.736067454429328416 ) ) ;
#19636 = CARTESIAN_POINT ( 'NONE',  ( -5.599154252763867134, 5.634694171087028636, 0.000000000000000000 ) ) ;
#19638 = ADVANCED_FACE ( 'NONE', ( #186854 ), #103657, .T. ) ;
#19639 = CARTESIAN_POINT ( 'NONE',  ( -2.493461049780994365, 3.507114751586604129, 11.73081193161140590 ) ) ;
#19640 = CARTESIAN_POINT ( 'NONE',  ( -11.80251051724185984, 12.30000000000000071, -1.695257889419022002 ) ) ;
#19641 = CARTESIAN_POINT ( 'NONE',  ( 0.8779421195594695471, -1.044212112285093585, 1.551753832453220294 ) ) ;
#19642 = CARTESIAN_POINT ( 'NONE',  ( -4.338283617754775889, 7.407916770541659091, 1.160293660280581785 ) ) ;
#19643 = CARTESIAN_POINT ( 'NONE',  ( 5.300918301777743480, 7.749796750553542779, -1.302405036909856761 ) ) ;
#19644 = CARTESIAN_POINT ( 'NONE',  ( -1.364683531250010295, 4.842708333674756283, 0.7879004041258379498 ) ) ;
#19645 = CARTESIAN_POINT ( 'NONE',  ( 1.488763880571320808, -1.816176428755595706, -0.5988469716494762007 ) ) ;
#19647 = EDGE_CURVE ( 'NONE', #143793, #163734, #175460, .T. ) ;
#19646 = CARTESIAN_POINT ( 'NONE',  ( 2.676313443976061190, -1.692906749566702507, -0.5160995803213176414 ) ) ;
#19648 = CARTESIAN_POINT ( 'NONE',  ( 1.119614361207950548, -0.4638517909370845071, 1.855054000551699778 ) ) ;
#19650 = CARTESIAN_POINT ( 'NONE',  ( 4.147977739690055898, 0.9062469702798245930, 1.687694244345463224 ) ) ;
#19649 = CARTESIAN_POINT ( 'NONE',  ( -8.371269781434001800, 11.85389961405997816, -1.199719254218446718 ) ) ;
#19651 = CARTESIAN_POINT ( 'NONE',  ( -2.974142338115852269, 6.685868392857900133, 0.1038623869373533903 ) ) ;
#19652 = CARTESIAN_POINT ( 'NONE',  ( 5.266046268760843141, -1.960244874886694744, 0.1909964021715639393 ) ) ;
#19653 = CARTESIAN_POINT ( 'NONE',  ( 1.055114822555893728, 0.4192091730233596381, 2.078585086915801128 ) ) ;
#19654 = CARTESIAN_POINT ( 'NONE',  ( 2.325000000000005507, -0.05106137233530404218, -0.4999999999999945044 ) ) ;
#19655 = CARTESIAN_POINT ( 'NONE',  ( 4.434354141042872399, 1.834536173243521917, 0.3649259964926266364 ) ) ;
#19657 = VERTEX_POINT ( 'NONE', #162409 ) ;
#19656 = CARTESIAN_POINT ( 'NONE',  ( 5.900961842893762466, 1.406060569669766114, -0.9988219321918601068 ) ) ;
#19659 = CARTESIAN_POINT ( 'NONE',  ( 4.541618270897912701, 4.400902192243413502, 1.214306433183764966E-14 ) ) ;
#19658 = CARTESIAN_POINT ( 'NONE',  ( 3.000804911251079510, -0.6410980074830170405, -2.111705341948390657 ) ) ;
#19660 = CARTESIAN_POINT ( 'NONE',  ( -1.364683531250010295, 4.842708333674756283, 0.7879004041258379498 ) ) ;
#19661 = CARTESIAN_POINT ( 'NONE',  ( 0.9946673667629982729, 2.031838985545178389, 0.3545390999590279368 ) ) ;
#19662 = CARTESIAN_POINT ( 'NONE',  ( 5.615048174354031474, 9.702639970055050966, 0.7998128361456462443 ) ) ;
#19663 = CARTESIAN_POINT ( 'NONE',  ( -8.829384350997580455, 11.32403438096243775, 1.599625672291269396 ) ) ;
#19664 = CARTESIAN_POINT ( 'NONE',  ( 3.919715808126649659, 7.587102519540811940, 0.000000000000000000 ) ) ;
#19665 = CARTESIAN_POINT ( 'NONE',  ( -3.421390767332295635, -0.02279856766746886365, -0.4144453184043222493 ) ) ;
#19666 = CARTESIAN_POINT ( 'NONE',  ( -7.722692672890413945, -6.459788825448667282, -7.834474503270543622 ) ) ;
#19667 = ORIENTED_EDGE ( 'NONE', *, *, #103048, .T. ) ;
#19668 = CARTESIAN_POINT ( 'NONE',  ( 3.385274849524767316, 0.04804411014160993310, 2.069964801482151895 ) ) ;
#19669 = CARTESIAN_POINT ( 'NONE',  ( 1.499999999999987121, 4.545833333333352932, -0.8660254037844323793 ) ) ;
#19670 = CARTESIAN_POINT ( 'NONE',  ( 5.769158057814842699, 6.689438141327490150, 1.199719254218462483 ) ) ;
#19671 = CARTESIAN_POINT ( 'NONE',  ( -6.468510628652166972, 6.779004017053734898, -0.3101152288892006781 ) ) ;
#19672 = CARTESIAN_POINT ( 'NONE',  ( 0.9440171659906453350, -1.283125807103436600, -1.559678575094858077 ) ) ;
#19673 = CARTESIAN_POINT ( 'NONE',  ( -0.7499999999999972244, 5.858333333333353821, -1.299038105676652011 ) ) ;
#19675 = CARTESIAN_POINT ( 'NONE',  ( 7.280365300858406385, 11.43758391773608984, 1.040834085586084257E-14 ) ) ;
#19674 = CARTESIAN_POINT ( 'NONE',  ( 0.1745949693968874838, 0.2569705180060793404, -1.790672585839627740 ) ) ;
#19676 = CARTESIAN_POINT ( 'NONE',  ( 6.556017512941495262, 1.755498886817616677, -0.9912500394320120645 ) ) ;
#19677 = CARTESIAN_POINT ( 'NONE',  ( 6.034394305845959927, 0.6080466156053351279, 1.816710885969755163 ) ) ;
#19678 = CARTESIAN_POINT ( 'NONE',  ( 6.639320575229281651, -0.0007625845807879281287, 2.103388539994067497 ) ) ;
#19679 = CARTESIAN_POINT ( 'NONE',  ( 3.333693798916517625, 0.9835563995168915552, -1.958507884819527867 ) ) ;
#19680 =( BOUNDED_CURVE ( )  B_SPLINE_CURVE ( 2, ( #121893, #139139, #55738, #171621, #56809, #6960, #169489 ),
 .UNSPECIFIED., .F., .T. ) 
 B_SPLINE_CURVE_WITH_KNOTS ( ( 3, 2, 2, 3 ),
 ( 0.3214285714285716744, 0.3273809523809525501, 0.3333333333333334259, 0.3392857142857143571 ),
 .UNSPECIFIED. ) 
 CURVE ( )  GEOMETRIC_REPRESENTATION_ITEM ( )  RATIONAL_B_SPLINE_CURVE ( ( 0.9999999999999950040, 0.8660254037844437036, 1.000000000000000000, 0.8660254037844387076, 1.000000000000000000, 0.8660254037844374864, 1.000000000000001332 ) ) 
 REPRESENTATION_ITEM ( '' )  );
#19682 = AXIS2_PLACEMENT_3D ( 'NONE', #32608, #49927, #101873 ) ;
#19681 = CARTESIAN_POINT ( 'NONE',  ( -0.7499999999999972244, 3.389583334016149863, -1.299038105676652011 ) ) ;
#19683 = CARTESIAN_POINT ( 'NONE',  ( 3.269685606991072468, 0.4601866041431811327, -1.856093204100267124 ) ) ;
#19684 = CARTESIAN_POINT ( 'NONE',  ( -5.525111292768871252, 6.404716915440499037, -1.199719254218446718 ) ) ;
#19685 = CARTESIAN_POINT ( 'NONE',  ( 3.836594282542914236, 5.499112634431936542, 1.443375672974062551 ) ) ;
#19687 = CARTESIAN_POINT ( 'NONE',  ( 0.6675924852559199651, 1.356316336250670496, 1.492241973137248934 ) ) ;
#19686 = CARTESIAN_POINT ( 'NONE',  ( -10.29027540264791440, 11.10766884595181203, 0.7216878364870438212 ) ) ;
#19688 = CARTESIAN_POINT ( 'NONE',  ( -0.6823417656250039265, 10.38020833367472839, -1.181850606188755259 ) ) ;
#19690 = CARTESIAN_POINT ( 'NONE',  ( -4.956387674247580755, 7.940146832334256111, 1.199719254218452935 ) ) ;
#19689 = CARTESIAN_POINT ( 'NONE',  ( -0.09359539843449991847, -0.9867227890145138236, -2.066685918926200571 ) ) ;
#19692 = ORIENTED_EDGE ( 'NONE', *, *, #138353, .T. ) ;
#19691 = CARTESIAN_POINT ( 'NONE',  ( 4.541862270049739969, 0.7358753100316551832, -1.560062421326340987 ) ) ;
#19693 = CARTESIAN_POINT ( 'NONE',  ( 0.1399997263885794929, 4.089933038008564559, -2.554595152914000078 ) ) ;
#19694 = CARTESIAN_POINT ( 'NONE',  ( 7.121056995675668411, 9.330985799753529264, -1.599625672291262513 ) ) ;
#19695 = CARTESIAN_POINT ( 'NONE',  ( 4.359110081993588182, 5.044382169536003602, -1.199719254218452047 ) ) ;
#19696 = DIRECTION ( 'NONE',  ( 0.000000000000000000, 0.7999999999999973799, -0.6000000000000034195 ) ) ;
#19697 = CARTESIAN_POINT ( 'NONE',  ( 1.680054527999317759, -1.087118939145682583, -1.632918184844594611 ) ) ;
#19698 = CARTESIAN_POINT ( 'NONE',  ( 11.44779965693254375, 10.10313923201305997, -3.599999932276613190 ) ) ;
#19699 = CARTESIAN_POINT ( 'NONE',  ( 4.976006071415387311, 5.764094157194782575, 1.199719254218462483 ) ) ;
#19700 = CARTESIAN_POINT ( 'NONE',  ( 0.07536363704233400851, 2.864322694550157866, -2.632457840217194089 ) ) ;
#19701 = ORIENTED_EDGE ( 'NONE', *, *, #126447, .F. ) ;
#19702 = CARTESIAN_POINT ( 'NONE',  ( 1.495620097461134202E-12, -5.796408561410189897, 10.41272866534516695 ) ) ;
#19703 = ORIENTED_EDGE ( 'NONE', *, *, #10155, .T. ) ;
#19704 = CARTESIAN_POINT ( 'NONE',  ( 4.406777823604307365, -0.4013596350818599556, -1.766266891646672166 ) ) ;
#19705 = ORIENTED_EDGE ( 'NONE', *, *, #82182, .F. ) ;
#19706 = CARTESIAN_POINT ( 'NONE',  ( 6.475954649182838807, 7.584310507915338562, 1.199719254218452047 ) ) ;
#19707 = PLANE ( 'NONE',  #53151 ) ;
#19708 = CARTESIAN_POINT ( 'NONE',  ( 5.303285216261115487, 1.594816061929973827, -0.8590795265051922591 ) ) ;
#19709 = CARTESIAN_POINT ( 'NONE',  ( 5.831415467209187575, 9.817418788470464008, 0.000000000000000000 ) ) ;
#19710 = CARTESIAN_POINT ( 'NONE',  ( 10.95308175811721085, 13.79999999999999893, -1.800000000000001155 ) ) ;
#19711 = CARTESIAN_POINT ( 'NONE',  ( 5.191320393234815533, 6.438618948542633724, -1.178512179637403623 ) ) ;
#19712 = ADVANCED_FACE ( 'NONE', ( #61695 ), #31341, .F. ) ;
#19713 = CARTESIAN_POINT ( 'NONE',  ( 6.689920442068890694, -1.216917952458838270, -1.408172490277598721 ) ) ;
#19714 = EDGE_CURVE ( 'NONE', #164705, #138703, #64510, .T. ) ;
#19715 = CARTESIAN_POINT ( 'NONE',  ( 2.601083430876732105, -0.1850255667073404386, 1.906624535778883578 ) ) ;
#19716 = CARTESIAN_POINT ( 'NONE',  ( -6.505896022970769188, -8.148356111791729361, -6.958662999125635018 ) ) ;
#19717 = CARTESIAN_POINT ( 'NONE',  ( -11.80100919632472589, 4.809168931535662495, -4.927235675632552159 ) ) ;
#19718 = B_SPLINE_CURVE_WITH_KNOTS ( 'NONE', 3,
 ( #165250, #183624, #197740, #126710, #180444, #143991 ),
 .UNSPECIFIED., .F., .F.,
 ( 4, 2, 4 ),
 ( 9.243101720622088096E-18, 9.928037272730919299E-05, 0.0001985607454546091432 ),
 .UNSPECIFIED. ) ;
#19719 = DIRECTION ( 'NONE',  ( 0.000000000000000000, 1.000000000000000000, 0.000000000000000000 ) ) ;
#19720 = CARTESIAN_POINT ( 'NONE',  ( 4.853455804012203778, 8.606189504748821051, 0.7216878364870438212 ) ) ;
#19721 = CARTESIAN_POINT ( 'NONE',  ( -8.337901282724359930, 12.67137589657970409, 1.040834085586084257E-14 ) ) ;
#19722 = CARTESIAN_POINT ( 'NONE',  ( 0.8663662989462637132, 1.066309655776727539, 1.880320099339624296 ) ) ;
#19723 = CARTESIAN_POINT ( 'NONE',  ( -4.925354943514475003, 8.968274210734028529, 0.000000000000000000 ) ) ;
#19724 = CARTESIAN_POINT ( 'NONE',  ( 6.364626766972446781, 6.390095747748157251, 0.7998128361456352531 ) ) ;
#19725 = CARTESIAN_POINT ( 'NONE',  ( 0.9908991873810431006, 1.612194894691898250, -0.8564790819722142290 ) ) ;
#19726 = CARTESIAN_POINT ( 'NONE',  ( -3.391510981712833939, 7.108513245306943062, 0.7998128361456341429 ) ) ;
#19727 = CARTESIAN_POINT ( 'NONE',  ( 2.696107482849848580, -1.820545782403935720, -0.1364615833806467338 ) ) ;
#19728 = EDGE_CURVE ( 'NONE', #38781, #22085, #81994, .T. ) ;
#19729 = CARTESIAN_POINT ( 'NONE',  ( -5.335766472694970730, 4.384919054141817263, 2.499999999999998668 ) ) ;
#19730 = CARTESIAN_POINT ( 'NONE',  ( 1.863391182279940494, -1.538030936729195552, -1.136358088520472931 ) ) ;
#19731 = CARTESIAN_POINT ( 'NONE',  ( 3.156658437648862225, -0.5693117071641734528, -1.885488911330883255 ) ) ;
#19732 = CARTESIAN_POINT ( 'NONE',  ( 3.298316653532318732, 1.529317551288728483, -1.196868631420761053 ) ) ;
#19733 = CARTESIAN_POINT ( 'NONE',  ( -5.752402313948099533, 9.933162809573264695, -0.7998128361456362523 ) ) ;
#19735 = CARTESIAN_POINT ( 'NONE',  ( 4.131183091185314460, 1.940096312829143299, 0.8565103500411813675 ) ) ;
#19734 = CARTESIAN_POINT ( 'NONE',  ( 6.156284269057003655, 9.340026192945279249, -1.199719254218452047 ) ) ;
#19736 = FACE_OUTER_BOUND ( 'NONE', #93501, .T. ) ;
#19737 = CARTESIAN_POINT ( 'NONE',  ( 9.759171643738394408, 10.28012176064996197, 0.000000000000000000 ) ) ;
#19738 = CARTESIAN_POINT ( 'NONE',  ( 5.922464229660435286, 6.137557782886555735, -0.7752440879994120237 ) ) ;
#19739 = FACE_OUTER_BOUND ( 'NONE', #21516, .T. ) ;
#19740 = CARTESIAN_POINT ( 'NONE',  ( 6.873057527484919937, 6.983264968346048818, 0.7998128361456352531 ) ) ;
#19741 = CARTESIAN_POINT ( 'NONE',  ( 11.89942855770813956, 12.30000000000000071, -0.7000000000000009548 ) ) ;
#19742 = CARTESIAN_POINT ( 'NONE',  ( 4.371595934376539816, 1.770262903079304451, -0.4459408992859363319 ) ) ;
#19743 = CARTESIAN_POINT ( 'NONE',  ( -3.894033820048823813, 8.999999999999998224, 0.7749999999999996891 ) ) ;
#19744 = CARTESIAN_POINT ( 'NONE',  ( -7.199016379176422120, 11.34267684244042584, 0.000000000000000000 ) ) ;
#19745 = VECTOR ( 'NONE', #42572, 1000.000000000000000 ) ;
#19746 = CARTESIAN_POINT ( 'NONE',  ( -4.845071979149651042, 8.194897641035423064, 0.9605101338234197650 ) ) ;
#19747 = DIRECTION ( 'NONE',  ( 0.000000000000000000, -0.000000000000000000, -1.000000000000000000 ) ) ;
#19748 = CARTESIAN_POINT ( 'NONE',  ( 4.557402362779487959, 0.4096945884842878582, -1.825068887194372991 ) ) ;
#19749 = CARTESIAN_POINT ( 'NONE',  ( 8.046927864910717432, 9.346836249606042202, 1.199719254218462483 ) ) ;
#19750 = CARTESIAN_POINT ( 'NONE',  ( 3.105993306306195301, -1.924270352051945299, 0.09518456514568535143 ) ) ;
#19751 = CARTESIAN_POINT ( 'NONE',  ( 6.789906393989944888, -1.279003670332454989, -1.487618534420579897 ) ) ;
#19752 = CARTESIAN_POINT ( 'NONE',  ( 3.408985558832261731, 6.064568021024562938, 1.199719254218462483 ) ) ;
#19753 = CARTESIAN_POINT ( 'NONE',  ( -1.364683531250014514, 9.651041667008064096, -0.7879004041258335089 ) ) ;
#19754 = CARTESIAN_POINT ( 'NONE',  ( -5.876569516519495551, 8.943415971659659292, 1.199719254218452047 ) ) ;
#19755 = CARTESIAN_POINT ( 'NONE',  ( 3.358669367883368118, 4.941533567329135401, -1.599625672291262513 ) ) ;
#19756 = CARTESIAN_POINT ( 'NONE',  ( -5.139949632912262700, 5.169231791251960750, 0.7216878364870257245 ) ) ;
#19757 = CARTESIAN_POINT ( 'NONE',  ( 1.423615893443540337, -1.536295912932123642, -1.457111741773434943 ) ) ;
#19758 = CARTESIAN_POINT ( 'NONE',  ( 8.971744963941056028, 11.49012176272984931, 1.599625672291281386 ) ) ;
#19759 = CARTESIAN_POINT ( 'NONE',  ( 0.7499999999999885647, 3.566666666666690411, -1.299038105676658228 ) ) ;
#19760 = CARTESIAN_POINT ( 'NONE',  ( 6.754741982670550371, -0.5462536098296210119, -1.996853278248729824 ) ) ;
#19762 = CARTESIAN_POINT ( 'NONE',  ( 4.085089063302896228, 7.714230733137671159, -0.6301764584765887633 ) ) ;
#19761 = CARTESIAN_POINT ( 'NONE',  ( 0.7492455685023796663, 1.839184785914184994, -0.09005233288367914257 ) ) ;
#19763 = CARTESIAN_POINT ( 'NONE',  ( 0.2635768167446932986, -2.297931531924101822, -0.05306211189425556751 ) ) ;
#19764 = CARTESIAN_POINT ( 'NONE',  ( 5.341549334104184865, 8.215262742221458581, 1.082531754730558626 ) ) ;
#19765 = CARTESIAN_POINT ( 'NONE',  ( 3.580761967785000888, 7.191656372475549119, -0.7216878364870338292 ) ) ;
#19766 = CARTESIAN_POINT ( 'NONE',  ( 1.623385997035782013, -2.157220310706788435, 0.7755101668525423708 ) ) ;
#19767 = CARTESIAN_POINT ( 'NONE',  ( -9.495732322661975644, -8.202835266173753581, 0.2934966634902112514 ) ) ;
#19768 = VECTOR ( 'NONE', #210248, 1000.000000000000000 ) ;
#19769 = CARTESIAN_POINT ( 'NONE',  ( -5.448397627845328550, 7.449826213943242514, 1.599625672291263179 ) ) ;
#19770 = CARTESIAN_POINT ( 'NONE',  ( 6.562452659285362699, -1.776534117310492711, -0.7846822752179910543 ) ) ;
#19771 = ORIENTED_EDGE ( 'NONE', *, *, #140437, .F. ) ;
#19772 = CARTESIAN_POINT ( 'NONE',  ( 9.056483423804305488, 9.668244870634271848, 1.040834085586084257E-14 ) ) ;
#19773 = EDGE_CURVE ( 'NONE', #120691, #164262, #96354, .T. ) ;
#19774 = CARTESIAN_POINT ( 'NONE',  ( 1.072522059793120652, 0.8197897455473095452, 1.838922316899212372 ) ) ;
#19775 = CARTESIAN_POINT ( 'NONE',  ( 6.403528931544730796, -1.954801056786956259, 0.4946215565981848528 ) ) ;
#19777 = LINE ( 'NONE', #69578, #202302 ) ;
#19776 = CARTESIAN_POINT ( 'NONE',  ( -7.018317073368468328, 11.33978701890523233, -0.7998128361456291469 ) ) ;
#19778 = CARTESIAN_POINT ( 'NONE',  ( -10.43230948805442893, 5.066484524551064794, 5.254757398418679060 ) ) ;
#19780 = CARTESIAN_POINT ( 'NONE',  ( 1.129378208368720271, -1.118813933885588474, -1.371354111526525754 ) ) ;
#19779 = CARTESIAN_POINT ( 'NONE',  ( 3.310569631373377231, 1.890246369116010960, 0.8934441069041214600 ) ) ;
#19781 = CARTESIAN_POINT ( 'NONE',  ( 4.207966135563057541, 7.175396087857926375, 1.156120096431498379 ) ) ;
#19783 = CARTESIAN_POINT ( 'NONE',  ( 5.578174268327147800, -2.235363620237617255, -0.5069547310770585735 ) ) ;
#19782 = CARTESIAN_POINT ( 'NONE',  ( -1.420000000000001039, 7.176846818246207960, -4.202462424328208712 ) ) ;
#19784 = CARTESIAN_POINT ( 'NONE',  ( 3.275097224137039742, 1.105054647683247460, 1.344453793780414186 ) ) ;
#19785 = CARTESIAN_POINT ( 'NONE',  ( 8.757677159423465696, 12.30470822171437284, 1.199719254218450271 ) ) ;
#19786 = CARTESIAN_POINT ( 'NONE',  ( 4.386945222473598527, 7.275797305264619652, -1.199719254218452047 ) ) ;
#19787 = CARTESIAN_POINT ( 'NONE',  ( 3.690549081386824248, -1.031632686913460883, -1.393354295182136715 ) ) ;
#19788 = CARTESIAN_POINT ( 'NONE',  ( 3.139314614211644816, -0.1572037376256547880, -2.165524352769617078 ) ) ;
#19789 = CARTESIAN_POINT ( 'NONE',  ( 5.281064527722868718, 6.119995689553514140, 1.199719254218462483 ) ) ;
#19790 = CARTESIAN_POINT ( 'NONE',  ( 4.153529959351897283, 1.954779968807466295, -0.4946301968136583849 ) ) ;
#19791 = CARTESIAN_POINT ( 'NONE',  ( 1.437500000000001110, 1.451031289061064156, -1.451031289061176288 ) ) ;
#19792 = CARTESIAN_POINT ( 'NONE',  ( -1.201851678989727383E-14, 4.618750000682821266, -1.732050807568863648 ) ) ;
#19793 = CARTESIAN_POINT ( 'NONE',  ( 1.694233118518298165, -1.916858602850049609, -0.1915058630488040703 ) ) ;
#19794 = CARTESIAN_POINT ( 'NONE',  ( -0.7500000000000006661, 8.489583334016129967, -1.299038105676657340 ) ) ;
#19795 = CARTESIAN_POINT ( 'NONE',  ( 5.941669428368816952, -2.091911387875099670, 0.7476460515099275783 ) ) ;
#19796 = ORIENTED_EDGE ( 'NONE', *, *, #135923, .F. ) ;
#19797 = CARTESIAN_POINT ( 'NONE',  ( -0.1106856583840878927, 5.722746153615347886, -2.590994828783958592 ) ) ;
#19798 = CARTESIAN_POINT ( 'NONE',  ( -0.7500000000000006661, 2.108333333333357817, -1.299038105676652011 ) ) ;
#19799 = CARTESIAN_POINT ( 'NONE',  ( 5.587931867126699537, 9.671004278289832001, -0.7998128361456291469 ) ) ;
#19800 = CARTESIAN_POINT ( 'NONE',  ( 5.490689023410166847, 5.508151403507724808, -0.7216878364870207285 ) ) ;
#19801 = CARTESIAN_POINT ( 'NONE',  ( 3.285556943750000070, -1.684374999522043836, 0.000000000000000000 ) ) ;
#19802 = CARTESIAN_POINT ( 'NONE',  ( 0.9443249964648057215, -1.413213925058560028, -1.713760899525147874 ) ) ;
#19803 = CARTESIAN_POINT ( 'NONE',  ( 6.197705743426439540, -1.420020466879829302, -1.353909852041992767 ) ) ;
#19804 = CARTESIAN_POINT ( 'NONE',  ( 8.432808358020016826, 10.86136238915529084, 1.443375672974076540 ) ) ;
#19805 = CARTESIAN_POINT ( 'NONE',  ( -0.4461809497497637444, 3.122791860410086606, 1.949595486268986821 ) ) ;
#19806 = CARTESIAN_POINT ( 'NONE',  ( 0.3335754702045168330, -1.976410766185803691, 0.8757516042032786885 ) ) ;
#19807 = CARTESIAN_POINT ( 'NONE',  ( 5.041653019435334393, 6.975290837464928728, -1.599625672291269396 ) ) ;
#19808 = CARTESIAN_POINT ( 'NONE',  ( -4.990809943606286048, 5.955604701363006015, -1.082531754730549967 ) ) ;
#19809 = CARTESIAN_POINT ( 'NONE',  ( 4.633292856664962933, 0.003200217577232782832, -2.062851381006901352 ) ) ;
#19810 = CARTESIAN_POINT ( 'NONE',  ( -6.227272627378437342, 6.159572908229946187, -0.7998128361456291469 ) ) ;
#19811 = CARTESIAN_POINT ( 'NONE',  ( 0.7499999999999902300, 3.847916667349481123, -1.299038105676658228 ) ) ;
#19812 = CARTESIAN_POINT ( 'NONE',  ( -1.364683531250000748, -0.9906249996585805295, 0.000000000000000000 ) ) ;
#19813 = CARTESIAN_POINT ( 'NONE',  ( 6.204356031920277736, -0.6731288877953770511, -1.745422550748019441 ) ) ;
#19814 = CARTESIAN_POINT ( 'NONE',  ( 4.236742506082516790, 1.733672338021419179, -0.04812345329192367627 ) ) ;
#19815 = CARTESIAN_POINT ( 'NONE',  ( 3.280519990774858119, 1.572054556770419387, -0.7471684773981291938 ) ) ;
#19816 = CARTESIAN_POINT ( 'NONE',  ( 8.541273586484978253, 12.90864358430044589, 0.000000000000000000 ) ) ;
#19817 = ADVANCED_FACE ( 'NONE', ( #46526 ), #2408, .F. ) ;
#19818 = CARTESIAN_POINT ( 'NONE',  ( 1.681587762198969216, 1.584507396495305587, 1.656812167128306035 ) ) ;
#19819 = CARTESIAN_POINT ( 'NONE',  ( 1.364683531249988535, 3.467708333674749621, -0.7879004041258239610 ) ) ;
#19820 = CARTESIAN_POINT ( 'NONE',  ( 5.407793395736015363, -0.9409669688741102433, -1.867122848840888416 ) ) ;
#19821 = CARTESIAN_POINT ( 'NONE',  ( 0.1109373197970727615, -1.806229982939497658, 0.3559056038356380736 ) ) ;
#19822 = CARTESIAN_POINT ( 'NONE',  ( 0.08972248771634809550, -9.919998018256677597, 10.99963958991171786 ) ) ;
#19823 = CARTESIAN_POINT ( 'NONE',  ( 1.776017750421728270, 1.753029812786778940, -0.9963028777105964462 ) ) ;
#19824 = CARTESIAN_POINT ( 'NONE',  ( 0.2170718473699268236, -0.1031819972749977166, 2.189145592210713698 ) ) ;
#19825 = CARTESIAN_POINT ( 'NONE',  ( 7.121823250997191046, 13.97725337314594007, -9.255175167006054693 ) ) ;
#19826 = CARTESIAN_POINT ( 'NONE',  ( -8.877891658850122880, 9.251961778280284321, 0.7998128361456462443 ) ) ;
#19827 = CARTESIAN_POINT ( 'NONE',  ( 6.830610463186557624, 6.863467050006115677, 1.040834085586084257E-14 ) ) ;
#19828 = CARTESIAN_POINT ( 'NONE',  ( 2.526173596586390957, -2.097057114080549844, 0.3136139059176298871 ) ) ;
#19829 = STYLED_ITEM ( 'NONE', ( #74660 ), #20283 ) ;
#19830 = CARTESIAN_POINT ( 'NONE',  ( -1.402160292154681736E-14, -0.8031249996585825279, -1.575800808251665908 ) ) ;
#19832 = EDGE_CURVE ( 'NONE', #71609, #191915, #188658, .T. ) ;
#19831 = CARTESIAN_POINT ( 'NONE',  ( 5.514214477338500231, -0.8245889995748825196, -1.628937154514856545 ) ) ;
#19833 = ORIENTED_EDGE ( 'NONE', *, *, #17156, .F. ) ;
#19834 = CARTESIAN_POINT ( 'NONE',  ( -6.957269102468015554, 8.145844036748005834, 1.199719254218452047 ) ) ;
#19835 = CARTESIAN_POINT ( 'NONE',  ( 1.737499999999999378, -3.922916665710749040, -3.009438278150925683 ) ) ;
#19836 = CARTESIAN_POINT ( 'NONE',  ( -5.422371370461663176, 8.413518134592214537, -1.199719254218446718 ) ) ;
#19837 = CARTESIAN_POINT ( 'NONE',  ( 2.250265822158686646, 0.9482326530925830887, -1.783330763309778577 ) ) ;
#19838 = CARTESIAN_POINT ( 'NONE',  ( 6.229534195615700654, -2.079954537573494466, 0.7377168454194837910 ) ) ;
#19839 = CARTESIAN_POINT ( 'NONE',  ( 9.297140650669039275, 11.86975006391249643, 1.599625672291281386 ) ) ;
#19840 = CARTESIAN_POINT ( 'NONE',  ( 4.610102165239228889, 1.860615736367857265, -0.04253844368732987574 ) ) ;
#19841 = CARTESIAN_POINT ( 'NONE',  ( 9.887974103068218668, 10.43039129653476493, 0.7998128361456462443 ) ) ;
#19842 = CARTESIAN_POINT ( 'NONE',  ( 11.84668730067608244, 13.40000000000000036, -1.400000000000001688 ) ) ;
#19843 = ORIENTED_EDGE ( 'NONE', *, *, #54959, .T. ) ;
#19844 = CARTESIAN_POINT ( 'NONE',  ( -3.253066792275140173, 5.882662793374543675, 1.199719254218462483 ) ) ;
#19845 = CARTESIAN_POINT ( 'NONE',  ( -8.507905087775398556, 9.884643009614800135, 1.199719254218462483 ) ) ;
#19846 = CARTESIAN_POINT ( 'NONE',  ( 5.514214477338500231, -0.8245889995748825196, -1.628937154514856545 ) ) ;
#19848 = CARTESIAN_POINT ( 'NONE',  ( -4.103288207896339301, 7.680416417065718093, 0.7589585138018557497 ) ) ;
#19847 = CARTESIAN_POINT ( 'NONE',  ( -5.589704470584107909, 9.743348658981940247, -0.7998128361456362523 ) ) ;
#19849 = CARTESIAN_POINT ( 'NONE',  ( -1.364683531250014514, -1.011458332991911568, -0.7879004041258359514 ) ) ;
#19850 = CARTESIAN_POINT ( 'NONE',  ( 1.422726403049366706, 0.6964842469411072212, 1.588000322196560399 ) ) ;
#19851 = CARTESIAN_POINT ( 'NONE',  ( 0.2162406733101406298, -0.09061050886127393345, 1.738091409524551878 ) ) ;
#19853 = CARTESIAN_POINT ( 'NONE',  ( 7.131225611108085616, 10.30321839872603462, 1.082531754730558626 ) ) ;
#19852 = CARTESIAN_POINT ( 'NONE',  ( 5.883493432195608719, 2.134490442297873880, -0.8776364701479767438 ) ) ;
#19854 = CARTESIAN_POINT ( 'NONE',  ( 3.217027588192558074, 6.975225629525113824, -1.734723475976807094E-15 ) ) ;
#19855 = CARTESIAN_POINT ( 'NONE',  ( 1.704443381354688203, -0.7389896827423731995, -1.923919429860524888 ) ) ;
#19856 = CARTESIAN_POINT ( 'NONE',  ( 4.794779880727245036, 8.745660294157122649, -0.7998128361456281477 ) ) ;
#19857 = CARTESIAN_POINT ( 'NONE',  ( 0.3157796101352361440, -1.620936768121715499, 1.198674607299075934 ) ) ;
#19858 = CARTESIAN_POINT ( 'NONE',  ( -0.3282377607281401488, 0.9486645496846495274, -1.225000000000020961 ) ) ;
#19859 = CARTESIAN_POINT ( 'NONE',  ( -4.762657100150483380, 8.778460060142702304, 0.000000000000000000 ) ) ;
#19860 = EDGE_CURVE ( 'NONE', #127955, #183713, #151657, .T. ) ;
#19861 = CARTESIAN_POINT ( 'NONE',  ( 0.2331951027847931901, -1.803461566636242797, 0.7967608462288151561 ) ) ;
#19862 = CIRCLE ( 'NONE', #37190, 2.250000000000006661 ) ;
#19864 = CARTESIAN_POINT ( 'NONE',  ( -7.783789588021474692, 8.253711738879413673, 0.7216878364870317197 ) ) ;
#19863 = CARTESIAN_POINT ( 'NONE',  ( 3.340010735810138520, -1.142844047782382466, -1.533173144288489276 ) ) ;
#19865 = CARTESIAN_POINT ( 'NONE',  ( 4.740968412965463230, 0.3751893352213676591, 2.174603215771487630 ) ) ;
#19866 = CARTESIAN_POINT ( 'NONE',  ( 1.224999999999961009, 1.708333334016139959, -0.7072540797573118043 ) ) ;
#19867 = CARTESIAN_POINT ( 'NONE',  ( -6.902509602688818191, 9.146290184594002781, -1.443375672974066548 ) ) ;
#19868 = CARTESIAN_POINT ( 'NONE',  ( 3.892599500454932304, 7.555466827257172113, 0.7216878364870257245 ) ) ;
#19869 = CARTESIAN_POINT ( 'NONE',  ( -3.621436428181653788, 7.239109909604962922, 0.7216878364870338292 ) ) ;
#19870 = CARTESIAN_POINT ( 'NONE',  ( 6.481110812017948142, -1.938455339442773706, -0.8599551062365148324 ) ) ;
#19871 = ORIENTED_EDGE ( 'NONE', *, *, #81363, .T. ) ;
#19872 = CARTESIAN_POINT ( 'NONE',  ( 3.153680125570026416, -1.885591857120081372, -1.329971080218894874 ) ) ;
#19873 = CARTESIAN_POINT ( 'NONE',  ( 4.949637131784443866, 1.452432516441283905, 1.319008059494260143 ) ) ;
#19874 = CARTESIAN_POINT ( 'NONE',  ( 0.9187138386215136787, -1.424830647414500051, 1.348730089142296418 ) ) ;
#19875 = CARTESIAN_POINT ( 'NONE',  ( 7.459735474692968715, 15.41013697600841859, 9.344700516680960689 ) ) ;
#19876 = CARTESIAN_POINT ( 'NONE',  ( 0.07933194154487524519, -7.246166700194011767, -9.499668754385622194 ) ) ;
#19877 = ORIENTED_EDGE ( 'NONE', *, *, #129757, .T. ) ;
#19878 = CARTESIAN_POINT ( 'NONE',  ( 0.5677576367011258895, 1.426771234092726104, 1.564575111376417915 ) ) ;
#19879 = CARTESIAN_POINT ( 'NONE',  ( -8.320953590485107298, 10.73086516036454618, 1.599625672291269396 ) ) ;
#19880 = CARTESIAN_POINT ( 'NONE',  ( -0.02377707250108065939, -0.1326659201078099481, -1.811169398030491928 ) ) ;
#19881 = CARTESIAN_POINT ( 'NONE',  ( 3.133805249272236804, 2.063032676455050396, -0.6766426178266419234 ) ) ;
#19882 = CARTESIAN_POINT ( 'NONE',  ( 0.3857320732078021175, 2.894052512584739834, 1.963429802559124138 ) ) ;
#19883 = CARTESIAN_POINT ( 'NONE',  ( 0.5102161431939798986, -0.7575819503438313562, 1.980855387931411915 ) ) ;
#19884 = CARTESIAN_POINT ( 'NONE',  ( 1.499999999999987121, 1.827083334016151861, -0.8660254037844253849 ) ) ;
#19885 = CARTESIAN_POINT ( 'NONE',  ( 9.915090410295563927, 10.46202698829998567, -0.7998128361456281477 ) ) ;
#19886 = CARTESIAN_POINT ( 'NONE',  ( 2.977454500823585093, 6.499579965040511276, -0.5808385047149626779 ) ) ;
#19887 = CARTESIAN_POINT ( 'NONE',  ( 6.454463653088309272, 6.866155873091829953, 0.6733577401037347254 ) ) ;
#19888 = CARTESIAN_POINT ( 'NONE',  ( 1.722021792205346902, -1.142311743720581196, -1.714993188781144928 ) ) ;
#19890 = LINE ( 'NONE', #201825, #193665 ) ;
#19889 = DIRECTION ( 'NONE',  ( 1.276756478318932585E-15, -1.000000000000000000, 1.665334536937738262E-16 ) ) ;
#19891 = CARTESIAN_POINT ( 'NONE',  ( -1.402160292154681736E-14, 1.696875000341421469, -1.575800808251659024 ) ) ;
#19892 = DIRECTION ( 'NONE',  ( 0.000000000000000000, 1.000000000000000000, 0.000000000000000000 ) ) ;
#19893 = ORIENTED_EDGE ( 'NONE', *, *, #141538, .F. ) ;
#19894 = CARTESIAN_POINT ( 'NONE',  ( 3.984940423737866055, -1.785409543757199291, -0.6854135386504257577 ) ) ;
#19895 = AXIS2_PLACEMENT_3D ( 'NONE', #25728, #175215, #123341 ) ;
#19896 = CARTESIAN_POINT ( 'NONE',  ( -3.475000000000000533, -1.079166666666665941, -2.006292185433948827 ) ) ;
#19897 = CARTESIAN_POINT ( 'NONE',  ( -3.090368948911150770, 5.692848642783215674, 1.199719254218462483 ) ) ;
#19898 = CARTESIAN_POINT ( 'NONE',  ( 0.8788404743438563704, -1.638286771785288254, -0.7734350870383081000 ) ) ;
#19900 = CARTESIAN_POINT ( 'NONE',  ( 1.252998012795783822, 0.1371590870133630458, -1.910833894730893601 ) ) ;
#19899 = CARTESIAN_POINT ( 'NONE',  ( 1.500000000000001110, 7.438721522839136568, -4.195160983902596286 ) ) ;
#19901 = CARTESIAN_POINT ( 'NONE',  ( 1.838419004579601834, -1.109345826794335688, 1.747895861591180156 ) ) ;
#19902 = CARTESIAN_POINT ( 'NONE',  ( -0.6823417656250246877, -0.1364583329919108468, 1.181850606188755259 ) ) ;
#19903 = AXIS2_PLACEMENT_3D ( 'NONE', #156088, #75893, #59638 ) ;
#19904 = CARTESIAN_POINT ( 'NONE',  ( 1.041797052332312568, 0.8010751512182741063, -1.801556251716707413 ) ) ;
#19905 = CARTESIAN_POINT ( 'NONE',  ( 5.426370213035293766, 1.145732239094964466, -1.548636736622555299 ) ) ;
#19907 = CARTESIAN_POINT ( 'NONE',  ( 6.486339200172205999, 6.751434215916642501, 0.1376000389162572446 ) ) ;
#19906 = CARTESIAN_POINT ( 'NONE',  ( 6.674453038267287752, -1.361800985140369402, 1.737325302230605883 ) ) ;
#19908 = CARTESIAN_POINT ( 'NONE',  ( -1.364683531250012516, 1.530208333674756505, 0.7879004041258379498 ) ) ;
#19909 = CARTESIAN_POINT ( 'NONE',  ( 4.193840287544727374, -1.420164769765386303, -1.496150262111215934 ) ) ;
#19910 = CARTESIAN_POINT ( 'NONE',  ( -4.889686956022917919, 8.856385215335397021, 1.214306433183764966E-14 ) ) ;
#19911 = CARTESIAN_POINT ( 'NONE',  ( 7.670162217029129259, 9.971608557999250166, 1.599625672291281386 ) ) ;
#19912 = CARTESIAN_POINT ( 'NONE',  ( -1.203941962966186052, 2.883481847795091202, 0.7750000000000083489 ) ) ;
#19913 = CARTESIAN_POINT ( 'NONE',  ( 4.157546660884947620, 8.002221537674429896, 1.040834085586084257E-14 ) ) ;
#19915 = CARTESIAN_POINT ( 'NONE',  ( -1.001543065824772872E-14, 4.212500000000023448, 1.732050807568877637 ) ) ;
#19914 = CARTESIAN_POINT ( 'NONE',  ( 5.297925755477892906, -0.7609016685872365127, 1.963875245004148562 ) ) ;
#19916 = CARTESIAN_POINT ( 'NONE',  ( 0.1335669894368500255, -0.0009366757763962055587, -2.153671288142432250 ) ) ;
#19917 = CARTESIAN_POINT ( 'NONE',  ( -1.364683531250014514, 1.551041667008084435, -0.7879004041258289570 ) ) ;
#19918 = CARTESIAN_POINT ( 'NONE',  ( 4.692742333269261934, -0.4685372120167423660, -2.110058259655919422 ) ) ;
#19919 = CARTESIAN_POINT ( 'NONE',  ( 4.371743357251212103, 0.4404049503993580639, -1.970906944672585315 ) ) ;
#19920 = SURFACE_STYLE_USAGE ( .BOTH. , #171516 ) ;
#19923 = CARTESIAN_POINT ( 'NONE',  ( 4.202664430556241726, 7.846932902383524144, 0.7216878364870298324 ) ) ;
#19922 = CARTESIAN_POINT ( 'NONE',  ( -3.285556943749998737, -3.230208332855375897, 1.896917185911908499 ) ) ;
#19921 = DIRECTION ( 'NONE',  ( 0.000000000000000000, 1.000000000000000000, 0.000000000000000000 ) ) ;
#19924 = CARTESIAN_POINT ( 'NONE',  ( -5.607179047703544583, 8.699403434699558346, 1.199719254218454489 ) ) ;
#19925 = CARTESIAN_POINT ( 'NONE',  ( 2.378138974734815392, -2.011451771401792321, -0.1435188914247695346 ) ) ;
#19926 = CARTESIAN_POINT ( 'NONE',  ( -8.341290820905609138, 10.75459192918846618, 1.599625672291269396 ) ) ;
#19927 = CARTESIAN_POINT ( 'NONE',  ( -2.903417451620861289, 6.539070793532962611, 0.7998128361456341429 ) ) ;
#19928 = CARTESIAN_POINT ( 'NONE',  ( -11.94980361490462784, 12.59667875264138992, -1.099999952232860512 ) ) ;
#19929 = CARTESIAN_POINT ( 'NONE',  ( 2.474997580123494245, 0.9706168436483512130, -11.64394813633530923 ) ) ;
#19930 = FACE_OUTER_BOUND ( 'NONE', #64730, .T. ) ;
#19931 = B_SPLINE_CURVE_WITH_KNOTS ( 'NONE', 3,
 ( #1366, #86916, #182265, #18697, #200637, #134633, #84779, #37088, #152984, #199577 ),
 .UNSPECIFIED., .F., .F.,
 ( 4, 2, 2, 2, 4 ),
 ( 0.000000000000000000, 0.0003729762227911204739, 0.0007459524455822409477, 0.001118928668373361367, 0.001491904891164481895 ),
 .UNSPECIFIED. ) ;
#19933 = CARTESIAN_POINT ( 'NONE',  ( 4.605092316430917876, -0.09611821078869468848, 2.014234682242924457 ) ) ;
#19932 = CARTESIAN_POINT ( 'NONE',  ( -7.497295758232731089, 8.809561808435409702, -1.082531754730543083 ) ) ;
#19934 = CARTESIAN_POINT ( 'NONE',  ( -0.7499999999999972244, 4.858333333333353821, -1.299038105676652011 ) ) ;
#19935 = CARTESIAN_POINT ( 'NONE',  ( 0.6973489402126078485, -0.6253137818992074992, 1.607738891190332753 ) ) ;
#19936 = CARTESIAN_POINT ( 'NONE',  ( 6.873057527484919937, 6.983264968346048818, 0.7998128361456352531 ) ) ;
#19938 = CARTESIAN_POINT ( 'NONE',  ( -0.4019237886466871523, 10.47991455036742714, -1.499999999999998668 ) ) ;
#19937 = CARTESIAN_POINT ( 'NONE',  ( 9.097157885089661278, 9.715698408800516717, 1.040834085586084257E-14 ) ) ;
#19939 = CYLINDRICAL_SURFACE ( 'NONE', #105935, 2.500000000000007994 ) ;
#19940 = CARTESIAN_POINT ( 'NONE',  ( 5.817618194842751222, -1.825074353437942554, 0.4092329068215995180 ) ) ;
#19941 = CARTESIAN_POINT ( 'NONE',  ( 0.2408851659233458842, 1.927091567462356547, 0.5821649069043339786 ) ) ;
#19942 = CARTESIAN_POINT ( 'NONE',  ( -4.248040861160308879, 3.981233870717535872, 0.4781583390340860551 ) ) ;
#19943 = CARTESIAN_POINT ( 'NONE',  ( -5.600926855776877211, 9.548515408466085930, -0.7216878364870338292 ) ) ;
#19944 = ORIENTED_EDGE ( 'NONE', *, *, #89552, .F. ) ;
#19945 = CARTESIAN_POINT ( 'NONE',  ( 0.7906389332529573100, 1.525030349845598820, -1.319245847334844735 ) ) ;
#19946 = CARTESIAN_POINT ( 'NONE',  ( 1.318313199092124188, -0.6538357601561273214, -1.689641652304620045 ) ) ;
#19947 = CARTESIAN_POINT ( 'NONE',  ( 7.635176783151273128, 8.936736330878529699, 1.199719254218452935 ) ) ;
#19948 = CARTESIAN_POINT ( 'NONE',  ( 6.332923096303629151, 0.2067577541180857514, 2.151790036905242953 ) ) ;
#19949 = EDGE_CURVE ( 'NONE', #132709, #147669, #154681, .T. ) ;
#19950 = PRODUCT_DEFINITION ( 'UNKNOWN', '', #194087, #197693 ) ;
#19951 = CARTESIAN_POINT ( 'NONE',  ( 9.070041577417981671, 9.684062716516882219, -0.7216878364870197293 ) ) ;
#19952 = CARTESIAN_POINT ( 'NONE',  ( 7.800018446563675489, 7.994443030612759848, -0.7998128361456281477 ) ) ;
#19954 = CARTESIAN_POINT ( 'NONE',  ( 0.7607752342545861524, -0.05021853532924521607, -1.915246365852550037 ) ) ;
#19953 = CARTESIAN_POINT ( 'NONE',  ( -5.739179097286464248, 5.590130456455974617, -0.7998128361456221525 ) ) ;
#19955 = DIRECTION ( 'NONE',  ( 0.7592566023653005702, 0.6507913734559639396, 0.000000000000000000 ) ) ;
#19956 = CARTESIAN_POINT ( 'NONE',  ( -15.75000000000000000, 10.19999999999999929, -3.200000000000001510 ) ) ;
#19957 = CARTESIAN_POINT ( 'NONE',  ( -1.364683531250014514, -0.6572916663252459379, 0.7879004041258379498 ) ) ;
#19959 = VERTEX_POINT ( 'NONE', #45373 ) ;
#19958 = CARTESIAN_POINT ( 'NONE',  ( 2.684151225825664788, 5.114964949229812596, -1.082531754730543083 ) ) ;
#19961 = CARTESIAN_POINT ( 'NONE',  ( -4.457933580795036654, 4.095344020549286590, -0.7998128361456221525 ) ) ;
#19960 = B_SPLINE_CURVE_WITH_KNOTS ( 'NONE', 3,
 ( #187798, #103363, #87107, #4751, #136943, #54610, #120758, #5826, #23150, #138009 ),
 .UNSPECIFIED., .F., .F.,
 ( 4, 2, 2, 2, 4 ),
 ( 0.000000000000000000, 0.0002598598948551708999, 0.0005197197897103416914, 0.0007795796845655125372, 0.001039439579420683383 ),
 .UNSPECIFIED. ) ;
#19962 = CARTESIAN_POINT ( 'NONE',  ( 3.643588467267334874, -1.635511012911139650, -1.413612897787956513 ) ) ;
#19963 = CARTESIAN_POINT ( 'NONE',  ( -5.261973015879593873, 8.192700047617899273, 1.082531754730549967 ) ) ;
#19964 = CARTESIAN_POINT ( 'NONE',  ( 5.397554552016212703, 8.350878506444006533, 1.082531754730547524 ) ) ;
#19965 = CARTESIAN_POINT ( 'NONE',  ( 0.5629301599625028407, 0.6213668382478373386, 2.027498709647377773 ) ) ;
#19966 = CARTESIAN_POINT ( 'NONE',  ( 0.000000000000000000, 2.999999999999999112, -2.420000000000000373 ) ) ;
#19967 = ADVANCED_FACE ( 'NONE', ( #123507 ), #92000, .F. ) ;
#19968 = CARTESIAN_POINT ( 'NONE',  ( 2.284392081957301812, -1.932574240873608629, -0.3883164474826616419 ) ) ;
#19969 = CARTESIAN_POINT ( 'NONE',  ( 5.080287894202283105, 0.9478536798121822704, 1.660923459347658282 ) ) ;
#19970 = EDGE_LOOP ( 'NONE', ( #174224, #38105, #87287 ) ) ;
#19971 = CARTESIAN_POINT ( 'NONE',  ( 0.000000000000000000, 7.999999999999992895, 0.000000000000000000 ) ) ;
#19972 = CARTESIAN_POINT ( 'NONE',  ( 5.810992205472774508, -1.553620646631387991, 1.210443464816546744 ) ) ;
#19973 = CARTESIAN_POINT ( 'NONE',  ( 0.4978614556471228081, -0.6533520819593687801, -1.828864621591755002 ) ) ;
#19974 = ORIENTED_EDGE ( 'NONE', *, *, #14937, .T. ) ;
#19975 = CARTESIAN_POINT ( 'NONE',  ( -5.957882158562513908, 5.915560371269843465, -0.7998128361456362523 ) ) ;
#19976 = CARTESIAN_POINT ( 'NONE',  ( -2.986538976760251263, 6.706322249520737522, -0.7998128361456481317 ) ) ;
#19978 = CARTESIAN_POINT ( 'NONE',  ( 6.495764994278809823, 6.751016379513001375, 0.7216878364870328300 ) ) ;
#19977 = CARTESIAN_POINT ( 'NONE',  ( 5.957918438201454059, 9.038323046955323292, -1.199719254218440723 ) ) ;
#19980 = VERTEX_POINT ( 'NONE', #43246 ) ;
#19979 = CARTESIAN_POINT ( 'NONE',  ( 5.514289750425454883, -1.912461473380810961, 0.004301308668797076962 ) ) ;
#19981 = CARTESIAN_POINT ( 'NONE',  ( 3.176612885197922953, -1.314426786483071208, 1.772596291930063961 ) ) ;
#19982 = CARTESIAN_POINT ( 'NONE',  ( 1.923171073188837843, 2.059116738528983692, 0.7940920450543451636 ) ) ;
#19983 = LINE ( 'NONE', #71924, #30603 ) ;
#19984 = CARTESIAN_POINT ( 'NONE',  ( 0.8207898099904624711, 1.447681275506585541, -1.249484660484905030 ) ) ;
#19985 = CARTESIAN_POINT ( 'NONE',  ( -9.800888885521233718, 4.518459255872631530, 6.931788714247765881 ) ) ;
#19986 = CARTESIAN_POINT ( 'NONE',  ( 10.99036836684473073, -7.696788179137236341, -0.4651914231089532836 ) ) ;
#19987 = CARTESIAN_POINT ( 'NONE',  ( 6.773846765307952822, -7.473374494058216300, -6.773846765307982132 ) ) ;
#19988 = CARTESIAN_POINT ( 'NONE',  ( 3.174344110969638866, -1.018096006688212096, -1.802650257252853772 ) ) ;
#19989 = CARTESIAN_POINT ( 'NONE',  ( -4.737684612971557740, 7.614716917520386374, 1.199719254218464037 ) ) ;
#19990 = CIRCLE ( 'NONE', #141130, 0.08000000000000020983 ) ;
#19991 = CARTESIAN_POINT ( 'NONE',  ( -4.604461168338175980, 8.383524640989071131, 0.06638267717353450725 ) ) ;
#19993 = CARTESIAN_POINT ( 'NONE',  ( 0.7433210806352362754, -1.853469564684958382, 1.112228649290482263 ) ) ;
#19992 = CARTESIAN_POINT ( 'NONE',  ( -3.255929445576174697, 6.950334786480840243, -0.7998128361456281477 ) ) ;
#19994 = CARTESIAN_POINT ( 'NONE',  ( 2.454835928891830221, -1.908367152989149718, -1.077367144120815023 ) ) ;
#19995 = CARTESIAN_POINT ( 'NONE',  ( 1.500000000000039524, 7.000000000000000000, 10.99818166789400742 ) ) ;
#19996 = SURFACE_STYLE_USAGE ( .BOTH. , #37325 ) ;
#19997 = CARTESIAN_POINT ( 'NONE',  ( 0.4019237886466814902, 12.82366454968462754, 1.499999999999999334 ) ) ;
#19998 = CARTESIAN_POINT ( 'NONE',  ( 0.6823417656249969321, 13.33854166700806942, -1.181850606188757036 ) ) ;
#19999 = CARTESIAN_POINT ( 'NONE',  ( -3.983063267364693960, 7.868933921892603323, -0.7998128361456481317 ) ) ;
#20000 = CARTESIAN_POINT ( 'NONE',  ( 6.486931489777390425, -1.733547045345487758, 0.05303144115107599060 ) ) ;
#20001 = CARTESIAN_POINT ( 'NONE',  ( -4.437596350374534815, 4.071617251725375475, -0.7998128361456221525 ) ) ;
#20002 = TOROIDAL_SURFACE ( 'NONE', #2828, 11.92000000000000171, 0.08000000000000000167 ) ;
#20003 = CARTESIAN_POINT ( 'NONE',  ( 4.012602964903419611, 0.7404812365185129419, 1.933494928807255375 ) ) ;
#20004 = CARTESIAN_POINT ( 'NONE',  ( 4.183301248788100501, 1.701634275673917784, 1.259637755991403374 ) ) ;
#20005 = CARTESIAN_POINT ( 'NONE',  ( 4.625302960556422427, 8.547937220624488575, 1.040834085586084257E-14 ) ) ;
#20006 = CARTESIAN_POINT ( 'NONE',  ( 1.364683531249990311, 5.113541667008084879, 0.7879004041258499402 ) ) ;
#20007 = CARTESIAN_POINT ( 'NONE',  ( 3.203910658309446990, 0.7132968404394635087, -1.835904812064126590 ) ) ;
#20008 = CARTESIAN_POINT ( 'NONE',  ( 0.5098338327763075606, -0.6861045072398126443, 1.785269576063217567 ) ) ;
#20009 = CARTESIAN_POINT ( 'NONE',  ( 4.752058238528302780, 0.8743775744927633209, 2.119134945200305431 ) ) ;
#20010 = CARTESIAN_POINT ( 'NONE',  ( 2.525780997283606499, -1.050937884436175418, -1.492673824175783093 ) ) ;
#20011 = CARTESIAN_POINT ( 'NONE',  ( 5.065906673361608270, 5.939254536123854677, -1.199719254218450271 ) ) ;
#20012 = CARTESIAN_POINT ( 'NONE',  ( 5.707619481228810798, 7.681975366232176583, -1.443375672974057666 ) ) ;
#20013 = CARTESIAN_POINT ( 'NONE',  ( -6.368579470117215813, 8.453095353268645695, 1.599625672291283607 ) ) ;
#20014 = CARTESIAN_POINT ( 'NONE',  ( 3.972906070543721579, -1.488974544083881746, 1.355118003239277336 ) ) ;
#20015 = CARTESIAN_POINT ( 'NONE',  ( 4.873855640358407904, -1.924671727690111966, 0.3787619532854279436 ) ) ;
#20016 = CARTESIAN_POINT ( 'NONE',  ( -8.182509401047415309, 9.505014708432145909, 1.199719254218462483 ) ) ;
#20017 = CARTESIAN_POINT ( 'NONE',  ( -6.410307701162927252, 6.373113827645189744, -0.7998128361456291469 ) ) ;
#20018 = CARTESIAN_POINT ( 'NONE',  ( 0.1751657365761547513, 0.002452341591364578209, -2.044164811867712483 ) ) ;
#20020 = CARTESIAN_POINT ( 'NONE',  ( 6.244957947127046438, -1.492741346086885024, 0.9504933407481640506 ) ) ;
#20019 = CARTESIAN_POINT ( 'NONE',  ( 6.714806893291140888, -0.1599574331335733013, 2.055667697375664016 ) ) ;
#20021 = CARTESIAN_POINT ( 'NONE',  ( 10.96107445065239538, -5.401429653175719103, -0.1376292675369649998 ) ) ;
#20022 = CARTESIAN_POINT ( 'NONE',  ( 1.377182423176852133, 2.023737929115625445, -0.8412682346608522099 ) ) ;
#20023 = CARTESIAN_POINT ( 'NONE',  ( 0.1162408695623952659, -0.08860816971513819917, 1.738289989025374016 ) ) ;
#20024 = CARTESIAN_POINT ( 'NONE',  ( 6.076025397218672630, 10.24044673006381245, -0.7998128361456291469 ) ) ;
#20025 = CARTESIAN_POINT ( 'NONE',  ( 0.2335667940002684184, 0.001055507091213009818, -2.153566573614831281 ) ) ;
#20026 = CARTESIAN_POINT ( 'NONE',  ( 0.8380132626705768528, 1.698558605200460869, 0.2991625477344951323 ) ) ;
#20027 = CARTESIAN_POINT ( 'NONE',  ( 0.4569821463788895644, 1.705326812283548765, 1.541052590308614745 ) ) ;
#20028 = CARTESIAN_POINT ( 'NONE',  ( 0.8904706703079521279, -0.5376514911656914419, -2.124458794526106864 ) ) ;
#20029 = CARTESIAN_POINT ( 'NONE',  ( 6.432912826982137844, 0.8947389043411910770, 1.484938929457087164 ) ) ;
#20030 = CARTESIAN_POINT ( 'NONE',  ( 3.071135375186518690, -2.039199700013223815, -0.8442704067812344393 ) ) ;
#20031 =( NAMED_UNIT ( * ) SI_UNIT ( $, .STERADIAN. ) SOLID_ANGLE_UNIT ( ) );
#20032 = VECTOR ( 'NONE', #62486, 1000.000000000000114 ) ;
#20033 = CARTESIAN_POINT ( 'NONE',  ( 0.5499837882529658994, 1.607816289776839991, 1.459057700483844311 ) ) ;
#20034 = DIRECTION ( 'NONE',  ( 0.000000000000000000, 0.000000000000000000, 1.000000000000000000 ) ) ;
#20035 = CARTESIAN_POINT ( 'NONE',  ( 0.9720387486300664515, -0.9465246498777776241, 1.894042457640370491 ) ) ;
#20036 = CARTESIAN_POINT ( 'NONE',  ( 6.620655732516649294, 2.950034989283246478, 2.626075342966327497 ) ) ;
#20037 = CARTESIAN_POINT ( 'NONE',  ( 5.719733624436385000, -1.879402930333987198, 0.4222299131634628111 ) ) ;
#20038 = ORIENTED_EDGE ( 'NONE', *, *, #154690, .F. ) ;
#20040 = CARTESIAN_POINT ( 'NONE',  ( -0.6823417656250246877, -0.8864583329919115684, 1.181850606188755259 ) ) ;
#20039 = CARTESIAN_POINT ( 'NONE',  ( 1.470720204089857930, -2.178542539925924171, -0.7136519110988813752 ) ) ;
#20041 = CARTESIAN_POINT ( 'NONE',  ( 2.686486993802192913, 6.285985259411197568, 0.7998128361456362523 ) ) ;
#20042 = CARTESIAN_POINT ( 'NONE',  ( 4.957477724091233995, 8.935474444748447098, -0.7998128361456281477 ) ) ;
#20043 = CARTESIAN_POINT ( 'NONE',  ( 3.651236063859903069, 0.3270389233705518484, 2.196992388787385231 ) ) ;
#20044 = CARTESIAN_POINT ( 'NONE',  ( -8.703971430293361067, 9.256980878204810637, 0.7216878364870438212 ) ) ;
#20045 = DIRECTION ( 'NONE',  ( 0.000000000000000000, 1.000000000000000000, 0.000000000000000000 ) ) ;
#20046 = CARTESIAN_POINT ( 'NONE',  ( 6.480434237652135998, 6.662854153456708950, 0.7216878364870317197 ) ) ;
#20047 = CARTESIAN_POINT ( 'NONE',  ( -6.670248387799091461, 10.72578085250020585, 0.000000000000000000 ) ) ;
#20048 = CARTESIAN_POINT ( 'NONE',  ( 5.722950238744200391, 7.770137593325314285, 1.443375672974065660 ) ) ;
#20049 = CARTESIAN_POINT ( 'NONE',  ( 2.233046271152541618, 2.016033844848092560, 0.04667593304989729741 ) ) ;
#20051 = CARTESIAN_POINT ( 'NONE',  ( 1.551709131853472368, 1.559248165652558082, 1.350213067335771511 ) ) ;
#20050 = CARTESIAN_POINT ( 'NONE',  ( 6.726816770674637347, 10.99970333242910669, -0.7998128361456291469 ) ) ;
#20052 = CARTESIAN_POINT ( 'NONE',  ( 6.983858524370782916, 7.320458831286981827, 0.7216878364870328300 ) ) ;
#20053 = CARTESIAN_POINT ( 'NONE',  ( 0.01093749962182561514, -1.805946196879631094, 0.3578947576599255664 ) ) ;
#20054 = DIRECTION ( 'NONE',  ( 0.000000000000000000, 7.228014483236694583E-17, -1.000000000000000000 ) ) ;
#20055 = CARTESIAN_POINT ( 'NONE',  ( -1.402160292154681736E-14, 1.946875000341422579, -1.575800808251660134 ) ) ;
#20056 = CARTESIAN_POINT ( 'NONE',  ( 1.723279953462612202, 1.994870059565261755, 0.2930690452552578429 ) ) ;
#20057 = CARTESIAN_POINT ( 'NONE',  ( -0.02423404108400224743, -1.785672699080865788, -0.4486397487279417118 ) ) ;
#20058 = CARTESIAN_POINT ( 'NONE',  ( 5.021132725759672510, -2.177342503763429082, 0.7171727232720275236 ) ) ;
#20059 = CARTESIAN_POINT ( 'NONE',  ( 3.556447125109524876, -1.624355972047783148, -0.8667379164201680641 ) ) ;
#20060 = CARTESIAN_POINT ( 'NONE',  ( 8.446893396513862839, 9.813462703143045474, -1.199719254218445830 ) ) ;
#20061 =( LENGTH_UNIT ( ) NAMED_UNIT ( * ) SI_UNIT ( .MILLI., .METRE. ) );
#20062 = CARTESIAN_POINT ( 'NONE',  ( 4.313378725478684395, -0.3118687524542098632, 1.798583714455632476 ) ) ;
#20063 = CARTESIAN_POINT ( 'NONE',  ( 4.852185490356213826, 0.1948433276699329531, -2.006959737079899497 ) ) ;
#20064 = CARTESIAN_POINT ( 'NONE',  ( -8.528242318195895066, 9.908369778438709474, 1.199719254218462483 ) ) ;
#20066 = CARTESIAN_POINT ( 'NONE',  ( -7.014364370223741929, 9.276787413384745662, -1.599625672291271394 ) ) ;
#20065 = CARTESIAN_POINT ( 'NONE',  ( 3.854571047428239527, 0.8115417623771915556, 2.112135835510853710 ) ) ;
#20067 = CARTESIAN_POINT ( 'NONE',  ( 6.071333362910682041, 0.1583771919418910934, -2.100070647415654079 ) ) ;
#20068 = CARTESIAN_POINT ( 'NONE',  ( -1.001543065824772872E-14, 4.243750000682819490, 1.732050807568877637 ) ) ;
#20069 = CARTESIAN_POINT ( 'NONE',  ( 3.648938843998358106, -0.4010542052625790110, -2.030977206718207473 ) ) ;
#20070 = CARTESIAN_POINT ( 'NONE',  ( 2.544126380858701797, 6.119897877643793116, 0.7998128361456462443 ) ) ;
#20071 = CARTESIAN_POINT ( 'NONE',  ( -0.6801582343750403048, 2.463541667008038782, 1.178068619123829430 ) ) ;
#20072 = APPLICATION_PROTOCOL_DEFINITION ( 'draft international standard', 'automotive_design', 1998, #122578 ) ;
#20075 = EDGE_CURVE ( 'NONE', #204725, #33202, #10707, .T. ) ;
#20074 = CARTESIAN_POINT ( 'NONE',  ( 1.734862838405337060, 0.1885825406544305305, 1.917253122483292715 ) ) ;
#20073 = CARTESIAN_POINT ( 'NONE',  ( -8.208571938070008400, 11.66408546346865016, -1.199719254218446718 ) ) ;
#20076 = CARTESIAN_POINT ( 'NONE',  ( -2.844178363816758814, 6.540234867753325076, -0.7998128361456481317 ) ) ;
#20077 = CARTESIAN_POINT ( 'NONE',  ( 0.3441184698094986727, -0.9315698024882634876, 1.735327799219071210 ) ) ;
#20078 = CARTESIAN_POINT ( 'NONE',  ( 5.207740400980577888, 5.248321020665011716, 0.000000000000000000 ) ) ;
#20079 = CARTESIAN_POINT ( 'NONE',  ( 5.841717777309253457, 6.007722996832359996, 0.3783690319567531435 ) ) ;
#20080 = CARTESIAN_POINT ( 'NONE',  ( 10.44245235073003286, 1.000000000000000888, -5.695529491621821983 ) ) ;
#20081 = AXIS2_PLACEMENT_3D ( 'NONE', #49852, #150567, #181967 ) ;
#20082 = CARTESIAN_POINT ( 'NONE',  ( -3.307299406729781399, 5.945934176904983381, -1.199719254218452935 ) ) ;
#20083 = CARTESIAN_POINT ( 'NONE',  ( 2.039591900818237491, 0.005460781979979567602, 2.221583674558536892 ) ) ;
#20084 = CARTESIAN_POINT ( 'NONE',  ( 3.610471823009605341, -0.8516972358460070947, -1.926234778997274244 ) ) ;
#20085 = CARTESIAN_POINT ( 'NONE',  ( -6.400331034103001748, 9.624747418832267698, 1.199719254218452935 ) ) ;
#20086 = CARTESIAN_POINT ( 'NONE',  ( 8.288111976655649471, 8.563885482386732306, -0.7998128361456291469 ) ) ;
#20087 = CARTESIAN_POINT ( 'NONE',  ( 0.5900176457281476328, 0.9615612750370464701, -1.593262740414502776 ) ) ;
#20088 = CARTESIAN_POINT ( 'NONE',  ( 6.449928391799196525, 8.548002428564306143, -1.599625672291262513 ) ) ;
#20089 =( BOUNDED_SURFACE ( )  B_SPLINE_SURFACE ( 3, 2, ( 
 ( #135548, #100893, #50021 ),
 ( #53218, #103040, #55352 ),
 ( #138750, #58549, #7645 ),
 ( #153927, #204768, #203705 ) ),
 .UNSPECIFIED., .F., .F., .T. ) 
 B_SPLINE_SURFACE_WITH_KNOTS ( ( 4, 4 ),
 ( 3, 3 ),
 ( 0.0002736160683302337414, 0.001000278046670503461 ),
 ( 0.000000000000000000, 1.000000000000000000 ),
 .UNSPECIFIED. ) 
 GEOMETRIC_REPRESENTATION_ITEM ( )  RATIONAL_B_SPLINE_SURFACE ( (
 ( 1.000000000000000000, 0.6273451206645834777, 1.000000000000000000),
 ( 1.000000000000000000, 0.6198151287834121614, 1.000000000000000000),
 ( 1.000000000000000000, 0.6183718462547956873, 1.000000000000000000),
 ( 1.000000000000000000, 0.6222643257228424041, 1.000000000000000000) ) ) 
 REPRESENTATION_ITEM ( '' )  SURFACE ( )  );
#20090 = CARTESIAN_POINT ( 'NONE',  ( 5.522248639467795428, 5.337044922334209573, -0.7998128361456231517 ) ) ;
#20091 = CARTESIAN_POINT ( 'NONE',  ( -6.631346530859867805, 6.909194838857525944, 0.000000000000000000 ) ) ;
#20092 = CARTESIAN_POINT ( 'NONE',  ( -8.690413276679693766, 9.241163032322203819, 1.040834085586084257E-14 ) ) ;
#20093 = CARTESIAN_POINT ( 'NONE',  ( 1.670341986359990205, 2.114562342887704283, -0.1611296783964668855 ) ) ;
#20094 = CARTESIAN_POINT ( 'NONE',  ( -5.427006627220116286, 9.553534508390610469, -0.7998128361456362523 ) ) ;
#20096 = CARTESIAN_POINT ( 'NONE',  ( 4.281663391851794565, -1.878042059144067633, 0.5673916069991248312 ) ) ;
#20095 = CARTESIAN_POINT ( 'NONE',  ( 1.224999999999967004, 0.3958333333333378667, -0.7072540797573018123 ) ) ;
#20097 = CARTESIAN_POINT ( 'NONE',  ( 3.116266767097406909, -1.064116542966097922, -1.881565754655416756 ) ) ;
#20098 = CARTESIAN_POINT ( 'NONE',  ( 1.997363575765517485, -1.840834563946552649, 0.04656924640939615057 ) ) ;
#20099 = CARTESIAN_POINT ( 'NONE',  ( -4.362038794589177648, 7.192753374110822051, -1.033456106840037192 ) ) ;
#20100 = CARTESIAN_POINT ( 'NONE',  ( 5.138483783005516337, -1.490010379379594241, 0.8989716238894971401 ) ) ;
#20102 = CONICAL_SURFACE ( 'NONE', #103153, 3.999999999999998224, 0.8621700546672330656 ) ;
#20101 = CARTESIAN_POINT ( 'NONE',  ( -3.501245407923692099, 15.00000000000335731, -11.28115623562607794 ) ) ;
#20103 = CARTESIAN_POINT ( 'NONE',  ( 4.338245966692901412, 8.005111361209628740, -0.7216878364870197293 ) ) ;
#20104 = CARTESIAN_POINT ( 'NONE',  ( -10.01587959479698320, 5.734125918284786572, -5.906598880481439551 ) ) ;
#20105 = CARTESIAN_POINT ( 'NONE',  ( 2.342841879718413622, 0.4729757327756216601, 2.109170662781891359 ) ) ;
#20106 = CARTESIAN_POINT ( 'NONE',  ( 3.778672575519220977, -1.986742196792599335, 0.3418835855632795795 ) ) ;
#20107 = CARTESIAN_POINT ( 'NONE',  ( -9.531018800282611281, 12.14260790512831889, 1.443375672974076540 ) ) ;
#20108 = CARTESIAN_POINT ( 'NONE',  ( 1.376082401959723089, 1.288024388040419632, 1.735935173841046675 ) ) ;
#20109 = EDGE_CURVE ( 'NONE', #53056, #32144, #109365, .T. ) ;
#20110 = CARTESIAN_POINT ( 'NONE',  ( 3.889495165534775811, 1.427134975246695969, 1.360358076685687978 ) ) ;
#20111 = CARTESIAN_POINT ( 'NONE',  ( 6.609000000000047947, 7.629137130509099585, 2.499999999999994227 ) ) ;
#20112 = CARTESIAN_POINT ( 'NONE',  ( 3.579573000355208645, -0.9547435552521261748, 1.691086383587044883 ) ) ;
#20115 = VERTEX_POINT ( 'NONE', #174316 ) ;
#20114 = CARTESIAN_POINT ( 'NONE',  ( -3.350273356352693188, 6.922752992471175482, 0.000000000000000000 ) ) ;
#20113 = CARTESIAN_POINT ( 'NONE',  ( -8.297226821439000588, 12.62392235841345389, 1.040834085586084257E-14 ) ) ;
#20116 = CARTESIAN_POINT ( 'NONE',  ( -4.787437638956939523, 5.718337012605431369, -1.082531754730549967 ) ) ;
#20117 = CARTESIAN_POINT ( 'NONE',  ( -0.1108833634137010304, 0.2458664895051872190, -1.931623620491630611 ) ) ;
#20118 = CARTESIAN_POINT ( 'NONE',  ( 3.576318658954677598, 7.394398545414291313, 0.7998128361456281477 ) ) ;
#20119 = CARTESIAN_POINT ( 'NONE',  ( -5.503684012504701961, 5.385662534202396934, 0.000000000000000000 ) ) ;
#20120 = CARTESIAN_POINT ( 'NONE',  ( -6.257970421159510188, 9.458660037064859694, 1.199719254218452047 ) ) ;
#20121 = CARTESIAN_POINT ( 'NONE',  ( -8.310784975052669665, 12.63974020429606249, -0.7216878364870267237 ) ) ;
#20122 = CARTESIAN_POINT ( 'NONE',  ( 0.08333923026508995024, -0.1592477204843331384, -2.171661519566956855 ) ) ;
#20123 = CARTESIAN_POINT ( 'NONE',  ( 3.285556943750000514, -3.113541666188709645, 1.896917185911906500 ) ) ;
#20124 = CARTESIAN_POINT ( 'NONE',  ( 3.871884822249270108, -1.933460040528666379, 0.3310023857948928838 ) ) ;
#20125 = CARTESIAN_POINT ( 'NONE',  ( 6.909851844459134362, 11.21324425184434936, -0.7998128361456291469 ) ) ;
#20126 = CARTESIAN_POINT ( 'NONE',  ( 1.986954140179174155, -2.015912935764123670, 0.05229865529512293942 ) ) ;
#20127 = ORIENTED_EDGE ( 'NONE', *, *, #55681, .T. ) ;
#20128 = CARTESIAN_POINT ( 'NONE',  ( 3.116528361068672481, 2.066776279341679956, 0.4593686614828630943 ) ) ;
#20129 = CARTESIAN_POINT ( 'NONE',  ( 0.7499999999999885647, 1.097916667349485564, -1.299038105676652899 ) ) ;
#20131 = CARTESIAN_POINT ( 'NONE',  ( -4.381256195510448315, 8.263215994737505454, 1.040834085586084257E-14 ) ) ;
#20130 = LINE ( 'NONE', #22248, #118175 ) ;
#20132 = CARTESIAN_POINT ( 'NONE',  ( 3.257574473681293270, 0.8286728953739975756, 1.644182576024610265 ) ) ;
#20133 = ORIENTED_EDGE ( 'NONE', *, *, #117402, .T. ) ;
#20134 = CARTESIAN_POINT ( 'NONE',  ( -7.458957065812611198, 11.85386701009007204, 0.7998128361456481317 ) ) ;
#20135 = CARTESIAN_POINT ( 'NONE',  ( -5.260200412422217475, 5.239248024021766703, -0.7216878364870237261 ) ) ;
#20136 = CARTESIAN_POINT ( 'NONE',  ( 4.605793411009856619, 1.573235607984494688, 1.422142093439874522 ) ) ;
#20137 = FACE_OUTER_BOUND ( 'NONE', #45275, .T. ) ;
#20138 = CARTESIAN_POINT ( 'NONE',  ( 5.425234023762710578, 9.481190127698507553, -0.7998128361456291469 ) ) ;
#20139 = CARTESIAN_POINT ( 'NONE',  ( 5.237599208242285087, -1.454345255708370255, -1.460303020606460445 ) ) ;
#20141 = CARTESIAN_POINT ( 'NONE',  ( 2.929072846782492245, -1.238530643895646488, -1.362589426554157157 ) ) ;
#20140 = CARTESIAN_POINT ( 'NONE',  ( -5.377780486114890124, 9.425827667109372143, 0.000000000000000000 ) ) ;
#20142 = CARTESIAN_POINT ( 'NONE',  ( 7.736899214892750010, 12.17813285068358020, 1.040834085586084257E-14 ) ) ;
#20143 = SURFACE_STYLE_USAGE ( .BOTH. , #104628 ) ;
#20144 = FILL_AREA_STYLE ('',( #168548 ) ) ;
#20145 = CARTESIAN_POINT ( 'NONE',  ( 10.96075698767266893, -7.841077028191733689, -0.3746540212967842121 ) ) ;
#20146 =( BOUNDED_SURFACE ( )  B_SPLINE_SURFACE ( 3, 3, ( 
 ( #51132, #46081, #66274, #82551, #34856, #3415, #2341, #16471, #210683, #204, #164876 ),
 ( #112200, #99883, #53259, #144670, #135589, #134545, #119389, #169136, #52196, #185377, #118322 ),
 ( #62312, #194439, #83618, #178207, #184308, #35932, #102010, #116190, #69481, #36997, #29823 ),
 ( #165945, #149700, #148638, #168080, #198423, #50067, #98827, #1281, #67339, #133484, #19678 ),
 ( #85758, #23940, #106327, #38081, #107410, #170201, #121546, #172350, #6616, #190707, #140950 ),
 ( #73771, #90044, #156102, #7688, #58592, #87894, #205898, #57532, #203746, #72696, #153967 ),
 ( #138791, #187517, #204811, #123689, #139867, #189651, #41302, #155031, #124747, #42368, #56462 ) ),
 .UNSPECIFIED., .T., .F., .T. ) 
 B_SPLINE_SURFACE_WITH_KNOTS ( ( 4, 3, 4 ),
 ( 4, 1, 1, 1, 1, 1, 1, 1, 4 ),
 ( 0.000000000000000000, 0.5000000000000000000, 1.000000000000000000 ),
 ( 0.000000000000000000, 0.2256777920876190668, 0.3978457394851813711, 0.5256768607792676740, 0.6183602023682204241, 0.6850295134299612121, 0.7345374503969632762, 0.7752450576501028756, 1.000000000000000000 ),
 .UNSPECIFIED. ) 
 GEOMETRIC_REPRESENTATION_ITEM ( )  RATIONAL_B_SPLINE_SURFACE ( (
 ( 1.000000000000000000, 1.000000000000000000, 1.000000000000000000, 1.000000000000000222, 0.9999999999999997780, 1.000000000000000444, 0.9999999999999997780, 1.000000000000000222, 0.9999999999999996669, 1.000000000000000222, 1.000000000000000222),
 ( 0.3333333333333333703, 0.3333333333333334259, 0.3333333333333333703, 0.3333333333333334259, 0.3333333333333333703, 0.3333333333333334259, 0.3333333333333333703, 0.3333333333333334259, 0.3333333333333333148, 0.3333333333333334259, 0.3333333333333334259),
 ( 0.3333333333333333703, 0.3333333333333334259, 0.3333333333333333703, 0.3333333333333334259, 0.3333333333333333703, 0.3333333333333334259, 0.3333333333333333703, 0.3333333333333334259, 0.3333333333333333148, 0.3333333333333334259, 0.3333333333333334259),
 ( 1.000000000000000000, 1.000000000000000000, 1.000000000000000000, 1.000000000000000222, 0.9999999999999997780, 1.000000000000000444, 0.9999999999999997780, 1.000000000000000222, 0.9999999999999996669, 1.000000000000000222, 1.000000000000000222),
 ( 0.3333333333333333703, 0.3333333333333334259, 0.3333333333333333703, 0.3333333333333334259, 0.3333333333333333703, 0.3333333333333334259, 0.3333333333333333703, 0.3333333333333334259, 0.3333333333333333148, 0.3333333333333334259, 0.3333333333333334259),
 ( 0.3333333333333333703, 0.3333333333333334259, 0.3333333333333333703, 0.3333333333333334259, 0.3333333333333333703, 0.3333333333333334259, 0.3333333333333333703, 0.3333333333333334259, 0.3333333333333333148, 0.3333333333333334259, 0.3333333333333334259),
 ( 1.000000000000000000, 1.000000000000000000, 1.000000000000000000, 1.000000000000000222, 0.9999999999999997780, 1.000000000000000444, 0.9999999999999997780, 1.000000000000000222, 0.9999999999999996669, 1.000000000000000222, 1.000000000000000222) ) ) 
 REPRESENTATION_ITEM ( '' )  SURFACE ( )  );
#20147 = VECTOR ( 'NONE', #91990, 1000.000000000000227 ) ;
#20148 = CARTESIAN_POINT ( 'NONE',  ( 2.684424123961434816, -1.133677649706768431, 1.893296980138805097 ) ) ;
#20149 = CARTESIAN_POINT ( 'NONE',  ( 4.763087504681410955, -2.017952330160921015, -1.023110994099560411 ) ) ;
#20150 = CARTESIAN_POINT ( 'NONE',  ( -6.670248388243482651, 9.765411638717282017, 1.082531754730548412 ) ) ;
#20151 = CARTESIAN_POINT ( 'NONE',  ( 4.412255891540381114, -1.811360455869342578, -0.03765339742955660374 ) ) ;
#20152 = CARTESIAN_POINT ( 'NONE',  ( 3.907376549751972572, -1.831493090834277249, 0.5616838290606884776 ) ) ;
#20153 = CARTESIAN_POINT ( 'NONE',  ( -0.6823417656249969321, 4.280208333674755394, -1.181850606188749264 ) ) ;
#20154 = CARTESIAN_POINT ( 'NONE',  ( 3.942224353883512222, 1.961846943226858597, 0.1946112770482635312 ) ) ;
#20155 = CARTESIAN_POINT ( 'NONE',  ( 5.295714669793899709, -0.6724083694377264164, 1.745798414713333413 ) ) ;
#20156 = CARTESIAN_POINT ( 'NONE',  ( 4.914427440023315441, 0.7117315627661743305, 1.719784830429422984 ) ) ;
#20157 = CARTESIAN_POINT ( 'NONE',  ( -0.6823417656249969321, 5.217708333674756283, -1.181850606188749264 ) ) ;
#20158 = CARTESIAN_POINT ( 'NONE',  ( -0.1531117392989979065, -1.803405091603600185, -0.9023890051431044945 ) ) ;
#20160 = CARTESIAN_POINT ( 'NONE',  ( 2.121831256377606501, -2.042539606455844758, 0.5128510974094899755 ) ) ;
#20159 = CARTESIAN_POINT ( 'NONE',  ( -9.642873567817536795, 12.27310513391906532, 1.599625672291281386 ) ) ;
#20161 = CARTESIAN_POINT ( 'NONE',  ( 4.189106276498237413, 3.989638198777126110, -0.7216878364870188411 ) ) ;
#20163 = CARTESIAN_POINT ( 'NONE',  ( 0.07479286986305289098, 7.629137130509083597, -2.455503679634088776 ) ) ;
#20162 = CARTESIAN_POINT ( 'NONE',  ( -0.6823417656250212460, 4.863541667008086655, 1.181850606188767472 ) ) ;
#20164 = CARTESIAN_POINT ( 'NONE',  ( 2.988655875014298857, -1.259908772670719657, 1.705623289672608678 ) ) ;
#20165 = DIRECTION ( 'NONE',  ( 0.7592566023653016805, -0.6507913734559627184, 0.000000000000000000 ) ) ;
#20166 = CARTESIAN_POINT ( 'NONE',  ( 1.494405286683021306, -1.076835855708496936, 1.708581493997686662 ) ) ;
#20167 = CARTESIAN_POINT ( 'NONE',  ( -1.364683531250014514, 1.488541667008084435, -0.7879004041258289570 ) ) ;
#20168 = CARTESIAN_POINT ( 'NONE',  ( -4.121315508874276112, 4.870918184183829602, -1.082531754730549967 ) ) ;
#20169 = CARTESIAN_POINT ( 'NONE',  ( 5.657830175604453338, 5.495223381160312393, 0.7998128361456341429 ) ) ;
#20170 = ORIENTED_EDGE ( 'NONE', *, *, #140961, .T. ) ;
#20171 = CARTESIAN_POINT ( 'NONE',  ( 2.231903258980330484, -1.410129017595105561, -1.638413920015222125 ) ) ;
#20172 = DIRECTION ( 'NONE',  ( 5.176899690512889973E-31, -0.6000000000000035305, 0.7999999999999974909 ) ) ;
#20175 = CARTESIAN_POINT ( 'NONE',  ( 4.229780737783593203, 4.037091736943370535, -0.7216878364870188411 ) ) ;
#20174 = CARTESIAN_POINT ( 'NONE',  ( -3.600749563572677836, 3.160087278256992427, -2.499999999999995115 ) ) ;
#20173 = CARTESIAN_POINT ( 'NONE',  ( 4.869313445963426190, 5.709895770826003414, 1.199719254218452935 ) ) ;
#20176 = CARTESIAN_POINT ( 'NONE',  ( 10.53432216769390095, 11.39239007183880581, -0.7216878364870257245 ) ) ;
#20177 = CARTESIAN_POINT ( 'NONE',  ( -7.788485247867485306, -6.306978362809775085, 7.768428355091874238 ) ) ;
#20178 = CARTESIAN_POINT ( 'NONE',  ( -8.568389894156720032, 10.05917163368005163, 1.082531754730558626 ) ) ;
#20179 = CARTESIAN_POINT ( 'NONE',  ( 6.585487052573138378, -0.8941505307449393314, 1.888277625537030380 ) ) ;
#20180 = CARTESIAN_POINT ( 'NONE',  ( 4.559605246071184226, 3.300000000000025135, 0.7750000000000135669 ) ) ;
#20182 = CARTESIAN_POINT ( 'NONE',  ( 1.364683531250000748, 11.50520833367472839, -0.7879004041258355073 ) ) ;
#20181 = CARTESIAN_POINT ( 'NONE',  ( 1.305971919559431704, -0.5478059591418303897, 2.195072679011981442 ) ) ;
#20183 = CARTESIAN_POINT ( 'NONE',  ( -9.481229494658258261, 9.955855920056455588, -0.7998128361456291469 ) ) ;
#20184 = CARTESIAN_POINT ( 'NONE',  ( -3.402733366905605905, 6.913679994791092298, 0.7216878364870317197 ) ) ;
#20185 = CARTESIAN_POINT ( 'NONE',  ( -1.201851678989727383E-14, 1.884375000341422135, 1.575800808251672791 ) ) ;
#20186 = CARTESIAN_POINT ( 'NONE',  ( 4.735857411151594754, 8.202189375375613878, -0.7076125000919450958 ) ) ;
#20187 = CARTESIAN_POINT ( 'NONE',  ( 1.499999999999993117, 9.104166666666666075, 0.8660254037844409281 ) ) ;
#20188 = CARTESIAN_POINT ( 'NONE',  ( 4.213312296666638979, -0.2916954692788272796, 1.699858598931931919 ) ) ;
#20189 = CARTESIAN_POINT ( 'NONE',  ( 4.634908411025333130, 6.500755460986618495, 1.599625672291268286 ) ) ;
#20190 = CARTESIAN_POINT ( 'NONE',  ( 2.213771126746429729, -0.8293587345859743110, -1.563345763006577238 ) ) ;
#20191 = B_SPLINE_CURVE_WITH_KNOTS ( 'NONE', 3,
 ( #43180, #141763, #209891, #157991, #90858, #159037, #189400, #76705, #191515, #110355, #106075 ),
 .UNSPECIFIED., .F., .F.,
 ( 4, 1, 1, 1, 1, 1, 1, 1, 4 ),
 ( 0.000000000000000000, 0.2256337125576066971, 0.3978389261578171299, 0.5257960283851228489, 0.6187025735204009225, 0.6856790771877526725, 0.7354782194756434022, 0.7762620033627533056, 0.9999999999999998890 ),
 .UNSPECIFIED. ) ;
#20192 = CARTESIAN_POINT ( 'NONE',  ( 2.736979112881072762, 1.896321534115693819, 0.6760404272549996874 ) ) ;
#20193 = CARTESIAN_POINT ( 'NONE',  ( 4.964015014492747291, 2.183396446337606989, -0.3195234977587738667 ) ) ;
#20194 = ORIENTED_EDGE ( 'NONE', *, *, #121776, .F. ) ;
#20195 = CARTESIAN_POINT ( 'NONE',  ( 3.972919405334675691, -1.493746422221740699, 1.359666112553897355 ) ) ;
#20196 = CARTESIAN_POINT ( 'NONE',  ( -5.399890319992785237, 9.521898816625391504, 0.7998128361456291469 ) ) ;
#20197 = CARTESIAN_POINT ( 'NONE',  ( 4.429314653828757109, -1.560513098751922900, -1.277029310785951388 ) ) ;
#20199 = ORIENTED_EDGE ( 'NONE', *, *, #58752, .T. ) ;
#20198 = CARTESIAN_POINT ( 'NONE',  ( 4.517698195727691157, -0.4766141805869225645, 1.747713001785702325 ) ) ;
#20200 = PRESENTATION_LAYER_ASSIGNMENT (  '', '', ( #213917 ) ) ;
#20201 = ORIENTED_EDGE ( 'NONE', *, *, #190484, .F. ) ;
#20202 = EDGE_CURVE ( 'NONE', #153466, #93052, #113307, .T. ) ;
#20203 = CARTESIAN_POINT ( 'NONE',  ( 2.307302758404996545, -0.4121581357655336730, 1.824517092411604757 ) ) ;
#20204 = CARTESIAN_POINT ( 'NONE',  ( -7.334597915313094241, 9.580116872663850813, 1.040834085586084257E-14 ) ) ;
#20205 = CARTESIAN_POINT ( 'NONE',  ( 2.232540727315056373, 1.246330492051262784, -1.450604739030990187 ) ) ;
#20206 = CARTESIAN_POINT ( 'NONE',  ( -1.115562610750309283E-14, 9.562500000000000000, 1.500000000000001554 ) ) ;
#20207 = CARTESIAN_POINT ( 'NONE',  ( -10.97260011637327182, 3.256560822415822454, -6.404599650317903681 ) ) ;
#20208 = CARTESIAN_POINT ( 'NONE',  ( 4.041739190205284160, 7.729463131965888856, 0.000000000000000000 ) ) ;
#20209 = CARTESIAN_POINT ( 'NONE',  ( -0.6823417656250212460, 3.363541667008085323, 1.181850606188767472 ) ) ;
#20210 = CARTESIAN_POINT ( 'NONE',  ( 0.1055216070770526038, 1.418477292093557329, 1.282857148695019989 ) ) ;
#20211 = CARTESIAN_POINT ( 'NONE',  ( 5.478903473698239601, 7.485416367438324059, -1.443375672974078761 ) ) ;
#20212 = CARTESIAN_POINT ( 'NONE',  ( 1.416376618315864144, 0.7919773292732554815, 1.795081228748253377 ) ) ;
#20213 = DIRECTION ( 'NONE',  ( -0.7408284471490504952, 0.000000000000000000, 0.6716942845482061220 ) ) ;
#20214 = CARTESIAN_POINT ( 'NONE',  ( -4.288121723672178476, 8.224835454251337552, -0.7998128361456362523 ) ) ;
#20215 = CARTESIAN_POINT ( 'NONE',  ( 4.500305224345508393, -0.9970752094022590217, 1.871535012320741265 ) ) ;
#20217 = CARTESIAN_POINT ( 'NONE',  ( 10.97058181929407716, -5.254568858751050620, -0.2903707658989311269 ) ) ;
#20216 = CARTESIAN_POINT ( 'NONE',  ( 9.745613490124728884, 10.26430391476735338, 0.7998128361456462443 ) ) ;
#20218 = CARTESIAN_POINT ( 'NONE',  ( 5.061777102197771327, 1.950294035894485356, -0.2865203566276338654 ) ) ;
#20219 = CARTESIAN_POINT ( 'NONE',  ( 0.6823417656249882723, 0.9260416670080831025, -1.181850606188749264 ) ) ;
#20220 = CARTESIAN_POINT ( 'NONE',  ( 1.037359019205979171, -0.04529029187893931357, 2.012842730658084278 ) ) ;
#20221 = EDGE_LOOP ( 'NONE', ( #44618, #59558, #19590, #9328 ) ) ;
#20222 = CARTESIAN_POINT ( 'NONE',  ( 1.212693198809017270, 2.041623912717607237, 0.5605823208302792571 ) ) ;
#20223 = CARTESIAN_POINT ( 'NONE',  ( 9.304767520285516014, 11.47811317756902660, 7.581012809288346865 ) ) ;
#20224 = CARTESIAN_POINT ( 'NONE',  ( 2.383334800519558705, -0.002349189141126820958, 2.070544812199434315 ) ) ;
#20225 = ORIENTED_EDGE ( 'NONE', *, *, #60818, .F. ) ;
#20226 = CARTESIAN_POINT ( 'NONE',  ( 4.228163802615382494, 6.026220084508304708, -1.599625672291269396 ) ) ;
#20227 = CARTESIAN_POINT ( 'NONE',  ( 5.794130544993763898, 7.853181283949808744, 1.599625672291269396 ) ) ;
#20228 = ORIENTED_EDGE ( 'NONE', *, *, #127295, .F. ) ;
#20230 = CARTESIAN_POINT ( 'NONE',  ( 3.867100128395839942, 5.534702787927018974, -1.599625672291255185 ) ) ;
#20229 = CARTESIAN_POINT ( 'NONE',  ( 4.804676392994963408, 1.818819718876990565, 1.030695182279812272 ) ) ;
#20233 = VERTEX_POINT ( 'NONE', #73585 ) ;
#20232 = CARTESIAN_POINT ( 'NONE',  ( 1.066738840199648042, -1.428349636637029407, 1.113955053652333493 ) ) ;
#20231 = CARTESIAN_POINT ( 'NONE',  ( 2.994927033977520470, 1.566606242385214731, -0.9370212210159312161 ) ) ;
#20234 = CARTESIAN_POINT ( 'NONE',  ( 10.71502147350184231, 11.39527989537399755, 0.000000000000000000 ) ) ;
#20235 = DIRECTION ( 'NONE',  ( 0.000000000000000000, -1.000000000000000000, -0.000000000000000000 ) ) ;
#20236 = CARTESIAN_POINT ( 'NONE',  ( 10.14838338295609077, 13.59592256598955018, 7.283497017817778918 ) ) ;
#20237 = CARTESIAN_POINT ( 'NONE',  ( 5.790102700048296747, -0.9971039342967463748, 1.968745932239771568 ) ) ;
#20238 = CARTESIAN_POINT ( 'NONE',  ( 1.364683531250000748, 9.067708333674731946, -0.7879004041258355073 ) ) ;
#20239 = ORIENTED_EDGE ( 'NONE', *, *, #76805, .F. ) ;
#20240 = CARTESIAN_POINT ( 'NONE',  ( 4.512308969215598431, -1.911949174345693336, -0.04343532550177275214 ) ) ;
#20241 = CARTESIAN_POINT ( 'NONE',  ( -2.462777459176719308, 6.024990802348131780, -0.7998128361456281477 ) ) ;
#20242 = CARTESIAN_POINT ( 'NONE',  ( 7.853197290813620945, 10.18514947741448573, 1.599625672291281386 ) ) ;
#20243 = CARTESIAN_POINT ( 'NONE',  ( 6.742638474511262636, -2.029596885996234334, -0.4079607620106340260 ) ) ;
#20244 = CARTESIAN_POINT ( 'NONE',  ( -0.6801582343750316451, 0.2135416670080853008, 1.178068619123807004 ) ) ;
#20245 = CARTESIAN_POINT ( 'NONE',  ( 5.978782553502139940, 6.077593855281705260, -0.7216878364870257245 ) ) ;
#20246 = EDGE_CURVE ( 'NONE', #112981, #172406, #2561, .T. ) ;
#20247 = CARTESIAN_POINT ( 'NONE',  ( 5.706613541269077494, 1.932210019790636224, 1.034112652976440394 ) ) ;
#20248 = CARTESIAN_POINT ( 'NONE',  ( 6.170730229783032428, 7.061345527190763249, -1.063955632616358615 ) ) ;
#20249 = CARTESIAN_POINT ( 'NONE',  ( -1.797526709181193283, 15.47023744923392385, -11.89807871921767735 ) ) ;
#20250 = ORIENTED_EDGE ( 'NONE', *, *, #29169, .T. ) ;
#20251 = AXIS2_PLACEMENT_3D ( 'NONE', #124707, #190666, #42326 ) ;
#20252 = CARTESIAN_POINT ( 'NONE',  ( 1.499999999999821032, 7.388542872122531691, -4.154462424328212222 ) ) ;
#20253 = CARTESIAN_POINT ( 'NONE',  ( 4.130043426961079511, 1.002751595458702738, -1.578879078160302818 ) ) ;
#20254 = CARTESIAN_POINT ( 'NONE',  ( 0.000000000000000000, -0.9843749995220403282, -3.793834371823813445 ) ) ;
#20255 = FACE_OUTER_BOUND ( 'NONE', #177544, .T. ) ;
#20256 = CARTESIAN_POINT ( 'NONE',  ( -7.890482213473404727, 8.307910125248191946, 0.7216878364870578100 ) ) ;
#20257 = CARTESIAN_POINT ( 'NONE',  ( 4.167152111353856547, 5.955039778036558040, 1.599625672291262513 ) ) ;
#20258 = CARTESIAN_POINT ( 'NONE',  ( 6.322179702674084467, 6.270297829408224111, 1.040834085586084257E-14 ) ) ;
#20259 = CARTESIAN_POINT ( 'NONE',  ( 6.772334134356085222, -0.9704686269969391432, -1.828672837219179392 ) ) ;
#20260 = EDGE_CURVE ( 'NONE', #68331, #206477, #44305, .T. ) ;
#20261 = CARTESIAN_POINT ( 'NONE',  ( 0.7203276360899166786, 1.987051886588153682, 0.3419113104980234241 ) ) ;
#20262 = CARTESIAN_POINT ( 'NONE',  ( -8.109748439268576803, 12.61312361245537517, 0.7998128361456481317 ) ) ;
#20263 = CARTESIAN_POINT ( 'NONE',  ( 4.667750024854814050, 8.667735138964429709, -0.7998128361456381397 ) ) ;
#20264 = DIRECTION ( 'NONE',  ( 1.000000000000000000, 0.000000000000000000, 0.000000000000000000 ) ) ;
#20265 = CARTESIAN_POINT ( 'NONE',  ( 1.816621679704206516, 2.045545470589833492, 0.7867152234099920038 ) ) ;
#20266 = CARTESIAN_POINT ( 'NONE',  ( 5.900976575431972293, 1.489821718068456979, -1.054992404821846863 ) ) ;
#20267 = CARTESIAN_POINT ( 'NONE',  ( -2.435661151949389147, 5.993355110582911038, 0.7998128361456341429 ) ) ;
#20268 = CARTESIAN_POINT ( 'NONE',  ( 4.828112100242277549, 6.726159765073026264, -1.443375672974068769 ) ) ;
#20269 = CARTESIAN_POINT ( 'NONE',  ( 9.423080456697809026, 10.95234760669099749, -1.199719254218446718 ) ) ;
#20270 = CARTESIAN_POINT ( 'NONE',  ( 3.541704441667858472, 5.155074486744371853, -1.599625672291262513 ) ) ;
#20271 = CARTESIAN_POINT ( 'NONE',  ( 7.838022202476093270, 8.316983122409855156, 0.7216878364870267237 ) ) ;
#20272 = ORIENTED_EDGE ( 'NONE', *, *, #198939, .T. ) ;
#20274 = CARTESIAN_POINT ( 'NONE',  ( 1.137358842852369545, -0.04729656459989117767, 2.012689239070045488 ) ) ;
#20273 = CARTESIAN_POINT ( 'NONE',  ( 3.315785976855676775, 1.165629053876730659, -1.425327459889616177 ) ) ;
#20275 = CARTESIAN_POINT ( 'NONE',  ( 2.566106820329843163, 1.847058390165011721, -1.367687711909180148 ) ) ;
#20277 = CARTESIAN_POINT ( 'NONE',  ( 1.516205985490867381, 0.7479433349990645130, 1.704208623783896259 ) ) ;
#20276 = CARTESIAN_POINT ( 'NONE',  ( 2.887523530030648988, 6.312601851770308414, 0.000000000000000000 ) ) ;
#20278 = CARTESIAN_POINT ( 'NONE',  ( 0.000000000000000000, -0.7875000000000005329, -4.012584370867899430 ) ) ;
#20279 = CARTESIAN_POINT ( 'NONE',  ( -4.741601036477307574, 6.554953847355395880, 1.599625672291267398 ) ) ;
#20280 = SURFACE_SIDE_STYLE ('',( #184910 ) ) ;
#20281 = CARTESIAN_POINT ( 'NONE',  ( 4.043146078444789460, 0.09904687726844901841, 1.909973672635330910 ) ) ;
#20282 = CARTESIAN_POINT ( 'NONE',  ( -9.110189153378817295, 12.71597221466224603, 1.199719254218462483 ) ) ;
#20283 = MANIFOLD_SOLID_BREP ( 'Fillet1', #32676 ) ;
#20284 = CARTESIAN_POINT ( 'NONE',  ( 6.450676980830294838, 6.774405823990504949, -0.3487213023658369826 ) ) ;
#20285 = CARTESIAN_POINT ( 'NONE',  ( -6.943184063974175757, 9.193743722760251202, -1.443375672974066548 ) ) ;
#20287 = CARTESIAN_POINT ( 'NONE',  ( 2.518242125168220102, 1.223528130051700025, -1.415109699333151561 ) ) ;
#20286 = CARTESIAN_POINT ( 'NONE',  ( 3.456657222422593545, -1.844998171120499020, -0.9834188347317989187 ) ) ;
#20288 = CARTESIAN_POINT ( 'NONE',  ( 7.293923454472077239, 10.49303254931736262, 1.082531754730558626 ) ) ;
#20289 = CARTESIAN_POINT ( 'NONE',  ( -6.773376349081642545, -7.645986912801316926, -6.661184041422457902 ) ) ;
#20290 = CARTESIAN_POINT ( 'NONE',  ( 3.386022052710332186, -0.3430625053944387770, -1.706099273433875130 ) ) ;
#20291 = CARTESIAN_POINT ( 'NONE',  ( 3.798255590122797898, 7.583048621785260401, -0.7998128361456221525 ) ) ;
#20293 = CARTESIAN_POINT ( 'NONE',  ( -0.1010051578917390280, 3.387064998577566488, -1.997555336163420181 ) ) ;
#20292 = DIRECTION ( 'NONE',  ( -1.000000000000000000, 4.440892098500626162E-15, 0.000000000000000000 ) ) ;
#20294 = CARTESIAN_POINT ( 'NONE',  ( 3.721100771531059781, -0.1247040890464539975, 1.720429258078775669 ) ) ;
#20295 = CARTESIAN_POINT ( 'NONE',  ( 3.562233144267571650, -1.470601008620987749, 1.625073949779440419 ) ) ;
#20296 = CARTESIAN_POINT ( 'NONE',  ( 6.059228469117068805, -1.890744221452178353, -1.137928576693452820 ) ) ;
#20297 = CARTESIAN_POINT ( 'NONE',  ( 6.983263157960363898, 2.958708369276577876, 2.506372104999963657 ) ) ;
#20298 = STYLED_ITEM ( 'NONE', ( #24560 ), #212553 ) ;
#20299 = CARTESIAN_POINT ( 'NONE',  ( 3.379888771869215436, -2.093702847677909595, 0.5742949676477026033 ) ) ;
#20300 = CARTESIAN_POINT ( 'NONE',  ( 1.822601884235462766, 1.703052241681313861, 0.6583118566880485911 ) ) ;
#20301 = CARTESIAN_POINT ( 'NONE',  ( 0.3386216902839487841, -1.901412053528793722, -0.4823507731460881520 ) ) ;
#20302 = CARTESIAN_POINT ( 'NONE',  ( 4.698512310153400762, 1.457641359173178275, -1.535954635999142948 ) ) ;
#20303 = VERTEX_POINT ( 'NONE', #207842 ) ;
#20305 = CARTESIAN_POINT ( 'NONE',  ( -1.201851678989727383E-14, 2.634375000341417916, 1.575800808251672791 ) ) ;
#20304 = CARTESIAN_POINT ( 'NONE',  ( 5.319995955860258974, 1.367515572929053791, -1.839686415443070100 ) ) ;
#20306 = CARTESIAN_POINT ( 'NONE',  ( 6.720655732516628511, 2.062125556784020652, 2.233254568942647733 ) ) ;
#20307 = CARTESIAN_POINT ( 'NONE',  ( 10.40318394038753702, 11.03146944007395724, -0.7998128361456281477 ) ) ;
#20308 = CARTESIAN_POINT ( 'NONE',  ( 0.2059360158346480729, 1.574223368660916611, 1.420867075595611650 ) ) ;
#20309 = CARTESIAN_POINT ( 'NONE',  ( -5.097502569058215194, 6.970172302033127210, -1.443375672974053447 ) ) ;
#20310 = CARTESIAN_POINT ( 'NONE',  ( 3.879041346841291649, 7.539648981374564407, 1.040834085586084257E-14 ) ) ;
#20311 = CARTESIAN_POINT ( 'NONE',  ( -5.436456408955534947, 6.405249234278626247, 1.082531754730546636 ) ) ;
#20312 = AXIS2_PLACEMENT_3D ( 'NONE', #72256, #53900, #120036 ) ;
#20314 = CARTESIAN_POINT ( 'NONE',  ( -1.402160292154681736E-14, 11.84375000068279604, 1.732050807568881190 ) ) ;
#20313 = CARTESIAN_POINT ( 'NONE',  ( 6.883263157960365142, 1.273421409013283823, 2.069651443392322765 ) ) ;
#20315 = ORIENTED_EDGE ( 'NONE', *, *, #145048, .T. ) ;
#20316 = CARTESIAN_POINT ( 'NONE',  ( 5.098279808040273586, -0.2930726886911338425, 1.994869512123042199 ) ) ;
#20318 = CARTESIAN_POINT ( 'NONE',  ( 4.592669665391247769, 2.021776019120101520, 0.4074096221951555297 ) ) ;
#20317 = CARTESIAN_POINT ( 'NONE',  ( 4.904298879841284098, 6.744767997946721216, 1.599625672291267398 ) ) ;
#20320 = CARTESIAN_POINT ( 'NONE',  ( -3.475000000000000533, -3.499999999999999556, 0.000000000000000000 ) ) ;
#20319 = CARTESIAN_POINT ( 'NONE',  ( 4.844006021832467646, 8.873367135438366304, 0.000000000000000000 ) ) ;
#20321 = CARTESIAN_POINT ( 'NONE',  ( 6.658989722967328717, 7.797851427330578566, 1.199719254218452935 ) ) ;
#20322 = CARTESIAN_POINT ( 'NONE',  ( 1.642778471875000035, -0.9260416661887073131, -2.845375778867859751 ) ) ;
#20323 = CYLINDRICAL_SURFACE ( 'NONE', #199735, 1.250000000000000000 ) ;
#20324 = CARTESIAN_POINT ( 'NONE',  ( 0.8496949173334772398, 2.088161746953997255, -0.1042977956757246832 ) ) ;
#20325 = CARTESIAN_POINT ( 'NONE',  ( 4.254529844270301453, 1.955172953530256219, -0.4926405443339901269 ) ) ;
#20326 = CARTESIAN_POINT ( 'NONE',  ( 4.370544011308346910, -0.004580445953385886559, -1.841430844414258861 ) ) ;
#20327 = CARTESIAN_POINT ( 'NONE',  ( 6.681470773436232413, 6.689470745297396270, -0.7998128361456281477 ) ) ;
#20328 = CARTESIAN_POINT ( 'NONE',  ( 0.8676543833149966689, 0.8442763457921966808, 1.503926039954103677 ) ) ;
#20329 = CARTESIAN_POINT ( 'NONE',  ( 11.33772463945036790, 12.69999999999999929, -3.600000000000000977 ) ) ;
#20330 = CARTESIAN_POINT ( 'NONE',  ( 0.8448572530952251913, 0.4413087945813984336, -2.255810399402935484 ) ) ;
#20331 = CARTESIAN_POINT ( 'NONE',  ( -6.063521013809733518, 8.097193820909906137, 1.599625672291283607 ) ) ;
#20332 = CARTESIAN_POINT ( 'NONE',  ( 0.7555949320777423095, -1.911880202960547948, -1.209378468041100607 ) ) ;
#20333 = CARTESIAN_POINT ( 'NONE',  ( 2.719469050394443421, -0.2056238487441063856, 2.096000168696035448 ) ) ;
#20334 = CARTESIAN_POINT ( 'NONE',  ( -5.743814354044916470, 6.730146830254374990, -1.199719254218453823 ) ) ;
#20335 = CARTESIAN_POINT ( 'NONE',  ( 8.098297826064319693, 8.342435640030188893, 0.7998128361456481317 ) ) ;
#20336 = CARTESIAN_POINT ( 'NONE',  ( 6.333067150914816423, 7.521571443223021625, 1.082531754730549967 ) ) ;
#20338 = EDGE_CURVE ( 'NONE', #209328, #195818, #50925, .T. ) ;
#20337 = CARTESIAN_POINT ( 'NONE',  ( -6.632963465583701534, 8.761543347979550589, -1.599625672291263179 ) ) ;
#20339 = B_SPLINE_CURVE_WITH_KNOTS ( 'NONE', 3,
 ( #109728, #97692, #113999, #159470, #43610, #195179, #63035, #110788, #7051, #139227 ),
 .UNSPECIFIED., .F., .F.,
 ( 4, 3, 3, 4 ),
 ( 7.620576258561039861E-17, 9.102628012183976516E-05, 0.0001374522152767717893, 0.0001846341747205655518 ),
 .UNSPECIFIED. ) ;
#20340 = CARTESIAN_POINT ( 'NONE',  ( 6.602457619730767391, 7.765583980183128787, 1.082531754730558626 ) ) ;
#20341 = CARTESIAN_POINT ( 'NONE',  ( 4.388746605030885206, 7.362284722717403085, 1.177686187499202619 ) ) ;
#20342 = CARTESIAN_POINT ( 'NONE',  ( -4.647747731386360215, 4.316793862905830892, 0.7998128361456341429 ) ) ;
#20343 = CARTESIAN_POINT ( 'NONE',  ( 5.467086432746695479, -1.751203904306109838, 1.366580491753234039 ) ) ;
#20344 = CARTESIAN_POINT ( 'NONE',  ( 2.713028398602938651, -0.2137989841624072795, 2.180988865010752509 ) ) ;
#20345 = CARTESIAN_POINT ( 'NONE',  ( -4.564291269294938225, 8.476756914152748124, 1.040834085586084257E-14 ) ) ;
#20347 = CIRCLE ( 'NONE', #141481, 0.07999999999999968248 ) ;
#20346 = CARTESIAN_POINT ( 'NONE',  ( -5.307090785106547415, 5.156303768904543894, -0.7998128361456362523 ) ) ;
#20348 = CARTESIAN_POINT ( 'NONE',  ( 5.213317179658601752, -1.656387821537348426, -1.051046178410528942 ) ) ;
#20349 = CARTESIAN_POINT ( 'NONE',  ( 0.6823417656249899377, 2.592708333674753618, 1.181850606188767472 ) ) ;
#20350 = CARTESIAN_POINT ( 'NONE',  ( 6.890000000000009450, 0.5473178204696281801, 2.329866691457019190 ) ) ;
#20351 = CARTESIAN_POINT ( 'NONE',  ( -5.924549939491850381, 6.014322472269677533, 0.000000000000000000 ) ) ;
#20352 = CARTESIAN_POINT ( 'NONE',  ( 4.359710196644346780, -1.641147893522959089, -1.343014508298406628 ) ) ;
#20353 = CARTESIAN_POINT ( 'NONE',  ( -7.160114521792834807, 8.486460042580672436, 1.082531754730549078 ) ) ;
#20354 = ORIENTED_EDGE ( 'NONE', *, *, #11240, .T. ) ;
#20356 = CARTESIAN_POINT ( 'NONE',  ( 4.559605246071182449, 3.300000000000025135, -0.7749999999999944711 ) ) ;
#20355 = CARTESIAN_POINT ( 'NONE',  ( -6.644904684473536882, 6.925012684740138980, 0.7216878364870317197 ) ) ;
#20357 = CARTESIAN_POINT ( 'NONE',  ( 6.817052309572890323, 6.847649204123507083, 0.7998128361456341429 ) ) ;
#20358 = CARTESIAN_POINT ( 'NONE',  ( 5.583513413114173041, -0.8223277247318347971, 1.647484189299788682 ) ) ;
#20359 = UNCERTAINTY_MEASURE_WITH_UNIT (LENGTH_MEASURE( 1.000000000000000082E-05 ), #16274, 'distance_accuracy_value', 'NONE');
#20360 = CARTESIAN_POINT ( 'NONE',  ( 1.224999999999998757, 0.9375000006827949317, -8.673617379884035472E-15 ) ) ;
#20361 = CARTESIAN_POINT ( 'NONE',  ( 0.6823417656249882723, 2.238541667008084435, -1.181850606188749264 ) ) ;
#20362 = CARTESIAN_POINT ( 'NONE',  ( 1.153398195617076682, 0.7042877955899041753, 1.591771711926233346 ) ) ;
#20363 = CARTESIAN_POINT ( 'NONE',  ( 0.2375137461210129197, 3.335658684549960284, 2.061805365461736983 ) ) ;
#20364 = CARTESIAN_POINT ( 'NONE',  ( -0.4320269763655096851, 3.055387103097219281, 0.4199383792806183902 ) ) ;
#20365 = CARTESIAN_POINT ( 'NONE',  ( 5.366167234668930419, 1.061923416652654550, 1.882811416686725359 ) ) ;
#20366 = EDGE_CURVE ( 'NONE', #39859, #52099, #159104, .T. ) ;
#20367 = AXIS2_PLACEMENT_3D ( 'NONE', #165931, #148622, #149685 ) ;
#20368 = CARTESIAN_POINT ( 'NONE',  ( -4.029797971759847997, 5.724516938518342535, -1.599625672291256295 ) ) ;
#20369 = CARTESIAN_POINT ( 'NONE',  ( -6.683806541412762314, 9.781229484081471526, -1.082531754730537976 ) ) ;
#20370 = CARTESIAN_POINT ( 'NONE',  ( 4.293933718354110418, -0.8299404887524584051, 1.996233173270183681 ) ) ;
#20371 = CARTESIAN_POINT ( 'NONE',  ( -0.6823417656249969321, 3.217708333674754062, -1.181850606188749264 ) ) ;
#20372 = CARTESIAN_POINT ( 'NONE',  ( 5.255133876903111734, -1.663856106090171538, -1.057019077474026680 ) ) ;
#20373 = CARTESIAN_POINT ( 'NONE',  ( 3.637800481086241433, 0.04416708034036923719, -1.733463101117929339 ) ) ;
#20374 = CARTESIAN_POINT ( 'NONE',  ( 1.189316404147572337, 1.662717542896676504, 1.427817766309902314 ) ) ;
#20375 = CARTESIAN_POINT ( 'NONE',  ( 1.940857006665818174, 2.282658722630509729, 0.3375727702036589450 ) ) ;
#20376 = CARTESIAN_POINT ( 'NONE',  ( 3.585278813505449858, 1.864625933638365485, -0.8777486340088790362 ) ) ;
#20377 = CARTESIAN_POINT ( 'NONE',  ( 0.3396542298245264213, 1.936664667523413152, 0.1439508268369827926 ) ) ;
#20378 = CARTESIAN_POINT ( 'NONE',  ( -7.673551755210395342, 8.054824590608001600, 1.040834085586084257E-14 ) ) ;
#20380 = EDGE_CURVE ( 'NONE', #37994, #72298, #51707, .T. ) ;
#20379 = CARTESIAN_POINT ( 'NONE',  ( -5.631432701629818460, 7.663367133358481631, 1.599625672291263179 ) ) ;
#20381 =( NAMED_UNIT ( * ) PLANE_ANGLE_UNIT ( ) SI_UNIT ( $, .RADIAN. ) );
#20382 = CARTESIAN_POINT ( 'NONE',  ( -4.679499295372141709, 5.488445928469455559, 1.199719254218452935 ) ) ;
#20383 = CARTESIAN_POINT ( 'NONE',  ( -6.900736999231456004, 8.113576589600553390, 1.082531754730549967 ) ) ;
#20384 = CARTESIAN_POINT ( 'NONE',  ( 2.977765718515757332, 2.095881712254169305, -0.6909776239150815513 ) ) ;
#20385 = CARTESIAN_POINT ( 'NONE',  ( -1.642778471874998480, -2.238541666188708312, 2.845375778867863303 ) ) ;
#20386 = CARTESIAN_POINT ( 'NONE',  ( 0.3911518402437937358, -1.704754640775848928, 0.7467128926999586636 ) ) ;
#20387 = DIRECTION ( 'NONE',  ( 2.433448702482861237E-17, -0.8987940462991643731, -0.4383711467890826219 ) ) ;
#20388 = DIRECTION ( 'NONE',  ( 1.000000000000000000, -0.000000000000000000, -0.000000000000000000 ) ) ;
#20389 = CARTESIAN_POINT ( 'NONE',  ( -9.536979704252539491, -7.995840219786908065, 0.1489494290324817893 ) ) ;
#20391 = CARTESIAN_POINT ( 'NONE',  ( 6.925078400183553029, 2.941156041390875941, 2.696161060448130975 ) ) ;
#20390 = CARTESIAN_POINT ( 'NONE',  ( -4.648357846327917819, 8.420182996469929293, -0.5132882116619559287 ) ) ;
#20392 = CARTESIAN_POINT ( 'NONE',  ( 5.964778383650899407, 0.1308802983275309528, -1.836551591404868233 ) ) ;
#20393 = ORIENTED_EDGE ( 'NONE', *, *, #50263, .F. ) ;
#20394 = CARTESIAN_POINT ( 'NONE',  ( 3.643480044026959241, -1.559369103033839465, -1.347540176210021423 ) ) ;
#20395 = CARTESIAN_POINT ( 'NONE',  ( 0.6801582343749796866, 1.473958333674751930, 1.178068619123789462 ) ) ;
#20396 = UNCERTAINTY_MEASURE_WITH_UNIT (LENGTH_MEASURE( 1.000000000000000082E-05 ), #111707, 'distance_accuracy_value', 'NONE');
#20397 = CARTESIAN_POINT ( 'NONE',  ( -5.042743069279040036, 7.970618449879118828, 1.199719254218464037 ) ) ;
#20398 = CARTESIAN_POINT ( 'NONE',  ( 2.578776193315842846, -1.391201028639722281, 1.464365899026105700 ) ) ;
#20399 = FACE_OUTER_BOUND ( 'NONE', #197140, .T. ) ;
#20400 = TOROIDAL_SURFACE ( 'NONE', #148296, 0.8299999999999998490, 0.08000000000000000167 ) ;
#20401 = CARTESIAN_POINT ( 'NONE',  ( 4.844340958784499662, 4.546152628203684820, 0.7998128361456341429 ) ) ;
#20402 = CARTESIAN_POINT ( 'NONE',  ( 1.604443549136617575, -0.7409017435648653782, -1.923293390451373819 ) ) ;
#20404 = CARTESIAN_POINT ( 'NONE',  ( 0.6823417656249934904, 12.69270833367473017, 1.181850606188764807 ) ) ;
#20403 = CARTESIAN_POINT ( 'NONE',  ( -1.483456582845284810, 7.293967155395466584, -4.258619948150268009 ) ) ;
#20405 = CARTESIAN_POINT ( 'NONE',  ( 7.318703993278529829, 7.432909501780090800, 1.040834085586084257E-14 ) ) ;
#20406 = CARTESIAN_POINT ( 'NONE',  ( 5.039771180630152614, -1.558841386063321455, -1.562417271110942307 ) ) ;
#20407 = CARTESIAN_POINT ( 'NONE',  ( 1.001511639980020130, 1.766541945284912263, 1.245431700958275600 ) ) ;
#20408 = CIRCLE ( 'NONE', #89561, 10.86343145750506700 ) ;
#20409 = CARTESIAN_POINT ( 'NONE',  ( -5.422898255786209099, 5.429062174613087599, -0.7216878364870207285 ) ) ;
#20410 = CARTESIAN_POINT ( 'NONE',  ( 0.7257964430846426396, 0.8128130212789463904, -1.845628942776005088 ) ) ;
#20411 = CARTESIAN_POINT ( 'NONE',  ( 1.880608668887576052, -0.2816854878555269392, 2.281025131504022863 ) ) ;
#20412 = CARTESIAN_POINT ( 'NONE',  ( -5.204170427930421283E-15, -7.242250812739418286, -9.811039896441874575 ) ) ;
#20413 = CARTESIAN_POINT ( 'NONE',  ( 6.287759715630294011, 1.828497742151834027, -0.5598019499635784602 ) ) ;
#20414 = CARTESIAN_POINT ( 'NONE',  ( 3.100381309523608131, 6.448533663283696704, -0.4548243241709319928 ) ) ;
#20415 = CARTESIAN_POINT ( 'NONE',  ( 1.621729638615863944, -1.036547396872866678, -1.557007864774778705 ) ) ;
#20416 = CARTESIAN_POINT ( 'NONE',  ( 4.030482632556767975, 0.5424685788828055300, 1.942097399793737633 ) ) ;
#20418 = CARTESIAN_POINT ( 'NONE',  ( 11.48767021851169190, 13.83004227463828784, 3.470194894594622159 ) ) ;
#20417 = CARTESIAN_POINT ( 'NONE',  ( -0.6823417656250212460, 2.051041667008083991, 1.181850606188767472 ) ) ;
#20420 = CARTESIAN_POINT ( 'NONE',  ( 5.145193760806440864, -1.806914327231067929, 1.081695767794567775 ) ) ;
#20419 = CARTESIAN_POINT ( 'NONE',  ( -6.692921386640485082, 10.96015871772258521, -0.7998128361456291469 ) ) ;
#20421 = CARTESIAN_POINT ( 'NONE',  ( 6.608709811657416999, 9.797579649320619311, -1.199719254218440723 ) ) ;
#20423 = CARTESIAN_POINT ( 'NONE',  ( -8.040148788103921973, 9.338927326664741457, 1.199719254218462483 ) ) ;
#20422 = CARTESIAN_POINT ( 'NONE',  ( 5.194709132691408549, 6.089524072008651423, 1.199719254218452935 ) ) ;
#20424 = CARTESIAN_POINT ( 'NONE',  ( 1.291015824433225490, 3.619357176192806946, -0.4575187270168888931 ) ) ;
#20425 = CARTESIAN_POINT ( 'NONE',  ( 5.713150811708690213, 1.648777711927760015, -1.166343465331370455 ) ) ;
#20426 = CARTESIAN_POINT ( 'NONE',  ( 1.499999999999987566, -1.193749999317185395, 0.000000000000000000 ) ) ;
#20427 = CARTESIAN_POINT ( 'NONE',  ( 1.182570505923411952, 1.231668817017372408, -1.654277799056037335 ) ) ;
#20428 = CARTESIAN_POINT ( 'NONE',  ( 9.097157885089661278, 9.715698408800516717, 1.040834085586084257E-14 ) ) ;
#20429 = CARTESIAN_POINT ( 'NONE',  ( 5.254667053748194760, 8.288139441751686931, 1.199719254218452047 ) ) ;
#20430 = CARTESIAN_POINT ( 'NONE',  ( 0.6823417656249882723, -0.8447916663252494907, 1.181850606188755259 ) ) ;
#20432 = CARTESIAN_POINT ( 'NONE',  ( 1.347111479062088405E-15, 5.000000000000000888, 11.00000000000000000 ) ) ;
#20431 = CARTESIAN_POINT ( 'NONE',  ( 5.367048706163317640, 7.354919138647580290, -1.599625672291281386 ) ) ;
#20433 = CARTESIAN_POINT ( 'NONE',  ( 8.392133896734671694, 8.893170422386358354, 0.7216878364870458196 ) ) ;
#20435 = CARTESIAN_POINT ( 'NONE',  ( 0.000000000000000000, 0.000000000000000000, 0.000000000000000000 ) ) ;
#20434 = CARTESIAN_POINT ( 'NONE',  ( 2.945941647375094785, 1.533668492858210497, 1.537084210998492795 ) ) ;
#20437 = CARTESIAN_POINT ( 'NONE',  ( 2.278628554356322500, 1.682734121078124812, -0.7478279864501293783 ) ) ;
#20436 = CARTESIAN_POINT ( 'NONE',  ( -5.910991785878175975, 6.958873840688411860, -1.082531754730544860 ) ) ;
#20438 = CARTESIAN_POINT ( 'NONE',  ( -0.6823417656250212460, 3.551041667008085323, 1.181850606188767472 ) ) ;
#20440 = CARTESIAN_POINT ( 'NONE',  ( 4.247736854543925133, 2.191053489037126045, -0.05455935714590579716 ) ) ;
#20439 = B_SPLINE_CURVE_WITH_KNOTS ( 'NONE', 3,
 ( #22973, #38190, #138907, #186562, #88006, #73891, #5644, #89091, #155145, #24053, #79215, #59766, #76020, #14189, #195105, #13139 ),
 .UNSPECIFIED., .F., .F.,
 ( 4, 3, 3, 3, 3, 4 ),
 ( 0.000000000000000000, 2.688023894042651662E-05, 5.355394816896161286E-05, 9.073944566322023530E-05, 0.0001419156937261415808, 0.0001738851243175521086 ),
 .UNSPECIFIED. ) ;
#20441 = CARTESIAN_POINT ( 'NONE',  ( 6.883263157960363365, 3.690127339433949327, 2.567897385111846731 ) ) ;
#20442 = CARTESIAN_POINT ( 'NONE',  ( 5.032209928657234599, 1.167594373104458461, -1.937845176762391874 ) ) ;
#20443 = CARTESIAN_POINT ( 'NONE',  ( -4.543954038874438162, 8.453030145328826350, 1.040834085586084257E-14 ) ) ;
#20444 = FACE_OUTER_BOUND ( 'NONE', #41048, .T. ) ;
#20445 = CARTESIAN_POINT ( 'NONE',  ( 5.364009635805341958, 7.578432035813580825, -1.241402483855597039 ) ) ;
#20446 = CARTESIAN_POINT ( 'NONE',  ( -1.500000000000001110, 13.77083333333332860, 0.8660254037844419273 ) ) ;
#20447 = CARTESIAN_POINT ( 'NONE',  ( -6.251718229232857915, 7.426664367927358512, -1.082531754730549967 ) ) ;
#20448 = CARTESIAN_POINT ( 'NONE',  ( 4.231553341240963384, 7.950912974840849579, -0.7216878364870357165 ) ) ;
#20449 = CARTESIAN_POINT ( 'NONE',  ( 5.307753102408475421, -1.761140305208692913, 0.1738094965475830145 ) ) ;
#20450 = CARTESIAN_POINT ( 'NONE',  ( 8.284195553149872993, 9.623648552551724578, -1.199719254218445830 ) ) ;
#20451 = CARTESIAN_POINT ( 'NONE',  ( 2.450341380362738075, 2.105475501793910631, 0.05272098179117353650 ) ) ;
#20453 = CARTESIAN_POINT ( 'NONE',  ( 0.7499999999999885647, 3.066666666666689522, -1.299038105676658228 ) ) ;
#20452 = CARTESIAN_POINT ( 'NONE',  ( -8.012344526598182026E-15, 11.79687500034140157, -1.575800808251669460 ) ) ;
#20455 = EDGE_CURVE ( 'NONE', #78710, #163734, #138660, .T. ) ;
#20454 = CARTESIAN_POINT ( 'NONE',  ( 2.084365741702984387, 1.136530121079984301, -1.608336531363078414 ) ) ;
#20456 = CARTESIAN_POINT ( 'NONE',  ( -3.634467696915153034, 6.397906858779740524, 1.199719254218452935 ) ) ;
#20457 = CARTESIAN_POINT ( 'NONE',  ( 1.499999999999961586, 5.327083334016154303, -0.8660254037844482555 ) ) ;
#20459 = ORIENTED_EDGE ( 'NONE', *, *, #188352, .F. ) ;
#20458 = CARTESIAN_POINT ( 'NONE',  ( 5.888875516108613262, -1.723027129771546484, -0.5597982944235294633 ) ) ;
#20460 = CARTESIAN_POINT ( 'NONE',  ( 5.504247177468175600, 8.405076892812779477, 1.082531754730558626 ) ) ;
#20461 = CARTESIAN_POINT ( 'NONE',  ( 0.6823417656249882723, -1.094791666325249713, 1.181850606188755259 ) ) ;
#20462 = CARTESIAN_POINT ( 'NONE',  ( 5.489076674590072535, 1.649195787720953987, -0.8828566466120501000 ) ) ;
#20463 = CARTESIAN_POINT ( 'NONE',  ( 10.53876547652418338, 11.18964789890005918, 0.7998128361456462443 ) ) ;
#20464 = CARTESIAN_POINT ( 'NONE',  ( 5.471561611210747245, -0.3092806512635417060, 2.046926588373791933 ) ) ;
#20465 = CARTESIAN_POINT ( 'NONE',  ( -5.492461626867567226, 6.540864998501174199, 1.082531754730549078 ) ) ;
#20466 =( NAMED_UNIT ( * ) PLANE_ANGLE_UNIT ( ) SI_UNIT ( $, .RADIAN. ) );
#20467 = CARTESIAN_POINT ( 'NONE',  ( -0.7500000000000215383, 0.4416666666666874130, 1.299038105676659116 ) ) ;
#20468 = CARTESIAN_POINT ( 'NONE',  ( 7.832860060393120882, 10.16142270859057462, 1.599625672291281386 ) ) ;
#20469 = CARTESIAN_POINT ( 'NONE',  ( -8.154339323615371171, 11.60081407993821045, 1.199719254218453823 ) ) ;
#20470 = CARTESIAN_POINT ( 'NONE',  ( 5.668190738965027897, 8.770583741171307679, -1.199719254218452047 ) ) ;
#20471 = CARTESIAN_POINT ( 'NONE',  ( -0.6823417656250246877, -0.1989583329919109023, 1.181850606188755259 ) ) ;
#20473 = EDGE_CURVE ( 'NONE', #54700, #167113, #124617, .T. ) ;
#20472 = CARTESIAN_POINT ( 'NONE',  ( 1.499999999999985123, 0.5458333333333577064, -0.8660254037844253849 ) ) ;
#20475 = CARTESIAN_POINT ( 'NONE',  ( 6.634017235788401301, 6.634108284708264414, 0.7998128361456341429 ) ) ;
#20474 = CARTESIAN_POINT ( 'NONE',  ( 5.512146440779991607, 1.959692598237902761, -0.09458084330612320789 ) ) ;
#20476 = CARTESIAN_POINT ( 'NONE',  ( 3.391953724946985105, 0.04666865176591523945, 2.015725201127672506 ) ) ;
#20477 = CARTESIAN_POINT ( 'NONE',  ( 3.028439059693835311, 0.4704065786719989761, 1.856910451861475631 ) ) ;
#20478 = DIRECTION ( 'NONE',  ( 0.9692622846690300831, 0.000000000000000000, 0.2460297208025325477 ) ) ;
#20479 = CARTESIAN_POINT ( 'NONE',  ( 0.1522426329377546128, 0.8445714516599597266, 2.022489037641273857 ) ) ;
#20480 = CARTESIAN_POINT ( 'NONE',  ( 0.2335667940003048615, 2.868049447791064743, -2.641685461849890171 ) ) ;
#20481 = CARTESIAN_POINT ( 'NONE',  ( 1.633845377418343237, 0.9265681688636999702, -1.624882239709434018 ) ) ;
#20482 = CARTESIAN_POINT ( 'NONE',  ( 0.6823417656249917140, 5.342708333674749177, 1.181850606188765695 ) ) ;
#20483 = CARTESIAN_POINT ( 'NONE',  ( 4.377201702235844927, -1.800125857882298508, -0.9014936589236545172 ) ) ;
#20484 = CARTESIAN_POINT ( 'NONE',  ( -7.263417608619167076, 9.497073181520933716, -1.599625672291263179 ) ) ;
#20486 = CARTESIAN_POINT ( 'NONE',  ( 4.728176305778284849, 2.111628383735635328, 0.1544883665849701437 ) ) ;
#20485 = CARTESIAN_POINT ( 'NONE',  ( -5.477130870240893401, 6.452702772444876445, 1.082531754730548412 ) ) ;
#20487 = CARTESIAN_POINT ( 'NONE',  ( -3.672711609586798782E-15, -9.954379061088836522, -9.579665937615013505 ) ) ;
#20488 = CARTESIAN_POINT ( 'NONE',  ( 6.162566008723842081, -0.7415158119226210598, -1.933206815039355320 ) ) ;
#20490 = CARTESIAN_POINT ( 'NONE',  ( 6.620655732516652847, 2.941130357193070033, 2.725706755162327966 ) ) ;
#20489 = CARTESIAN_POINT ( 'NONE',  ( 1.329752858235648150, 1.027315703197308361, -1.820849364048042318 ) ) ;
#20492 = ORIENTED_EDGE ( 'NONE', *, *, #72514, .F. ) ;
#20491 = CARTESIAN_POINT ( 'NONE',  ( 6.458013382736495167, 1.820430347099718293, -0.1376817787434730933 ) ) ;
#20493 = CARTESIAN_POINT ( 'NONE',  ( 8.263858322729371153, 9.599921783727809910, -1.199719254218446718 ) ) ;
#20494 = CARTESIAN_POINT ( 'NONE',  ( -3.470524135418306066, 6.992769224722549914, -0.7216878364870351614 ) ) ;
#20495 = DIRECTION ( 'NONE',  ( 0.000000000000000000, 1.000000000000000000, 0.000000000000000000 ) ) ;
#20496 = CARTESIAN_POINT ( 'NONE',  ( -10.19097401674926395, 4.476076320095182304, 5.708917106338025960 ) ) ;
#20497 = CARTESIAN_POINT ( 'NONE',  ( 6.385527161912102123, 9.433236874664039817, -1.082531754730537976 ) ) ;
#20498 = CARTESIAN_POINT ( 'NONE',  ( -1.907692715643321657, 3.236394383240515982, 0.4609675857477188998 ) ) ;
#20500 = CARTESIAN_POINT ( 'NONE',  ( 0.9436867518335406713, -1.148578278726499757, -1.400746029399003501 ) ) ;
#20499 = CARTESIAN_POINT ( 'NONE',  ( 5.830888582329017744, 8.960397891762626799, -1.199719254218452047 ) ) ;
#20501 = CARTESIAN_POINT ( 'NONE',  ( -6.808165692356648258, 11.09461040772476714, 0.7998128361456481317 ) ) ;
#20502 = CARTESIAN_POINT ( 'NONE',  ( 5.464099601507359516, 6.333536608968757697, 1.199719254218462483 ) ) ;
#20503 = B_SPLINE_CURVE_WITH_KNOTS ( 'NONE', 3,
 ( #65623, #211896, #164231, #195671, #197776, #49414, #181529, #128623, #45172, #165287 ),
 .UNSPECIFIED., .F., .F.,
 ( 4, 3, 3, 4 ),
 ( 3.263880750628924922E-18, 3.125190611472425774E-05, 6.297331589974846625E-05, 6.656384948891156620E-05 ),
 .UNSPECIFIED. ) ;
#20504 = CARTESIAN_POINT ( 'NONE',  ( -6.992767129439147133, -7.336076765398686028, -7.649321060469615574 ) ) ;
#20505 = CARTESIAN_POINT ( 'NONE',  ( 4.010558181858147719, 7.580895019428740333, -0.2605091080661054437 ) ) ;
#20506 = CARTESIAN_POINT ( 'NONE',  ( 3.009020027229115879, 5.597941567487558778, -1.199719254218446718 ) ) ;
#20507 = VERTEX_POINT ( 'NONE', #59517 ) ;
#20508 = VECTOR ( 'NONE', #40218, 1000.000000000000000 ) ;
#20509 = CARTESIAN_POINT ( 'NONE',  ( 6.081657687927014777, -0.6766999560612970699, 1.899624756701682626 ) ) ;
#20510 = CARTESIAN_POINT ( 'NONE',  ( 0.3816889160728509367, 0.2035859187828891470, -2.110680546376259681 ) ) ;
#20511 = CARTESIAN_POINT ( 'NONE',  ( -3.000121558099561270, 6.395101958814021437, -0.7378544084795432001 ) ) ;
#20512 = CARTESIAN_POINT ( 'NONE',  ( -0.1394461523061013564, 4.080274402048936544, -2.835111295649892060 ) ) ;
#20513 = CARTESIAN_POINT ( 'NONE',  ( 1.854512760316388897, 2.488359591189891251, 2.484105960264901825 ) ) ;
#20514 = CARTESIAN_POINT ( 'NONE',  ( -4.121315508874269007, 5.831287398485176077, -1.443375672974053447 ) ) ;
#20515 = CARTESIAN_POINT ( 'NONE',  ( 9.734391104931951588, 11.41950637958454706, 1.082531754730548412 ) ) ;
#20516 = CARTESIAN_POINT ( 'NONE',  ( 3.907052821786443975, -1.612583007836394966, 1.130340192709837766 ) ) ;
#20517 = ADVANCED_FACE ( 'NONE', ( #55265 ), #147730, .T. ) ;
#20519 = CARTESIAN_POINT ( 'NONE',  ( 4.464470365011488973, -1.956567236562205325, -0.4871837624095613495 ) ) ;
#20518 = B_SPLINE_CURVE_WITH_KNOTS ( 'NONE', 3,
 ( #79233, #111807, #98686, #130195, #97637, #163694 ),
 .UNSPECIFIED., .F., .F.,
 ( 4, 2, 4 ),
 ( 0.0006378314054480077946, 0.0009584618939205538689, 0.001279092382393099943 ),
 .UNSPECIFIED. ) ;
#20520 = CARTESIAN_POINT ( 'NONE',  ( -5.530836599371015794, 8.540060901653093950, 1.199719254218452047 ) ) ;
#20521 = CARTESIAN_POINT ( 'NONE',  ( -5.181866634007240791, 6.340624232048664766, 1.284222742053082733 ) ) ;
#20522 = CARTESIAN_POINT ( 'NONE',  ( 4.998067021457727854, -0.7363416341295281331, -2.064161796032103258 ) ) ;
#20523 = FACE_OUTER_BOUND ( 'NONE', #146390, .T. ) ;
#20524 = CARTESIAN_POINT ( 'NONE',  ( 3.487250860276095210, 1.742034520097140771, -0.8226350277544016709 ) ) ;
#20525 = CARTESIAN_POINT ( 'NONE',  ( -6.184490626128011925, 10.36698949712469364, -0.7998128361456291469 ) ) ;
#20526 = EDGE_CURVE ( 'NONE', #56362, #6371, #108347, .T. ) ;
#20527 = CARTESIAN_POINT ( 'NONE',  ( -0.02968770228140016343, 0.003472272166151618711, -1.826291111852257343 ) ) ;
#20528 = CARTESIAN_POINT ( 'NONE',  ( 0.1331565106231328566, 1.371277436080810208, -2.201942895618694607 ) ) ;
#20529 =( LENGTH_UNIT ( ) NAMED_UNIT ( * ) SI_UNIT ( .MILLI., .METRE. ) );
#20530 = ORIENTED_EDGE ( 'NONE', *, *, #114198, .F. ) ;
#20531 = CARTESIAN_POINT ( 'NONE',  ( 4.095971805104288599, 5.871996087412059140, 1.443375672974058777 ) ) ;
#20532 = CARTESIAN_POINT ( 'NONE',  ( 5.313322838536244319, -1.661678602684885986, -1.056841482759300233 ) ) ;
#20534 = CARTESIAN_POINT ( 'NONE',  ( 4.020185130887462321, -2.007537125943322120, 0.1504822817294942383 ) ) ;
#20533 = CARTESIAN_POINT ( 'NONE',  ( 0.5736477084636192325, -1.077812090576779402, 1.615333711560530849 ) ) ;
#20535 = CARTESIAN_POINT ( 'NONE',  ( 5.729893540575130118, -2.074111880986319711, -0.9905765078317919636 ) ) ;
#20537 = CARTESIAN_POINT ( 'NONE',  ( 3.959670595502752022, -0.5440038360976228171, 1.779617975935204655 ) ) ;
#20536 = DIRECTION ( 'NONE',  ( 0.000000000000000000, -1.000000000000000000, 0.000000000000000000 ) ) ;
#20538 = CARTESIAN_POINT ( 'NONE',  ( 6.013923656113508542, 9.173938811177871244, -1.199719254218452047 ) ) ;
#20539 = CARTESIAN_POINT ( 'NONE',  ( -1.500000000000001110, 11.52083333333333393, 0.8660254037844418162 ) ) ;
#20540 = CARTESIAN_POINT ( 'NONE',  ( -6.449928391799210736, 8.548002428564306143, -1.599625672291263179 ) ) ;
#20541 = CARTESIAN_POINT ( 'NONE',  ( -3.038435823238377687, 6.558942537171132514, -0.7216878364870458196 ) ) ;
#20542 = CARTESIAN_POINT ( 'NONE',  ( 0.2401087780563165297, 2.186128513634697512, 0.1550312349237955856 ) ) ;
#20543 = CARTESIAN_POINT ( 'NONE',  ( 5.829642864196168617, 6.863966765392747860, 1.082531754730558626 ) ) ;
#20544 = ORIENTED_EDGE ( 'NONE', *, *, #60132, .F. ) ;
#20545 = CARTESIAN_POINT ( 'NONE',  ( 10.71948157449259043, -8.605866298767898215, -0.1871092468795605146 ) ) ;
#20546 = CARTESIAN_POINT ( 'NONE',  ( -6.636492533740866577E-13, -6.372041098632465150, -9.837588353259592466 ) ) ;
#20547 = CARTESIAN_POINT ( 'NONE',  ( 0.4338677482375961070, 0.9413943332680120291, -1.564114433284753636 ) ) ;
#20548 = CARTESIAN_POINT ( 'NONE',  ( -3.924195396151603177, 6.665646164563756138, 1.199719254218464037 ) ) ;
#20549 = CARTESIAN_POINT ( 'NONE',  ( 2.971044740931504613, -1.708945904174772989, -0.2933555621278273184 ) ) ;
#20550 = CARTESIAN_POINT ( 'NONE',  ( 6.609000000000047947, 2.072800852438889230, 2.208748404276588584 ) ) ;
#20551 = CARTESIAN_POINT ( 'NONE',  ( 3.840479349152599919, 7.346192795665340114, 0.4818892653144311033 ) ) ;
#20552 = CARTESIAN_POINT ( 'NONE',  ( 5.777927443424748510, 1.091106472389313131, 1.463626628978510702 ) ) ;
#20553 = CARTESIAN_POINT ( 'NONE',  ( 2.852341167582587378, -1.956174252073937359, -0.1491622203949396763 ) ) ;
#20554 = AXIS2_PLACEMENT_3D ( 'NONE', #197162, #210207, #180915 ) ;
#20555 = CARTESIAN_POINT ( 'NONE',  ( -1.352083138863443345E-14, -0.6249999993171989621, 1.414508159514555441 ) ) ;
#20556 = CARTESIAN_POINT ( 'NONE',  ( -9.528683032306089373, 10.01121838064558744, 0.7998128361456462443 ) ) ;
#20557 = CARTESIAN_POINT ( 'NONE',  ( 7.721532178182734185, 8.967207948423393304, 1.199719254218462483 ) ) ;
#20558 = AXIS2_PLACEMENT_3D ( 'NONE', #194790, #81046, #109361 ) ;
#20559 = CARTESIAN_POINT ( 'NONE',  ( 4.828832153679845973, 1.461785933843419150, -1.536352341152541046 ) ) ;
#20560 = CARTESIAN_POINT ( 'NONE',  ( 5.996449078994045223, 10.21788403546024782, 0.7998128361456331437 ) ) ;
#20561 = CARTESIAN_POINT ( 'NONE',  ( -10.63367255181986160, 11.30037282007833532, 1.040834085586084257E-14 ) ) ;
#20562 = CARTESIAN_POINT ( 'NONE',  ( 1.498975721005956219, 0.3999860688887920679, 2.031077231357696355 ) ) ;
#20564 = CARTESIAN_POINT ( 'NONE',  ( -1.402160292154681736E-14, -0.2406249996585799189, -1.575800808251665908 ) ) ;
#20563 = CARTESIAN_POINT ( 'NONE',  ( -11.97929049433705551, 11.37999999999999901, 0.7046979865771804130 ) ) ;
#20566 = ORIENTED_EDGE ( 'NONE', *, *, #140442, .F. ) ;
#20565 = CARTESIAN_POINT ( 'NONE',  ( 4.934350062338543452, -1.187533444586796438, -1.877053939226761115 ) ) ;
#20567 = CARTESIAN_POINT ( 'NONE',  ( 3.024404714233555946, -2.025920917938589749, 1.086156575756046294 ) ) ;
#20568 = CARTESIAN_POINT ( 'NONE',  ( 8.107412671292031803, 11.44210330227398487, 1.082531754730557072 ) ) ;
#20570 = CARTESIAN_POINT ( 'NONE',  ( 0.000000000000000000, -1.946874999522044014, -3.793834371823813001 ) ) ;
#20569 = CARTESIAN_POINT ( 'NONE',  ( 4.523580528814945545, 5.306540700819438960, 1.199719254218452047 ) ) ;
#20571 = DIRECTION ( 'NONE',  ( 0.000000000000000000, 0.000000000000000000, 1.000000000000000000 ) ) ;
#20572 = DIRECTION ( 'NONE',  ( 1.276756478318932585E-15, -1.000000000000000000, 1.665334536937738262E-16 ) ) ;
#20573 = CARTESIAN_POINT ( 'NONE',  ( -0.4356160240586506860, -9.063431457505064515, 9.626717610576623230 ) ) ;
#20574 = CARTESIAN_POINT ( 'NONE',  ( 3.076317393561965208, 0.8638369986560844316, 1.706277067364105893 ) ) ;
#20575 = CARTESIAN_POINT ( 'NONE',  ( -11.80248046418316044, 13.79999999999999893, -1.695421849633145017 ) ) ;
#20576 = CARTESIAN_POINT ( 'NONE',  ( 3.996854971928843092, 1.456802638785438475, -0.9229968019349673591 ) ) ;
#20577 = CARTESIAN_POINT ( 'NONE',  ( 3.292204118033771110, -0.8216723425069611952, -1.841733987974409237 ) ) ;
#20578 = CARTESIAN_POINT ( 'NONE',  ( 4.430533913404213209, -1.776825693393409455, -1.458421372522151538 ) ) ;
#20579 = DIRECTION ( 'NONE',  ( 0.000000000000000000, 7.254698431490414842E-17, -1.000000000000000000 ) ) ;
#20580 = CARTESIAN_POINT ( 'NONE',  ( 6.498663405296385420, -0.5599463640075187376, -2.030188946737851108 ) ) ;
#20581 = CARTESIAN_POINT ( 'NONE',  ( -5.397554552016258889, 7.390509292142662723, 1.443375672974058777 ) ) ;
#20582 = CARTESIAN_POINT ( 'NONE',  ( 4.340886628629798238, -1.540457278443696509, 0.8709714020649069743 ) ) ;
#20584 = CARTESIAN_POINT ( 'NONE',  ( 0.3754557147975129960, 2.136610487456944263, -0.8307393200860619942 ) ) ;
#20583 = CARTESIAN_POINT ( 'NONE',  ( 6.713222337422018349, 7.861122810861019161, -1.199719254218452047 ) ) ;
#20585 = CARTESIAN_POINT ( 'NONE',  ( 6.351489326974223637, 1.835832825663574752, -0.1405570519043483624 ) ) ;
#20586 = CARTESIAN_POINT ( 'NONE',  ( 0.5149768381150775509, 4.156357524118265090, -0.4000488691750970216 ) ) ;
#20587 = CARTESIAN_POINT ( 'NONE',  ( 5.718738293430368991, -0.05686238728638653983, 2.190873718245327506 ) ) ;
#20588 = CARTESIAN_POINT ( 'NONE',  ( -3.156015896931072540, 6.904045323053366268, 0.000000000000000000 ) ) ;
#20589 = CARTESIAN_POINT ( 'NONE',  ( -1.752700365193352367E-14, -0.2656249996585993145, 1.570758158831780271 ) ) ;
#20590 = CARTESIAN_POINT ( 'NONE',  ( -11.86145016429273014, 10.19999999999999929, -1.180000000000002158 ) ) ;
#20591 = CARTESIAN_POINT ( 'NONE',  ( 0.2390591215055883068, -2.106223889411312999, -0.5266447289704286883 ) ) ;
#20592 = CARTESIAN_POINT ( 'NONE',  ( 1.428923106112218067, -1.700960256238340573, 1.082842518468102089 ) ) ;
#20593 = CARTESIAN_POINT ( 'NONE',  ( -1.001543065824772872E-14, 5.321875000341422357, 1.575800808251672791 ) ) ;
#20594 = CARTESIAN_POINT ( 'NONE',  ( 4.512281715141372551, -0.8252044610495885557, -1.740951444232276657 ) ) ;
#20595 = CARTESIAN_POINT ( 'NONE',  ( -1.364683531250010295, 12.13020833367473017, 0.7879004041258445001 ) ) ;
#20596 = CARTESIAN_POINT ( 'NONE',  ( 0.9146621208586953600, -2.221583675102642097, 0.007239306818007660779 ) ) ;
#20598 = ORIENTED_EDGE ( 'NONE', *, *, #27948, .T. ) ;
#20597 = DIRECTION ( 'NONE',  ( 0.000000000000000000, 8.546850786086437571E-32, 1.000000000000000000 ) ) ;
#20599 = CARTESIAN_POINT ( 'NONE',  ( -5.361443639997861332, 4.701392137926268866, 2.440314829665658714 ) ) ;
#20600 = CARTESIAN_POINT ( 'NONE',  ( 0.000000000000000000, 13.87999999999998302, 0.000000000000000000 ) ) ;
#20601 = CARTESIAN_POINT ( 'NONE',  ( 9.083072846151447166, 12.68433652289702884, 1.199719254218450271 ) ) ;
#20602 = LINE ( 'NONE', #185237, #101092 ) ;
#20603 = CARTESIAN_POINT ( 'NONE',  ( 3.861425177953237142, 7.342474422772079734, -0.7004879694037218218 ) ) ;
#20604 = CARTESIAN_POINT ( 'NONE',  ( 3.913389451132457619, -0.8987009378256786141, -1.490314472085547237 ) ) ;
#20605 = CARTESIAN_POINT ( 'NONE',  ( 1.890992312513404716, 0.1891058464698439912, 1.952711869325058691 ) ) ;
#20607 = CARTESIAN_POINT ( 'NONE',  ( 1.364683531249988535, 2.676041667008082214, 0.7879004041258500513 ) ) ;
#20606 = CARTESIAN_POINT ( 'NONE',  ( 5.606460214450851964, 6.499623990736163037, 1.199719254218462483 ) ) ;
#20608 = CARTESIAN_POINT ( 'NONE',  ( 10.53876547652418338, 11.18964789890005918, 0.7998128361456462443 ) ) ;
#20609 = CARTESIAN_POINT ( 'NONE',  ( 6.478960399985357554, 1.830089090633261417, 0.7073212282268787066 ) ) ;
#20610 = CARTESIAN_POINT ( 'NONE',  ( -9.006694118179950692, 9.402231314165087284, 1.040834085586084257E-14 ) ) ;
#20611 = CARTESIAN_POINT ( 'NONE',  ( -3.592547517496929466, 7.135129837147637488, -0.7216878364870257245 ) ) ;
#20612 = CARTESIAN_POINT ( 'NONE',  ( 5.120327457147888950, 1.987497208294352280, 0.3399611521368098854 ) ) ;
#20613 = CARTESIAN_POINT ( 'NONE',  ( 0.9192595896337816264, 2.091463038127399532, 0.8634530567685079205 ) ) ;
#20615 = ORIENTED_EDGE ( 'NONE', *, *, #24925, .T. ) ;
#20614 = CARTESIAN_POINT ( 'NONE',  ( -7.230575994789712801, 7.330093503543126054, 0.7998128361456341429 ) ) ;
#20616 = CARTESIAN_POINT ( 'NONE',  ( 0.7499999999999885647, -0.4854166659838468623, 1.299038105676657340 ) ) ;
#20617 = CARTESIAN_POINT ( 'NONE',  ( 1.299835797595794151, -1.870726058509405210, -0.005653028302576856845 ) ) ;
#20618 = CARTESIAN_POINT ( 'NONE',  ( 0.03525962724756306205, -1.394606873943932346, 1.030409205853829668 ) ) ;
#20619 = CARTESIAN_POINT ( 'NONE',  ( 3.755584314896889264, 2.174856280799509545, -0.2696606696684644700 ) ) ;
#20620 = CARTESIAN_POINT ( 'NONE',  ( 6.018676637735699941, 1.555688181992231245, -1.704518584337791021 ) ) ;
#20621 = CARTESIAN_POINT ( 'NONE',  ( 0.8837498274346058391, 1.383631269908250472, 1.527543229604712893 ) ) ;
#20622 = CARTESIAN_POINT ( 'NONE',  ( 3.538947879116743689, -1.471199320522957876, -1.267674678009507394 ) ) ;
#20623 = CARTESIAN_POINT ( 'NONE',  ( -3.836594282542926226, 5.499112634431936542, 1.443375672974064550 ) ) ;
#20624 = CARTESIAN_POINT ( 'NONE',  ( 5.958239543830242901, 0.7576973323653662939, 1.710380810381225691 ) ) ;
#20625 = EDGE_CURVE ( 'NONE', #119323, #138593, #180742, .T. ) ;
#20626 = CARTESIAN_POINT ( 'NONE',  ( 0.6801582343749831283, 1.057291667008075642, -1.178068619123862515 ) ) ;
#20627 = CARTESIAN_POINT ( 'NONE',  ( 4.131482539099665452, 0.5404898895830790861, 1.942541833525657680 ) ) ;
#20628 = CARTESIAN_POINT ( 'NONE',  ( -5.246642258364192735, 5.223430177620739023, 0.7216878364870317197 ) ) ;
#20629 = CARTESIAN_POINT ( 'NONE',  ( -6.469175572376043348, 7.576401584974034265, 1.199719254218452047 ) ) ;
#20630 = CARTESIAN_POINT ( 'NONE',  ( 8.748035429315576650, 11.22912730566677553, -1.599625672291255185 ) ) ;
#20632 = DIRECTION ( 'NONE',  ( 0.000000000000000000, 1.000000000000000000, 0.000000000000000000 ) ) ;
#20631 = CARTESIAN_POINT ( 'NONE',  ( 1.594096589105632011, -1.816728215151931058, -0.1805768397986490248 ) ) ;
#20633 = CARTESIAN_POINT ( 'NONE',  ( -4.447956913735107598, 7.346977611736363656, 1.199719254218452935 ) ) ;
#20634 = CARTESIAN_POINT ( 'NONE',  ( -1.138412281109779656E-15, -6.920331743278516967, -9.905860218026836250 ) ) ;
#20635 = CARTESIAN_POINT ( 'NONE',  ( -10.82994025801865590, 5.589394046361075397, 6.507174183487985708 ) ) ;
#20636 = EDGE_LOOP ( 'NONE', ( #39828, #2259, #46682, #114349 ) ) ;
#20637 = CARTESIAN_POINT ( 'NONE',  ( -6.089020385868867180, 7.236850217336030511, -1.082531754730549967 ) ) ;
#20638 = LINE ( 'NONE', #51035, #128922 ) ;
#20639 = CARTESIAN_POINT ( 'NONE',  ( -9.215791728987058562, 11.77484298861683598, -1.599625672291263179 ) ) ;
#20640 = CARTESIAN_POINT ( 'NONE',  ( 6.006511931541290927, -2.010153113457528118, -0.1956843118748711474 ) ) ;
#20642 = EDGE_LOOP ( 'NONE', ( #93306, #213462, #168074, #204382 ) ) ;
#20641 = CARTESIAN_POINT ( 'NONE',  ( 0.08289510313583270396, -1.381697626658566547, 1.608636130391014163 ) ) ;
#20643 = CARTESIAN_POINT ( 'NONE',  ( -6.936931872047518155, 8.122117267924091166, 1.199719254218452047 ) ) ;
#20644 = CARTESIAN_POINT ( 'NONE',  ( 4.873266149108180123, 7.772895376346490970, 1.199719254218462483 ) ) ;
#20645 = AXIS2_PLACEMENT_3D ( 'NONE', #208782, #174200, #126573 ) ;
#20646 = CARTESIAN_POINT ( 'NONE',  ( 5.770404196412942888, -1.309395467888567754, 1.591445708773833401 ) ) ;
#20647 = CARTESIAN_POINT ( 'NONE',  ( 4.412732527109735514, -1.242725882911545288, -1.587838301257207263 ) ) ;
#20648 = VERTEX_POINT ( 'NONE', #121412 ) ;
#20649 = CARTESIAN_POINT ( 'NONE',  ( -11.84668730067608422, 10.90000000000000036, -1.320000000000001616 ) ) ;
#20650 = CARTESIAN_POINT ( 'NONE',  ( 2.703961570921634028, 5.242040035128820108, -1.199719254218446718 ) ) ;
#20652 = ORIENTED_EDGE ( 'NONE', *, *, #148219, .T. ) ;
#20651 = CARTESIAN_POINT ( 'NONE',  ( -6.607619761813764647, 8.802252036906432764, 1.599625672291269396 ) ) ;
#20653 = CARTESIAN_POINT ( 'NONE',  ( 4.595450297557979624, 8.489593704440707711, 0.02661077391274621617 ) ) ;
#20654 = CARTESIAN_POINT ( 'NONE',  ( 4.147814418418220406, -0.1948115906579734602, -2.006652602119996853 ) ) ;
#20655 = CARTESIAN_POINT ( 'NONE',  ( 3.855264089065893351, 1.827008581971893530, -0.2271198879545410221 ) ) ;
#20656 = CARTESIAN_POINT ( 'NONE',  ( -0.001697653062873135657, 15.43814226012838375, 11.93887736635299213 ) ) ;
#20657 = CARTESIAN_POINT ( 'NONE',  ( 2.297912027771050081, 1.785232721601331507, 1.462330537539487496 ) ) ;
#20658 = CARTESIAN_POINT ( 'NONE',  ( 6.831329296439236032, 9.063246493969506545, -1.599625672291267398 ) ) ;
#20659 = CARTESIAN_POINT ( 'NONE',  ( 5.395850447034295172, -0.7835752172833524432, 2.014745138864987073 ) ) ;
#20660 = CARTESIAN_POINT ( 'NONE',  ( 6.774270308322468459, 11.05506579301824743, 0.7998128361456462443 ) ) ;
#20661 = CARTESIAN_POINT ( 'NONE',  ( -0.1294898018152357000, -0.0008549345193622873455, -1.926395771554180625 ) ) ;
#20662 = CARTESIAN_POINT ( 'NONE',  ( -6.410307701162927252, 6.373113827645189744, -0.7998128361456291469 ) ) ;
#20664 = EDGE_CURVE ( 'NONE', #143294, #38441, #64824, .T. ) ;
#20663 = AXIS2_PLACEMENT_3D ( 'NONE', #117657, #67729, #133880 ) ;
#20665 = CARTESIAN_POINT ( 'NONE',  ( 2.680843577923686105, 0.4731804818897447640, -0.1027188127693821618 ) ) ;
#20666 = CARTESIAN_POINT ( 'NONE',  ( -5.558479791478509568, 5.587240632920778438, 0.000000000000000000 ) ) ;
#20667 = CARTESIAN_POINT ( 'NONE',  ( 1.920565142479381038, 1.744437793965779582, 0.6759427408406930571 ) ) ;
#20668 =( BOUNDED_SURFACE ( )  B_SPLINE_SURFACE ( 3, 2, ( 
 ( #189811, #39301, #7850 ),
 ( #161322, #187671, #173604 ),
 ( #145104, #5694, #121708 ),
 ( #127847, #211108, #90204 ),
 ( #105396, #77924, #203907 ),
 ( #112632, #62733, #128893 ),
 ( #206056, #25176, #29184 ),
 ( #194874, #106489, #88053 ) ),
 .UNSPECIFIED., .F., .F., .T. ) 
 B_SPLINE_SURFACE_WITH_KNOTS ( ( 4, 2, 2, 4 ),
 ( 3, 3 ),
 ( 0.000000000000000000, 0.0005123566476021777739, 0.0007685349714032666067, 0.001024713295204355548 ),
 ( 0.000000000000000000, 1.000000000000000000 ),
 .UNSPECIFIED. ) 
 GEOMETRIC_REPRESENTATION_ITEM ( )  RATIONAL_B_SPLINE_SURFACE ( (
 ( 1.000000000000000000, 0.7100530722026823227, 1.000000000000000000),
 ( 1.000000000000000000, 0.7667719522827138867, 1.000000000000000000),
 ( 1.000000000000000000, 0.8160440554223366005, 1.000000000000000000),
 ( 1.000000000000000000, 0.8737249316769485352, 1.000000000000000000),
 ( 1.000000000000000000, 0.8903164784319946845, 1.000000000000000000),
 ( 1.000000000000000000, 0.9150853305241298807, 1.000000000000000000),
 ( 1.000000000000000000, 0.9227739504732653808, 1.000000000000000000),
 ( 1.000000000000000000, 0.9238795325112855172, 1.000000000000000000) ) ) 
 REPRESENTATION_ITEM ( '' )  SURFACE ( )  );
#20669 = CARTESIAN_POINT ( 'NONE',  ( 6.473508845062264427, 1.886732274579514756, -0.5718055884485659934 ) ) ;
#20671 = SURFACE_STYLE_USAGE ( .BOTH. , #3349 ) ;
#20670 = CARTESIAN_POINT ( 'NONE',  ( 1.499999999999985123, -0.6729166659838520248, -0.8660254037844323793 ) ) ;
#20672 = CARTESIAN_POINT ( 'NONE',  ( 1.190363680384380229, -0.9894552095768920363, 1.972713631218452557 ) ) ;
#20673 = ORIENTED_EDGE ( 'NONE', *, *, #99741, .F. ) ;
#20674 = LINE ( 'NONE', #66211, #64268 ) ;
#20675 = CARTESIAN_POINT ( 'NONE',  ( 2.869522067586683711, 6.499526178826442013, 0.7998128361456362523 ) ) ;
#20676 = CARTESIAN_POINT ( 'NONE',  ( -3.764360206088648297, 7.543504007078730922, -0.7998128361456281477 ) ) ;
#20677 = CARTESIAN_POINT ( 'NONE',  ( -7.968353659517141807, -5.197284395437294258, 7.583532603600725785 ) ) ;
#20678 = CARTESIAN_POINT ( 'NONE',  ( 5.717641559312711230, -1.923570962979544330, 0.4312651734501466994 ) ) ;
#20679 = CARTESIAN_POINT ( 'NONE',  ( 6.533790081910475500, -1.501629927769430273, -1.752384480091616847 ) ) ;
#20680 = CARTESIAN_POINT ( 'NONE',  ( 6.865680895677650497, -0.4029405758906497437, 1.823372528724865438 ) ) ;
#20681 = CARTESIAN_POINT ( 'NONE',  ( 3.942276525692486544, -1.021014944866809326, 1.792092113122957242 ) ) ;
#20682 = CARTESIAN_POINT ( 'NONE',  ( 4.338245966692901412, 8.005111361209628740, -0.7216878364870197293 ) ) ;
#20683 = CARTESIAN_POINT ( 'NONE',  ( 7.517069824134078537, 7.734612647770044092, 0.000000000000000000 ) ) ;
#20684 = ORIENTED_EDGE ( 'NONE', *, *, #145950, .T. ) ;
#20685 = CARTESIAN_POINT ( 'NONE',  ( 6.900736999231407154, 10.99468423250458038, -0.7216878364870267237 ) ) ;
#20686 = CARTESIAN_POINT ( 'NONE',  ( 1.364683531249990311, 3.696875000341416584, 1.214306433183764966E-14 ) ) ;
#20687 = CARTESIAN_POINT ( 'NONE',  ( -10.62808266865025608, 4.100636420088800804, -5.574739771788820519 ) ) ;
#20688 = CARTESIAN_POINT ( 'NONE',  ( 3.972175818679561043, 7.578029521860726092, -0.7216878364870197293 ) ) ;
#20689 = CARTESIAN_POINT ( 'NONE',  ( 6.021977204206338641, 2.140098014189107278, -0.3652067468529682226 ) ) ;
#20691 = CARTESIAN_POINT ( 'NONE',  ( 4.968220237687512864, -1.735557695065930606, -0.6152675618510683453 ) ) ;
#20690 = CARTESIAN_POINT ( 'NONE',  ( 9.855659161987905037, -6.334709917115484146, -0.4359479416626658166 ) ) ;
#20692 = CARTESIAN_POINT ( 'NONE',  ( 5.491164291198047387, 6.230432265623782939, -0.9768187426044780963 ) ) ;
#20693 = CARTESIAN_POINT ( 'NONE',  ( -11.92619526913699879, 12.69999999999999929, -1.328859060402686199 ) ) ;
#20694 = CARTESIAN_POINT ( 'NONE',  ( 0.4209003391736841349, -0.09842406703440903515, 1.868101828653282226 ) ) ;
#20695 = CARTESIAN_POINT ( 'NONE',  ( -4.232483270035822365, 7.525443216328503659, 1.020073867034466675 ) ) ;
#20696 = CARTESIAN_POINT ( 'NONE',  ( -10.88932262995847822, -6.511064858252409771, 0.06814526087293559797 ) ) ;
#20697 = CARTESIAN_POINT ( 'NONE',  ( 5.348589505275513467, 7.707351500233518671, -1.315919829448284784 ) ) ;
#20698 = CARTESIAN_POINT ( 'NONE',  ( 0.6801455168885979230, 0.9429141125626202546, 1.663586755705208420 ) ) ;
#20699 = CARTESIAN_POINT ( 'NONE',  ( 1.463349669262783870, 1.744408624272808073, -0.2979475530153224416 ) ) ;
#20700 = CARTESIAN_POINT ( 'NONE',  ( 6.111982388360997831, -0.6759622889470856544, 1.896349411511048855 ) ) ;
#20702 = CARTESIAN_POINT ( 'NONE',  ( 4.815990648786471873, 0.9809511849332609446, -1.645218558792021613 ) ) ;
#20701 = CARTESIAN_POINT ( 'NONE',  ( -9.989660255170729641, 10.54902514065433827, -0.7998128361456291469 ) ) ;
#20703 = CARTESIAN_POINT ( 'NONE',  ( -0.1409997244345879974, 2.021982482314553131, -2.415666835770650778 ) ) ;
#20704 = CARTESIAN_POINT ( 'NONE',  ( 4.949637397294944563, 1.457986120030363431, 1.324331637980098675 ) ) ;
#20705 = CARTESIAN_POINT ( 'NONE',  ( 6.117445925308827803, 1.681535965833020230, 1.118592408852390641 ) ) ;
#20706 = DIRECTION ( 'NONE',  ( -0.4243160830846597342, 0.9055141421511274658, 0.000000000000000000 ) ) ;
#20707 = CARTESIAN_POINT ( 'NONE',  ( 3.748781033766034998, -1.529746656882627454, 1.076398355447941491 ) ) ;
#20709 = EDGE_LOOP ( 'NONE', ( #207102, #57626 ) ) ;
#20708 = CARTESIAN_POINT ( 'NONE',  ( 5.725168984891365831, -0.03570264050535218447, 1.724697241110892509 ) ) ;
#20711 = CARTESIAN_POINT ( 'NONE',  ( 3.551873057100287223, 5.166937871415542283, 1.443375672974062551 ) ) ;
#20710 = CARTESIAN_POINT ( 'NONE',  ( 3.686314334879085663, -1.088174899301070253, 1.919869060924610293 ) ) ;
#20712 = STYLED_ITEM ( 'NONE', ( #207806 ), #160339 ) ;
#20713 = CARTESIAN_POINT ( 'NONE',  ( -1.201851678989727383E-14, 2.759375000341417916, -1.575800808251660134 ) ) ;
#20714 = CARTESIAN_POINT ( 'NONE',  ( 0.5903720789649337108, 1.061967407477812264, -1.768178413720230990 ) ) ;
#20715 = CARTESIAN_POINT ( 'NONE',  ( 5.601490020740366838, 9.686822124172440596, 1.040834085586084257E-14 ) ) ;
#20716 = CARTESIAN_POINT ( 'NONE',  ( -8.371269781434001800, 11.85389961405997816, -1.199719254218446718 ) ) ;
#20717 = CARTESIAN_POINT ( 'NONE',  ( -8.758160245763034979, 1.972237431423827347, -7.885882905893924821 ) ) ;
#20718 = CARTESIAN_POINT ( 'NONE',  ( -5.251085567194492043, 5.020688004682003047, -0.7998128361456221525 ) ) ;
#20719 = VERTEX_POINT ( 'NONE', #22730 ) ;
#20720 = CARTESIAN_POINT ( 'NONE',  ( 3.244645865714153032, -2.039272935636734285, -0.3565889006169955522 ) ) ;
#20721 = CARTESIAN_POINT ( 'NONE',  ( -0.7499999999999972244, 5.108333333333353821, -1.299038105676652011 ) ) ;
#20722 = CARTESIAN_POINT ( 'NONE',  ( 4.497554271431305040, 6.270232621468402989, -1.599625672291256295 ) ) ;
#20723 = CARTESIAN_POINT ( 'NONE',  ( -6.579637281422358264, 6.781222396613637571, 0.3437121870633503828 ) ) ;
#20724 = CARTESIAN_POINT ( 'NONE',  ( 1.277996545170931197, 1.989402420072207800, -0.3474319251903742467 ) ) ;
#20725 = FILL_AREA_STYLE_COLOUR ( '', #146345 ) ;
#20726 = EDGE_CURVE ( 'NONE', #23505, #163825, #26798, .T. ) ;
#20728 = CARTESIAN_POINT ( 'NONE',  ( 9.422553571817644524, 10.09532670998316384, 0.000000000000000000 ) ) ;
#20727 = CARTESIAN_POINT ( 'NONE',  ( 0.07479286986305544449, 2.888457405263197941, -2.344396930208477947 ) ) ;
#20729 = CARTESIAN_POINT ( 'NONE',  ( 6.327499943094792023, -1.427716970705223520, 1.423745300580002482 ) ) ;
#20730 = CARTESIAN_POINT ( 'NONE',  ( 5.383970194100923479, -1.915903400165029469, 0.006849619181082886032 ) ) ;
#20731 = CARTESIAN_POINT ( 'NONE',  ( 1.369155121446740960E-15, 19.00000000000000000, -11.18000000000000149 ) ) ;
#20732 = CARTESIAN_POINT ( 'NONE',  ( 4.124703146219878214, 0.1084699374758208573, 2.189010777610411740 ) ) ;
#20733 = CARTESIAN_POINT ( 'NONE',  ( 0.7499999999999902300, 3.847916667349481123, -1.299038105676658228 ) ) ;
#20734 = CARTESIAN_POINT ( 'NONE',  ( 2.074333847954575205, 0.8209984392052707136, 1.727357542596375861 ) ) ;
#20735 = CARTESIAN_POINT ( 'NONE',  ( -4.578903193113314174, 6.365139696764064325, 1.599625672291267398 ) ) ;
#20736 = CARTESIAN_POINT ( 'NONE',  ( 2.833290915131624566, 6.249330467721451399, -0.7216878364870267237 ) ) ;
#20738 = CARTESIAN_POINT ( 'NONE',  ( 1.317982704262925520, 0.9913799330133237220, -1.755781447868165257 ) ) ;
#20737 = FILL_AREA_STYLE_COLOUR ( '', #184176 ) ;
#20739 = CARTESIAN_POINT ( 'NONE',  ( -1.364683531250000748, 11.17187500034139802, 0.000000000000000000 ) ) ;
#20741 = CARTESIAN_POINT ( 'NONE',  ( -5.276058054373441664, 6.184431147304315424, -1.199719254218453823 ) ) ;
#20740 = CARTESIAN_POINT ( 'NONE',  ( 6.198795224570643470, 1.821041368708445907, 1.219022265761634971 ) ) ;
#20743 = ORIENTED_EDGE ( 'NONE', *, *, #110343, .T. ) ;
#20742 = CARTESIAN_POINT ( 'NONE',  ( 3.293694421395336303, -0.6999868571894217739, 1.576533365092074757 ) ) ;
#20744 = CARTESIAN_POINT ( 'NONE',  ( 0.1394461523056772234, 0.2496508530322391062, -1.754170159799403717 ) ) ;
#20745 = CARTESIAN_POINT ( 'NONE',  ( 6.988338112840064120, 10.24047933403371502, 1.199719254218460707 ) ) ;
#20746 = CARTESIAN_POINT ( 'NONE',  ( 4.527533231959700366, 7.369540306339926516, 1.199719254218462483 ) ) ;
#20747 = DIRECTION ( 'NONE',  ( 0.000000000000000000, 0.000000000000000000, 1.000000000000000000 ) ) ;
#20748 = CARTESIAN_POINT ( 'NONE',  ( 1.099968687278202406, 0.7983322178258808188, -1.792280776234013828 ) ) ;
#20749 = ADVANCED_FACE ( 'NONE', ( #63784 ), #9490, .T. ) ;
#20750 = CARTESIAN_POINT ( 'NONE',  ( 3.493197133815315603, 7.227147089426516402, -0.7998128361456291469 ) ) ;
#20751 = CARTESIAN_POINT ( 'NONE',  ( -2.788906526875773208E-15, 10.68750000000000000, -1.499999999999998446 ) ) ;
#20752 = ORIENTED_EDGE ( 'NONE', *, *, #159680, .F. ) ;
#20754 =( BOUNDED_SURFACE ( )  B_SPLINE_SURFACE ( 3, 2, ( 
 ( #24953, #121488, #91055 ),
 ( #56404, #4413, #72638 ),
 ( #54274, #187460, #39088 ),
 ( #70484, #154973, #136600 ),
 ( #40158, #156038, #106272 ),
 ( #172293, #23881, #7627 ) ),
 .UNSPECIFIED., .F., .F., .T. ) 
 B_SPLINE_SURFACE_WITH_KNOTS ( ( 4, 2, 4 ),
 ( 3, 3 ),
 ( 0.000000000000000000, 0.0003754691837024765901, 0.0007509383674049531802 ),
 ( 0.000000000000000000, 1.000000000000000000 ),
 .UNSPECIFIED. ) 
 GEOMETRIC_REPRESENTATION_ITEM ( )  RATIONAL_B_SPLINE_SURFACE ( (
 ( 1.000000000000000000, 0.6711954675835395401, 1.000000000000000000),
 ( 1.000000000000000000, 0.6709646295273183902, 1.000000000000000000),
 ( 1.000000000000000000, 0.6771840716651685854, 1.000000000000000000),
 ( 1.000000000000000000, 0.6927481755874828062, 1.000000000000000000),
 ( 1.000000000000000000, 0.7017972101304553734, 1.000000000000000000),
 ( 1.000000000000000000, 0.7071067811865399122, 1.000000000000000000) ) ) 
 REPRESENTATION_ITEM ( '' )  SURFACE ( )  );
#20753 = CARTESIAN_POINT ( 'NONE',  ( -2.331034670843834533E-15, -6.105866302529035394, 10.72111444838893135 ) ) ;
#20755 = PRESENTATION_LAYER_ASSIGNMENT (  '', '', ( #58814 ) ) ;
#20756 = ORIENTED_EDGE ( 'NONE', *, *, #151575, .F. ) ;
#20757 = CARTESIAN_POINT ( 'NONE',  ( 3.527799351415283002, -1.784095038623861651, 0.3127521441018704107 ) ) ;
#20758 = ORIENTED_EDGE ( 'NONE', *, *, #118802, .T. ) ;
#20759 = CARTESIAN_POINT ( 'NONE',  ( 9.728138913005292210, 11.30824913904973705, -1.199719254218440723 ) ) ;
#20760 = CARTESIAN_POINT ( 'NONE',  ( 3.410758162289653672, 6.136912401716668519, -1.199719254218453823 ) ) ;
#20761 = CARTESIAN_POINT ( 'NONE',  ( 4.670457322363490427, 0.6978976414240989357, 1.671844709466139722 ) ) ;
#20762 = CARTESIAN_POINT ( 'NONE',  ( 6.821160681006781523, 9.051383109298340557, 1.443375672974063439 ) ) ;
#20763 = CARTESIAN_POINT ( 'NONE',  ( -9.093502852636577316, 1.000000000000000888, -7.666967846417613863 ) ) ;
#20764 = CARTESIAN_POINT ( 'NONE',  ( 5.794097129154974546, 6.036864960932135205, -0.5213279746436976225 ) ) ;
#20766 = CARTESIAN_POINT ( 'NONE',  ( -1.402160292154681736E-14, 15.17187500034140157, 1.575800808251682339 ) ) ;
#20765 = CARTESIAN_POINT ( 'NONE',  ( 4.580409787399508659, 1.145788356511275863, -1.466404039444089591 ) ) ;
#20767 = CARTESIAN_POINT ( 'NONE',  ( 2.390125374076298659, -0.7353994070154221685, -1.769027144041198429 ) ) ;
#20768 = CARTESIAN_POINT ( 'NONE',  ( -5.775410249741537605, 5.840326167560951909, 0.7216878364870206175 ) ) ;
#20769 = FACE_OUTER_BOUND ( 'NONE', #70562, .T. ) ;
#20770 = CARTESIAN_POINT ( 'NONE',  ( 5.992340707560147806, 8.974519344586754599, 1.082531754730558626 ) ) ;
#20771 = EDGE_CURVE ( 'NONE', #106155, #173996, #152598, .T. ) ;
#20772 = CARTESIAN_POINT ( 'NONE',  ( -4.115063316947640715, 4.759660943649018705, 1.199719254218462483 ) ) ;
#20773 = CARTESIAN_POINT ( 'NONE',  ( -5.261446130555064826, 8.296048364692991228, 1.199719254218452935 ) ) ;
#20774 = CARTESIAN_POINT ( 'NONE',  ( 1.675843188381221038, -1.117204103763050016, 1.766894365349908069 ) ) ;
#20775 = CARTESIAN_POINT ( 'NONE',  ( 6.204791576909545192, 7.267953590263130259, -1.199719254218452047 ) ) ;
#20776 = CARTESIAN_POINT ( 'NONE',  ( 0.08272424614634911466, -0.1293432359340887239, -1.795996506534849324 ) ) ;
#20777 = CARTESIAN_POINT ( 'NONE',  ( -3.716906668440817185, 7.488141546489591072, 0.7998128361456341429 ) ) ;
#20778 = ADVANCED_FACE ( 'NONE', ( #112608 ), #44357, .F. ) ;
#20779 = CARTESIAN_POINT ( 'NONE',  ( 2.326929888710258965, -0.002694909042751796133, 1.825762228105472840 ) ) ;
#20780 = CARTESIAN_POINT ( 'NONE',  ( -4.222669843016490177, 3.519858668466411267, 2.499999999999998668 ) ) ;
#20781 = CARTESIAN_POINT ( 'NONE',  ( 2.091926199050548441, 1.179367891222588005, 1.505316542580182659 ) ) ;
#20782 = CARTESIAN_POINT ( 'NONE',  ( 1.363649640492822668, -0.4818474322187695780, 1.909556114072549882 ) ) ;
#20783 = CARTESIAN_POINT ( 'NONE',  ( 3.860829347334773232, 0.2347576860389360420, -1.927744540433872888 ) ) ;
#20784 = EDGE_LOOP ( 'NONE', ( #10984, #122377, #4421, #39009 ) ) ;
#20785 = CARTESIAN_POINT ( 'NONE',  ( -0.4000000000000080158, 4.050057683544674880, -0.8916696671246466810 ) ) ;
#20786 = CARTESIAN_POINT ( 'NONE',  ( -3.820365424000704557, 7.679119771301277098, -0.7998128361456481317 ) ) ;
#20788 = CARTESIAN_POINT ( 'NONE',  ( 3.972980863544761654, -1.569110274459505350, 1.426624754300914510 ) ) ;
#20787 = CARTESIAN_POINT ( 'NONE',  ( 4.598150373690133463, 5.393538853173795111, -1.199719254218452047 ) ) ;
#20789 = CARTESIAN_POINT ( 'NONE',  ( 6.400381488218092052, -6.708819892820498509, 7.008396152629734033 ) ) ;
#20790 = CARTESIAN_POINT ( 'NONE',  ( 7.750457368506414646, 12.19395069656619945, 0.7998128361456462443 ) ) ;
#20791 = CARTESIAN_POINT ( 'NONE',  ( 5.809489818682099127, 6.211223759639540987, 0.9523037572534819306 ) ) ;
#20792 =( LENGTH_UNIT ( ) NAMED_UNIT ( * ) SI_UNIT ( .MILLI., .METRE. ) );
#20793 = ORIENTED_EDGE ( 'NONE', *, *, #43786, .F. ) ;
#20794 = CARTESIAN_POINT ( 'NONE',  ( 5.742760583840166966, 8.857581893525663830, 1.199719254218452047 ) ) ;
#20795 = DIRECTION ( 'NONE',  ( 1.000000000000000000, -0.000000000000000000, -0.000000000000000000 ) ) ;
#20796 = CARTESIAN_POINT ( 'NONE',  ( 4.143042835627613663, -1.587387879459275286, 0.9017181768668989239 ) ) ;
#20797 = CARTESIAN_POINT ( 'NONE',  ( -8.694134400161971216E-15, 3.603753425775781505, -11.89624657422419673 ) ) ;
#20798 = CARTESIAN_POINT ( 'NONE',  ( -9.327646496521992958, 9.984601788804893019, -0.7216878364870267237 ) ) ;
#20799 = CARTESIAN_POINT ( 'NONE',  ( -4.636310691425048702, 8.434871236368708836, 0.4628797641644845084 ) ) ;
#20800 = CARTESIAN_POINT ( 'NONE',  ( 6.825879202496176745, -6.900108348306368988, -6.758184431511345736 ) ) ;
#20801 = CARTESIAN_POINT ( 'NONE',  ( 4.821099876132087125, -0.09137817997613774390, 1.868553921495450965 ) ) ;
#20802 = CARTESIAN_POINT ( 'NONE',  ( 7.507464373665139412, 9.781794407407920389, 1.599625672291281386 ) ) ;
#20803 = CARTESIAN_POINT ( 'NONE',  ( 2.613793455771874719, -1.905494007693061098, 0.2829725131217008527 ) ) ;
#20804 = CARTESIAN_POINT ( 'NONE',  ( 6.473494419632052299, -0.2434444386649399217, 1.946554233954982172 ) ) ;
#20805 = CARTESIAN_POINT ( 'NONE',  ( 3.517450787741589036, 6.191110788085444128, -1.199719254218446718 ) ) ;
#20806 = CARTESIAN_POINT ( 'NONE',  ( -1.402160292154681736E-14, 8.734375000341403350, 1.575800808251682339 ) ) ;
#20807 = CARTESIAN_POINT ( 'NONE',  ( -7.386494761346872551, 7.511998731193139989, -0.7998128361456291469 ) ) ;
#20808 = CARTESIAN_POINT ( 'NONE',  ( 3.310162060030825248, 7.013606170011280838, -0.7998128361456291469 ) ) ;
#20809 = AXIS2_PLACEMENT_3D ( 'NONE', #45714, #93400, #79258 ) ;
#20810 = CARTESIAN_POINT ( 'NONE',  ( -3.811250578772977349, 7.460559751961507224, -0.7216878364870458196 ) ) ;
#20811 = CARTESIAN_POINT ( 'NONE',  ( 0.8611331728165865229, -0.05642918589183294059, -2.116647836221299261 ) ) ;
#20812 = CARTESIAN_POINT ( 'NONE',  ( 10.53876547652418338, 11.18964789890005918, 0.7998128361456462443 ) ) ;
#20813 = DIRECTION ( 'NONE',  ( 0.000000000000000000, 1.000000000000000000, 0.000000000000000000 ) ) ;
#20814 = CARTESIAN_POINT ( 'NONE',  ( 6.332887962430945983, -1.963924782908726296, -0.6550794379977520343 ) ) ;
#20816 = CARTESIAN_POINT ( 'NONE',  ( 4.166517013042797757, 7.612504677086913141, -0.8493068020909979587 ) ) ;
#20815 = CARTESIAN_POINT ( 'NONE',  ( 0.5734669319550633748, -1.023298125840161887, 1.530493987491374330 ) ) ;
#20817 = CARTESIAN_POINT ( 'NONE',  ( 6.117888908451988073, 0.2214900195740623634, 2.288030219478351057 ) ) ;
#20818 = CARTESIAN_POINT ( 'NONE',  ( 4.514501963670558560, 8.210743357683563559, 1.040834085586084257E-14 ) ) ;
#20819 = CARTESIAN_POINT ( 'NONE',  ( 3.445180431648323882, 6.073108699348104267, 1.082531754730549078 ) ) ;
#20820 = CARTESIAN_POINT ( 'NONE',  ( 1.043418098205237676, -1.810020423698131653, -1.406424589915030943 ) ) ;
#20821 = CARTESIAN_POINT ( 'NONE',  ( 7.792125355486789751, -6.646943093533971947, -7.591565991045878370 ) ) ;
#20822 = CARTESIAN_POINT ( 'NONE',  ( -6.611536185319534908, 7.742488966741438716, 1.199719254218452047 ) ) ;
#20823 = CARTESIAN_POINT ( 'NONE',  ( 6.369087006730828726, 1.857646680926292815, -0.5659663566517159072 ) ) ;
#20824 = CARTESIAN_POINT ( 'NONE',  ( 8.148087131688683371, 10.52918762510205042, -1.443375672974063439 ) ) ;
#20825 = ORIENTED_EDGE ( 'NONE', *, *, #205051, .T. ) ;
#20826 = CARTESIAN_POINT ( 'NONE',  ( 6.064708884584704585, 0.6063723501847050334, 1.813766235492550560 ) ) ;
#20827 = CARTESIAN_POINT ( 'NONE',  ( 4.260029445439558415, 7.236136616047151193, -2.499999999999996891 ) ) ;
#20829 = DIRECTION ( 'NONE',  ( 0.000000000000000000, 0.000000000000000000, -1.000000000000000000 ) ) ;
#20828 = CARTESIAN_POINT ( 'NONE',  ( -8.853638004923878313, 10.28799807962136548, 1.199719254218462483 ) ) ;
#20830 = CARTESIAN_POINT ( 'NONE',  ( -10.44369227015510049, 5.112964020592959180, 5.232143560358710310 ) ) ;
#20832 = CARTESIAN_POINT ( 'NONE',  ( 1.586397006687990885, -0.2552452650203296813, -1.751205042619798258 ) ) ;
#20831 = CARTESIAN_POINT ( 'NONE',  ( 2.607466773009491146, -2.067780616408128935, 0.3074339443978144626 ) ) ;
#20833 = CARTESIAN_POINT ( 'NONE',  ( 0.07538891330674882263, -7.154544010627095219, -9.499700864329891914 ) ) ;
#20835 = CARTESIAN_POINT ( 'NONE',  ( 4.523529124507605914, -1.408076564469705527, -1.808723714663774240 ) ) ;
#20834 = CARTESIAN_POINT ( 'NONE',  ( 3.088225128862704949, 6.824956093640315302, 0.7998128361456281477 ) ) ;
#20836 = CARTESIAN_POINT ( 'NONE',  ( 3.556370828957751140, -1.535720284108733624, -0.8187001993567950553 ) ) ;
#20837 = CARTESIAN_POINT ( 'NONE',  ( 2.354312230267378236, 5.898448035287240820, -0.7998128361456281477 ) ) ;
#20838 = CARTESIAN_POINT ( 'NONE',  ( 4.766573523656222555, 7.718696989977711809, 1.199719254218452047 ) ) ;
#20839 = CARTESIAN_POINT ( 'NONE',  ( 3.092811855500672280, 0.9656183884470933565, -1.439801824928796048 ) ) ;
#20840 = CARTESIAN_POINT ( 'NONE',  ( 3.859984642892180684, -0.6334943099049659132, 2.076686793900458294 ) ) ;
#20841 = CARTESIAN_POINT ( 'NONE',  ( 4.473300617505036492, 7.306268922809479704, -1.199719254218452047 ) ) ;
#20842 = CARTESIAN_POINT ( 'NONE',  ( 4.716029918043215474, 1.032482702726954527, -1.731993998903176957 ) ) ;
#20843 = CARTESIAN_POINT ( 'NONE',  ( 1.750000000000001332, 1.008799782768345906E-13, 2.052068128417951165 ) ) ;
#20844 = CARTESIAN_POINT ( 'NONE',  ( -0.7499999999999972244, 3.389583334016149863, -1.299038105676652011 ) ) ;
#20845 = CARTESIAN_POINT ( 'NONE',  ( 2.028227463090884974, 1.110962183858194452, -1.573585318204050676 ) ) ;
#20846 = CARTESIAN_POINT ( 'NONE',  ( -1.364683531250014514, 15.33854166700806587, -0.7879004041258335089 ) ) ;
#20847 = CARTESIAN_POINT ( 'NONE',  ( 4.025785557498418044, -0.3775041287265075152, 2.188942893082143293 ) ) ;
#20848 = EDGE_LOOP ( 'NONE', ( #208730, #207265, #122997, #16586 ) ) ;
#20849 = CARTESIAN_POINT ( 'NONE',  ( -0.1106856583840696712, 2.878213433396461962, -2.485464591233726317 ) ) ;
#20850 = CARTESIAN_POINT ( 'NONE',  ( -1.500000000000013101, 1.379166666666689745, -0.8660254037844313801 ) ) ;
#20851 = CARTESIAN_POINT ( 'NONE',  ( 7.786460292950004636, 7.978625184730144149, 1.040834085586084257E-14 ) ) ;
#20852 = CARTESIAN_POINT ( 'NONE',  ( 5.463572716182834910, 5.476515711742504067, 0.7216878364870317197 ) ) ;
#20853 = CARTESIAN_POINT ( 'NONE',  ( -3.285556943749998737, -2.180208332855376518, 1.896917185911908721 ) ) ;
#20854 = CARTESIAN_POINT ( 'NONE',  ( 0.5400543498376106921, -2.107395444675621121, 0.7023712877645065245 ) ) ;
#20855 = CARTESIAN_POINT ( 'NONE',  ( 5.459412808053472510, 1.602871733476991079, 1.130958114227413436 ) ) ;
#20856 = CARTESIAN_POINT ( 'NONE',  ( 7.293923454472069245, 11.45340176361870199, 0.7216878364870438212 ) ) ;
#20857 = LINE ( 'NONE', #18734, #7536 ) ;
#20858 = CARTESIAN_POINT ( 'NONE',  ( 0.5269342146079664113, 2.068330297753611546, 0.6279826202375409228 ) ) ;
#20859 = CARTESIAN_POINT ( 'NONE',  ( 5.716698046817569434, 6.698511138489155137, -1.199719254218452047 ) ) ;
#20860 = CARTESIAN_POINT ( 'NONE',  ( -4.665414256878293031, 7.496714828783040296, -1.082531754730549967 ) ) ;
#20861 = CARTESIAN_POINT ( 'NONE',  ( 3.578633024105078331, 1.310608547571969540, -1.592757226543355165 ) ) ;
#20862 = CARTESIAN_POINT ( 'NONE',  ( -3.879604511804807032, 7.677955697080923514, 0.7998128361456341429 ) ) ;
#20863 = CARTESIAN_POINT ( 'NONE',  ( -0.7500000000000215383, 3.472916667349487785, 1.299038105676671107 ) ) ;
#20864 = CARTESIAN_POINT ( 'NONE',  ( -1.364683531249997417, 5.821875000341418804, 1.214306433183764966E-14 ) ) ;
#20865 = CARTESIAN_POINT ( 'NONE',  ( 5.272658424858247095, -1.760895560629770262, -0.6313210838888929644 ) ) ;
#20866 = CARTESIAN_POINT ( 'NONE',  ( 3.744493841719060967, 1.720499418279351822, -0.2165549783500023973 ) ) ;
#20867 = CARTESIAN_POINT ( 'NONE',  ( 3.807932448155851191, 1.227607710457185197, -1.234010206841095636 ) ) ;
#20868 = CARTESIAN_POINT ( 'NONE',  ( 0.9609334056123096657, -2.075215392668391168, -0.9741618742916816620 ) ) ;
#20869 = CARTESIAN_POINT ( 'NONE',  ( -0.6823417656250212460, 3.363541667008085323, 1.181850606188767472 ) ) ;
#20870 = CARTESIAN_POINT ( 'NONE',  ( 5.355056023315875713, 0.4066876561409601964, -2.050628154503638889 ) ) ;
#20871 = CARTESIAN_POINT ( 'NONE',  ( 6.281195871053392388, 1.340900550492612364, 1.404911987746715774 ) ) ;
#20872 = CARTESIAN_POINT ( 'NONE',  ( 0.000000000000000000, 0.000000000000000000, 0.000000000000000000 ) ) ;
#20873 = CARTESIAN_POINT ( 'NONE',  ( 1.318982659667154334, 0.9913977828604101372, -1.755770081111128977 ) ) ;
#20874 = CARTESIAN_POINT ( 'NONE',  ( 0.04132284026489921325, -1.696808583893465894, -1.386471574116483696 ) ) ;
#20875 = DIRECTION ( 'NONE',  ( 0.000000000000000000, 1.000000000000000000, 0.000000000000000000 ) ) ;
#20876 = CARTESIAN_POINT ( 'NONE',  ( -7.153898609505128015, 11.49796547773133604, 0.7998128361456481317 ) ) ;
#20877 = CARTESIAN_POINT ( 'NONE',  ( 6.331821432781979730, 7.345878745455822312, -1.199719254218445830 ) ) ;
#20878 = CARTESIAN_POINT ( 'NONE',  ( 2.350376503035214615, 0.9972050307137376723, -1.871358364749615033 ) ) ;
#20879 = CARTESIAN_POINT ( 'NONE',  ( -0.6823417656250246877, -0.9489583329919115684, 1.181850606188755259 ) ) ;
#20880 = CARTESIAN_POINT ( 'NONE',  ( 5.725187622324654946, -0.04035785615889506128, 1.825416780793003069 ) ) ;
#20881 = ORIENTED_EDGE ( 'NONE', *, *, #103751, .F. ) ;
#20882 = CARTESIAN_POINT ( 'NONE',  ( -6.038177310039794854, 8.137902509836795417, -1.599625672291271394 ) ) ;
#20883 = CARTESIAN_POINT ( 'NONE',  ( -3.469446951953614189E-15, 3.507114751586604129, 11.99288524841339054 ) ) ;
#20884 = CARTESIAN_POINT ( 'NONE',  ( 5.817857313595521163, 9.801600942587855414, -0.7216878364870458196 ) ) ;
#20885 = CARTESIAN_POINT ( 'NONE',  ( 3.130865767068502503, -4.306442547369423224, -1.507748171479097010 ) ) ;
#20886 = CARTESIAN_POINT ( 'NONE',  ( -7.369020184227459858, 8.555943955475521889, 1.199719254218450271 ) ) ;
#20887 = CARTESIAN_POINT ( 'NONE',  ( 2.179950100978587990, 1.979969115219997189, -0.3981650194792104025 ) ) ;
#20888 = CARTESIAN_POINT ( 'NONE',  ( 0.1125219251090440048, -0.9011682483198739657, -1.901734387108368063 ) ) ;
#20889 = ADVANCED_FACE ( 'NONE', ( #194853 ), #171337, .T. ) ;
#20890 = CARTESIAN_POINT ( 'NONE',  ( 8.530051201292206287, 13.10347683481629488, 0.000000000000000000 ) ) ;
#20891 = CARTESIAN_POINT ( 'NONE',  ( 4.188223417972539053, 0.9984873940180930552, -1.570204455898941420 ) ) ;
#20892 = CARTESIAN_POINT ( 'NONE',  ( 8.378048858240820351, 11.86180853700128601, -1.199719254218446718 ) ) ;
#20893 = DIRECTION ( 'NONE',  ( -0.000000000000000000, -1.000000000000000000, -0.000000000000000000 ) ) ;
#20894 = CARTESIAN_POINT ( 'NONE',  ( -4.172158584703340445, 5.890604320285754980, -1.599625672291256295 ) ) ;
#20895 = CARTESIAN_POINT ( 'NONE',  ( -7.483210719738908168, 10.81783070874899799, 1.199719254218453823 ) ) ;
#20896 = CARTESIAN_POINT ( 'NONE',  ( 4.846238042176662653, 1.821038859956089606, 0.1311717439725426648 ) ) ;
#20898 = CARTESIAN_POINT ( 'NONE',  ( -4.244195945626527688, 7.512047922924973697, -1.038054094898384294 ) ) ;
#20897 = CARTESIAN_POINT ( 'NONE',  ( -7.286581212701773502, 7.465709267765667789, 0.7998128361456341429 ) ) ;
#20899 = CARTESIAN_POINT ( 'NONE',  ( -1.402160292154681736E-14, -0.6781249996585819728, 1.575800808251672791 ) ) ;
#20900 = CARTESIAN_POINT ( 'NONE',  ( 2.125947893326819660, 0.3012468308378027371, -1.707275946889510676 ) ) ;
#20901 = CARTESIAN_POINT ( 'NONE',  ( 0.2513753182956691146, 0.6612109069651134208, 1.610038921780505339 ) ) ;
#20903 = CARTESIAN_POINT ( 'NONE',  ( 8.161645285746708112, 9.584636257201740506, -1.082531754730543083 ) ) ;
#20902 = CARTESIAN_POINT ( 'NONE',  ( 5.022255751415273473, -1.231121986244879452, -1.951710362602774307 ) ) ;
#20904 = CARTESIAN_POINT ( 'NONE',  ( 5.076602173674213070, 4.887400388900169368, 0.000000000000000000 ) ) ;
#20905 = CARTESIAN_POINT ( 'NONE',  ( 1.809912028077927282, -2.045576594096469414, 0.2490995888081939946 ) ) ;
#20906 = CARTESIAN_POINT ( 'NONE',  ( 4.632082037363250748, 8.555846143565791095, -0.7998128361456231517 ) ) ;
#20907 = EDGE_CURVE ( 'NONE', #77951, #55386, #170621, .T. ) ;
#20908 = EDGE_CURVE ( 'NONE', #30079, #175863, #158247, .T. ) ;
#20909 = CARTESIAN_POINT ( 'NONE',  ( 0.4388270972612972609, 1.158508728638860230, 1.649830871073371119 ) ) ;
#20910 = CARTESIAN_POINT ( 'NONE',  ( 8.946219267268480380, 14.55181358891489296, -7.930791147577251898 ) ) ;
#20911 = CARTESIAN_POINT ( 'NONE',  ( -7.045397100956844127, 8.248660034984974132, -1.199719254218452047 ) ) ;
#20912 = CARTESIAN_POINT ( 'NONE',  ( 6.491075539335432687, 1.626419376453295706, -0.9240138038444989377 ) ) ;
#20914 = CARTESIAN_POINT ( 'NONE',  ( -3.623772196602547346, 7.449761006003425834, 0.000000000000000000 ) ) ;
#20913 = CARTESIAN_POINT ( 'NONE',  ( 3.568532368641282648, 0.6928216322696268969, 1.782650395559831180 ) ) ;
#20915 = CARTESIAN_POINT ( 'NONE',  ( 4.688207069967821106, -1.042061291317699423, 1.945354640606362873 ) ) ;
#20916 = CARTESIAN_POINT ( 'NONE',  ( 1.224999999999979661, 1.437500000682781387, -2.602085213965210642E-14 ) ) ;
#20917 = CARTESIAN_POINT ( 'NONE',  ( -2.788906526875773208E-15, 10.68750000000000000, -1.499999999999998446 ) ) ;
#20918 = CARTESIAN_POINT ( 'NONE',  ( 3.404505970362959655, 6.986024375483197879, 0.7216878364870257245 ) ) ;
#20919 = CARTESIAN_POINT ( 'NONE',  ( -5.438229012412903352, 6.477593614970734492, -1.082531754730549967 ) ) ;
#20920 = CARTESIAN_POINT ( 'NONE',  ( 6.235037545507011281, 1.978399733989940401, 0.7636319146847592165 ) ) ;
#20921 = ORIENTED_EDGE ( 'NONE', *, *, #48897, .F. ) ;
#20922 = CARTESIAN_POINT ( 'NONE',  ( 3.645846906810937149, -1.745625206895658810, -1.509303248858377966 ) ) ;
#20923 = CARTESIAN_POINT ( 'NONE',  ( 4.105873170248697690, 0.6631157982108953908, -1.846516426336957784 ) ) ;
#20924 = CARTESIAN_POINT ( 'NONE',  ( -3.935609729716867289, 7.813571461303467913, 0.7998128361456350310 ) ) ;
#20925 = CARTESIAN_POINT ( 'NONE',  ( 0.3737810522974581717, -1.925036204310347943, 0.3769080146646397456 ) ) ;
#20926 = DIRECTION ( 'NONE',  ( 0.000000000000000000, 0.000000000000000000, -1.000000000000000000 ) ) ;
#20927 = EDGE_LOOP ( 'NONE', ( #137637, #58230, #5190, #199214 ) ) ;
#20928 = CARTESIAN_POINT ( 'NONE',  ( 5.647672796105281279, 1.985869605424210649, -0.3494789899042491932 ) ) ;
#20929 =( BOUNDED_CURVE ( )  B_SPLINE_CURVE ( 2, ( #186240, #72486, #183052, #20539, #21581, #201411, #118125, #70341, #38943 ),
 .UNSPECIFIED., .F., .T. ) 
 B_SPLINE_CURVE_WITH_KNOTS ( ( 3, 2, 2, 2, 3 ),
 ( 0.5625000000000000000, 0.5654761904761904656, 0.5714285714285713969, 0.5773809523809523281, 0.5803571428571429047 ),
 .UNSPECIFIED. ) 
 CURVE ( )  GEOMETRIC_REPRESENTATION_ITEM ( )  RATIONAL_B_SPLINE_CURVE ( ( 0.9330127018922194093, 0.9330127018922194093, 1.000000000000000000, 0.8660254037844387076, 1.000000000000000000, 0.8660254037844387076, 1.000000000000000000, 0.9330127018922180770, 0.9330127018922194093 ) ) 
 REPRESENTATION_ITEM ( '' )  );
#20930 = CARTESIAN_POINT ( 'NONE',  ( -9.332089804907933939, 9.781859615347734405, 1.040834085586084257E-14 ) ) ;
#20931 = FACE_OUTER_BOUND ( 'NONE', #23964, .T. ) ;
#20932 = CARTESIAN_POINT ( 'NONE',  ( 3.590846382830733763, 2.117060681034032221, 0.4805534470472500042 ) ) ;
#20933 = DIRECTION ( 'NONE',  ( 0.000000000000000000, 0.000000000000000000, 1.000000000000000000 ) ) ;
#20934 = CARTESIAN_POINT ( 'NONE',  ( 0.5980879788009090259, 1.428637019467562830, 1.567290143595565066 ) ) ;
#20935 = CARTESIAN_POINT ( 'NONE',  ( -1.201851678989727383E-14, 1.743750000682815493, 1.732050807568877637 ) ) ;
#20936 = CARTESIAN_POINT ( 'NONE',  ( 7.892817981449907982, 12.36003807833360391, 0.7998128361456462443 ) ) ;
#20937 = DIRECTION ( 'NONE',  ( -0.000000000000000000, -1.000000000000000000, -0.000000000000000000 ) ) ;
#20938 = CARTESIAN_POINT ( 'NONE',  ( 5.214490215732396017, 7.828485850976955263, 1.269369371331245500 ) ) ;
#20939 = ORIENTED_EDGE ( 'NONE', *, *, #137354, .T. ) ;
#20940 = CARTESIAN_POINT ( 'NONE',  ( 1.423197193765327384, -0.05341811584172677374, 2.060271317188705709 ) ) ;
#20942 = CARTESIAN_POINT ( 'NONE',  ( 0.4208425991348082040, 2.777615014373102653, 1.955394415493260984 ) ) ;
#20941 = CARTESIAN_POINT ( 'NONE',  ( -9.398826802771548472, 11.98838390803207865, -1.599625672291263179 ) ) ;
#20943 = CARTESIAN_POINT ( 'NONE',  ( -1.364683531250000748, 1.759375000341421913, 0.000000000000000000 ) ) ;
#20944 = DIRECTION ( 'NONE',  ( -1.000000000000000000, 7.771561172376097755E-16, 4.440892098500627148E-16 ) ) ;
#20945 = ORIENTED_EDGE ( 'NONE', *, *, #85279, .T. ) ;
#20946 = CARTESIAN_POINT ( 'NONE',  ( 4.705663775918221603, 1.419457463540532816, 1.281590252682027087 ) ) ;
#20947 = CARTESIAN_POINT ( 'NONE',  ( 7.374709211190586089, 7.568525266002632534, 0.000000000000000000 ) ) ;
#20948 = CARTESIAN_POINT ( 'NONE',  ( -9.978437869977950569, 11.70422760547153906, -1.082531754730539753 ) ) ;
#20949 = CARTESIAN_POINT ( 'NONE',  ( 0.3163054335677130680, -0.6107064426322272865, -1.705642966030767260 ) ) ;
#20951 = CARTESIAN_POINT ( 'NONE',  ( 0.8662487887013297083, -1.869732701101217476, -0.4164899194021577933 ) ) ;
#20950 = CARTESIAN_POINT ( 'NONE',  ( 7.553974597844359096, -6.709380320845432344, 7.821934338880126347 ) ) ;
#20952 = CARTESIAN_POINT ( 'NONE',  ( 2.418496320782090869, 0.8830982243829659240, 1.872697815963566992 ) ) ;
#20953 = CARTESIAN_POINT ( 'NONE',  ( -1.364683531250000748, -0.1781249996585798634, 0.000000000000000000 ) ) ;
#20954 = CARTESIAN_POINT ( 'NONE',  ( 0.09253734621218495660, -0.4319466259074012937, -1.930967020758065589 ) ) ;
#20955 = CARTESIAN_POINT ( 'NONE',  ( 3.105874302609371362, -1.823586186413633126, 0.09019715141062728536 ) ) ;
#20957 = CARTESIAN_POINT ( 'NONE',  ( 5.654245663017247736, 7.339362581565530341, 1.229167601055790815 ) ) ;
#20956 = CARTESIAN_POINT ( 'NONE',  ( 0.4347317753056179623, 1.181035649988096958, -1.982462206444644437 ) ) ;
#20958 = CARTESIAN_POINT ( 'NONE',  ( -0.6823417656250003738, 1.217708333674752286, -1.181850606188749264 ) ) ;
#20959 = CARTESIAN_POINT ( 'NONE',  ( 4.457523014600942801, 1.654850327679569633, 1.231099151980449724 ) ) ;
#20960 = CARTESIAN_POINT ( 'NONE',  ( -7.088215381846223906, 7.164006121775713609, 0.7998128361456341429 ) ) ;
#20961 = CARTESIAN_POINT ( 'NONE',  ( 6.414979237560321401, 10.63589287712906462, 1.040834085586084257E-14 ) ) ;
#20962 = CARTESIAN_POINT ( 'NONE',  ( 4.843287188579786573, 6.673587691474970107, -1.599625672291256517 ) ) ;
#20963 = AXIS2_PLACEMENT_3D ( 'NONE', #135698, #132530, #36038 ) ;
#20964 = CARTESIAN_POINT ( 'NONE',  ( 6.179819089730593795, 6.104210447640811665, 1.040834085586084257E-14 ) ) ;
#20966 = CARTESIAN_POINT ( 'NONE',  ( -1.201851678989727383E-14, 4.087500000000022560, -1.732050807568863648 ) ) ;
#20965 = CARTESIAN_POINT ( 'NONE',  ( 5.614326327132292072, -0.9438296153482359507, -1.882684210903639022 ) ) ;
#20967 = CARTESIAN_POINT ( 'NONE',  ( 6.338344951546218908, -1.110931056888088353, 1.746890944850580052 ) ) ;
#20968 = CARTESIAN_POINT ( 'NONE',  ( 0.6823417656249899377, 1.655208333674752730, 1.181850606188755259 ) ) ;
#20969 = CARTESIAN_POINT ( 'NONE',  ( 3.233815116076131257, -1.449111151313630996, -1.604113057997895053 ) ) ;
#20970 = CARTESIAN_POINT ( 'NONE',  ( 3.826823269871942657, 1.426704988148481901, -1.429811943454310397 ) ) ;
#20971 = CARTESIAN_POINT ( 'NONE',  ( 6.620655732516625314, 7.629137130509059617, 2.773739711112707340 ) ) ;
#20972 = ADVANCED_FACE ( 'NONE', ( #94186 ), #131138, .F. ) ;
#20975 = CARTESIAN_POINT ( 'NONE',  ( 4.677199807034550183, 8.400557508274889784, 1.040834085586084257E-14 ) ) ;
#20974 = CARTESIAN_POINT ( 'NONE',  ( 3.285556943750000514, -3.113541666188709645, 1.896917185911906500 ) ) ;
#20973 = CARTESIAN_POINT ( 'NONE',  ( 11.09999999999960529, -3.437048488108780511E-15, -0.2598076211376266764 ) ) ;
#20976 = CARTESIAN_POINT ( 'NONE',  ( -5.468734858265826837, 7.473552982767158070, 1.599625672291263179 ) ) ;
#20977 = CARTESIAN_POINT ( 'NONE',  ( 2.536342520008515233, 0.6839386381054488595, 1.897109991223707937 ) ) ;
#20978 = CARTESIAN_POINT ( 'NONE',  ( -7.503547950159405566, 10.84155747757291266, 1.199719254218453823 ) ) ;
#20980 = CARTESIAN_POINT ( 'NONE',  ( 1.817809523595309340, 0.8386016503486221074, 1.021477770318707234 ) ) ;
#20979 = CARTESIAN_POINT ( 'NONE',  ( -4.578903193113314174, 6.365139696764064325, 1.599625672291267398 ) ) ;
#20981 = CARTESIAN_POINT ( 'NONE',  ( -2.788906526875773208E-15, 12.68749999999999822, -1.499999999999998446 ) ) ;
#20982 = CARTESIAN_POINT ( 'NONE',  ( -1.126385703232235747, 3.299232110657536410, -0.7749999999999935829 ) ) ;
#20983 = CARTESIAN_POINT ( 'NONE',  ( -0.4019237886466871523, 13.19866454968462932, -1.499999999999998668 ) ) ;
#20985 = CARTESIAN_POINT ( 'NONE',  ( 4.253529916566947122, 1.955168710539030075, -0.4926619687581067497 ) ) ;
#20984 = CARTESIAN_POINT ( 'NONE',  ( -8.066738210006693777, 10.43428054980638997, 1.443375672974090751 ) ) ;
#20986 = CARTESIAN_POINT ( 'NONE',  ( -1.001543065824772872E-14, 4.712500000000017231, 1.732050807568877637 ) ) ;
#20987 = CARTESIAN_POINT ( 'NONE',  ( 0.6823417656249934904, 15.00520833367473195, 1.181850606188764807 ) ) ;
#20988 = CARTESIAN_POINT ( 'NONE',  ( 6.440463960111763697, 1.706863596762456581, 0.2470990609701722573 ) ) ;
#20989 = CARTESIAN_POINT ( 'NONE',  ( 6.249382461256315580, 6.255644057745969988, -0.7998128361456481317 ) ) ;
#20991 = CARTESIAN_POINT ( 'NONE',  ( -6.120066830577914452, 5.977401641919705355, -0.003186534051367873044 ) ) ;
#20990 = CARTESIAN_POINT ( 'NONE',  ( 7.768458830950378591, 12.00702636951006497, 1.040834085586084257E-14 ) ) ;
#20992 = AXIS2_PLACEMENT_3D ( 'NONE', #108520, #208069, #209127 ) ;
#20993 = DIRECTION ( 'NONE',  ( -0.000000000000000000, 1.000000000000000000, -0.000000000000000000 ) ) ;
#20994 = CARTESIAN_POINT ( 'NONE',  ( 5.378141472655761923, -1.040010688794581029, 1.554561134376866161 ) ) ;
#20995 = CARTESIAN_POINT ( 'NONE',  ( -0.1106856583841060310, -0.002128758811529348188, -1.996853503091333470 ) ) ;
#20996 = PLANE ( 'NONE',  #206305 ) ;
#20997 = CARTESIAN_POINT ( 'NONE',  ( -9.604686356149274573, 4.518459255872632419, 7.193747284969079558 ) ) ;
#20998 = ORIENTED_EDGE ( 'NONE', *, *, #188915, .T. ) ;
#20999 = CARTESIAN_POINT ( 'NONE',  ( 1.019157904985489305, -1.821734318179563106, 0.8647433871810316086 ) ) ;
#21000 = CARTESIAN_POINT ( 'NONE',  ( 0.9139796618767962455, -1.811767225755844146, 0.001225010880583424656 ) ) ;
#21001 = CARTESIAN_POINT ( 'NONE',  ( 4.380693030546913391, 7.164540064729805202, 1.082531754730549078 ) ) ;
#21002 = LINE ( 'NONE', #120750, #100658 ) ;
#21003 = CARTESIAN_POINT ( 'NONE',  ( 8.229436053370669413, 10.62409470039771442, 1.443375672974076540 ) ) ;
#21004 = CARTESIAN_POINT ( 'NONE',  ( 7.786460292950004636, 7.978625184730144149, 1.040834085586084257E-14 ) ) ;
#21006 = CARTESIAN_POINT ( 'NONE',  ( 6.257445408045815505, 1.831477697454777953, -0.5614084181123339956 ) ) ;
#21005 = CARTESIAN_POINT ( 'NONE',  ( -5.229694566569281555, 7.124396299129368337, 1.599625672291267398 ) ) ;
#21007 = CARTESIAN_POINT ( 'NONE',  ( -8.014278199453791274, 8.522615118883788199, 1.530808498934192557E-16 ) ) ;
#21008 = CARTESIAN_POINT ( 'NONE',  ( -1.402160292154681736E-14, -0.6156249996585817508, 1.575800808251672791 ) ) ;
#21010 = EDGE_LOOP ( 'NONE', ( #139408, #208304, #1303, #139435 ) ) ;
#21009 = CARTESIAN_POINT ( 'NONE',  ( 2.575685996916329046, 5.948791396470269888, 0.7216878364870438212 ) ) ;
#21011 = CARTESIAN_POINT ( 'NONE',  ( -2.435661151949389147, 5.993355110582911038, 0.7998128361456341429 ) ) ;
#21012 = ADVANCED_FACE ( 'NONE', ( #114736 ), #98425, .F. ) ;
#21013 = CARTESIAN_POINT ( 'NONE',  ( 3.063507763784904192, 0.3185916186679502715, -2.137983152197140413 ) ) ;
#21014 = CARTESIAN_POINT ( 'NONE',  ( -6.699137298928187434, 8.909022496873262753, 1.443375672974064550 ) ) ;
#21015 = CARTESIAN_POINT ( 'NONE',  ( 6.129694847154206983, 8.244672969803623630, -1.443375672974078761 ) ) ;
#21016 = CARTESIAN_POINT ( 'NONE',  ( 0.4223351350958382544, -2.109807164369668087, 0.2139620856976830465 ) ) ;
#21017 = EDGE_CURVE ( 'NONE', #22696, #198538, #31552, .T. ) ;
#21018 = CARTESIAN_POINT ( 'NONE',  ( 6.229513028222847026, -1.717969363144413952, 0.6179237509907066217 ) ) ;
#21019 = CARTESIAN_POINT ( 'NONE',  ( 1.950399328871486704, 0.6145138020485548802, 1.873222726689319106 ) ) ;
#21020 = CARTESIAN_POINT ( 'NONE',  ( 4.429883728109570207, -1.874397765517330061, 0.3784635845696313061 ) ) ;
#21021 = ORIENTED_EDGE ( 'NONE', *, *, #149834, .F. ) ;
#21023 = ADVANCED_FACE ( 'NONE', ( #66953 ), #200157, .T. ) ;
#21022 = CARTESIAN_POINT ( 'NONE',  ( 9.500385102287568273, -7.162053774861992572, -0.01083140255524948393 ) ) ;
#21024 = CARTESIAN_POINT ( 'NONE',  ( 6.232857221494619182, -1.869652508273983882, -0.6194465747909986275 ) ) ;
#21025 = CARTESIAN_POINT ( 'NONE',  ( 0.5330192132981932396, -1.372706249750287322, -1.373872859839823990 ) ) ;
#21026 = ORIENTED_EDGE ( 'NONE', *, *, #20473, .F. ) ;
#21027 = CARTESIAN_POINT ( 'NONE',  ( -5.418418667316934112, 6.350518529071726981, -1.199719254218453823 ) ) ;
#21028 = CARTESIAN_POINT ( 'NONE',  ( -3.135678666510573365, 6.880318554229450712, 0.000000000000000000 ) ) ;
#21030 = CARTESIAN_POINT ( 'NONE',  ( 5.763624699140868834, 7.817591130454727200, -1.443375672974078761 ) ) ;
#21029 = CARTESIAN_POINT ( 'NONE',  ( 8.015895134177609904, 10.37496362800581018, 1.599625672291281386 ) ) ;
#21032 = ORIENTED_EDGE ( 'NONE', *, *, #189421, .F. ) ;
#21031 = CARTESIAN_POINT ( 'NONE',  ( 5.092401474535850348, -1.059014397921493433, 1.592059587274458510 ) ) ;
#21033 = CARTESIAN_POINT ( 'NONE',  ( 0.9036964725192305758, 1.805054822729842190, 1.269220749904229839 ) ) ;
#21034 = CARTESIAN_POINT ( 'NONE',  ( 0.3405876332337732237, 3.079852035184926784, -0.4461735512528454684 ) ) ;
#21035 = CARTESIAN_POINT ( 'NONE',  ( -0.02298948590537253436, -1.708053232816408196, -0.8599758793098393195 ) ) ;
#21036 = CARTESIAN_POINT ( 'NONE',  ( -1.500000000000015099, 8.729166666666664298, -0.8660254037844309360 ) ) ;
#21038 = CARTESIAN_POINT ( 'NONE',  ( -4.623560037311160720, 8.450214339770131033, 0.4765305399337668169 ) ) ;
#21037 = PRODUCT_DEFINITION_FORMATION_WITH_SPECIFIED_SOURCE ( 'ANY', '', #74733, .NOT_KNOWN. ) ;
#21039 = CARTESIAN_POINT ( 'NONE',  ( -6.558483974469827338, -6.776276029125435585, -6.864213375409891071 ) ) ;
#21040 = CARTESIAN_POINT ( 'NONE',  ( 2.647004975520852454, -0.3514972095969396970, -2.040143077068845123 ) ) ;
#21041 = CARTESIAN_POINT ( 'NONE',  ( -5.656776405399756236, 7.622658444431597680, -1.599625672291256295 ) ) ;
#21042 = AXIS2_PLACEMENT_3D ( 'NONE', #185030, #52913, #68064 ) ;
#21043 = CARTESIAN_POINT ( 'NONE',  ( -4.617805310829839804, 8.366410568267871994, -0.2388493967704352627 ) ) ;
#21045 = CARTESIAN_POINT ( 'NONE',  ( 0.3214396764580421118, -0.1044536432763705502, 2.159311484102262479 ) ) ;
#21044 = CARTESIAN_POINT ( 'NONE',  ( -4.548924232584923288, 5.265832011892554121, -1.199719254218446718 ) ) ;
#21046 = FACE_OUTER_BOUND ( 'NONE', #168599, .T. ) ;
#21047 = CARTESIAN_POINT ( 'NONE',  ( 0.05436647835300240789, -9.474608021433732929, 9.500000000000147438 ) ) ;
#21048 = CARTESIAN_POINT ( 'NONE',  ( 1.364683531249997417, 13.04687500034139980, 2.602085213965210642E-15 ) ) ;
#21050 = CARTESIAN_POINT ( 'NONE',  ( -6.306477729012051725, 7.386587434382707151, 1.199719254218452047 ) ) ;
#21049 = DIRECTION ( 'NONE',  ( 0.000000000000000000, 1.000000000000000000, 0.000000000000000000 ) ) ;
#21051 = CARTESIAN_POINT ( 'NONE',  ( 5.924387396467542644, -1.262448726827345435, -1.189203582418095761 ) ) ;
#21052 = EDGE_CURVE ( 'NONE', #12842, #65209, #3014, .T. ) ;
#21053 = CARTESIAN_POINT ( 'NONE',  ( -4.925689880466507908, 4.641059703499347044, -0.7998128361456221525 ) ) ;
#21054 = CARTESIAN_POINT ( 'NONE',  ( 3.766520095694513959, -0.8345382577515870759, -1.894767260282135712 ) ) ;
#21055 = CARTESIAN_POINT ( 'NONE',  ( 4.587589571003643840, -0.5631140419127963481, 2.040926637660822163 ) ) ;
#21056 = CARTESIAN_POINT ( 'NONE',  ( 7.775764792637399836, 9.030479331953833011, -1.199719254218441611 ) ) ;
#21057 = CARTESIAN_POINT ( 'NONE',  ( -1.364683531250010740, 4.780208333674755394, 0.7879004041258379498 ) ) ;
#21058 = CARTESIAN_POINT ( 'NONE',  ( 2.483201282919132336, -0.004963586128624993335, 1.969629312250702036 ) ) ;
#21059 = CARTESIAN_POINT ( 'NONE',  ( 0.6153073421325053749, 1.564839666810373231, 1.099065937236625157 ) ) ;
#21060 = CARTESIAN_POINT ( 'NONE',  ( 4.576316751016760165, -2.222806176453680393, -0.5595744876762742681 ) ) ;
#21061 = CARTESIAN_POINT ( 'NONE',  ( 2.666400811807769777, -1.259032629953384719, 1.322343945743660543 ) ) ;
#21062 = CARTESIAN_POINT ( 'NONE',  ( 6.540882763950133238, 6.595727744222092959, 0.000000000000000000 ) ) ;
#21063 = CARTESIAN_POINT ( 'NONE',  ( 5.843201017365476702, 6.879784610756938257, -1.082531754730543083 ) ) ;
#21064 = CARTESIAN_POINT ( 'NONE',  ( -6.344325816190970357, 9.489131654609717970, 1.199719254218452047 ) ) ;
#21065 = CARTESIAN_POINT ( 'NONE',  ( 3.902593620319398937, -1.991888969257959774, -0.2912845021679384971 ) ) ;
#21066 = CARTESIAN_POINT ( 'NONE',  ( 3.731260466781026963, 0.05263058604075031982, -1.961233346245725429 ) ) ;
#21067 = CARTESIAN_POINT ( 'NONE',  ( -6.669721502918952716, 9.868759955792373972, 1.199719254218452047 ) ) ;
#21068 = CARTESIAN_POINT ( 'NONE',  ( -6.247609857798938293, 6.183299677053865295, -0.7998128361456291469 ) ) ;
#21069 = CARTESIAN_POINT ( 'NONE',  ( 0.07556134207192373442, 6.947017789483680872, -2.839293120204011256 ) ) ;
#21071 = CARTESIAN_POINT ( 'NONE',  ( 4.117836676938036788, -0.9100935957705791335, -1.517748890920249671 ) ) ;
#21070 = CARTESIAN_POINT ( 'NONE',  ( 6.281206920390010495, 1.440802673026912117, 1.515107276980606654 ) ) ;
#21072 = CARTESIAN_POINT ( 'NONE',  ( 0.3401085955914601722, 2.185883683461706362, 0.1570275565265024931 ) ) ;
#21073 = CARTESIAN_POINT ( 'NONE',  ( -0.05959145049940026140, -1.342969899416647905, -1.106900597494438143 ) ) ;
#21074 = CARTESIAN_POINT ( 'NONE',  ( 7.949158136313996259, 8.168439335321471262, 1.040834085586084257E-14 ) ) ;
#21075 = DIRECTION ( 'NONE',  ( -0.6507913734559658270, -0.7592566023652989049, 0.000000000000000000 ) ) ;
#21076 = CARTESIAN_POINT ( 'NONE',  ( 0.3514386742532841779, -1.080868183629126067, 2.028406642177064345 ) ) ;
#21077 = CARTESIAN_POINT ( 'NONE',  ( 0.08191350661116909848, -1.027414926483052326, 1.935800647029708443 ) ) ;
#21078 = CARTESIAN_POINT ( 'NONE',  ( 6.555961055344926791, 1.506409351870329649, -0.8582156258899288348 ) ) ;
#21079 = CARTESIAN_POINT ( 'NONE',  ( 3.246891520140795517, 0.5363302883765566076, 2.140594385818309409 ) ) ;
#21080 = CARTESIAN_POINT ( 'NONE',  ( 0.6026744816367580748, 2.165159614417012879, 0.1613400170472640283 ) ) ;
#21081 = DIRECTION ( 'NONE',  ( 0.000000000000000000, -1.000000000000000000, 0.000000000000000000 ) ) ;
#21082 = CARTESIAN_POINT ( 'NONE',  ( 1.569685796324036264, 1.464237652897076414, 1.529633472619792656 ) ) ;
#21083 = CARTESIAN_POINT ( 'NONE',  ( 3.125000000000001776, -2.052068128417947168, 1.787079010424618414E-13 ) ) ;
#21084 = CARTESIAN_POINT ( 'NONE',  ( 6.727182134110193168, 3.677753830905213128, 2.802861976130672783 ) ) ;
#21085 = CARTESIAN_POINT ( 'NONE',  ( 5.333004766823168374, 0.1418691241366967226, 1.921211455432366044 ) ) ;
#21086 = VERTEX_POINT ( 'NONE', #69095 ) ;
#21088 = CARTESIAN_POINT ( 'NONE',  ( -1.364683531250014514, -1.157291666325248158, 0.7879004041258379498 ) ) ;
#21087 = CARTESIAN_POINT ( 'NONE',  ( 1.681587762198969216, 1.584507396495305587, 1.656812167128306035 ) ) ;
#21089 = CARTESIAN_POINT ( 'NONE',  ( 3.497113557321089861, 6.167384019261527683, -1.199719254218446718 ) ) ;
#21090 = CARTESIAN_POINT ( 'NONE',  ( 5.738125327081736060, 7.717565519727259904, 1.599625672291267398 ) ) ;
#21091 = CARTESIAN_POINT ( 'NONE',  ( 3.545754021904829134, -2.051903114543842666, 0.8512574589945339776 ) ) ;
#21092 = CARTESIAN_POINT ( 'NONE',  ( -8.405692050792730186, 9.869357483088723626, 1.082531754730558626 ) ) ;
#21093 = FILL_AREA_STYLE ('',( #135958 ) ) ;
#21094 = CARTESIAN_POINT ( 'NONE',  ( 6.832946231607457399, 7.074118146404578589, -0.7216878364870257245 ) ) ;
#21095 = CARTESIAN_POINT ( 'NONE',  ( -7.822691444960700125, 11.10992853822074444, -1.082531754730543083 ) ) ;
#21096 = VECTOR ( 'NONE', #76115, 1000.000000000000000 ) ;
#21097 = CARTESIAN_POINT ( 'NONE',  ( 6.102578539926878598, 7.252668063737060855, -1.082531754730548412 ) ) ;
#21098 = CARTESIAN_POINT ( 'NONE',  ( 2.110000207431836472, 0.002812218110825881467, 2.016597019944998959 ) ) ;
#21100 = CARTESIAN_POINT ( 'NONE',  ( 6.672339319202143848, -0.9689918024566068766, -1.820889590527257740 ) ) ;
#21099 = CARTESIAN_POINT ( 'NONE',  ( 9.074484886248265880, 9.481320543578137361, 0.7998128361456462443 ) ) ;
#21101 = CARTESIAN_POINT ( 'NONE',  ( 6.712695452097489301, 7.964471127936110229, -1.082531754730548412 ) ) ;
#21102 = CARTESIAN_POINT ( 'NONE',  ( 6.497592319816168249, -1.739837010378456617, 0.05289828334312414448 ) ) ;
#21103 = DIRECTION ( 'NONE',  ( 1.000000000000000000, 0.000000000000000000, -0.000000000000000000 ) ) ;
#21104 = CARTESIAN_POINT ( 'NONE',  ( -1.402160292154681736E-14, 2.196875000341423689, -1.575800808251660134 ) ) ;
#21105 = CARTESIAN_POINT ( 'NONE',  ( 2.899370140885823233, -0.5591585085688542955, 1.679125488999051452 ) ) ;
#21106 = CARTESIAN_POINT ( 'NONE',  ( 1.477185633673218534, -2.006960102380969779, -0.1948397147320118372 ) ) ;
#21107 = CARTESIAN_POINT ( 'NONE',  ( 6.515217664332146441, -1.685650512211306129, 0.4329046258050253670 ) ) ;
#21108 = CARTESIAN_POINT ( 'NONE',  ( 4.968466765020612463, -2.157917790226408172, -0.7739415147586664601 ) ) ;
#21109 = CARTESIAN_POINT ( 'NONE',  ( 3.573999110145977820, -1.774750109099573869, -0.4897004633943187191 ) ) ;
#21110 = CARTESIAN_POINT ( 'NONE',  ( 8.178592977541601527, 10.56477777859713463, 1.599625672291281386 ) ) ;
#21111 = CARTESIAN_POINT ( 'NONE',  ( 4.541915102786819425, 0.7800907816924649296, -1.650662693317282770 ) ) ;
#21112 = CARTESIAN_POINT ( 'NONE',  ( 4.992814645674492624, -2.006446365708704160, 0.2004330516618065550 ) ) ;
#21113 = CARTESIAN_POINT ( 'NONE',  ( -6.991200766141138168, 11.30815132714001159, 0.7998128361456481317 ) ) ;
#21115 = CARTESIAN_POINT ( 'NONE',  ( -7.605197822622922210, 7.837428646007010613, -0.7998128361456362523 ) ) ;
#21114 = CARTESIAN_POINT ( 'NONE',  ( 3.063607368349754889, 0.3334396122402134011, -2.237705976790417939 ) ) ;
#21116 = CARTESIAN_POINT ( 'NONE',  ( 6.264693295067493395, -1.491911088229242788, 1.486630704232002609 ) ) ;
#21117 = CARTESIAN_POINT ( 'NONE',  ( -0.4634916963857253491, 7.369626292149035862, -4.459501722865316431 ) ) ;
#21118 = CARTESIAN_POINT ( 'NONE',  ( 3.139188941651628539, -0.1496422021231707811, -2.064996656166856237 ) ) ;
#21119 = CARTESIAN_POINT ( 'NONE',  ( 9.459838494033030898, 12.05956421450382088, 1.599625672291281386 ) ) ;
#21120 = CARTESIAN_POINT ( 'NONE',  ( 1.360316468749992236, 1.546875000341396689, -1.040834085586084257E-14 ) ) ;
#21121 = CARTESIAN_POINT ( 'NONE',  ( 5.953796468794862129, -1.535729488331440074, -1.462440914314271811 ) ) ;
#21122 = APPLICATION_PROTOCOL_DEFINITION ( 'draft international standard', 'automotive_design', 1998, #29814 ) ;
#21124 = CARTESIAN_POINT ( 'NONE',  ( 1.717283182695702015, -0.2364092415704423800, 1.911874917900743931 ) ) ;
#21123 = CARTESIAN_POINT ( 'NONE',  ( -10.00321840878439339, 10.56484298653695397, 1.040834085586084257E-14 ) ) ;
#21125 = UNCERTAINTY_MEASURE_WITH_UNIT (LENGTH_MEASURE( 1.000000000000000082E-05 ), #138828, 'distance_accuracy_value', 'NONE');
#21126 = CARTESIAN_POINT ( 'NONE',  ( -10.62873463776380056, 11.29999999999998117, 3.199999999999997957 ) ) ;
#21127 = B_SPLINE_CURVE_WITH_KNOTS ( 'NONE', 3,
 ( #86496, #55071, #70218, #5209, #100609, #69150, #199151, #187189, #119059, #151512, #201284, #37749, #185042, #38818, #136329, #85426 ),
 .UNSPECIFIED., .F., .F.,
 ( 4, 3, 3, 3, 3, 4 ),
 ( 0.000000000000000000, 3.083448363908645134E-05, 6.173412828017592617E-05, 9.147751612222104365E-05, 0.0001189036761826361657, 0.0001300740652511593631 ),
 .UNSPECIFIED. ) ;
#21128 = CARTESIAN_POINT ( 'NONE',  ( 0.1331715793776600265, 0.003733371859311259821, -1.953671397793784070 ) ) ;
#21129 = CARTESIAN_POINT ( 'NONE',  ( 4.868786560638889149, 6.773613302202437403, 1.443375672974065660 ) ) ;
#21130 = CARTESIAN_POINT ( 'NONE',  ( 5.849792259110643933, 6.002811869646802911, -0.3480847251615213356 ) ) ;
#21131 = CARTESIAN_POINT ( 'NONE',  ( 1.244150428498992600, 3.277476754118171964, -0.7749999999999874767 ) ) ;
#21132 = CARTESIAN_POINT ( 'NONE',  ( -3.567766978690493307, 7.314145241780881435, 1.040834085586084257E-14 ) ) ;
#21133 = CARTESIAN_POINT ( 'NONE',  ( 0.1061415085658158342, 1.651838695520141398, 1.485519503937395402 ) ) ;
#21134 = CARTESIAN_POINT ( 'NONE',  ( 3.118299990072324057, -1.036503014707575332, -1.833135815837197535 ) ) ;
#21136 = CARTESIAN_POINT ( 'NONE',  ( -5.191846479390389568, 5.021852078902356631, 0.7998128361456281477 ) ) ;
#21135 = CIRCLE ( 'NONE', #114623, 3.475000000000000089 ) ;
#21137 = CARTESIAN_POINT ( 'NONE',  ( 5.777746017718023097, 9.892454120646377191, 0.7998128361456462443 ) ) ;
#21138 = CARTESIAN_POINT ( 'NONE',  ( 0.9591554131188588794, 1.518337787816389284, 1.075887112759424280 ) ) ;
#21139 = CARTESIAN_POINT ( 'NONE',  ( 6.612626235163189925, 8.737816579155630592, -1.599625672291262513 ) ) ;
#21140 = CARTESIAN_POINT ( 'NONE',  ( 5.684946482831785275, 5.526859072925533134, -0.7998128361456231517 ) ) ;
#21141 = CARTESIAN_POINT ( 'NONE',  ( -6.075462232699549325, 9.141770800574526845, 1.082531754730549967 ) ) ;
#21142 = CARTESIAN_POINT ( 'NONE',  ( -7.700668062882072284, 10.00719871149432549, -1.443375672974059665 ) ) ;
#21143 = CARTESIAN_POINT ( 'NONE',  ( 0.7738737444688469358, 0.4079195088417563730, -2.080830740624163955 ) ) ;
#21144 = CARTESIAN_POINT ( 'NONE',  ( -7.937372586157736443, 8.224965870130965584, 0.7998128361456341429 ) ) ;
#21146 = CARTESIAN_POINT ( 'NONE',  ( 4.158614545834369736, -0.6132839004606009947, -1.863630207987923004 ) ) ;
#21145 = CARTESIAN_POINT ( 'NONE',  ( 1.224999999999982991, 1.395833333333318382, -0.7072540797572817173 ) ) ;
#21147 = CARTESIAN_POINT ( 'NONE',  ( 2.711983997553393699, -2.138339778157403615, 0.3160903847422363300 ) ) ;
#21148 = CARTESIAN_POINT ( 'NONE',  ( 1.680954830071922812, 1.270413995023990106, 1.332975479855981416 ) ) ;
#21149 = CARTESIAN_POINT ( 'NONE',  ( -5.251027302601237956, 6.428042375187708934, -1.158707231040608576 ) ) ;
#21150 = CARTESIAN_POINT ( 'NONE',  ( 3.204748380415303188, -0.3384778632026878564, 1.706898776778777993 ) ) ;
#21151 = CARTESIAN_POINT ( 'NONE',  ( 4.015246738442954211, 7.790260991562450776, 0.2862651747304548744 ) ) ;
#21152 = CARTESIAN_POINT ( 'NONE',  ( 6.005898861173831094, 6.109229547565340646, 1.040834085586084257E-14 ) ) ;
#21153 = CARTESIAN_POINT ( 'NONE',  ( -9.979842676043658045, 5.589819607760295739, 5.978770845575332338 ) ) ;
#21155 = EDGE_CURVE ( 'NONE', #49028, #118348, #172523, .T. ) ;
#21154 = AXIS2_PLACEMENT_3D ( 'NONE', #33832, #136688, #70569 ) ;
#21156 = CARTESIAN_POINT ( 'NONE',  ( 0.4444780689869810564, 2.156031605563761833, 0.1575401717312311101 ) ) ;
#21157 = CARTESIAN_POINT ( 'NONE',  ( 3.268907511149142575, -2.013924394373915128, 0.09611935726179518524 ) ) ;
#21158 = CARTESIAN_POINT ( 'NONE',  ( -10.26315909542058336, 11.07603315418659840, -0.7216878364870267237 ) ) ;
#21159 = CARTESIAN_POINT ( 'NONE',  ( 0.4093245661422850734, 1.881582470445356314, 1.064130679222355491 ) ) ;
#21160 = CARTESIAN_POINT ( 'NONE',  ( 3.010573890873136094, 1.429054271512670615, -1.358355385302984164 ) ) ;
#21161 = CARTESIAN_POINT ( 'NONE',  ( 6.609000000000029296, 3.690475914267136837, 2.614198802211770367 ) ) ;
#21162 = CARTESIAN_POINT ( 'NONE',  ( 2.138135174613201350, 0.4275120379338535614, 1.894264587998186089 ) ) ;
#21165 = ORIENTED_EDGE ( 'NONE', *, *, #202366, .T. ) ;
#21164 = CARTESIAN_POINT ( 'NONE',  ( -5.831415467653581430, 5.975941931783510519, 0.7216878364870257245 ) ) ;
#21163 = CARTESIAN_POINT ( 'NONE',  ( 6.398695753475230674, -1.876852914212179035, -0.3660984893600614520 ) ) ;
#21166 = CARTESIAN_POINT ( 'NONE',  ( -5.031484404002922517, 6.963427452793760963, 1.443375672974058777 ) ) ;
#21167 = CARTESIAN_POINT ( 'NONE',  ( -0.1110810684432986112, 0.7552414886912374170, -1.881935688996359213 ) ) ;
#21168 = CARTESIAN_POINT ( 'NONE',  ( 3.725458348705031231, 7.568394850123006279, -1.734723475976807094E-15 ) ) ;
#21169 = CARTESIAN_POINT ( 'NONE',  ( -5.224688093219839402, 7.188831756880171397, -1.599625672291271394 ) ) ;
#21170 = CARTESIAN_POINT ( 'NONE',  ( -6.903036488013351679, 8.082572653217566128, -1.199719254218452047 ) ) ;
#21171 = DIRECTION ( 'NONE',  ( 0.000000000000000000, 0.000000000000000000, 1.000000000000000000 ) ) ;
#21172 = CARTESIAN_POINT ( 'NONE',  ( 6.774459802350780713, -1.427793189328768753, 1.813748355473641549 ) ) ;
#21173 = CARTESIAN_POINT ( 'NONE',  ( -10.27770456272603461, 4.830393611244395480, 6.108565810605171897 ) ) ;
#21174 = EDGE_CURVE ( 'NONE', #87955, #132709, #103772, .T. ) ;
#21175 = CARTESIAN_POINT ( 'NONE',  ( 3.924618397835403893, -1.320764108826902428, 1.450678906977073579 ) ) ;
#21176 = CARTESIAN_POINT ( 'NONE',  ( 8.959240580532112475, 9.346868853575953651, -0.7998128361456221525 ) ) ;
#21177 = CARTESIAN_POINT ( 'NONE',  ( 2.022111496571117772, -1.799922141918413487, 0.9091460122201827643 ) ) ;
#21178 = ORIENTED_EDGE ( 'NONE', *, *, #206094, .T. ) ;
#21179 = CARTESIAN_POINT ( 'NONE',  ( 2.835287003684193508, -1.733785568389034193, -1.215143187034111838 ) ) ;
#21180 = CARTESIAN_POINT ( 'NONE',  ( -1.500000000000013101, 1.910416667349488451, -0.8660254037844313801 ) ) ;
#21183 = ORIENTED_EDGE ( 'NONE', *, *, #89270, .F. ) ;
#21182 = CARTESIAN_POINT ( 'NONE',  ( -4.530395885260773525, 8.437212299446219532, 0.7998128361456481317 ) ) ;
#21181 = FILL_AREA_STYLE ('',( #184761 ) ) ;
#21184 = CARTESIAN_POINT ( 'NONE',  ( 3.310337721246572773, 1.664907390794263531, 0.7863323413084821745 ) ) ;
#21185 = VERTEX_POINT ( 'NONE', #153585 ) ;
#21186 = CARTESIAN_POINT ( 'NONE',  ( -10.15913717534155047, 10.74674821418697057, 0.7998128361456462443 ) ) ;
#21187 = CARTESIAN_POINT ( 'NONE',  ( 4.025719079702368752, -0.3592959752154977204, 2.089770972018199835 ) ) ;
#21188 = CARTESIAN_POINT ( 'NONE',  ( -9.886825906824906696, 3.934660213246447658, -6.000867881395567593 ) ) ;
#21189 = CARTESIAN_POINT ( 'NONE',  ( 6.287230548435207567, 8.358188277972981695, -1.599625672291262513 ) ) ;
#21190 = CARTESIAN_POINT ( 'NONE',  ( 5.220021542613917376, -1.098816822949649774, -1.743189258048108314 ) ) ;
#21192 = CARTESIAN_POINT ( 'NONE',  ( 2.595044651933966495, -0.5755060336137384214, 1.749081985381637061 ) ) ;
#21191 = CARTESIAN_POINT ( 'NONE',  ( -7.888146445052511169, 8.097259028849730811, 1.040834085586084257E-14 ) ) ;
#21193 = CARTESIAN_POINT ( 'NONE',  ( 9.043452155515161905, 10.50944792197790889, 1.199719254218453823 ) ) ;
#21194 = CARTESIAN_POINT ( 'NONE',  ( -1.364683531250010295, 5.530208333674751842, 0.7879004041258379498 ) ) ;
#21195 =( LENGTH_UNIT ( ) NAMED_UNIT ( * ) SI_UNIT ( .MILLI., .METRE. ) );
#21196 = CARTESIAN_POINT ( 'NONE',  ( -4.816538118508267630, 5.092449105792602460, -0.9495590845017554127 ) ) ;
#21197 = FACE_OUTER_BOUND ( 'NONE', #48616, .T. ) ;
#21198 = AXIS2_PLACEMENT_3D ( 'NONE', #136303, #20388, #156823 ) ;
#21199 = CARTESIAN_POINT ( 'NONE',  ( 1.840723031453334935, 2.183200880077686978, 0.3216222850719457349 ) ) ;
#21200 = CARTESIAN_POINT ( 'NONE',  ( 4.060077147624012284, 2.245929291707829289, -0.2719227649434445282 ) ) ;
#21201 = CARTESIAN_POINT ( 'NONE',  ( -8.080296364064746939, 9.489729181906076505, 1.082531754730558626 ) ) ;
#21202 = CARTESIAN_POINT ( 'NONE',  ( 3.076200346286896536, 0.8185659037078784062, 1.616202036402814901 ) ) ;
#21203 = CARTESIAN_POINT ( 'NONE',  ( 4.733546111355320107, 0.5950593785610300834, -1.821060146467222918 ) ) ;
#21204 = CARTESIAN_POINT ( 'NONE',  ( 1.364683531249988535, 4.217708333674752730, -0.7879004041258239610 ) ) ;
#21205 = CARTESIAN_POINT ( 'NONE',  ( 4.223478185285460818, -1.886956702611849002, 0.5710618836329334203 ) ) ;
#21206 = CARTESIAN_POINT ( 'NONE',  ( 1.149297380808786517, -1.516923518071541910, -1.187294353726556562 ) ) ;
#21207 = CARTESIAN_POINT ( 'NONE',  ( 5.366025703835962446, 0.9229158262306772498, 1.627043297953718382 ) ) ;
#21208 = CARTESIAN_POINT ( 'NONE',  ( 3.194261032343487461, -0.9352514745577229505, 2.109854200106716426 ) ) ;
#21209 = CARTESIAN_POINT ( 'NONE',  ( 4.633164157742322153, 0.0009153448507570947738, -1.861241882716960561 ) ) ;
#21210 = CARTESIAN_POINT ( 'NONE',  ( 0.4644097342742965484, -8.233137084989849086, 9.488641820551103834 ) ) ;
#21211 = CARTESIAN_POINT ( 'NONE',  ( 0.5675926644314840397, 1.357872185771633156, 1.490966652548594285 ) ) ;
#21213 = CARTESIAN_POINT ( 'NONE',  ( 1.559346616682453668, -1.807134503733454078, -1.081319387842846425 ) ) ;
#21212 = CARTESIAN_POINT ( 'NONE',  ( -3.090895833791289071, 6.549869539491048442, 1.040834085586084257E-14 ) ) ;
#21214 = CARTESIAN_POINT ( 'NONE',  ( 3.429849674132933846, 5.024577257953626308, -1.443375672974058777 ) ) ;
#21216 = CARTESIAN_POINT ( 'NONE',  ( -8.967828540435322182, 12.54988483289483980, 1.199719254218462483 ) ) ;
#21215 = CARTESIAN_POINT ( 'NONE',  ( -1.364683531250012516, 5.051041667008085767, -0.7879004041258300672 ) ) ;
#21217 = CARTESIAN_POINT ( 'NONE',  ( 3.322626870553476941, -0.8629183168706102691, -1.937285153019531414 ) ) ;
#21218 = DIRECTION ( 'NONE',  ( -0.6292706268317957985, 0.7771862570881697962, 0.000000000000000000 ) ) ;
#21219 = CARTESIAN_POINT ( 'NONE',  ( 1.037374617392500031, -0.04523278242563041895, 2.019440925237799167 ) ) ;
#21220 = CARTESIAN_POINT ( 'NONE',  ( -1.201851678989727383E-14, 1.071875000341418138, 1.575800808251672791 ) ) ;
#21221 = CARTESIAN_POINT ( 'NONE',  ( -4.785665035943912571, 4.685623418130398399, 1.214306433183764966E-14 ) ) ;
#21222 = CARTESIAN_POINT ( 'NONE',  ( 5.847644326195776010, 5.716673223516856694, -0.7998128361456281477 ) ) ;
#21223 = VERTEX_POINT ( 'NONE', #204430 ) ;
#21224 = CARTESIAN_POINT ( 'NONE',  ( 1.669428131952359839, 0.1607934374257547205, -2.155692497560882437 ) ) ;
#21225 = CARTESIAN_POINT ( 'NONE',  ( 4.772106882330221289, 6.590544000850480089, -1.443375672974051449 ) ) ;
#21226 = EDGE_CURVE ( 'NONE', #181635, #139784, #79116, .T. ) ;
#21229 = CARTESIAN_POINT ( 'NONE',  ( 3.226477370372305753, 4.787309570232886280, 1.443375672974062551 ) ) ;
#21228 = CARTESIAN_POINT ( 'NONE',  ( 6.925078400183550364, 2.460400685555228950, 2.239421262742965268 ) ) ;
#21227 = CARTESIAN_POINT ( 'NONE',  ( 5.224688093219824303, 7.188831756880171397, -1.599625672291283607 ) ) ;
#21230 = CARTESIAN_POINT ( 'NONE',  ( 10.18181017373857067, 11.94149529319227909, 1.082531754730548412 ) ) ;
#21231 = CARTESIAN_POINT ( 'NONE',  ( 6.245327377194020535, 0.3399632236478037917, -1.987496870419297013 ) ) ;
#21232 = CARTESIAN_POINT ( 'NONE',  ( -9.015808963407680565, 9.620791333504852716, 1.040834085586084257E-14 ) ) ;
#21233 = CARTESIAN_POINT ( 'NONE',  ( 0.3456114054924685486, 0.6817542107791437767, -2.082909237240769151 ) ) ;
#21234 = FACE_OUTER_BOUND ( 'NONE', #84959, .T. ) ;
#21236 = CARTESIAN_POINT ( 'NONE',  ( -0.6823417656250039265, 12.31770833367473017, -1.181850606188755259 ) ) ;
#21235 = CARTESIAN_POINT ( 'NONE',  ( 6.819229411136438657, -0.1619093195798972928, 2.126376854085454404 ) ) ;
#21237 = CARTESIAN_POINT ( 'NONE',  ( -9.833741488613570780, 10.36711991300432345, 0.7998128361456462443 ) ) ;
#21238 = CARTESIAN_POINT ( 'NONE',  ( -5.056828107772866510, 5.962349549565537643, -1.082531754730543971 ) ) ;
#21239 = CARTESIAN_POINT ( 'NONE',  ( 0.6823417656249899377, 1.655208333674752730, 1.181850606188755259 ) ) ;
#21240 = CARTESIAN_POINT ( 'NONE',  ( -9.296355089585910693E-16, 2.750000000682797818, -1.225000000000007860 ) ) ;
#21241 = CARTESIAN_POINT ( 'NONE',  ( -0.7500000000000179856, 9.791666666666671404, 1.299038105676658228 ) ) ;
#21242 = CARTESIAN_POINT ( 'NONE',  ( 4.389066697632080682, 1.539216480442310075, -0.7786167122535156970 ) ) ;
#21243 = CARTESIAN_POINT ( 'NONE',  ( 5.554000203453580475, 6.508696987897830688, -1.199719254218452047 ) ) ;
#21244 = CARTESIAN_POINT ( 'NONE',  ( 1.545802484126792109, 1.767419949743149532, 0.09338694931935660748 ) ) ;
#21245 = CARTESIAN_POINT ( 'NONE',  ( 9.911173986789782120, 11.52179005846497972, -1.199719254218440723 ) ) ;
#21246 = CARTESIAN_POINT ( 'NONE',  ( 5.438574045396407541, 2.173287242562565780, 0.3821286992964008089 ) ) ;
#21247 = ORIENTED_EDGE ( 'NONE', *, *, #191462, .F. ) ;
#21248 = CARTESIAN_POINT ( 'NONE',  ( 4.588152005245718534, 1.166368207181975869, 1.648760302449885584 ) ) ;
#21249 = CARTESIAN_POINT ( 'NONE',  ( -6.720001414228860881, 7.869031733802326123, -1.199719254218452047 ) ) ;
#21251 = CARTESIAN_POINT ( 'NONE',  ( 3.532827515057835654, -1.646827434736859441, 1.163287548526056980 ) ) ;
#21250 = CARTESIAN_POINT ( 'NONE',  ( 3.809332071562030908, 1.790574611000576244, -1.135637872363919110 ) ) ;
#21253 = EDGE_LOOP ( 'NONE', ( #177585, #92321, #90498, #136120 ) ) ;
#21252 = CARTESIAN_POINT ( 'NONE',  ( 4.095841850722721667, 1.188128187434208893, 1.367607970084052660 ) ) ;
#21254 = CARTESIAN_POINT ( 'NONE',  ( 5.923986774528332333, 5.876015756563318426, -0.7998128361456481317 ) ) ;
#21255 = VERTEX_POINT ( 'NONE', #156796 ) ;
#21256 = CARTESIAN_POINT ( 'NONE',  ( 1.199835987674138460, -1.870836310881810682, -0.003643258294119822160 ) ) ;
#21257 = AXIS2_PLACEMENT_3D ( 'NONE', #185622, #106578, #205069 ) ;
#21258 = CARTESIAN_POINT ( 'NONE',  ( -10.91828647086820858, -9.953005061877725268, 0.1753736836078399752 ) ) ;
#21259 = CARTESIAN_POINT ( 'NONE',  ( 6.410821795378537580, -0.4906875946298261959, -1.743675775721682752 ) ) ;
#21260 = CARTESIAN_POINT ( 'NONE',  ( 2.535011536075336913, 5.133042487381361596, -2.419999999999995044 ) ) ;
#21261 = CARTESIAN_POINT ( 'NONE',  ( -10.28140399934106242, 4.005782094233665269, -7.421933058660648008 ) ) ;
#21262 = DIRECTION ( 'NONE',  ( -0.7592566023653004592, -0.6507913734559639396, -0.000000000000000000 ) ) ;
#21263 = CARTESIAN_POINT ( 'NONE',  ( -1.364683531249997417, 3.071875000341423245, 1.214306433183764966E-14 ) ) ;
#21264 = CARTESIAN_POINT ( 'NONE',  ( -0.01753026575586694516, -1.247696154478775021, 1.449428981083925150 ) ) ;
#21265 = ADVANCED_FACE ( 'NONE', ( #6232 ), #72939, .T. ) ;
#21266 = CARTESIAN_POINT ( 'NONE',  ( 5.885648082108199119, 6.999582529615296700, 1.082531754730549967 ) ) ;
#21267 = CARTESIAN_POINT ( 'NONE',  ( 1.785527960060459440, -1.848404783191982315, 0.6579185095809261252 ) ) ;
#21268 = CARTESIAN_POINT ( 'NONE',  ( -4.258669648468323743, 6.061810238003387141, 1.443375672974065660 ) ) ;
#21269 = CARTESIAN_POINT ( 'NONE',  ( -4.749098946536820520, 8.762642214260091933, 0.7998128361456281477 ) ) ;
#21270 = CARTESIAN_POINT ( 'NONE',  ( 3.674183785563363447, 2.104178206457421485, -0.2630699042918820396 ) ) ;
#21272 = CARTESIAN_POINT ( 'NONE',  ( 0.000000000000000000, 2.800000000000024691, -0.7749999999999935829 ) ) ;
#21271 = CARTESIAN_POINT ( 'NONE',  ( 2.069187086148546406, 1.970899860167973694, -11.59589854942352893 ) ) ;
#21273 = CARTESIAN_POINT ( 'NONE',  ( 6.011001170722232168, 1.737326539053269059, 0.9316862151012759163 ) ) ;
#21274 = CARTESIAN_POINT ( 'NONE',  ( -1.364683531250000748, 1.259375000341421469, 0.000000000000000000 ) ) ;
#21275 = CARTESIAN_POINT ( 'NONE',  ( 1.301040509920841526, -0.2996390532185671529, -1.990687865782204469 ) ) ;
#21276 = ORIENTED_EDGE ( 'NONE', *, *, #91128, .T. ) ;
#21277 = CARTESIAN_POINT ( 'NONE',  ( 0.8435474745839615096, 0.4086855458026328880, -2.077256349191716200 ) ) ;
#21279 = EDGE_CURVE ( 'NONE', #7325, #102958, #59367, .T. ) ;
#21278 = CARTESIAN_POINT ( 'NONE',  ( 12.00010846780092066, 6.571259622882246632, -0.4985838157269280035 ) ) ;
#21280 = CARTESIAN_POINT ( 'NONE',  ( 2.752462066230080495, -2.064650614848703825, -0.1547973748374023295 ) ) ;
#21281 = CARTESIAN_POINT ( 'NONE',  ( 4.203910148689107729, 7.062256385849379647, -1.199719254218448494 ) ) ;
#21282 = CARTESIAN_POINT ( 'NONE',  ( 6.900173834712277632, 7.014900660111269559, -0.7998128361456341429 ) ) ;
#21283 = ORIENTED_EDGE ( 'NONE', *, *, #113401, .T. ) ;
#21285 = CARTESIAN_POINT ( 'NONE',  ( 4.547870462380197765, 7.393267075163835855, 1.199719254218462483 ) ) ;
#21284 = CARTESIAN_POINT ( 'NONE',  ( 5.050766879278534738, -1.765858898356540196, -1.118837652998798005 ) ) ;
#21288 = ORIENTED_EDGE ( 'NONE', *, *, #19563, .F. ) ;
#21287 = CARTESIAN_POINT ( 'NONE',  ( 1.541375357114631806, -1.705629342057282560, 0.6104535550692562484 ) ) ;
#21286 = CARTESIAN_POINT ( 'NONE',  ( 2.854317205943053271, 0.6132515345431620579, 1.719634925709014439 ) ) ;
#21289 = CARTESIAN_POINT ( 'NONE',  ( 0.3000000000000009881, 3.214163249644255593, -0.5238375172407520042 ) ) ;
#21290 = FACE_OUTER_BOUND ( 'NONE', #155097, .T. ) ;
#21291 = STYLED_ITEM ( 'NONE', ( #187970 ), #172604 ) ;
#21292 = CARTESIAN_POINT ( 'NONE',  ( 4.190592561755676293, -2.182319254149690302, -0.3268587364041104504 ) ) ;
#21293 = CARTESIAN_POINT ( 'NONE',  ( 6.662942426112080874, 9.860851032851066122, 1.199719254218460707 ) ) ;
#21294 = CARTESIAN_POINT ( 'NONE',  ( -0.6823417656250003738, 9.713541667008065872, 1.181850606188754593 ) ) ;
#21295 = ORIENTED_EDGE ( 'NONE', *, *, #201653, .T. ) ;
#21296 = CARTESIAN_POINT ( 'NONE',  ( 3.352119889487484183, 0.8575151890419380196, -1.709291564166728783 ) ) ;
#21297 = CARTESIAN_POINT ( 'NONE',  ( -4.810445574750349174, 4.506608013497163334, 0.7998128361456341429 ) ) ;
#21298 = CARTESIAN_POINT ( 'NONE',  ( 7.609150525767641504, 9.900428251527500834, -1.599625672291262513 ) ) ;
#21299 = CARTESIAN_POINT ( 'NONE',  ( 6.074686117427479104, 1.393331124738606874, -1.531503843499823159 ) ) ;
#21300 = CARTESIAN_POINT ( 'NONE',  ( 0.5980308150947402090, 0.002692760363722866267, 1.225484906753091519 ) ) ;
#21301 = CARTESIAN_POINT ( 'NONE',  ( 6.146043800834426918, 0.6857851511376764631, 2.081541312870714311 ) ) ;
#21302 = CARTESIAN_POINT ( 'NONE',  ( 5.092389439195339484, 7.944299729584391123, -1.199137415704543130 ) ) ;
#21303 = CARTESIAN_POINT ( 'NONE',  ( -8.171065180669568662, 15.47018273137357802, -8.834024877852263202 ) ) ;
#21304 = CIRCLE ( 'NONE', #211509, 2.400000000000007461 ) ;
#21305 = DIRECTION ( 'NONE',  ( 0.000000000000000000, 1.000000000000000000, 0.000000000000000000 ) ) ;
#21306 = CARTESIAN_POINT ( 'NONE',  ( 3.778450875046265534, -1.801938340082277712, -0.5016190811713144848 ) ) ;
#21307 = CARTESIAN_POINT ( 'NONE',  ( -3.285556943750000070, -1.246874999522043392, 0.000000000000000000 ) ) ;
#21308 = CARTESIAN_POINT ( 'NONE',  ( 10.50000000000000000, 10.09290055818100740, 3.599999999999996536 ) ) ;
#21309 = ADVANCED_FACE ( 'NONE', ( #190882, #108651 ), #106853, .F. ) ;
#21310 = CARTESIAN_POINT ( 'NONE',  ( -7.700668062882072284, 10.00719871149432549, -1.443375672974059665 ) ) ;
#21311 = CARTESIAN_POINT ( 'NONE',  ( 5.734172623936983904, 5.654565914206774124, 0.7998128361456352531 ) ) ;
#21312 = CARTESIAN_POINT ( 'NONE',  ( 0.4616802850961505555, -0.5308588990461468038, 1.896450293990773472 ) ) ;
#21313 = CARTESIAN_POINT ( 'NONE',  ( 1.142204091441896718, 0.8197918422115093584, 1.842440257734210274 ) ) ;
#21314 = CARTESIAN_POINT ( 'NONE',  ( -10.32183501870554387, 10.93656236477829502, 0.7998128361456462443 ) ) ;
#21315 = CARTESIAN_POINT ( 'NONE',  ( 6.156284269057003655, 9.340026192945279249, -1.199719254218452047 ) ) ;
#21316 = CARTESIAN_POINT ( 'NONE',  ( 0.000000000000000000, -7.154544010627095219, 0.000000000000000000 ) ) ;
#21317 = CARTESIAN_POINT ( 'NONE',  ( 1.465048628566959055, 0.1585425061045864503, -2.185770122351132994 ) ) ;
#21318 = CARTESIAN_POINT ( 'NONE',  ( 6.076747101522134820, -1.735163100867884500, -0.5679748894881069265 ) ) ;
#21319 = CARTESIAN_POINT ( 'NONE',  ( -3.110706179331648169, 5.716575411607132118, 1.199719254218462483 ) ) ;
#21320 = CARTESIAN_POINT ( 'NONE',  ( 6.427974226654860956, 7.632296364919712417, -1.082531754730548412 ) ) ;
#21321 = CARTESIAN_POINT ( 'NONE',  ( 7.886038904643079661, 12.35212915539230139, -0.7998128361456352531 ) ) ;
#21322 = CARTESIAN_POINT ( 'NONE',  ( 5.040934186182656873, 4.775511393501539636, 1.040834085586084257E-14 ) ) ;
#21323 = CARTESIAN_POINT ( 'NONE',  ( 5.076602173674213070, 4.887400388900169368, 0.000000000000000000 ) ) ;
#21324 = VERTEX_POINT ( 'NONE', #132335 ) ;
#21326 = CARTESIAN_POINT ( 'NONE',  ( 0.2408851659233458842, 1.927091567462356547, 0.5821649069043339786 ) ) ;
#21325 = CARTESIAN_POINT ( 'NONE',  ( 3.790429961727882713, 1.553415782126759792, -0.9881970032953185656 ) ) ;
#21327 = CARTESIAN_POINT ( 'NONE',  ( 1.845480572931688767, -1.229624162049542058, 1.941665159144045250 ) ) ;
#21329 = CARTESIAN_POINT ( 'NONE',  ( 6.842638302680406071, -1.923265442670134329, -0.3857968560932593660 ) ) ;
#21328 = CARTESIAN_POINT ( 'NONE',  ( 2.711267533052988732, 6.106969855296372707, -0.7216878364870267237 ) ) ;
#21330 = CARTESIAN_POINT ( 'NONE',  ( -3.285556943750000514, -3.638541666188706891, -1.896917185911906500 ) ) ;
#21331 = CARTESIAN_POINT ( 'NONE',  ( -4.578903193113314174, 6.365139696764064325, 1.599625672291267398 ) ) ;
#21332 = CARTESIAN_POINT ( 'NONE',  ( -15.75000000000000000, 13.40000000000000036, -3.600000000000002309 ) ) ;
#21333 = CARTESIAN_POINT ( 'NONE',  ( 4.306835718904429733, -0.4242474483713705169, -1.864571660543254961 ) ) ;
#21334 = CARTESIAN_POINT ( 'NONE',  ( -9.053093885623068715, 11.58502883802551153, -1.599625672291263179 ) ) ;
#21335 = CARTESIAN_POINT ( 'NONE',  ( 6.477827756726281194, 6.756902019748111776, -0.2091553196570776485 ) ) ;
#21336 = CARTESIAN_POINT ( 'NONE',  ( -4.309512724297390740, 6.121127159803966933, 1.599625672291270506 ) ) ;
#21338 = CARTESIAN_POINT ( 'NONE',  ( 1.217418975555501826, -1.825842229346545498, 0.4062821374252246764 ) ) ;
#21337 = CARTESIAN_POINT ( 'NONE',  ( 2.999644136165266595, -2.088248420355208523, 0.1050208477483879216 ) ) ;
#21339 = CARTESIAN_POINT ( 'NONE',  ( 6.954969614130424027, 11.05795561655343384, 1.040834085586084257E-14 ) ) ;
#21340 = CARTESIAN_POINT ( 'NONE',  ( -0.6823417656250212460, 3.613541667008085767, 1.181850606188767472 ) ) ;
#21341 = CARTESIAN_POINT ( 'NONE',  ( 2.928976884739741493, -1.170936322307249089, -1.287801759770091925 ) ) ;
#21342 = CARTESIAN_POINT ( 'NONE',  ( 5.183294799126148433, 4.941598775268944976, 1.040834085586084257E-14 ) ) ;
#21343 = CARTESIAN_POINT ( 'NONE',  ( 0.3337279542187601145, 3.354361423484768956, -1.974754334845483905 ) ) ;
#21344 = CARTESIAN_POINT ( 'NONE',  ( 3.879312468746206832, 1.623315624747388775, -0.5835212994509741957 ) ) ;
#21345 =( BOUNDED_CURVE ( )  B_SPLINE_CURVE ( 2, ( #130753, #179444, #196747, #32115, #14777, #180498, #68844 ),
 .UNSPECIFIED., .F., .T. ) 
 B_SPLINE_CURVE_WITH_KNOTS ( ( 3, 2, 2, 3 ),
 ( 0.2749999999999999112, 0.2833333333333333259, 0.2916666666666667962, 0.3000000000000002109 ),
 .UNSPECIFIED. ) 
 CURVE ( )  GEOMETRIC_REPRESENTATION_ITEM ( )  RATIONAL_B_SPLINE_CURVE ( ( 1.000000000000001776, 0.8660254037844369313, 1.000000000000000000, 0.8660254037844387076, 1.000000000000000000, 0.8660254037844351549, 1.000000000000003553 ) ) 
 REPRESENTATION_ITEM ( '' )  );
#21346 = CARTESIAN_POINT ( 'NONE',  ( 3.720431430916489646, 2.081484170424623859, 0.6860852429351402826 ) ) ;
#21347 = CARTESIAN_POINT ( 'NONE',  ( 5.830760709146560750, 2.125890151018691832, 0.5921790101122563765 ) ) ;
#21348 = CARTESIAN_POINT ( 'NONE',  ( 1.123270288250311610, 3.172697346350006331, 0.7749999999993734123 ) ) ;
#21349 = MECHANICAL_DESIGN_GEOMETRIC_PRESENTATION_REPRESENTATION (  '', ( #142334 ), #152961 ) ;
#21350 = CARTESIAN_POINT ( 'NONE',  ( 3.151421466623941292, 1.864366918651944927, -1.112252681494025897 ) ) ;
#21351 = CARTESIAN_POINT ( 'NONE',  ( 1.769861954154128725, 0.9373860217288846330, 1.566528536362868707 ) ) ;
#21352 = CARTESIAN_POINT ( 'NONE',  ( 4.161989969715272686, 4.726297878971393196, 2.420000000000010587 ) ) ;
#21353 = CARTESIAN_POINT ( 'NONE',  ( 4.048151681910251654, 1.001636719310808887, 1.865476516996619649 ) ) ;
#21354 = CIRCLE ( 'NONE', #66347, 0.08000000000000020983 ) ;
#21355 = ORIENTED_EDGE ( 'NONE', *, *, #65262, .F. ) ;
#21357 = CARTESIAN_POINT ( 'NONE',  ( -1.364683531250012516, 3.092708333674755838, 0.7879004041258379498 ) ) ;
#21356 = CARTESIAN_POINT ( 'NONE',  ( 5.249693134425458041, 2.289860626911474739, -0.1101728261837572470 ) ) ;
#21358 = CARTESIAN_POINT ( 'NONE',  ( 6.620655732516673275, 1.290356161719278028, 1.942653802560645460 ) ) ;
#21359 = CARTESIAN_POINT ( 'NONE',  ( 8.516493047678546091, 13.08765898893368629, -0.7998128361456352531 ) ) ;
#21360 = CARTESIAN_POINT ( 'NONE',  ( 0.6453774867190856801, 0.1600191834128759094, 2.114519675249281416 ) ) ;
#21361 = CARTESIAN_POINT ( 'NONE',  ( -5.599154252763867134, 5.634694171087028636, 0.000000000000000000 ) ) ;
#21362 = CYLINDRICAL_SURFACE ( 'NONE', #35653, 3.475000000000000089 ) ;
#21363 = CARTESIAN_POINT ( 'NONE',  ( -5.707619481228822345, 7.681975366232176583, -1.443375672974051449 ) ) ;
#21365 = CARTESIAN_POINT ( 'NONE',  ( -1.500000000000008216, 11.78125000068279427, 3.469446951953614189E-15 ) ) ;
#21364 = CARTESIAN_POINT ( 'NONE',  ( 6.883263157960358924, 4.692138088316172073, 2.616388454592593504 ) ) ;
#21366 = ORIENTED_EDGE ( 'NONE', *, *, #101879, .T. ) ;
#21367 = CARTESIAN_POINT ( 'NONE',  ( 4.957657809308734898, -1.899617967926207740, -0.6767155953601932117 ) ) ;
#21369 = CARTESIAN_POINT ( 'NONE',  ( 4.416881224320576393, -1.531859844946925397, 1.381376250335116795 ) ) ;
#21368 = CARTESIAN_POINT ( 'NONE',  ( 5.066996723205273057, 6.934582148538044777, 1.599625672291267398 ) ) ;
#21371 = CARTESIAN_POINT ( 'NONE',  ( 6.883263157960399781, 2.970623603138924818, 2.399364662246627589 ) ) ;
#21370 = CARTESIAN_POINT ( 'NONE',  ( 6.261886844665240481, 8.398896966899865646, 1.599625672291268286 ) ) ;
#21372 = CARTESIAN_POINT ( 'NONE',  ( 5.040599249230596435, 9.102725900736217568, 0.7998128361456341429 ) ) ;
#21373 = CARTESIAN_POINT ( 'NONE',  ( 1.642778471875000035, -1.626041666188710044, -2.845375778867859751 ) ) ;
#21374 = DIRECTION ( 'NONE',  ( 1.000000000000000000, -5.578564026256504688E-16, 0.000000000000000000 ) ) ;
#21375 = CARTESIAN_POINT ( 'NONE',  ( 0.5508686287750690358, -1.767239575335936230, -1.116659500934626514 ) ) ;
#21376 = CARTESIAN_POINT ( 'NONE',  ( 4.799454022740247794, 1.388487131293577592, -1.462444391756134943 ) ) ;
#21377 = CARTESIAN_POINT ( 'NONE',  ( 3.649809678215182096, 0.6660801477775115664, 1.716721118343276453 ) ) ;
#21378 = CARTESIAN_POINT ( 'NONE',  ( 4.333802657862601215, 8.207853534148366492, 0.7998128361456462443 ) ) ;
#21379 = SURFACE_SIDE_STYLE ('',( #133063 ) ) ;
#21380 = CARTESIAN_POINT ( 'NONE',  ( 0.8149653058732795330, -0.2595981955949409614, 1.704996164590016683 ) ) ;
#21381 = DIRECTION ( 'NONE',  ( 1.000000000000000000, -0.000000000000000000, -0.000000000000000000 ) ) ;
#21382 = CARTESIAN_POINT ( 'NONE',  ( 1.284255082537180570, 1.875723515222413207, -1.328569176028525645 ) ) ;
#21383 = CARTESIAN_POINT ( 'NONE',  ( -7.223796917982883592, 7.322184580601816428, -0.7998128361456291469 ) ) ;
#21384 = CARTESIAN_POINT ( 'NONE',  ( 0.3864610594027502732, -1.064975819449946126, 1.996106434226818216 ) ) ;
#21385 = CARTESIAN_POINT ( 'NONE',  ( 2.614012881481563522, -2.083059734262616036, 0.3096129728813925008 ) ) ;
#21386 = CARTESIAN_POINT ( 'NONE',  ( -5.971440312176176768, 5.931378217152456500, 0.000000000000000000 ) ) ;
#21387 = CARTESIAN_POINT ( 'NONE',  ( 7.613066949273408213, 8.840665181362512115, -1.199719254218441611 ) ) ;
#21388 = CARTESIAN_POINT ( 'NONE',  ( 5.519577934094851202, 8.493239118869080784, 1.082531754730547524 ) ) ;
#21389 = CARTESIAN_POINT ( 'NONE',  ( 5.843750000000004441, 1.895863743164205140, 0.7852924748296741253 ) ) ;
#21390 = CARTESIAN_POINT ( 'NONE',  ( -6.551614543901706611, 8.666636272683888365, 1.599625672291283607 ) ) ;
#21391 = CARTESIAN_POINT ( 'NONE',  ( 5.612712405933139692, 9.491988873656591608, 1.040834085586084257E-14 ) ) ;
#21392 = CARTESIAN_POINT ( 'NONE',  ( 4.798800619506367049, 6.970516071510092893, 1.407892184351482889 ) ) ;
#21393 = CARTESIAN_POINT ( 'NONE',  ( -3.164938793786285842, 5.779846795137578930, -1.199719254218452935 ) ) ;
#21394 = CARTESIAN_POINT ( 'NONE',  ( 3.480930870787651621, -1.489476591903232228, 1.648259452209248854 ) ) ;
#21395 = CARTESIAN_POINT ( 'NONE',  ( 1.799034956846547795, 1.823213324544867397, 1.215573211712846158 ) ) ;
#21396 = CARTESIAN_POINT ( 'NONE',  ( -5.738125327081750271, 7.717565519727259904, 1.599625672291269396 ) ) ;
#21397 = AXIS2_PLACEMENT_3D ( 'NONE', #97011, #79662, #131661 ) ;
#21398 = CARTESIAN_POINT ( 'NONE',  ( -3.623772196602547346, 7.449761006003425834, 0.000000000000000000 ) ) ;
#21399 = CARTESIAN_POINT ( 'NONE',  ( 5.652778587040098834, -0.4750822840141955550, -1.903360745478323679 ) ) ;
#21400 = CARTESIAN_POINT ( 'NONE',  ( -1.364683531250012516, 1.780208333674757615, 0.7879004041258379498 ) ) ;
#21401 = CARTESIAN_POINT ( 'NONE',  ( -3.526529353330355221, 6.168015774643768268, -1.082531754730546636 ) ) ;
#21402 = CARTESIAN_POINT ( 'NONE',  ( -5.761852096127856981, 5.824508321678349532, 0.000000000000000000 ) ) ;
#21403 = CARTESIAN_POINT ( 'NONE',  ( 4.851869265964163347, -1.501451181749386743, -1.497782127133556518 ) ) ;
#21404 = CARTESIAN_POINT ( 'NONE',  ( -3.797165540279144214, 6.587721009371067638, 1.199719254218452935 ) ) ;
#21405 = ORIENTED_EDGE ( 'NONE', *, *, #183143, .T. ) ;
#21407 = CARTESIAN_POINT ( 'NONE',  ( 5.682550338946039226, -2.108058120380253087, -0.4779004524640489970 ) ) ;
#21406 = CARTESIAN_POINT ( 'NONE',  ( -6.021229618244897885, 7.157760988441397743, 1.082531754730548412 ) ) ;
#21408 = CARTESIAN_POINT ( 'NONE',  ( 4.808338034340912337, 8.761478140039733020, 1.040834085586084257E-14 ) ) ;
#21409 = CARTESIAN_POINT ( 'NONE',  ( 5.056134578334451568, -1.329838508726857382, 1.273713382018211382 ) ) ;
#21410 = CARTESIAN_POINT ( 'NONE',  ( -5.912397865540070185, 5.999963284693008880, 0.01096864257240509621 ) ) ;
#21411 = CARTESIAN_POINT ( 'NONE',  ( 1.364683531249990311, 3.196875000341416140, 1.214306433183764966E-14 ) ) ;
#21412 = CARTESIAN_POINT ( 'NONE',  ( 6.456985410506528744, 0.2896317775202154610, -1.715898445072817413 ) ) ;
#21413 = CARTESIAN_POINT ( 'NONE',  ( 11.41381676900476805, 12.56958039977607733, 3.704697931490188889 ) ) ;
#21414 = CARTESIAN_POINT ( 'NONE',  ( 1.364683531249986537, -0.8239583329919186738, 0.7879004041258500513 ) ) ;
#21415 = CARTESIAN_POINT ( 'NONE',  ( -0.4304495291404314417, 3.052659083096569415, 0.4198826858263652873 ) ) ;
#21416 = EDGE_CURVE ( 'NONE', #33049, #95100, #189819, .T. ) ;
#21417 = CARTESIAN_POINT ( 'NONE',  ( 5.401312781148373432, 1.764888628567516049, 1.247983453017486699 ) ) ;
#21418 = CARTESIAN_POINT ( 'NONE',  ( -4.731959306369413198, 5.479372931307791461, -1.199719254218446718 ) ) ;
#21419 = CARTESIAN_POINT ( 'NONE',  ( -6.033015167956794933, 9.982342096017511324, -0.7216878364870267237 ) ) ;
#21420 = CARTESIAN_POINT ( 'NONE',  ( 3.784175263432405956, -1.067420458145739826, 1.879713924940962677 ) ) ;
#21421 = CARTESIAN_POINT ( 'NONE',  ( 4.727780648284140241, -1.210341919374293473, -1.556009220651358715 ) ) ;
#21422 = CARTESIAN_POINT ( 'NONE',  ( 4.182719533963025427, -0.8905394866418876454, -1.487461311242815443 ) ) ;
#21423 = CARTESIAN_POINT ( 'NONE',  ( 0.6971427418834205136, 1.794861059153027627, 1.257291590721874686 ) ) ;
#21424 = CARTESIAN_POINT ( 'NONE',  ( 1.800300592175264613, -0.7760554750895022336, 2.173288546431056734 ) ) ;
#21425 = CARTESIAN_POINT ( 'NONE',  ( 3.761055697714862589, -1.815786459315921642, -0.9745866149870155981 ) ) ;
#21426 = CARTESIAN_POINT ( 'NONE',  ( 6.181195893160847277, 1.342424930544680928, 1.403604608442722057 ) ) ;
#21427 = CARTESIAN_POINT ( 'NONE',  ( -8.324343128666356506, 8.814081192973304724, 1.040834085586084257E-14 ) ) ;
#21428 = CARTESIAN_POINT ( 'NONE',  ( -5.173318132066234476, 8.193232366456022930, -1.199719254218453823 ) ) ;
#21429 = SURFACE_STYLE_FILL_AREA ( #139503 ) ;
#21430 = CARTESIAN_POINT ( 'NONE',  ( -3.006876207180748217, 6.730049018344652190, -0.7998128361456481317 ) ) ;
#21431 = CARTESIAN_POINT ( 'NONE',  ( -7.822691444960716112, 8.228820895316715678, -0.7216878364870267237 ) ) ;
#21432 = CARTESIAN_POINT ( 'NONE',  ( 3.891806949550260519, 1.596497936513015192, 1.523729906679156754 ) ) ;
#21433 = CARTESIAN_POINT ( 'NONE',  ( -3.285556943750000514, -1.626041666188708046, -1.896917185911906500 ) ) ;
#21434 = ORIENTED_EDGE ( 'NONE', *, *, #125500, .F. ) ;
#21435 = CARTESIAN_POINT ( 'NONE',  ( 0.9185399124422718442, -1.353032588479759157, 1.277947871810279246 ) ) ;
#21436 = CARTESIAN_POINT ( 'NONE',  ( 1.492729907964629898, 3.265405474989949486, 0.1664789471928639075 ) ) ;
#21437 = CARTESIAN_POINT ( 'NONE',  ( 0.000000000000000000, -0.5000000000000004441, 1.249999999999999778 ) ) ;
#21438 = CARTESIAN_POINT ( 'NONE',  ( -9.495223711095324148, -8.169755926620650754, 0.3080734816350879646 ) ) ;
#21440 = FACE_OUTER_BOUND ( 'NONE', #84457, .T. ) ;
#21439 = CARTESIAN_POINT ( 'NONE',  ( -6.265495719280979259, 6.992744598377811371, -0.9808356887253886214 ) ) ;
#21441 = CARTESIAN_POINT ( 'NONE',  ( -0.2104748580754166598, -0.006608320950483163522, -2.103482951484026753 ) ) ;
#21442 = VERTEX_POINT ( 'NONE', #31612 ) ;
#21443 = CARTESIAN_POINT ( 'NONE',  ( 3.397389285588784169, 1.623555618760182062, 1.269252347208242870 ) ) ;
#21444 = CARTESIAN_POINT ( 'NONE',  ( -0.6801582343750247617, 0.09895833367471601472, -1.178068619123872729 ) ) ;
#21445 = CARTESIAN_POINT ( 'NONE',  ( -4.367698041896780126, 8.247398148854895084, 0.7998128361456481317 ) ) ;
#21446 = CARTESIAN_POINT ( 'NONE',  ( 3.023105066167310895, 5.702484939155337607, -2.419999999999995044 ) ) ;
#21447 = CARTESIAN_POINT ( 'NONE',  ( 4.009460741339333723, 5.700790169694431420, -1.599625672291256295 ) ) ;
#21448 = CIRCLE ( 'NONE', #142580, 0.07999999999999991840 ) ;
#21449 = CARTESIAN_POINT ( 'NONE',  ( 2.237249138949083171, -1.841491494976960075, 0.9254197329602343869 ) ) ;
#21451 = CARTESIAN_POINT ( 'NONE',  ( 0.6823417656249934904, 13.44270833367473195, 1.181850606188764807 ) ) ;
#21450 = CARTESIAN_POINT ( 'NONE',  ( -10.19171921354153554, 3.593199521514539807, -6.350946922499482561 ) ) ;
#21452 = CARTESIAN_POINT ( 'NONE',  ( 5.819474248763732760, 7.812472595022922128, -1.599625672291262513 ) ) ;
#21453 = DIRECTION ( 'NONE',  ( -8.638326563840814399E-31, 0.000000000000000000, -1.000000000000000000 ) ) ;
#21454 = EDGE_CURVE ( 'NONE', #78850, #29771, #5245, .T. ) ;
#21455 = CARTESIAN_POINT ( 'NONE',  ( 6.041676539500916654, -1.595688354349385607, -1.524751901930617715 ) ) ;
#21456 = CARTESIAN_POINT ( 'NONE',  ( 6.661402789601885033, 0.3967159107356016401, -2.227235065690711835 ) ) ;
#21457 = CARTESIAN_POINT ( 'NONE',  ( -3.945059511896602089, 7.546393830613923548, 1.040834085586084257E-14 ) ) ;
#21458 = CARTESIAN_POINT ( 'NONE',  ( 0.9191581010105540628, -1.820984308097562954, 0.8666112775468015617 ) ) ;
#21459 = CARTESIAN_POINT ( 'NONE',  ( 1.634533438177967923, 0.1689203749893586071, -2.292248917674902575 ) ) ;
#21460 = CARTESIAN_POINT ( 'NONE',  ( -4.278334434596112068, 3.985349064379731576, -0.2033706498285611231 ) ) ;
#21461 = CARTESIAN_POINT ( 'NONE',  ( -0.4355862708379995563, -6.583980363595115293, -9.606148981167580203 ) ) ;
#21462 = CARTESIAN_POINT ( 'NONE',  ( 1.498681428038322050, 1.531199225506232553, -1.074333469806128427 ) ) ;
#21463 = CARTESIAN_POINT ( 'NONE',  ( 3.257046257486408969, 0.04465439498414420366, -2.016188763087948033 ) ) ;
#21465 = CARTESIAN_POINT ( 'NONE',  ( -6.471393748265538370, 5.229711127717889596, -2.419999999999995044 ) ) ;
#21464 = CARTESIAN_POINT ( 'NONE',  ( -1.201851678989727383E-14, 1.071875000341418138, 1.575800808251672791 ) ) ;
#21467 = CARTESIAN_POINT ( 'NONE',  ( 5.567048526788405560, -1.903460050192711028, -0.9016015758830184801 ) ) ;
#21466 = CARTESIAN_POINT ( 'NONE',  ( -6.855619230004478482, 11.14997286831390788, -0.7998128361456291469 ) ) ;
#21468 = CARTESIAN_POINT ( 'NONE',  ( 6.096362627639171805, 10.26417349888772179, -0.7998128361456291469 ) ) ;
#21470 = CARTESIAN_POINT ( 'NONE',  ( -8.227100285394159940, 8.492705175914988303, 0.7998128361456602331 ) ) ;
#21469 = CARTESIAN_POINT ( 'NONE',  ( 5.598591087800349086, 5.496387455380669529, -0.7998128361456481317 ) ) ;
#21471 = CARTESIAN_POINT ( 'NONE',  ( -0.1589091098076596542, -6.723650695528558430, -9.611540586923219109 ) ) ;
#21472 = CARTESIAN_POINT ( 'NONE',  ( 3.568621913994294292, 0.7309530501433506577, 1.883054584751037819 ) ) ;
#21473 = CARTESIAN_POINT ( 'NONE',  ( -1.201851678989727383E-14, 4.946875000341420581, -1.575800808251660134 ) ) ;
#21474 = CARTESIAN_POINT ( 'NONE',  ( 0.8837254586576195337, -1.959797800638187093, 0.6432524670345032280 ) ) ;
#21475 = CARTESIAN_POINT ( 'NONE',  ( 6.954969614130424027, 11.05795561655343384, 1.040834085586084257E-14 ) ) ;
#21476 = CARTESIAN_POINT ( 'NONE',  ( 5.431013727915853906, 0.1530101862373678123, 2.156222312673663488 ) ) ;
#21477 = CARTESIAN_POINT ( 'NONE',  ( 6.984385409695311964, 8.177479728513226576, 1.199719254218452935 ) ) ;
#21478 = CARTESIAN_POINT ( 'NONE',  ( 0.6823417656249882723, -0.09479166632524876901, 1.181850606188755259 ) ) ;
#21480 = CARTESIAN_POINT ( 'NONE',  ( 9.649519181572159710, 4.269047846895349885, -7.134145857028189042 ) ) ;
#21479 = CARTESIAN_POINT ( 'NONE',  ( 5.505492895601038938, 8.580769590579979678, -1.199719254218452047 ) ) ;
#21481 = CARTESIAN_POINT ( 'NONE',  ( 8.120970824461352322, 9.537182719035495637, -1.082531754730543083 ) ) ;
#21483 = CARTESIAN_POINT ( 'NONE',  ( 6.520158902582616101, 5.290451655907108197, 2.438235897557466281 ) ) ;
#21482 = CARTESIAN_POINT ( 'NONE',  ( 3.016274402391531773, 2.160936140102893255, -0.2104436154053441199 ) ) ;
#21485 = CARTESIAN_POINT ( 'NONE',  ( 1.821575194732877545, 1.059174331173462935, -1.505913648122420900 ) ) ;
#21484 = CARTESIAN_POINT ( 'NONE',  ( -5.178851490740209229, 7.065079377328788546, 1.443375672974064550 ) ) ;
#21486 = CARTESIAN_POINT ( 'NONE',  ( -1.364683531250012516, 3.238541667008084879, -0.7879004041258289570 ) ) ;
#21487 = CARTESIAN_POINT ( 'NONE',  ( 3.439196427729715566, -1.660734982795486481, -1.430121640581414111 ) ) ;
#21488 = CARTESIAN_POINT ( 'NONE',  ( 6.883263157960364254, 2.038911835798001171, 2.358809022084580764 ) ) ;
#21489 = CARTESIAN_POINT ( 'NONE',  ( 4.417028899805944597, 2.066919071766720517, 0.9206345982136554529 ) ) ;
#21490 = CARTESIAN_POINT ( 'NONE',  ( -4.530395885260773525, 8.437212299446219532, 0.7998128361456481317 ) ) ;
#21491 = CARTESIAN_POINT ( 'NONE',  ( -1.201851678989727383E-14, 5.759375000341417028, -1.575800808251660801 ) ) ;
#21492 = CARTESIAN_POINT ( 'NONE',  ( 6.292946923374557855, 6.878031543426355476, -0.7329977330566839200 ) ) ;
#21493 = CARTESIAN_POINT ( 'NONE',  ( -1.500000000000015099, 13.72916666666666607, -0.8660254037844309360 ) ) ;
#21494 = CARTESIAN_POINT ( 'NONE',  ( -6.902509602688830626, 7.225551755991315162, -0.7216878364870338292 ) ) ;
#21495 = CARTESIAN_POINT ( 'NONE',  ( 6.048345925472191631, 6.229027465905275562, 0.7216878364870328300 ) ) ;
#21496 = CARTESIAN_POINT ( 'NONE',  ( 5.782415762239879520, -1.726843194930051562, -0.3863986657466413899 ) ) ;
#21497 = VECTOR ( 'NONE', #182075, 1000.000000000000000 ) ;
#21498 = CARTESIAN_POINT ( 'NONE',  ( 3.457684585873057159, -1.525941150838805216, -1.313146537923309376 ) ) ;
#21499 = CARTESIAN_POINT ( 'NONE',  ( 7.934546212495622086, 10.28005655271014795, -1.599625672291262513 ) ) ;
#21500 = CARTESIAN_POINT ( 'NONE',  ( 1.395691461817370804, 1.594359505120213960, 1.375974583626845993 ) ) ;
#21501 = CARTESIAN_POINT ( 'NONE',  ( -1.364683531250010295, 12.13020833367473017, 0.7879004041258445001 ) ) ;
#21502 = CARTESIAN_POINT ( 'NONE',  ( 2.453506318599480096, 1.520516184767862100, 1.251830903418025054 ) ) ;
#21503 = CARTESIAN_POINT ( 'NONE',  ( -9.345711740228626496, 15.44303320414337222, -7.452166123625171501 ) ) ;
#21505 = VERTEX_POINT ( 'NONE', #97687 ) ;
#21504 = CARTESIAN_POINT ( 'NONE',  ( 5.765820309002536170, 0.5175119463115984697, -1.736122601384345820 ) ) ;
#21506 = CARTESIAN_POINT ( 'NONE',  ( 6.697364695470787943, 7.876308901879812474, -1.082531754730543083 ) ) ;
#21507 = CARTESIAN_POINT ( 'NONE',  ( 0.2248163340835918345, 3.434981140918095477, -1.989104691395113367 ) ) ;
#21508 = CARTESIAN_POINT ( 'NONE',  ( 5.014452206985246185, 1.289541220462528504, -1.355370375751355105 ) ) ;
#21509 = CARTESIAN_POINT ( 'NONE',  ( 5.594608825991118195, 2.038665915018455177, 0.3594684214384344378 ) ) ;
#21510 = CARTESIAN_POINT ( 'NONE',  ( -5.438229012412899799, 7.437962829272074750, -1.443375672974066548 ) ) ;
#21511 = CARTESIAN_POINT ( 'NONE',  ( 1.499999999999987121, 0.7958333333333510451, -0.8660254037844253849 ) ) ;
#21512 = CARTESIAN_POINT ( 'NONE',  ( 6.913768267964901071, 10.15348118167935709, -1.199719254218441611 ) ) ;
#21513 = CARTESIAN_POINT ( 'NONE',  ( -8.045874094706015001, 11.47427131287732927, -1.199719254218446718 ) ) ;
#21514 = CARTESIAN_POINT ( 'NONE',  ( 5.182959862174088883, 9.268813282503625572, 0.7998128361456331437 ) ) ;
#21515 = CARTESIAN_POINT ( 'NONE',  ( -1.402160292154681736E-14, -0.6781249996585819728, 1.575800808251672791 ) ) ;
#21516 = EDGE_LOOP ( 'NONE', ( #109719, #67136, #1048, #182706 ) ) ;
#21517 = CARTESIAN_POINT ( 'NONE',  ( -0.7500000000000215383, 0.9416666666666878571, 1.299038105676659116 ) ) ;
#21519 = CARTESIAN_POINT ( 'NONE',  ( 3.811813743736467419, 7.598866467667865443, 1.040834085586084257E-14 ) ) ;
#21518 = CARTESIAN_POINT ( 'NONE',  ( 4.844172697165038066, -0.9265620464425131653, 1.729294158640543699 ) ) ;
#21520 = CARTESIAN_POINT ( 'NONE',  ( 2.934922540206804875, 1.076151813804010926, 1.704677747124828446 ) ) ;
#21521 = CARTESIAN_POINT ( 'NONE',  ( 1.991283197800724825, -0.4156388933829333610, 1.869923353789121556 ) ) ;
#21522 = FACE_OUTER_BOUND ( 'NONE', #3845, .T. ) ;
#21523 = CARTESIAN_POINT ( 'NONE',  ( 0.8025787753177977546, 1.655945718051672566, -1.435626523826734280 ) ) ;
#21524 =( BOUNDED_SURFACE ( )  B_SPLINE_SURFACE ( 3, 2, ( 
 ( #118024, #115886, #48708 ),
 ( #182951, #84390, #162460 ),
 ( #15108, #2037, #14036 ),
 ( #166714, #81197, #68107 ),
 ( #164578, #16163, #180820 ),
 ( #51902, #49760, #82248 ),
 ( #148339, #150477, #31390 ),
 ( #163521, #147275, #47659 ),
 ( #197071, #134243, #32447 ),
 ( #199179, #96410, #213307 ),
 ( #64932, #200250, #97465 ),
 ( #131082, #198128, #181871 ),
 ( #80122, #98516, #34566 ),
 ( #113770, #100637, #146227 ) ),
 .UNSPECIFIED., .F., .F., .T. ) 
 B_SPLINE_SURFACE_WITH_KNOTS ( ( 4, 2, 2, 2, 2, 2, 4 ),
 ( 3, 3 ),
 ( 5.529431079676072613E-18, 0.0003635382096235338103, 0.0007270764192470620911, 0.001090614628870590318, 0.001454152838494118761, 0.002181229257741175431, 0.002908305676988231885 ),
 ( 0.000000000000000000, 1.000000000000000000 ),
 .UNSPECIFIED. ) 
 GEOMETRIC_REPRESENTATION_ITEM ( )  RATIONAL_B_SPLINE_SURFACE ( (
 ( 1.000000000000000000, 0.8435419936913700623, 1.000000000000000000),
 ( 1.000000000000000000, 0.8440768467786702312, 1.000000000000000000),
 ( 1.000000000000000000, 0.8446657806964728010, 1.000000000000000000),
 ( 1.000000000000000000, 0.8458791039628983377, 1.000000000000000000),
 ( 1.000000000000000000, 0.8464799219268367425, 1.000000000000000000),
 ( 1.000000000000000000, 0.8478096660418573682, 1.000000000000000000),
 ( 1.000000000000000000, 0.8485318165228228349, 1.000000000000000000),
 ( 1.000000000000000000, 0.8497005200740803676, 1.000000000000000000),
 ( 1.000000000000000000, 0.8500955636246768643, 1.000000000000000000),
 ( 1.000000000000000000, 0.8503664178925908201, 1.000000000000000000),
 ( 1.000000000000000000, 0.8504660752369725962, 1.000000000000000000),
 ( 1.000000000000000000, 0.8507447348240169127, 1.000000000000000000),
 ( 1.000000000000000000, 0.8509461865225793620, 1.000000000000000000),
 ( 1.000000000000000000, 0.8509626965061065640, 1.000000000000000000) ) ) 
 REPRESENTATION_ITEM ( '' )  SURFACE ( )  );
#21525 = FACE_OUTER_BOUND ( 'NONE', #20848, .T. ) ;
#21526 = CARTESIAN_POINT ( 'NONE',  ( 2.671000074538076863, 0.09590037325727870932, -1.868228684465601752 ) ) ;
#21527 = CARTESIAN_POINT ( 'NONE',  ( -1.201851678989727383E-14, 5.696875000341416140, -1.575800808251660134 ) ) ;
#21528 = CARTESIAN_POINT ( 'NONE',  ( 4.324480843662709795, -0.8647720088908043001, -1.818167814553457884 ) ) ;
#21529 =( REPRESENTATION_RELATIONSHIP ('NONE','NONE', #84563, #62426 ) REPRESENTATION_RELATIONSHIP_WITH_TRANSFORMATION ( #193264 )SHAPE_REPRESENTATION_RELATIONSHIP( ) );
#21530 = CARTESIAN_POINT ( 'NONE',  ( -8.320953590485107298, 10.73086516036454618, 1.599625672291269396 ) ) ;
#21532 = CARTESIAN_POINT ( 'NONE',  ( 4.376635333690025220, -0.4654363970535125294, -2.065280895323940324 ) ) ;
#21531 = CARTESIAN_POINT ( 'NONE',  ( -4.880572111239580124, 7.677455982212699759, 1.082531754730560403 ) ) ;
#21534 = ADVANCED_FACE ( 'NONE', ( #203399 ), #163745, .T. ) ;
#21533 = DIRECTION ( 'NONE',  ( -0.000000000000000000, 1.000000000000000000, -0.000000000000000000 ) ) ;
#21535 = CARTESIAN_POINT ( 'NONE',  ( 5.863751307568212390, -0.5067217619753560109, 2.007263066363853987 ) ) ;
#21537 = CARTESIAN_POINT ( 'NONE',  ( 11.86239285000045918, 13.87999999999998302, 1.812080536912751283 ) ) ;
#21536 = CARTESIAN_POINT ( 'NONE',  ( 1.505537475160537264, -2.074567991729712180, 0.2591490344204059881 ) ) ;
#21539 = VERTEX_POINT ( 'NONE', #213517 ) ;
#21538 = CARTESIAN_POINT ( 'NONE',  ( 5.948246703923279810, 1.823645139926059144, 0.08696428134234018836 ) ) ;
#21540 = CARTESIAN_POINT ( 'NONE',  ( 6.588372581236919601, 9.773852880496709972, -1.199719254218440723 ) ) ;
#21541 = CARTESIAN_POINT ( 'NONE',  ( -3.791842586888578559, 7.437917094763062842, 0.3113814200439020130 ) ) ;
#21542 = CARTESIAN_POINT ( 'NONE',  ( -9.429696025003076798, 5.003427382976973981, 6.891771494149568689 ) ) ;
#21543 = CARTESIAN_POINT ( 'NONE',  ( 7.904040366642699489, 8.323727970612377902, 0.7216878364870458196 ) ) ;
#21544 = CARTESIAN_POINT ( 'NONE',  ( 0.09094460184115825407, 13.35659826982236531, -1.523293917897329708 ) ) ;
#21545 = CARTESIAN_POINT ( 'NONE',  ( 0.8557779741884026237, 0.7350315055517571139, -1.655818919202347361 ) ) ;
#21546 = CARTESIAN_POINT ( 'NONE',  ( -7.483210719738908168, 10.81783070874899799, 1.199719254218453823 ) ) ;
#21547 = CARTESIAN_POINT ( 'NONE',  ( 5.035963992472171746, 7.962709526937818083, 1.199719254218462483 ) ) ;
#21548 = PLANE ( 'NONE',  #204533 ) ;
#21549 = CARTESIAN_POINT ( 'NONE',  ( 4.351804119862229037, 4.179452349368450115, -0.7216878364870188411 ) ) ;
#21550 = CARTESIAN_POINT ( 'NONE',  ( -1.420000000000056550, 7.388542872122504157, -4.154462424328204229 ) ) ;
#21551 = CARTESIAN_POINT ( 'NONE',  ( 4.220665892555866883, 3.818531717603609987, -0.7998128361456211532 ) ) ;
#21552 = VERTEX_POINT ( 'NONE', #32659 ) ;
#21553 = CARTESIAN_POINT ( 'NONE',  ( 5.694935465533643715, 1.779635825068434984, 0.9480254120717497290 ) ) ;
#21554 = CARTESIAN_POINT ( 'NONE',  ( 0.6980877996264934771, 1.427081234210248573, 1.568565553304770877 ) ) ;
#21555 = CARTESIAN_POINT ( 'NONE',  ( 1.034320804586478904, -6.966782166145887105E-15, -0.7758101520237091764 ) ) ;
#21556 = AXIS2_PLACEMENT_3D ( 'NONE', #178138, #147771, #132607 ) ;
#21557 = AXIS2_PLACEMENT_3D ( 'NONE', #32804, #16523, #113060 ) ;
#21558 = CARTESIAN_POINT ( 'NONE',  ( -0.1394461523061195918, 0.2309855492786689335, -2.314897844796594661 ) ) ;
#21559 = EDGE_CURVE ( 'NONE', #189420, #63704, #191329, .T. ) ;
#21560 = CARTESIAN_POINT ( 'NONE',  ( -4.107757355260591936, 7.736207981205250661, 1.040834085586084257E-14 ) ) ;
#21561 = CARTESIAN_POINT ( 'NONE',  ( 9.029367117021314115, 12.51771682229149008, -1.082531754730543083 ) ) ;
#21562 = CARTESIAN_POINT ( 'NONE',  ( 3.555474331475856786, 1.549626312082365898, 1.215309171139463684 ) ) ;
#21563 = CARTESIAN_POINT ( 'NONE',  ( 4.499625164952708367, -1.976952908697379607, 0.3961224619316304763 ) ) ;
#21564 = CARTESIAN_POINT ( 'NONE',  ( -6.880926654135487652, 7.986501503701545879, 1.199719254218450271 ) ) ;
#21565 = DIRECTION ( 'NONE',  ( -8.638326563840814399E-31, 0.000000000000000000, -1.000000000000000000 ) ) ;
#21566 = CARTESIAN_POINT ( 'NONE',  ( 4.312563266315373234, 2.003113633248252867, 0.8892094534625747393 ) ) ;
#21567 = CARTESIAN_POINT ( 'NONE',  ( 3.153258193586833347, -1.574033464040735408, -1.110325110657943481 ) ) ;
#21568 = CARTESIAN_POINT ( 'NONE',  ( -7.857113714319432063, 9.125386407249497012, 1.199719254218462483 ) ) ;
#21569 = CARTESIAN_POINT ( 'NONE',  ( -0.02968770228140017037, 2.049257630910449990, -2.243713227073070637 ) ) ;
#21570 = CARTESIAN_POINT ( 'NONE',  ( 0.3291288957359936318, 2.113116833900237967, 0.6364493931270903682 ) ) ;
#21571 = CARTESIAN_POINT ( 'NONE',  ( 1.220146605508150803E-14, 11.68749999999999822, -1.499999999999998446 ) ) ;
#21572 = ORIENTED_EDGE ( 'NONE', *, *, #12043, .T. ) ;
#21573 = CARTESIAN_POINT ( 'NONE',  ( 5.424670859243587273, 5.501406555305196733, -0.7216878364870458196 ) ) ;
#21574 = CARTESIAN_POINT ( 'NONE',  ( 4.838697515689712958, -1.909247481386136647, -0.4825833779809485802 ) ) ;
#21576 = CARTESIAN_POINT ( 'NONE',  ( 4.266274873615797603, 2.012593780953766842, -0.05172614775082911426 ) ) ;
#21575 = CARTESIAN_POINT ( 'NONE',  ( 0.3275467377269140057, 0.9974989819340736030, -1.666164454441501297 ) ) ;
#21577 = CARTESIAN_POINT ( 'NONE',  ( 5.360842878201462547, -0.8341330746063200241, 2.141841041818067559 ) ) ;
#21579 = CARTESIAN_POINT ( 'NONE',  ( 3.432308073483012922, -1.112138214925220803, 1.491878268611693814 ) ) ;
#21578 =( NAMED_UNIT ( * ) SI_UNIT ( $, .STERADIAN. ) SOLID_ANGLE_UNIT ( ) );
#21580 = CARTESIAN_POINT ( 'NONE',  ( 7.374709211190586089, 7.568525266002632534, 0.000000000000000000 ) ) ;
#21581 = CARTESIAN_POINT ( 'NONE',  ( -1.500000000000008216, 11.49999999999999645, 3.469446951953614189E-15 ) ) ;
#21582 = DIRECTION ( 'NONE',  ( 0.000000000000000000, 0.000000000000000000, -1.000000000000000000 ) ) ;
#21583 = CARTESIAN_POINT ( 'NONE',  ( -5.696397096036042385, 9.797547045350714967, -0.7998128361456231517 ) ) ;
#21584 = CARTESIAN_POINT ( 'NONE',  ( -4.746763178560296836, 6.631252689777363152, 1.443375672974058777 ) ) ;
#21585 = CARTESIAN_POINT ( 'NONE',  ( 0.5213437761196970666, -2.079166062760181788, 0.6930039600180630810 ) ) ;
#21586 = CARTESIAN_POINT ( 'NONE',  ( 6.670248388243460447, 6.884303995813253252, -0.7216878364870257245 ) ) ;
#21587 = VERTEX_POINT ( 'NONE', #81414 ) ;
#21588 = AXIS2_PLACEMENT_3D ( 'NONE', #144020, #157042, #41164 ) ;
#21589 = CARTESIAN_POINT ( 'NONE',  ( 9.818302567231148359, -8.862962251182139539, -0.6073963244357859503 ) ) ;
#21590 = CARTESIAN_POINT ( 'NONE',  ( -9.540655113774947793, 4.518467169708413778, -7.145788969735951568 ) ) ;
#21591 = CARTESIAN_POINT ( 'NONE',  ( 0.8908993799596062191, 1.611356928563783208, -0.8583080905386344384 ) ) ;
#21592 = CARTESIAN_POINT ( 'NONE',  ( -5.005985031943793295, 6.863401842066301661, -1.599625672291256295 ) ) ;
#21593 = CARTESIAN_POINT ( 'NONE',  ( 2.338123177510130102, 0.4612838472501363252, -1.671594290515050041 ) ) ;
#21594 = CARTESIAN_POINT ( 'NONE',  ( 1.224999999999958789, 1.916666667349501196, 0.7072540797572717253 ) ) ;
#21595 = CARTESIAN_POINT ( 'NONE',  ( 6.509000000000012776, 0.5843741663743782233, 2.053293374786519188 ) ) ;
#21596 = CARTESIAN_POINT ( 'NONE',  ( -6.392833124043511894, 7.417059051927569868, 1.199719254218450271 ) ) ;
#21597 = CARTESIAN_POINT ( 'NONE',  ( 1.084637062511527361, 3.307371192708035590, -1.105835307554789759 ) ) ;
#21598 = CARTESIAN_POINT ( 'NONE',  ( 0.3915760470782835845, -1.894197279051227811, 0.8358220917567968922 ) ) ;
#21599 = CARTESIAN_POINT ( 'NONE',  ( 5.373610676068619973, 1.758448663713826132, -0.4906839848310071139 ) ) ;
#21600 = CARTESIAN_POINT ( 'NONE',  ( 3.748837004188230182, -0.3782986639458625899, -1.924763881548184230 ) ) ;
#21601 = CARTESIAN_POINT ( 'NONE',  ( -3.755786496842897795E-14, -0.2499999993171491686, -1.414508159514577423 ) ) ;
#21602 = CARTESIAN_POINT ( 'NONE',  ( -9.124801077197171040, 10.60435499727357289, -1.199719254218441611 ) ) ;
#21603 = CARTESIAN_POINT ( 'NONE',  ( 5.764187864104357573, 9.876636274763768597, 1.040834085586084257E-14 ) ) ;
#21604 = CARTESIAN_POINT ( 'NONE',  ( 3.791739704763209318, 1.996120715041304061, -0.7158466834289513026 ) ) ;
#21605 = CARTESIAN_POINT ( 'NONE',  ( 6.827182134110198142, 6.033542260787205791, 2.783941933017803905 ) ) ;
#21606 = CARTESIAN_POINT ( 'NONE',  ( -9.378489572351046633, 11.96465713920816043, -1.599625672291263179 ) ) ;
#21607 = CARTESIAN_POINT ( 'NONE',  ( 1.323191598296684646, -1.869966582492128548, -0.8887066864657000576 ) ) ;
#21608 = CARTESIAN_POINT ( 'NONE',  ( -0.7500000000000006661, 15.23958333401612819, -1.299038105676657340 ) ) ;
#21610 = VERTEX_POINT ( 'NONE', #17450 ) ;
#21609 = CARTESIAN_POINT ( 'NONE',  ( 4.811300260135710438, 1.847242992945047568, -1.233362022257722845 ) ) ;
#21611 = CARTESIAN_POINT ( 'NONE',  ( 2.163060705912169812, 1.417378650759585357, 1.809622876518288681 ) ) ;
#21612 = CARTESIAN_POINT ( 'NONE',  ( 7.931156674314368438, 12.19684052010138586, 1.040834085586084257E-14 ) ) ;
#21614 = CARTESIAN_POINT ( 'NONE',  ( -3.475000000000000533, 0.000000000000000000, 0.000000000000000000 ) ) ;
#21613 = CARTESIAN_POINT ( 'NONE',  ( 7.526184669361807522, 7.953172667109813077, 0.000000000000000000 ) ) ;
#21615 = FACE_OUTER_BOUND ( 'NONE', #115763, .T. ) ;
#21616 = CARTESIAN_POINT ( 'NONE',  ( -10.93186801223271409, -5.758458176070771373, 3.167056189783827390E-15 ) ) ;
#21617 = ORIENTED_EDGE ( 'NONE', *, *, #95057, .T. ) ;
#21618 = CARTESIAN_POINT ( 'NONE',  ( -0.3931996164520709103, -9.201308816821677894, 9.491928691056637390 ) ) ;
#21619 = CARTESIAN_POINT ( 'NONE',  ( 2.654443970922310214, 1.898414275235399407, 0.2300336082040748686 ) ) ;
#21620 = CARTESIAN_POINT ( 'NONE',  ( -0.5448033855394223135, 6.555371112116565868, -3.373828149488691253 ) ) ;
#21621 = CARTESIAN_POINT ( 'NONE',  ( 3.750762392430748271, -1.410035727865316613, 0.9929894849482110430 ) ) ;
#21622 = CARTESIAN_POINT ( 'NONE',  ( 2.360564879530482330, -1.931125380751706810, -0.5807522007576990664 ) ) ;
#21623 = CARTESIAN_POINT ( 'NONE',  ( 4.043764476089898530, -1.703284420474758143, 1.543771250003633355 ) ) ;
#21624 = CARTESIAN_POINT ( 'NONE',  ( 3.532755146446086680, 2.206387722723508915, 0.4996636332569806549 ) ) ;
#21625 = CARTESIAN_POINT ( 'NONE',  ( 5.918611218600786650, 1.415673333675367296, -1.559471542009479350 ) ) ;
#21626 = CARTESIAN_POINT ( 'NONE',  ( -4.990809943606273613, 7.876343129965691858, -1.082531754730549967 ) ) ;
#21627 = CARTESIAN_POINT ( 'NONE',  ( 4.639784515242838303, 0.7573303825321504590, -1.599664492173937358 ) ) ;
#21629 = CARTESIAN_POINT ( 'NONE',  ( 1.060933235008169051, -2.074266264760935563, -0.9759354127518887756 ) ) ;
#21628 = CARTESIAN_POINT ( 'NONE',  ( 7.700104897918568447, 7.948153567185284096, 0.000000000000000000 ) ) ;
#21630 = CARTESIAN_POINT ( 'NONE',  ( 5.384640740818634974, 1.621930891500168670, -0.8712783443201177480 ) ) ;
#21631 = CARTESIAN_POINT ( 'NONE',  ( -4.731959306369413198, 5.479372931307791461, -1.199719254218446718 ) ) ;
#21632 = CARTESIAN_POINT ( 'NONE',  ( 5.841772037242090931, 2.188765561305112683, 0.1107676204459909497 ) ) ;
#21633 = CARTESIAN_POINT ( 'NONE',  ( -5.492988512192097161, 6.437516681426083132, 1.199719254218452935 ) ) ;
#21634 = CARTESIAN_POINT ( 'NONE',  ( 1.360316468749981800, -0.4739583329918962695, 0.7853790794158760358 ) ) ;
#21635 = CARTESIAN_POINT ( 'NONE',  ( 9.488641820551102057, -8.233137084989836652, -0.4644097342743017665 ) ) ;
#21636 = CARTESIAN_POINT ( 'NONE',  ( 6.355931484454268698, -0.7012994977402075003, 1.948090369817329526 ) ) ;
#21637 = CARTESIAN_POINT ( 'NONE',  ( 1.727750297885573882, 0.7672897036171549834, -1.865047645237365215 ) ) ;
#21638 = AXIS2_PLACEMENT_3D ( 'NONE', #76796, #158079, #105067 ) ;
#21639 = CARTESIAN_POINT ( 'NONE',  ( 1.499999999999987121, -0.9645833326505173222, 0.8660254037844524744 ) ) ;
#21640 = CARTESIAN_POINT ( 'NONE',  ( 4.055238279289786973, -1.602352113334176043, -1.069235405101864878 ) ) ;
#21641 = CARTESIAN_POINT ( 'NONE',  ( -0.6823417656250039265, 10.06770833367473550, -1.181850606188755259 ) ) ;
#21642 = CARTESIAN_POINT ( 'NONE',  ( 1.635333617853749200, 2.074933741853498770, 0.7937918740310870858 ) ) ;
#21644 = ORIENTED_EDGE ( 'NONE', *, *, #178677, .T. ) ;
#21643 = CARTESIAN_POINT ( 'NONE',  ( 2.838652716839808576, 6.463511936288419690, 0.1785095769484796591 ) ) ;
#21647 = AXIS2_PLACEMENT_3D ( 'NONE', #164071, #32989, #147820 ) ;
#21646 = CARTESIAN_POINT ( 'NONE',  ( 0.000000000000000000, 0.02011834319527033843, -6.938893903907228378E-15 ) ) ;
#21645 = CARTESIAN_POINT ( 'NONE',  ( 1.499999999999819256, 7.176846818246210624, -4.202462424328214041 ) ) ;
#21648 = CARTESIAN_POINT ( 'NONE',  ( -3.131570295076647525, 6.597323077657299528, 1.040834085586084257E-14 ) ) ;
#21649 = CARTESIAN_POINT ( 'NONE',  ( 4.566398809704347528, 4.221886787610169556, -0.7998128361456211532 ) ) ;
#21650 = DIRECTION ( 'NONE',  ( 0.000000000000000000, 0.000000000000000000, 1.000000000000000000 ) ) ;
#21651 = SURFACE_STYLE_FILL_AREA ( #183122 ) ;
#21652 = CARTESIAN_POINT ( 'NONE',  ( 4.722041168748464912, 1.667336974042502584, 0.4991589302964939412 ) ) ;
#21653 = CARTESIAN_POINT ( 'NONE',  ( 2.348037267531626338, -0.8415878996531295231, 1.772339229757218471 ) ) ;
#21655 = CARTESIAN_POINT ( 'NONE',  ( -0.6823417656250003738, 2.280208333674753174, -1.181850606188749264 ) ) ;
#21654 = CARTESIAN_POINT ( 'NONE',  ( 5.983225862332436584, 5.874851682342960402, 0.7998128361456341429 ) ) ;
#21656 = ADVANCED_FACE ( 'NONE', ( #65140 ), #13393, .T. ) ;
#21657 = CARTESIAN_POINT ( 'NONE',  ( -4.409122955247444686, 7.142713865425108111, 1.076920909521961622 ) ) ;
#21658 = CARTESIAN_POINT ( 'NONE',  ( 9.459838494033030898, 12.05956421450382088, 1.599625672291281386 ) ) ;
#21659 = CARTESIAN_POINT ( 'NONE',  ( 6.742638286788313451, -1.923764577213080029, -0.3838556375530403630 ) ) ;
#21660 = CARTESIAN_POINT ( 'NONE',  ( -8.941766003412679353, 10.39081407785832845, -1.199719254218446718 ) ) ;
#21661 = CARTESIAN_POINT ( 'NONE',  ( -5.734735788456164940, 5.792872629394710593, 0.7216878364870317197 ) ) ;
#21662 = CARTESIAN_POINT ( 'NONE',  ( 5.050017674172561755, 0.9981218692422781924, 1.752141108012375437 ) ) ;
#21663 = CARTESIAN_POINT ( 'NONE',  ( 1.534417833908331863, 1.113959020207640593, -1.969227013157865303 ) ) ;
#21665 = ORIENTED_EDGE ( 'NONE', *, *, #114498, .T. ) ;
#21664 = CARTESIAN_POINT ( 'NONE',  ( -6.566226467720086113, 6.555019055295208119, 1.040834085586084257E-14 ) ) ;
#21666 = CARTESIAN_POINT ( 'NONE',  ( 1.499999999999985123, -0.9229166659838452524, -0.8660254037844323793 ) ) ;
#21667 = CARTESIAN_POINT ( 'NONE',  ( 1.493192106177696044, 1.412881632968411516, 1.225925835885120829 ) ) ;
#21668 = CARTESIAN_POINT ( 'NONE',  ( 0.3340423123194468658, 0.5469568729883391711, -1.645723886551814452 ) ) ;
#21670 = CARTESIAN_POINT ( 'NONE',  ( 3.825867475279482566, 1.171244075711602051, -1.852137614134836907 ) ) ;
#21669 = CARTESIAN_POINT ( 'NONE',  ( 1.360316468749985575, 2.036458333674739940, -0.7853790794159022370 ) ) ;
#21671 = CARTESIAN_POINT ( 'NONE',  ( 5.456226512670824036, 2.305251103711564387, -0.1065007851034898423 ) ) ;
#21672 = CARTESIAN_POINT ( 'NONE',  ( 0.5849274615713345726, -0.2514902370338990001, -2.045404637917444646 ) ) ;
#21673 = CARTESIAN_POINT ( 'NONE',  ( 3.134642302965468641, -1.712256071497103349, 0.9161664635699683368 ) ) ;
#21674 = CARTESIAN_POINT ( 'NONE',  ( -4.378920427089552092, 8.052564898339037214, 0.7216878364870317197 ) ) ;
#21675 = DIRECTION ( 'NONE',  ( -0.6507913734559640506, -0.7592566023653004592, 0.000000000000000000 ) ) ;
#21676 = FACE_OUTER_BOUND ( 'NONE', #108148, .T. ) ;
#21677 = CARTESIAN_POINT ( 'NONE',  ( 3.885388821667290493, -0.6351983117205138862, -1.913803978180687482 ) ) ;
#21678 = CARTESIAN_POINT ( 'NONE',  ( -3.755245360860925086, 6.364574773437617239, -1.082531754730548412 ) ) ;
#21679 = CARTESIAN_POINT ( 'NONE',  ( -6.631873415740034083, 7.766215735565355160, 1.199719254218452047 ) ) ;
#21680 = CARTESIAN_POINT ( 'NONE',  ( 9.420217803396747414, 9.884675613584706255, 0.7998128361456462443 ) ) ;
#21682 = CARTESIAN_POINT ( 'NONE',  ( -6.672971353125990213, -7.009934032700016360, 6.761775799041313206 ) ) ;
#21681 = CARTESIAN_POINT ( 'NONE',  ( 0.8030139110496161692, 1.490934425176414502, 1.053415343471690857 ) ) ;
#21683 = CARTESIAN_POINT ( 'NONE',  ( -5.204350862799341115, 7.165104988056252289, -1.599625672291271394 ) ) ;
#21684 = CARTESIAN_POINT ( 'NONE',  ( -3.969505113751027547, 7.853116076009993840, 1.214306433183764966E-14 ) ) ;
#21685 = CARTESIAN_POINT ( 'NONE',  ( -11.69053533621101160, 4.400474013969419396, 5.144636342886200531 ) ) ;
#21686 = ORIENTED_EDGE ( 'NONE', *, *, #186211, .F. ) ;
#21687 = CARTESIAN_POINT ( 'NONE',  ( 6.737187473210400235, -1.842164534206979676, 0.9240717516781959961 ) ) ;
#21688 = CARTESIAN_POINT ( 'NONE',  ( -5.763624699140868834, 9.738329559057408602, -0.7216878364870338292 ) ) ;
#21689 = DIRECTION ( 'NONE',  ( 1.000000000000000000, 1.725633230170963762E-31, 8.638326563840814399E-31 ) ) ;
#21690 = CARTESIAN_POINT ( 'NONE',  ( -9.646789991323334590, 11.21334206375407305, 1.199719254218462483 ) ) ;
#21691 = CARTESIAN_POINT ( 'NONE',  ( 5.971354884044596467, -1.733367664992270685, -1.036320259733174209 ) ) ;
#21693 = EDGE_LOOP ( 'NONE', ( #104758, #54905, #191283, #98116 ) ) ;
#21692 = CARTESIAN_POINT ( 'NONE',  ( 6.182328207180960433, 1.139467527619671294, 1.906663674214443382 ) ) ;
#21694 = CARTESIAN_POINT ( 'NONE',  ( -5.901542003698421190, 10.10715911428198055, 0.000000000000000000 ) ) ;
#21695 = AXIS2_PLACEMENT_3D ( 'NONE', #156701, #106929, #11492 ) ;
#21696 = CARTESIAN_POINT ( 'NONE',  ( 6.063521013809720195, 8.097193820909906137, 1.599625672291281386 ) ) ;
#21697 = CARTESIAN_POINT ( 'NONE',  ( 5.278222320829740077, -1.146742738506721704, 1.712165125756033968 ) ) ;
#21698 = CARTESIAN_POINT ( 'NONE',  ( 4.447888798048591497, -1.802416534049579910, -0.9041112711936499791 ) ) ;
#21699 = VERTEX_POINT ( 'NONE', #48926 ) ;
#21700 = CYLINDRICAL_SURFACE ( 'NONE', #190671, 0.08000000000000041800 ) ;
#21701 = CARTESIAN_POINT ( 'NONE',  ( 4.325214697959421706, 5.004837554829479451, 1.199719254218462483 ) ) ;
#21703 = ORIENTED_EDGE ( 'NONE', *, *, #146654, .F. ) ;
#21702 = CARTESIAN_POINT ( 'NONE',  ( -7.391130018105325661, 8.652015104991543026, -1.199719254218452047 ) ) ;
#21704 = CARTESIAN_POINT ( 'NONE',  ( 4.710809438828709617, 8.349644928513606956, 0.6747337923850562635 ) ) ;
#21705 = CARTESIAN_POINT ( 'NONE',  ( 4.024767406304472495, 2.001204788683898617, -0.2439926020210633206 ) ) ;
#21706 = CARTESIAN_POINT ( 'NONE',  ( 3.204851553285171573, -0.3583046703147829137, 1.805758307424263354 ) ) ;
#21707 = ADVANCED_FACE ( 'NONE', ( #137383 ), #179480, .T. ) ;
#21708 = DIRECTION ( 'NONE',  ( 0.000000000000000000, 0.000000000000000000, 1.000000000000000000 ) ) ;
#21709 = CARTESIAN_POINT ( 'NONE',  ( 2.262750896497740527, 0.9887190084108381516, 2.085292768615305992 ) ) ;
#21710 = CARTESIAN_POINT ( 'NONE',  ( 5.032011289327418702, 5.899709921417326974, 1.199719254218452935 ) ) ;
#21711 = CARTESIAN_POINT ( 'NONE',  ( 4.358765367649009903, -1.604958417591015207, 1.448176592534822005 ) ) ;
#21712 = CARTESIAN_POINT ( 'NONE',  ( 9.284636267260101050, 9.726497154758602548, -0.7998128361456281477 ) ) ;
#21713 = CARTESIAN_POINT ( 'NONE',  ( -0.07675543424010172755, -1.195724141806488561, -1.531021551883532172 ) ) ;
#21714 = CARTESIAN_POINT ( 'NONE',  ( -4.062639585589296942, 7.891496616496157301, 0.7998128361456341429 ) ) ;
#21715 = CARTESIAN_POINT ( 'NONE',  ( -0.9738393980073648537, 15.51858052053983172, 11.99373428513897188 ) ) ;
#21716 = FACE_OUTER_BOUND ( 'NONE', #12497, .T. ) ;
#21717 = STYLED_ITEM ( 'NONE', ( #52924 ), #77868 ) ;
#21718 = CARTESIAN_POINT ( 'NONE',  ( 2.553401164250346245, 0.5009360343536627402, -1.802255699741683870 ) ) ;
#21719 = VECTOR ( 'NONE', #71573, 1000.000000000000000 ) ;
#21720 = CARTESIAN_POINT ( 'NONE',  ( 6.561403051094389483, 0.3373947195176879021, -1.942235834477159084 ) ) ;
#21723 = EDGE_CURVE ( 'NONE', #34262, #135468, #169100, .T. ) ;
#21722 = CARTESIAN_POINT ( 'NONE',  ( -6.505933609711270549, 8.683618192786854095, -1.599625672291271394 ) ) ;
#21721 = CARTESIAN_POINT ( 'NONE',  ( 1.364683531249990311, 5.134375000341417916, 1.214306433183764966E-14 ) ) ;
#21724 = CARTESIAN_POINT ( 'NONE',  ( 1.963769682107346037, 0.3752889857368995608, -2.174583152744386627 ) ) ;
#21725 = EDGE_LOOP ( 'NONE', ( #131808, #96762, #164675, #104687 ) ) ;
#21726 = DIRECTION ( 'NONE',  ( 0.7592566023653004592, 0.6507913734559639396, 0.000000000000000000 ) ) ;
#21727 = CARTESIAN_POINT ( 'NONE',  ( 4.813308228051395687, 5.574280006603454574, 1.199719254218462483 ) ) ;
#21728 = CARTESIAN_POINT ( 'NONE',  ( -3.249150368769345043, 6.942425863539538611, 0.7998128361456341429 ) ) ;
#21729 = CARTESIAN_POINT ( 'NONE',  ( 3.019342412789784547, 6.452475500722323787, 0.1501914610189964416 ) ) ;
#21730 = CARTESIAN_POINT ( 'NONE',  ( 5.946159419501746868, 1.969187058922382993, 0.09738397392708775246 ) ) ;
#21731 = ADVANCED_FACE ( 'NONE', ( #5194, #186100 ), #181044, .F. ) ;
#21732 = CARTESIAN_POINT ( 'NONE',  ( 5.479250216003205054, -0.05159697844352681417, -2.307286710698839727 ) ) ;
#21733 = CARTESIAN_POINT ( 'NONE',  ( 0.2210476084268316321, -1.750679471464357650, -0.8856473702157914296 ) ) ;
#21734 = CARTESIAN_POINT ( 'NONE',  ( 4.329007229187351591, -1.922695762783795947, -0.7470244877981512266 ) ) ;
#21735 = CARTESIAN_POINT ( 'NONE',  ( 5.260200412422194383, 7.159986452624450770, -1.443375672974051449 ) ) ;
#21736 = CARTESIAN_POINT ( 'NONE',  ( 7.289443866002793371, 8.533381260871966134, 1.199719254218452047 ) ) ;
#21737 = CARTESIAN_POINT ( 'NONE',  ( 6.426201622753093368, 10.44105962661321563, 1.040834085586084257E-14 ) ) ;
#21738 = CARTESIAN_POINT ( 'NONE',  ( 0.6823417656249899377, 3.488541667008085323, -1.181850606188754593 ) ) ;
#21739 = CARTESIAN_POINT ( 'NONE',  ( -10.29157903258815487, 3.766103264033962450, -6.172328895365623680 ) ) ;
#21740 = CARTESIAN_POINT ( 'NONE',  ( 4.134873662043553111, 7.767843672452050541, -0.7216878364870197293 ) ) ;
#21741 = CARTESIAN_POINT ( 'NONE',  ( 6.531686450800388677, 2.079676181002787061, -0.6237389289161490158 ) ) ;
#21742 = CARTESIAN_POINT ( 'NONE',  ( -0.02984615528259876305, 7.053682067332115224, -3.954834431657083371 ) ) ;
#21744 = CARTESIAN_POINT ( 'NONE',  ( 5.372543328820884589, -0.05112055865702340440, -1.840719716649619198 ) ) ;
#21743 = CARTESIAN_POINT ( 'NONE',  ( 1.224999999999965006, 0.4166666673494940354, 0.7072540797572456350 ) ) ;
#21745 = DIRECTION ( 'NONE',  ( -8.638326563840814399E-31, 0.000000000000000000, -1.000000000000000000 ) ) ;
#21746 = CARTESIAN_POINT ( 'NONE',  ( 6.216381822182693639, 2.044192415450503120, 0.7905562269360306704 ) ) ;
#21747 = CARTESIAN_POINT ( 'NONE',  ( 0.1806930697454533219, -0.1309388314422038346, -1.840455529407057256 ) ) ;
#21749 = CARTESIAN_POINT ( 'NONE',  ( -5.328671718129330159, 6.540706332611327944, 1.372188321006672540 ) ) ;
#21748 = AXIS2_PLACEMENT_3D ( 'NONE', #49886, #34688, #181997 ) ;
#21750 = CARTESIAN_POINT ( 'NONE',  ( -10.85353573482952072, -6.836568542495036205, 0.4635785636673775967 ) ) ;
#21751 = CARTESIAN_POINT ( 'NONE',  ( 5.997720278586790243, 7.186234674792547850, 1.197368251494409286 ) ) ;
#21752 = CARTESIAN_POINT ( 'NONE',  ( 0.4516295384478057895, -1.352486712789632950, -1.352142238705160704 ) ) ;
#21753 = CARTESIAN_POINT ( 'NONE',  ( 2.078617942332625201, -0.08328603760934982780, -1.768007077409910588 ) ) ;
#21754 = CARTESIAN_POINT ( 'NONE',  ( 6.358070405704149941, 0.7683137238208622710, -1.860897411154702530 ) ) ;
#21756 = CARTESIAN_POINT ( 'NONE',  ( 4.095261013068919098, -0.3237038700398958690, 1.887879439767611744 ) ) ;
#21755 = CARTESIAN_POINT ( 'NONE',  ( -8.992082194361570302, 11.51384853155376220, 1.599625672291269396 ) ) ;
#21757 = CARTESIAN_POINT ( 'NONE',  ( -1.530148271428807716, 1.292818251517726447, 1.500000000002693623 ) ) ;
#21758 = CARTESIAN_POINT ( 'NONE',  ( 5.705506402468259353, -1.551454039220935055, -1.213164361648248368 ) ) ;
#21759 = CARTESIAN_POINT ( 'NONE',  ( 0.1938080739139167730, 1.976361990896974508, -0.7691651810952588875 ) ) ;
#21760 = FACE_OUTER_BOUND ( 'NONE', #172155, .T. ) ;
#21761 = CARTESIAN_POINT ( 'NONE',  ( 2.377632874612686020, 1.149002834218125102, 1.476114537088555112 ) ) ;
#21763 = EDGE_LOOP ( 'NONE', ( #111698, #171731, #28810, #155056, #176706 ) ) ;
#21762 = CARTESIAN_POINT ( 'NONE',  ( 5.883370885758751001, 1.591107372635025330, -0.6665480857693687478 ) ) ;
#21765 = CARTESIAN_POINT ( 'NONE',  ( 2.548569689688999329, 5.917155704705049146, -0.7216878364870267237 ) ) ;
#21764 = CARTESIAN_POINT ( 'NONE',  ( 3.229339687698820072, 0.05429069646168545316, 2.206380697113208722 ) ) ;
#21766 = CARTESIAN_POINT ( 'NONE',  ( 0.6823417656249899377, 3.488541667008085323, -1.181850606188754593 ) ) ;
#21767 = CARTESIAN_POINT ( 'NONE',  ( 1.258340527071156956, -2.062851378465610175, -0.001992840727984764547 ) ) ;
#21768 = CARTESIAN_POINT ( 'NONE',  ( 7.613066949273408213, 8.840665181362512115, -1.199719254218441611 ) ) ;
#21769 = CARTESIAN_POINT ( 'NONE',  ( -9.236128959407555072, 11.79856975744075598, -1.599625672291263179 ) ) ;
#21770 = CARTESIAN_POINT ( 'NONE',  ( -4.765854690403601879, 5.518917546014321829, 1.199719254218462483 ) ) ;
#21771 = LINE ( 'NONE', #55378, #206684 ) ;
#21772 = VERTEX_POINT ( 'NONE', #37730 ) ;
#21773 = CARTESIAN_POINT ( 'NONE',  ( 3.174344110969638866, -1.018096006688212096, -1.802650257252853772 ) ) ;
#21774 = CARTESIAN_POINT ( 'NONE',  ( -0.7500000000000215383, 4.191666666666690411, 1.299038105676671107 ) ) ;
#21775 = CARTESIAN_POINT ( 'NONE',  ( 5.983225862332436584, 5.874851682342960402, 0.7998128361456341429 ) ) ;
#21776 = CARTESIAN_POINT ( 'NONE',  ( -6.111218785694742195, 7.101581614182197022, 1.130138924470771800 ) ) ;
#21777 = CARTESIAN_POINT ( 'NONE',  ( 1.119792439799172978, -0.4886160933238526405, 1.959555815251372568 ) ) ;
#21778 = DIRECTION ( 'NONE',  ( 1.000000000000000000, 0.000000000000000000, 0.000000000000000000 ) ) ;
#21779 = CARTESIAN_POINT ( 'NONE',  ( 1.364683531249988535, 3.363541667008084879, 0.7879004041258500513 ) ) ;
#21780 = EDGE_LOOP ( 'NONE', ( #81064, #36126, #92101, #200527 ) ) ;
#21782 = CARTESIAN_POINT ( 'NONE',  ( 7.931156674314368438, 12.19684052010138586, 1.040834085586084257E-14 ) ) ;
#21781 = CARTESIAN_POINT ( 'NONE',  ( 0.07479286986302942364, 7.629137130509078268, -2.455503679634089220 ) ) ;
#21783 = CARTESIAN_POINT ( 'NONE',  ( 6.222029796014385106, -1.727739227931901489, -1.038831587593692873 ) ) ;
#21784 = CARTESIAN_POINT ( 'NONE',  ( 5.981633625760849782, -0.6386546108097415075, 1.806296054365429393 ) ) ;
#21785 = CARTESIAN_POINT ( 'NONE',  ( -1.500000000000039302, 7.564371094685074404, -10.87018506808106899 ) ) ;
#21786 = CARTESIAN_POINT ( 'NONE',  ( 3.966501855323391723, -2.045284974426237579, -0.7877190255709336508 ) ) ;
#21787 = CARTESIAN_POINT ( 'NONE',  ( 1.499999999999987121, 1.535416667349486453, 0.8660254037844524744 ) ) ;
#21788 = CARTESIAN_POINT ( 'NONE',  ( 1.968876373762207477, -1.476028252698018406, 1.215921256797661609 ) ) ;
#21789 = CARTESIAN_POINT ( 'NONE',  ( -6.043183783389232566, 8.073467052085995022, 1.599625672291269396 ) ) ;
#21790 = CARTESIAN_POINT ( 'NONE',  ( 5.653386866774156694, 5.697965554099049257, -0.7216878364870207285 ) ) ;
#21792 = CARTESIAN_POINT ( 'NONE',  ( 0.8609541034889023337, -0.05231784723681161264, -2.015913592316537883 ) ) ;
#21791 = CARTESIAN_POINT ( 'NONE',  ( 10.16279779336423772, 3.829867255648782720, -5.736760595005132579 ) ) ;
#21794 = EDGE_CURVE ( 'NONE', #11785, #88459, #15627, .T. ) ;
#21793 = CARTESIAN_POINT ( 'NONE',  ( 1.364683531249996529, 10.52604166700806765, 0.7879004041258405033 ) ) ;
#21796 = CARTESIAN_POINT ( 'NONE',  ( -4.118644803501354978, 8.027112380718707030, 0.7998128361456352531 ) ) ;
#21795 = CARTESIAN_POINT ( 'NONE',  ( 5.706613541269077494, 1.932210019790636224, 1.034112652976440394 ) ) ;
#21798 = EDGE_LOOP ( 'NONE', ( #200999, #34723, #34247, #207814 ) ) ;
#21797 = CARTESIAN_POINT ( 'NONE',  ( 3.557352906045672114, 0.4196458916515317661, -1.672789571874600645 ) ) ;
#21799 = CARTESIAN_POINT ( 'NONE',  ( 0.1394461523057136665, 2.058909413595513715, -2.136561586061051621 ) ) ;
#21800 = CARTESIAN_POINT ( 'NONE',  ( 7.470706336329915764, 8.674577799595093452, -1.199719254218441611 ) ) ;
#21801 = CARTESIAN_POINT ( 'NONE',  ( 5.834086172582112262, 5.700855377634248100, 1.040834085586084257E-14 ) ) ;
#21802 = FILL_AREA_STYLE ('',( #171286 ) ) ;
#21803 = CARTESIAN_POINT ( 'NONE',  ( 1.240593047436115759, -1.913272810121857237, -0.4332019784048374289 ) ) ;
#21804 = CARTESIAN_POINT ( 'NONE',  ( 4.318600669050608687, 4.999583595936801572, -2.499999999999996891 ) ) ;
#21805 = CARTESIAN_POINT ( 'NONE',  ( 5.352771719296971042, 5.139321848801576387, 0.7998128361456341429 ) ) ;
#21806 = DIRECTION ( 'NONE',  ( -1.000000000000000000, -3.451266460341926649E-31, -8.638326563840809144E-31 ) ) ;
#21807 = ORIENTED_EDGE ( 'NONE', *, *, #70875, .F. ) ;
#21809 = CIRCLE ( 'NONE', #63285, 11.09999999999999964 ) ;
#21808 = CARTESIAN_POINT ( 'NONE',  ( -2.331034670843834533E-15, -7.256398209935973398, 9.569423160902228886 ) ) ;
#21810 = ORIENTED_EDGE ( 'NONE', *, *, #166214, .F. ) ;
#21811 = CARTESIAN_POINT ( 'NONE',  ( 4.477109312160544974, -1.620259271022955305, -0.8101795318041657978 ) ) ;
#21812 = ORIENTED_EDGE ( 'NONE', *, *, #78667, .T. ) ;
#21813 = CARTESIAN_POINT ( 'NONE',  ( 8.757677159423465696, 12.30470822171437284, 1.199719254218450271 ) ) ;
#21814 = AXIS2_PLACEMENT_3D ( 'NONE', #11955, #92185, #8762 ) ;
#21815 = CARTESIAN_POINT ( 'NONE',  ( 4.760848217054122422, 5.583353003765119560, -1.199719254218452047 ) ) ;
#21816 = CARTESIAN_POINT ( 'NONE',  ( 4.494648839764849413, -1.758179434694202570, -0.4356380854809716041 ) ) ;
#21817 = CARTESIAN_POINT ( 'NONE',  ( 0.3689019803512919582, -6.583711573986999355, 9.609441814500817358 ) ) ;
#21818 = CARTESIAN_POINT ( 'NONE',  ( 5.782412516234797017, 6.044064802175099338, 0.5499171889626064402 ) ) ;
#21820 = CARTESIAN_POINT ( 'NONE',  ( -1.402160292154681736E-14, 14.42187500034139980, 1.575800808251682339 ) ) ;
#21819 = CARTESIAN_POINT ( 'NONE',  ( 5.670303652858919463, -0.8369403475225531963, -1.662290214344812833 ) ) ;
#21821 = CARTESIAN_POINT ( 'NONE',  ( 2.284663151613754550, 1.537047112958013440, -1.143011353438025957 ) ) ;
#21822 = CARTESIAN_POINT ( 'NONE',  ( -11.14389002924298566, 7.220603907090449525, 3.549113525960188031 ) ) ;
#21823 = CARTESIAN_POINT ( 'NONE',  ( -10.99960280095053378, -9.919999999999998153, 0.09350563796403016381 ) ) ;
#21824 = CARTESIAN_POINT ( 'NONE',  ( -5.896220218617790110, 6.102442225045867197, -0.7164689422466080648 ) ) ;
#21825 = CARTESIAN_POINT ( 'NONE',  ( 6.290620087060792009, 10.28288116830553101, -0.7216878364870267237 ) ) ;
#21826 = B_SPLINE_CURVE_WITH_KNOTS ( 'NONE', 3,
 ( #41392, #25104, #54423, #7778, #20821, #137819, #74937, #119482 ),
 .UNSPECIFIED., .F., .F.,
 ( 4, 2, 2, 4 ),
 ( 6.987453456569233415E-16, 0.0002305131806122158098, 0.0004610263612237329054, 0.0009220527224467680184 ),
 .UNSPECIFIED. ) ;
#21827 = CARTESIAN_POINT ( 'NONE',  ( -5.088387723830502196, 4.830873854090670605, -0.7998128361456221525 ) ) ;
#21828 = SURFACE_STYLE_FILL_AREA ( #121586 ) ;
#21829 = CARTESIAN_POINT ( 'NONE',  ( 1.517645033149318978, -1.162591604200275963, -1.737351732476496657 ) ) ;
#21830 = CARTESIAN_POINT ( 'NONE',  ( 6.866278450678116485, 6.975356045404744521, 0.000000000000000000 ) ) ;
#21831 = CARTESIAN_POINT ( 'NONE',  ( 6.563506682682211490, 0.3285509523427312950, -1.898022546839329472 ) ) ;
#21832 = CARTESIAN_POINT ( 'NONE',  ( -6.064574784014443942, 5.969758757638621738, -0.7998128361456291469 ) ) ;
#21833 = CARTESIAN_POINT ( 'NONE',  ( 2.660947563312371589, -1.587261545009664765, -0.9017329732442301848 ) ) ;
#21834 = CARTESIAN_POINT ( 'NONE',  ( -3.600749563572741785, 3.160087278256925813, 2.499999999999998668 ) ) ;
#21835 = CARTESIAN_POINT ( 'NONE',  ( 1.880979024232478425, -1.749874716401520036, -0.7718601483891265325 ) ) ;
#21836 = CARTESIAN_POINT ( 'NONE',  ( 1.838274926946784182, -1.056231965017372598, 1.662188548998255078 ) ) ;
#21837 = CARTESIAN_POINT ( 'NONE',  ( 4.177243316516196181, 1.270932653052879502, 1.468510540936379671 ) ) ;
#21838 = ORIENTED_EDGE ( 'NONE', *, *, #8484, .F. ) ;
#21839 = CARTESIAN_POINT ( 'NONE',  ( -3.941149012854040290, 4.002721280689181427, -0.7037892630772435432 ) ) ;
#21840 = CARTESIAN_POINT ( 'NONE',  ( -4.305596300791617814, 7.180890229968955651, 1.199719254218452935 ) ) ;
#21842 = CARTESIAN_POINT ( 'NONE',  ( 3.744478000529617656, 1.131475959888720295, -1.793321066073015224 ) ) ;
#21841 = CARTESIAN_POINT ( 'NONE',  ( 7.828907357248368726, 8.098423103070084395, 0.7998128361456281477 ) ) ;
#21843 = CARTESIAN_POINT ( 'NONE',  ( -10.59765138761703085, 13.79999999999998295, 3.303242380465396977 ) ) ;
#21844 = CARTESIAN_POINT ( 'NONE',  ( 7.899597058256738968, 12.36794700127490820, 1.040834085586084257E-14 ) ) ;
#21845 = CARTESIAN_POINT ( 'NONE',  ( -4.911796789900812144, 8.952456364851418158, 0.7998128361456291469 ) ) ;
#21846 = CARTESIAN_POINT ( 'NONE',  ( 1.500000000000001332, 11.65625000068279427, 0.000000000000000000 ) ) ;
#21847 = ORIENTED_EDGE ( 'NONE', *, *, #168724, .T. ) ;
#21848 = AXIS2_PLACEMENT_3D ( 'NONE', #51394, #202940, #88153 ) ;
#21849 = CARTESIAN_POINT ( 'NONE',  ( 5.851225812749518695, 8.984124660586543243, -1.199719254218452047 ) ) ;
#21850 = CARTESIAN_POINT ( 'NONE',  ( -15.75000000000000000, 9.799999999999998934, -3.200000000000001510 ) ) ;
#21851 = CARTESIAN_POINT ( 'NONE',  ( 3.615676881913011176, -1.798418494116042821, 0.3134422064149794407 ) ) ;
#21852 = LINE ( 'NONE', #50132, #184023 ) ;
#21853 = CARTESIAN_POINT ( 'NONE',  ( -10.14113571334194930, 10.93367254176152059, -0.7216878364870267237 ) ) ;
#21854 = CARTESIAN_POINT ( 'NONE',  ( -4.585403371929053229, 8.498043419817562949, 0.04945426522169442396 ) ) ;
#21855 = DIRECTION ( 'NONE',  ( 0.9992060137953822085, -3.484297484817962848E-16, -0.03984146075563036599 ) ) ;
#21856 = CARTESIAN_POINT ( 'NONE',  ( 4.223419137798128276, -1.790188510885984297, 0.5427707113358354318 ) ) ;
#21857 = CARTESIAN_POINT ( 'NONE',  ( 7.914208982075123799, 10.25632978388623684, -1.599625672291262513 ) ) ;
#21858 = CARTESIAN_POINT ( 'NONE',  ( 1.699704897782030377, -0.6493637136964022227, 1.813892859743936103 ) ) ;
#21859 = CARTESIAN_POINT ( 'NONE',  ( 6.825062041929172985, -1.792332737533608666, -0.7979697884207545000 ) ) ;
#21860 = CARTESIAN_POINT ( 'NONE',  ( -0.6823417656250003738, 9.213541667008065872, 1.181850606188754593 ) ) ;
#21861 = CARTESIAN_POINT ( 'NONE',  ( -7.576308911938196999, 7.733448573549685179, 0.7998128361456462443 ) ) ;
#21862 = CARTESIAN_POINT ( 'NONE',  ( 2.998324526916512411, 6.649795714711241423, 0.000000000000000000 ) ) ;
#21863 = ADVANCED_FACE ( 'NONE', ( #157902 ), #207135, .F. ) ;
#21864 = CARTESIAN_POINT ( 'NONE',  ( -5.763624699140894592, 5.896852701852039580, -0.7216878364870338292 ) ) ;
#21865 = STYLED_ITEM ( 'NONE', ( #160832 ), #81437 ) ;
#21866 = CIRCLE ( 'NONE', #129152, 1.500000000000000222 ) ;
#21867 = CARTESIAN_POINT ( 'NONE',  ( 0.8786900280967164800, -0.5185874880111912555, -2.052613615991748297 ) ) ;
#21868 = CARTESIAN_POINT ( 'NONE',  ( 8.543609354905870035, 13.11929468069890525, 0.7998128361456462443 ) ) ;
#21869 = CARTESIAN_POINT ( 'NONE',  ( -4.297571505851936813, 4.116180966356429494, 1.214306433183764966E-14 ) ) ;
#21870 = CARTESIAN_POINT ( 'NONE',  ( 5.401260523219934662, -1.778462342247935979, 1.059464396209061521 ) ) ;
#21872 = CARTESIAN_POINT ( 'NONE',  ( -0.6823417656250212460, 2.363541667008084435, 1.181850606188767472 ) ) ;
#21871 = CARTESIAN_POINT ( 'NONE',  ( 0.5910386730991653570, -0.6632029860377097741, 1.717849102829023922 ) ) ;
#21873 = CARTESIAN_POINT ( 'NONE',  ( 5.397245865906225681, -1.031513598091776673, -2.054350403923683732 ) ) ;
#21874 = CARTESIAN_POINT ( 'NONE',  ( 6.480434237652132445, 7.623223367758051872, 1.082531754730558626 ) ) ;
#21876 = PRESENTATION_STYLE_ASSIGNMENT (( #184399 ) ) ;
#21875 = CARTESIAN_POINT ( 'NONE',  ( 2.957086901556340575, 6.464035461875470290, 0.7216878364870257245 ) ) ;
#21877 = CARTESIAN_POINT ( 'NONE',  ( 1.957357739143847919, 0.3891275796813770116, -2.258848713223185367 ) ) ;
#21878 = CARTESIAN_POINT ( 'NONE',  ( 7.235142258280562899, -6.594478602024301139, -7.235142258280586880 ) ) ;
#21879 = CARTESIAN_POINT ( 'NONE',  ( -6.231907884136888676, 7.299589282028351001, -1.199719254218453823 ) ) ;
#21880 = CARTESIAN_POINT ( 'NONE',  ( 5.788998755281030029, 1.472039788614720290, 1.266697539889444446 ) ) ;
#21881 = ORIENTED_EDGE ( 'NONE', *, *, #13809, .F. ) ;
#21882 = CARTESIAN_POINT ( 'NONE',  ( 8.731087737076324018, 9.288616569451617622, 1.040834085586084257E-14 ) ) ;
#21883 = VERTEX_POINT ( 'NONE', #205547 ) ;
#21884 = CARTESIAN_POINT ( 'NONE',  ( 5.941656858135131891, -1.798430535887390658, 0.6506349336675710804 ) ) ;
#21885 = CARTESIAN_POINT ( 'NONE',  ( 5.647672796105281279, 1.985869605424210649, -0.3494789899042491932 ) ) ;
#21887 = CARTESIAN_POINT ( 'NONE',  ( -2.609770642201835855, -0.3830433331901521576, -0.1872689674646474400 ) ) ;
#21886 = CARTESIAN_POINT ( 'NONE',  ( -6.842061076390810292, 11.13415502243129218, 0.000000000000000000 ) ) ;
#21888 = CARTESIAN_POINT ( 'NONE',  ( 1.642778471875001811, -1.830208332855375097, 2.845375778867859751 ) ) ;
#21890 = CARTESIAN_POINT ( 'NONE',  ( 1.533702468213002712, 0.8761213712049474855, -1.537698828099523629 ) ) ;
#21889 = CARTESIAN_POINT ( 'NONE',  ( 2.800817752552913209, 1.766549217158249085, 1.117748608743725169 ) ) ;
#21891 = FACE_OUTER_BOUND ( 'NONE', #204676, .T. ) ;
#21892 = CARTESIAN_POINT ( 'NONE',  ( 3.715000766203532034, -0.1696613574440029304, 2.286031353463747529 ) ) ;
#21893 = CARTESIAN_POINT ( 'NONE',  ( 2.923474784230184920, 0.9664119506291848349, -1.447106689822146963 ) ) ;
#21894 = EDGE_CURVE ( 'NONE', #33092, #113056, #185941, .T. ) ;
#21895 = CARTESIAN_POINT ( 'NONE',  ( 10.16199982864259788, 11.81442020729326536, 1.199719254218452047 ) ) ;
#21896 = DIRECTION ( 'NONE',  ( 0.1510067114093955887, -0.000000000000000000, 0.9885327375000383388 ) ) ;
#21897 = CARTESIAN_POINT ( 'NONE',  ( 2.266548906626513649, -1.733607756391885912, 0.03760194650299571173 ) ) ;
#21898 = CARTESIAN_POINT ( 'NONE',  ( 3.965408508876398841, 1.860285638359628235, 1.119340054616506874 ) ) ;
#21899 = CARTESIAN_POINT ( 'NONE',  ( 3.161022370280501814, 6.839609865302569425, 0.000000000000000000 ) ) ;
#21900 = CARTESIAN_POINT ( 'NONE',  ( 4.856657812281613751, -1.900414607462055816, -0.6748505307947461063 ) ) ;
#21901 = CARTESIAN_POINT ( 'NONE',  ( 2.156250000000001776, -1.895863743164040160, 0.7852924748301010061 ) ) ;
#21902 = CARTESIAN_POINT ( 'NONE',  ( -1.201851678989727383E-14, 2.993750000682821266, 1.732050807568877637 ) ) ;
#21903 = CARTESIAN_POINT ( 'NONE',  ( 0.7801460289126905812, -1.072782840069667509, 1.599849161009530674 ) ) ;
#21904 = CARTESIAN_POINT ( 'NONE',  ( 1.364683531250000303, 15.25520833367473017, -0.7879004041258355073 ) ) ;
#21905 = CARTESIAN_POINT ( 'NONE',  ( 4.641020947978182321, 2.126209183204033959, 0.6434571820467527292 ) ) ;
#21906 = ORIENTED_EDGE ( 'NONE', *, *, #15354, .F. ) ;
#21907 = CARTESIAN_POINT ( 'NONE',  ( -0.1108833634137010027, 1.377173795795206157, -2.152720132533674668 ) ) ;
#21908 = CARTESIAN_POINT ( 'NONE',  ( -1.402160292154681736E-14, -0.03749999999998095135, 1.732050807568877637 ) ) ;
#21909 = CARTESIAN_POINT ( 'NONE',  ( 8.450809820019639318, 8.753699632978056755, -0.7998128361456291469 ) ) ;
#21910 = CARTESIAN_POINT ( 'NONE',  ( 6.616015773344440021, 6.821032611764393572, 1.040834085586084257E-14 ) ) ;
#21911 = CARTESIAN_POINT ( 'NONE',  ( -1.642778471874998480, -1.801041666188708090, 2.845375778867863303 ) ) ;
#21912 = CARTESIAN_POINT ( 'NONE',  ( 0.8037664367953377687, 1.956346004370253633, -1.052120880887427390 ) ) ;
#21913 = CARTESIAN_POINT ( 'NONE',  ( 5.846142468697441252, -0.8834969228576605715, 1.751761657833034613 ) ) ;
#21914 = CARTESIAN_POINT ( 'NONE',  ( 10.41229878561526512, 11.25002945941372623, -0.7216878364870257245 ) ) ;
#21915 = CARTESIAN_POINT ( 'NONE',  ( -1.363015705810363576, 4.003158907273498990, -0.6271916676896991394 ) ) ;
#21916 = CARTESIAN_POINT ( 'NONE',  ( 0.5972264258897291844, 1.797487153981947916, -1.200333582630601637 ) ) ;
#21917 = CARTESIAN_POINT ( 'NONE',  ( -6.156811154381562012, 6.355570232966157640, 0.7216878364870257245 ) ) ;
#21918 = CARTESIAN_POINT ( 'NONE',  ( 3.613784930257180950, 0.5038104997578238820, -2.000076687661219044 ) ) ;
#21919 = CARTESIAN_POINT ( 'NONE',  ( -5.416646063859567484, 6.278174148379618735, 1.199719254218450271 ) ) ;
#21920 =( BOUNDED_CURVE ( )  B_SPLINE_CURVE ( 2, ( #67281, #19619, #151779, #200490, #132359, #101949, #4410 ),
 .UNSPECIFIED., .F., .T. ) 
 B_SPLINE_CURVE_WITH_KNOTS ( ( 3, 2, 2, 3 ),
 ( 0.4499999999999999556, 0.4583333333333331483, 0.4666666666666663965, 0.4749999999999995892 ),
 .UNSPECIFIED. ) 
 CURVE ( )  GEOMETRIC_REPRESENTATION_ITEM ( )  RATIONAL_B_SPLINE_CURVE ( ( 1.000000000000000888, 0.8660254037844378194, 1.000000000000000000, 0.8660254037844387076, 1.000000000000000000, 0.8660254037844449249, 0.9999999999999937828 ) ) 
 REPRESENTATION_ITEM ( '' )  );
#21921 = CARTESIAN_POINT ( 'NONE',  ( -1.500000000000013101, 4.160416667349482900, -0.8660254037844313801 ) ) ;
#21922 = CARTESIAN_POINT ( 'NONE',  ( 1.364683531249984538, -1.094791666325247936, -0.7879004041258309554 ) ) ;
#21923 = CARTESIAN_POINT ( 'NONE',  ( 4.481629103029507455, 1.220264704679861811, 1.417821649906551906 ) ) ;
#21924 = CARTESIAN_POINT ( 'NONE',  ( 3.973097536218972436, -1.716008982208137468, -0.2490561736530460535 ) ) ;
#21925 = CARTESIAN_POINT ( 'NONE',  ( 3.456370904947672074, -1.536751586138744852, -0.8169772437159742440 ) ) ;
#21926 = CARTESIAN_POINT ( 'NONE',  ( 0.5566822826340491748, -1.655162342056889502, 1.586242259447123493 ) ) ;
#21927 = CARTESIAN_POINT ( 'NONE',  ( -1.364683531250012516, 4.301041667008089320, -0.7879004041258300672 ) ) ;
#21928 = CARTESIAN_POINT ( 'NONE',  ( 4.651946873442760477, 0.8016356570225026124, 1.931162265472508910 ) ) ;
#21929 = CARTESIAN_POINT ( 'NONE',  ( 0.05820987927622478519, -1.643049995186950829, -0.8308948761173093889 ) ) ;
#21930 = EDGE_CURVE ( 'NONE', #196589, #192824, #157450, .T. ) ;
#21931 = FACE_OUTER_BOUND ( 'NONE', #84845, .T. ) ;
#21932 = CARTESIAN_POINT ( 'NONE',  ( 0.3170300144729014669, 1.034162889623980286, -1.730867746391979933 ) ) ;
#21933 = CARTESIAN_POINT ( 'NONE',  ( 0.8617730121942971389, -1.675286201960282995, -1.300076073212981242 ) ) ;
#21934 = CARTESIAN_POINT ( 'NONE',  ( 6.925078400183550364, -0.007619068086212391067, 2.144148427808051594 ) ) ;
#21935 = CARTESIAN_POINT ( 'NONE',  ( 7.739551183390158684, 13.97472016681189189, -10.04165774006234102 ) ) ;
#21936 = CARTESIAN_POINT ( 'NONE',  ( -7.853197290813634268, 10.18514947741448573, 1.599625672291295375 ) ) ;
#21937 = CARTESIAN_POINT ( 'NONE',  ( 5.795220594837462436, 8.848508896363995291, -1.199719254218440723 ) ) ;
#21938 = CARTESIAN_POINT ( 'NONE',  ( 2.367978261241600713, 0.5630001329197281690, -2.044326955284565539 ) ) ;
#21939 =( NAMED_UNIT ( * ) PLANE_ANGLE_UNIT ( ) SI_UNIT ( $, .RADIAN. ) );
#21940 = CARTESIAN_POINT ( 'NONE',  ( 4.582524934692378871, -1.771534430979417429, -0.4408631061849078714 ) ) ;
#21941 = EDGE_LOOP ( 'NONE', ( #147627, #127454, #39084, #9598 ) ) ;
#21942 = CARTESIAN_POINT ( 'NONE',  ( -5.433785704026946384, 9.561443431331920095, 0.000000000000000000 ) ) ;
#21943 = FILL_AREA_STYLE_COLOUR ( '', #164606 ) ;
#21944 = CARTESIAN_POINT ( 'NONE',  ( -1.737500000000000266, -3.864583332377418579, -3.009438278150923907 ) ) ;
#21945 = CARTESIAN_POINT ( 'NONE',  ( -7.705111371268023923, 7.883718109434487253, 1.040834085586084257E-14 ) ) ;
#21946 = CARTESIAN_POINT ( 'NONE',  ( 2.338154391725711267, -1.166417678377267064, -1.648725491961404055 ) ) ;
#21947 = CARTESIAN_POINT ( 'NONE',  ( 5.315527377757141458, -0.3284926246858720922, 2.182075488366498117 ) ) ;
#21948 = CARTESIAN_POINT ( 'NONE',  ( -5.659602779061863487, 5.567567761852417085, 0.7998128361456281477 ) ) ;
#21949 = CARTESIAN_POINT ( 'NONE',  ( 3.854231730816888302, -1.858662791824859051, -0.09517680055876918954 ) ) ;
#21950 = CARTESIAN_POINT ( 'NONE',  ( 7.553864141108259211, 11.96459193126834464, 1.040834085586084257E-14 ) ) ;
#21951 = CARTESIAN_POINT ( 'NONE',  ( 1.500000000000053291, 7.750000000000000000, 15.74999999999999289 ) ) ;
#21952 = ORIENTED_EDGE ( 'NONE', *, *, #101780, .F. ) ;
#21953 = ORIENTED_EDGE ( 'NONE', *, *, #59990, .F. ) ;
#21954 = CARTESIAN_POINT ( 'NONE',  ( -5.576481253922474401, 5.400316305864651056, -0.7998128361456221525 ) ) ;
#21955 =( GEOMETRIC_REPRESENTATION_CONTEXT ( 3 ) GLOBAL_UNCERTAINTY_ASSIGNED_CONTEXT ( ( #128101 ) ) GLOBAL_UNIT_ASSIGNED_CONTEXT ( ( #8072, #126185, #62179 ) ) REPRESENTATION_CONTEXT ( 'NONE', 'WORKASPACE' ) );
#21956 = CARTESIAN_POINT ( 'NONE',  ( -8.239604668803112375, 10.63595808506888396, -1.599625672291263179 ) ) ;
#21957 = CARTESIAN_POINT ( 'NONE',  ( 4.670415550810885996, -1.190324863180821646, 1.384379922071424351 ) ) ;
#21958 = CIRCLE ( 'NONE', #101621, 12.00000000000000178 ) ;
#21960 = CARTESIAN_POINT ( 'NONE',  ( -4.061770719603903679, 7.733366158448967909, -0.6361108440643822304 ) ) ;
#21959 = CARTESIAN_POINT ( 'NONE',  ( -5.029148636026397945, 4.832037928311032182, 0.7998128361456281477 ) ) ;
#21961 = CARTESIAN_POINT ( 'NONE',  ( -0.6823417656250246877, -0.6989583329919113464, 1.181850606188755259 ) ) ;
#21962 = CARTESIAN_POINT ( 'NONE',  ( 0.9832555119714074809, 1.599142458273569600, 0.6705785602827417646 ) ) ;
#21963 = CARTESIAN_POINT ( 'NONE',  ( 0.4271921415617612183, 0.8987490902026186168, -1.490136572063437637 ) ) ;
#21964 = CARTESIAN_POINT ( 'NONE',  ( 5.953837893508783452, 0.6757001976828447276, -2.206575258351393565 ) ) ;
#21965 = CARTESIAN_POINT ( 'NONE',  ( 4.529305835417093640, 7.441884687032027657, -1.199719254218450271 ) ) ;
#21966 = CARTESIAN_POINT ( 'NONE',  ( 1.001328657153805146, 1.683097017759589420, 1.188813969666648873 ) ) ;
#21967 = CARTESIAN_POINT ( 'NONE',  ( 5.144429221381498607, 8.089252293998699272, -1.199719254218452047 ) ) ;
#21968 = CARTESIAN_POINT ( 'NONE',  ( 6.415373042369045820, 0.7112672321729663905, 2.185653275185605704 ) ) ;
#21969 = CARTESIAN_POINT ( 'NONE',  ( -0.5942495929466964366, -3.232243495192077098, 3.244776806288057980 ) ) ;
#21970 = CARTESIAN_POINT ( 'NONE',  ( -7.273023059088104425, 7.449891421883056530, 0.000000000000000000 ) ) ;
#21971 = CARTESIAN_POINT ( 'NONE',  ( 6.104356062600288624, -0.6750377415852754082, -1.744797942764392928 ) ) ;
#21974 = EDGE_CURVE ( 'NONE', #177833, #46648, #142735, .T. ) ;
#21973 = CARTESIAN_POINT ( 'NONE',  ( -4.821859908315634158, 5.654533310236863564, 1.199719254218452935 ) ) ;
#21972 = CARTESIAN_POINT ( 'NONE',  ( 3.427896188528327226, -1.883279545317056547, 0.3315703044584616399 ) ) ;
#21975 = CARTESIAN_POINT ( 'NONE',  ( 5.092482806099829062, -2.189899077852827780, -0.2726905915074183673 ) ) ;
#21976 = CARTESIAN_POINT ( 'NONE',  ( 0.6124999999999932720, 1.979166667349464781, -1.060881119635938008 ) ) ;
#21977 = CARTESIAN_POINT ( 'NONE',  ( 5.614485009834906393, 6.683225611963085733, -1.082531754730548412 ) ) ;
#21978 = CARTESIAN_POINT ( 'NONE',  ( 4.462041952228939401, 6.299077925724123617, -1.443375672974068769 ) ) ;
#21979 = CARTESIAN_POINT ( 'NONE',  ( -4.462041952228944730, 7.259447140025469203, -1.082531754730549967 ) ) ;
#21980 = CARTESIAN_POINT ( 'NONE',  ( 6.041668349913133618, -1.996727924239691587, 0.7141442534656232688 ) ) ;
#21981 = EDGE_CURVE ( 'NONE', #174627, #103981, #82774, .T. ) ;
#21982 = CARTESIAN_POINT ( 'NONE',  ( 3.136059509142240742, -1.548504943098116593, -1.711042559064612334 ) ) ;
#21983 = CARTESIAN_POINT ( 'NONE',  ( 4.088298575758734898, 1.051444423028622399, -1.656135347060924135 ) ) ;
#21984 = DIRECTION ( 'NONE',  ( 0.3502638921866464417, -1.953969548649013438E-16, 0.9366510587354618389 ) ) ;
#21985 = CARTESIAN_POINT ( 'NONE',  ( 1.147228161472005681, 1.732707765124143817, -0.9198407203683529598 ) ) ;
#21986 = DIRECTION ( 'NONE',  ( 1.224643483124940471E-16, 0.002327115863039739760, 0.9999972922622140103 ) ) ;
#21987 = CARTESIAN_POINT ( 'NONE',  ( 4.161361007603033180, 7.399433999391101580, -0.7812420967184935394 ) ) ;
#21988 = ORIENTED_EDGE ( 'NONE', *, *, #119470, .F. ) ;
#21989 = CARTESIAN_POINT ( 'NONE',  ( 6.175017591530616023, 1.752142144017948100, -0.9981200475188132248 ) ) ;
#21990 = CARTESIAN_POINT ( 'NONE',  ( -8.286004436246233951, 12.81875560892930466, 1.040834085586084257E-14 ) ) ;
#21991 = DIRECTION ( 'NONE',  ( 0.1828377250218585215, -0.9633937422820121332, -0.1960685177194217976 ) ) ;
#21992 =( NAMED_UNIT ( * ) SI_UNIT ( $, .STERADIAN. ) SOLID_ANGLE_UNIT ( ) );
#21993 = CARTESIAN_POINT ( 'NONE',  ( 2.606498238493897279, 2.170487999849361138, 0.05724136673956359972 ) ) ;
#21994 = CARTESIAN_POINT ( 'NONE',  ( 3.881377115262160782, 7.750300077773022878, 0.7998128361456271485 ) ) ;
#21995 = CARTESIAN_POINT ( 'NONE',  ( 0.3695850531008069706, -1.794773754367712693, -1.129184308951653781 ) ) ;
#21996 = CARTESIAN_POINT ( 'NONE',  ( -1.500000000000001332, 1.181250000682816603, 0.000000000000000000 ) ) ;
#21997 = CARTESIAN_POINT ( 'NONE',  ( 8.432281472695482449, 11.92507992053172572, 1.199719254218450271 ) ) ;
#21998 = FACE_OUTER_BOUND ( 'NONE', #37368, .T. ) ;
#21999 = CARTESIAN_POINT ( 'NONE',  ( 5.901825473515108555, 7.257632781371366804, 1.250113620240392631 ) ) ;
#22000 = CARTESIAN_POINT ( 'NONE',  ( 0.4388362695032248517, 0.3497011122354178325, 2.030714657000245893 ) ) ;
#22002 = CARTESIAN_POINT ( 'NONE',  ( 0.4019237886466816012, 8.457585450998168497, -1.499999999999998668 ) ) ;
#22001 = CARTESIAN_POINT ( 'NONE',  ( -1.734723475976807094E-15, 2.999999999999988898, -6.938893903907228378E-15 ) ) ;
#22003 = CARTESIAN_POINT ( 'NONE',  ( -1.201851678989727383E-14, 2.321875000341416584, 1.575800808251672791 ) ) ;
#22004 = CARTESIAN_POINT ( 'NONE',  ( -5.000000000000013323, 11.39843543023555661, 0.7750000000000004663 ) ) ;
#22005 = ORIENTED_EDGE ( 'NONE', *, *, #207859, .F. ) ;
#22006 = CARTESIAN_POINT ( 'NONE',  ( 3.193911838225035105, 1.215006091714765368, 1.476655219734591906 ) ) ;
#22007 =( BOUNDED_SURFACE ( )  B_SPLINE_SURFACE ( 3, 3, ( 
 ( #12182, #123902, #43651, #176830, #42588, #140087, #58808, #108693, #59872, #174721 ),
 ( #26294, #175775, #29518, #206112, #28444, #189871, #107626, #94535, #91334, #144378 ),
 ( #92409, #10049, #210377, #158448, #8986, #76124, #93469, #159508, #95611, #73994 ),
 ( #11107, #62019, #77182, #143304, #111902, #157392, #128173, #15370, #115091, #81463 ),
 ( #129243, #149663, #195216, #112966, #212510, #97735, #213562, #180035, #65184, #198384 ),
 ( #50026, #33767, #147541, #67303, #17494, #64151, #148599, #178978, #181088, #130293 ),
 ( #199450, #168, #145444, #47929, #48974, #31657, #14300, #30592, #116149, #196282 ) ),
 .UNSPECIFIED., .T., .F., .T. ) 
 B_SPLINE_SURFACE_WITH_KNOTS ( ( 4, 3, 4 ),
 ( 4, 1, 1, 1, 1, 1, 1, 4 ),
 ( 0.000000000000000000, 0.5000000000000000000, 1.000000000000000000 ),
 ( 0.000000000000000000, 0.09090790722575105287, 0.1825853934691276381, 0.2551728700554835028, 0.3603391217242263855, 0.5205903519787860034, 0.7335386666926504429, 0.9999999999999998890 ),
 .UNSPECIFIED. ) 
 GEOMETRIC_REPRESENTATION_ITEM ( )  RATIONAL_B_SPLINE_SURFACE ( (
 ( 1.000000000000000222, 1.000000000000000222, 1.000000000000000222, 1.000000000000000222, 1.000000000000000222, 1.000000000000000444, 1.000000000000000222, 1.000000000000000222, 1.000000000000000222, 1.000000000000000222),
 ( 0.3333333333333334259, 0.3333333333333334259, 0.3333333333333334259, 0.3333333333333333148, 0.3333333333333334259, 0.3333333333333335369, 0.3333333333333334259, 0.3333333333333334814, 0.3333333333333334259, 0.3333333333333334259),
 ( 0.3333333333333334259, 0.3333333333333334259, 0.3333333333333334259, 0.3333333333333333148, 0.3333333333333334259, 0.3333333333333335369, 0.3333333333333334259, 0.3333333333333334814, 0.3333333333333334259, 0.3333333333333334259),
 ( 1.000000000000000222, 1.000000000000000222, 1.000000000000000222, 1.000000000000000222, 1.000000000000000222, 1.000000000000000444, 1.000000000000000222, 1.000000000000000222, 1.000000000000000222, 1.000000000000000222),
 ( 0.3333333333333334259, 0.3333333333333334259, 0.3333333333333334259, 0.3333333333333333148, 0.3333333333333334259, 0.3333333333333335369, 0.3333333333333334259, 0.3333333333333334814, 0.3333333333333334259, 0.3333333333333334259),
 ( 0.3333333333333334259, 0.3333333333333334259, 0.3333333333333334259, 0.3333333333333333148, 0.3333333333333334259, 0.3333333333333335369, 0.3333333333333334259, 0.3333333333333334814, 0.3333333333333334259, 0.3333333333333334259),
 ( 1.000000000000000222, 1.000000000000000222, 1.000000000000000222, 1.000000000000000222, 1.000000000000000222, 1.000000000000000444, 1.000000000000000222, 1.000000000000000222, 1.000000000000000222, 1.000000000000000222) ) ) 
 REPRESENTATION_ITEM ( '' )  SURFACE ( )  );
#22008 = CARTESIAN_POINT ( 'NONE',  ( 5.559369761212399119, 0.3421458929979518948, -1.736264261622854743 ) ) ;
#22009 = CARTESIAN_POINT ( 'NONE',  ( 6.363572996767764778, 8.517530811019446091, -1.599625672291283607 ) ) ;
#22010 = CARTESIAN_POINT ( 'NONE',  ( -4.066556009095094737, 6.831733546331167695, 1.199719254218464037 ) ) ;
#22011 = CARTESIAN_POINT ( 'NONE',  ( 0.5975729546051986585, 1.217269667385068477, 1.341803709015822132 ) ) ;
#22013 = CARTESIAN_POINT ( 'NONE',  ( 0.7959256443332961561, -0.8641892358523853845, -1.709830222631677943 ) ) ;
#22012 = CARTESIAN_POINT ( 'NONE',  ( -6.717748655459615748, -7.246166700180828535, 6.717748655459638840 ) ) ;
#22014 = CARTESIAN_POINT ( 'NONE',  ( 2.295452831283749440, -1.850383948470477602, 0.9288054807428181014 ) ) ;
#22015 = CARTESIAN_POINT ( 'NONE',  ( -1.364683531250014514, 0.8010416670080889867, -0.7879004041258289570 ) ) ;
#22016 = CARTESIAN_POINT ( 'NONE',  ( 6.561405567229332547, 0.3174558530528898692, -1.843364171016811603 ) ) ;
#22017 = CARTESIAN_POINT ( 'NONE',  ( 3.053144290054691901, -1.492835736363471888, -1.050712463094093385 ) ) ;
#22019 = CARTESIAN_POINT ( 'NONE',  ( 6.400493444083267036, 6.807005473012165631, 0.5116258143813920967 ) ) ;
#22018 = CARTESIAN_POINT ( 'NONE',  ( 0.1886478520232073020, -1.081937125009281964, 2.038365869624358506 ) ) ;
#22020 = CARTESIAN_POINT ( 'NONE',  ( -1.364683531250012516, 0.7802083336747528408, 0.7879004041258379498 ) ) ;
#22021 = CARTESIAN_POINT ( 'NONE',  ( 4.615719743604500103, 0.4549637584481819319, -2.011722621177906678 ) ) ;
#22023 = CARTESIAN_POINT ( 'NONE',  ( -5.388475986427523345, 8.373973519885682393, 1.199719254218452047 ) ) ;
#22022 = AXIS2_PLACEMENT_3D ( 'NONE', #99968, #67428, #3498 ) ;
#22024 = CARTESIAN_POINT ( 'NONE',  ( 7.426115451983150706, 9.686887332112256388, -1.599625672291262513 ) ) ;
#22025 = CARTESIAN_POINT ( 'NONE',  ( 4.222474775652216294, 7.013638773981186958, 1.199719254218462483 ) ) ;
#22026 = CARTESIAN_POINT ( 'NONE',  ( -1.001543065824772872E-14, 4.462500000000024336, 1.732050807568877637 ) ) ;
#22027 = CARTESIAN_POINT ( 'NONE',  ( 6.127406499145813257, 0.1562011534181114436, -2.064545280851529885 ) ) ;
#22029 = CARTESIAN_POINT ( 'NONE',  ( 0.6823417656249882723, 1.238541667008083547, -1.181850606188749264 ) ) ;
#22028 = CIRCLE ( 'NONE', #70426, 0.07999999999999993228 ) ;
#22030 = CARTESIAN_POINT ( 'NONE',  ( 3.198656860129048152, -0.6241516536032962748, -2.069545307505623821 ) ) ;
#22031 = CARTESIAN_POINT ( 'NONE',  ( 4.160810511097835729, 0.5408905907967902493, 1.945810383981197544 ) ) ;
#22032 = CARTESIAN_POINT ( 'NONE',  ( 6.720655732516636505, 1.219515403015670296, 2.385684514189966521 ) ) ;
#22035 = CARTESIAN_POINT ( 'NONE',  ( 7.795575138177731844, 8.197185204069915798, 1.040834085586084257E-14 ) ) ;
#22034 = CARTESIAN_POINT ( 'NONE',  ( 3.285556943749998737, -3.405208332855374831, -1.896917185911906500 ) ) ;
#22033 = CARTESIAN_POINT ( 'NONE',  ( 4.207966135563082410, 7.175396087857922822, -1.043745235818753780 ) ) ;
#22036 = CARTESIAN_POINT ( 'NONE',  ( -5.336015975430226099, 8.383046517047350932, -1.199719254218453823 ) ) ;
#22037 = CARTESIAN_POINT ( 'NONE',  ( 2.694546298722868549, 1.457235452327232395, -1.394086077981852911 ) ) ;
#22038 = CARTESIAN_POINT ( 'NONE',  ( -6.042130013184518589, 10.20090211535728031, -0.7998128361456291469 ) ) ;
#22040 = PRESENTATION_STYLE_ASSIGNMENT (( #57781 ) ) ;
#22039 = CARTESIAN_POINT ( 'NONE',  ( -3.415764635639130020, 6.072476943965863683, 1.199719254218462483 ) ) ;
#22041 = CARTESIAN_POINT ( 'NONE',  ( -0.08058608058608696112, -6.134628647623513231, 10.99970480893081870 ) ) ;
#22042 = CARTESIAN_POINT ( 'NONE',  ( 5.519756697582540284, -0.4584384640409415734, 1.856529252577573397 ) ) ;
#22043 = CARTESIAN_POINT ( 'NONE',  ( -11.13927487678572525, 5.784125462700367315, -4.477470366402338087 ) ) ;
#22045 = CARTESIAN_POINT ( 'NONE',  ( 4.921500000981174239, -1.427949280599305482, -1.423951169029838315 ) ) ;
#22044 = CARTESIAN_POINT ( 'NONE',  ( -8.975134502122321223, 9.573337795338607847, 1.040834085586084257E-14 ) ) ;
#22046 = CARTESIAN_POINT ( 'NONE',  ( -1.001543065824772872E-14, 5.212500000000019895, 1.732050807568877637 ) ) ;
#22047 = CARTESIAN_POINT ( 'NONE',  ( 0.6823417656249934904, 15.25520833367473372, 1.181850606188764807 ) ) ;
#22048 = CARTESIAN_POINT ( 'NONE',  ( 6.264645798839446833, -1.215808215430391304, 1.223651055087880080 ) ) ;
#22049 = CARTESIAN_POINT ( 'NONE',  ( 7.035755370848908896, 7.173079118937375931, 0.7998128361456352531 ) ) ;
#22051 = CARTESIAN_POINT ( 'NONE',  ( -1.500000000000008216, 10.53125000068279249, 3.469446951953614189E-15 ) ) ;
#22050 = CARTESIAN_POINT ( 'NONE',  ( 9.761507412159302177, 10.49077285704843199, -0.7216878364870257245 ) ) ;
#22052 = CARTESIAN_POINT ( 'NONE',  ( -11.45846087878769559, 11.09311600781452434, -3.566076377698187194 ) ) ;
#22053 = CARTESIAN_POINT ( 'NONE',  ( 5.079306140367803479, 1.745876537259077432, -0.6719496041647440299 ) ) ;
#22054 = CARTESIAN_POINT ( 'NONE',  ( 6.152595719530761009, 1.991896818749523845, 0.2912318779872117847 ) ) ;
#22055 = DIRECTION ( 'NONE',  ( 0.000000000000000000, 0.000000000000000000, -1.000000000000000000 ) ) ;
#22056 = CARTESIAN_POINT ( 'NONE',  ( 2.202089267374872872, 0.7962392033929905910, -1.911209141678638090 ) ) ;
#22057 = CARTESIAN_POINT ( 'NONE',  ( -1.483013432599996628, 7.294277089886567644, -4.259227663825902788 ) ) ;
#22058 = ORIENTED_EDGE ( 'NONE', *, *, #195648, .T. ) ;
#22059 = CARTESIAN_POINT ( 'NONE',  ( 1.036732716359071604, -1.587823911754655315, 1.242746109592095527 ) ) ;
#22060 = CARTESIAN_POINT ( 'NONE',  ( 0.8612205622890884982, -1.428740940428592898, -1.113706988620609240 ) ) ;
#22061 = CARTESIAN_POINT ( 'NONE',  ( 5.221298554594243413, 5.264138866547622975, -0.7216878364870458196 ) ) ;
#22062 = CARTESIAN_POINT ( 'NONE',  ( -0.1412570932018016034, -6.646059016331633096, -10.87798840695972657 ) ) ;
#22063 = CARTESIAN_POINT ( 'NONE',  ( 8.880227426826646564, 9.462612874160329923, 0.7216878364870458196 ) ) ;
#22064 = CARTESIAN_POINT ( 'NONE',  ( 7.263417608619159083, 9.497073181520933716, -1.599625672291262513 ) ) ;
#22066 = CARTESIAN_POINT ( 'NONE',  ( 6.573869778094940663, -0.8146055380063941254, 1.732351315116484880 ) ) ;
#22065 = CARTESIAN_POINT ( 'NONE',  ( -6.205881626753225966, 8.263281202677319470, 1.599625672291283607 ) ) ;
#22067 = CARTESIAN_POINT ( 'NONE',  ( 3.179715765502636682, 5.975770656120749535, 2.499999999999999556 ) ) ;
#22068 = LINE ( 'NONE', #23148, #97424 ) ;
#22069 = CARTESIAN_POINT ( 'NONE',  ( 0.6823417656249882723, -1.094791666325249713, 1.181850606188755259 ) ) ;
#22071 = ORIENTED_EDGE ( 'NONE', *, *, #40535, .T. ) ;
#22070 = CARTESIAN_POINT ( 'NONE',  ( 3.375617060122621194, 6.882044303544283537, 1.040834085586084257E-14 ) ) ;
#22072 = CARTESIAN_POINT ( 'NONE',  ( -4.647747731386360215, 4.316793862905830892, 0.7998128361456341429 ) ) ;
#22073 = CARTESIAN_POINT ( 'NONE',  ( -6.873620692448438874, 10.96304854125777695, 0.000000000000000000 ) ) ;
#22074 = CARTESIAN_POINT ( 'NONE',  ( 2.747127081003514881, -1.797865629537301668, 1.199965651887124896 ) ) ;
#22075 = CARTESIAN_POINT ( 'NONE',  ( -5.966997003790221576, 9.015228033513643879, -1.082531754730549967 ) ) ;
#22076 = CARTESIAN_POINT ( 'NONE',  ( 5.885648082108188461, 8.920320958217979879, 1.082531754730549967 ) ) ;
#22077 = CARTESIAN_POINT ( 'NONE',  ( 0.7211286721200690364, 1.601891702520108485, -1.389630591760198541 ) ) ;
#22078 = CARTESIAN_POINT ( 'NONE',  ( 5.930640623865814476, 1.760069778787749506, 0.4843501209313359479 ) ) ;
#22079 = CARTESIAN_POINT ( 'NONE',  ( 2.442595505675814405, 0.4281495253689853175, 1.924161874619955359 ) ) ;
#22080 = CARTESIAN_POINT ( 'NONE',  ( 4.324404969281474109, -0.8226261416362996570, -1.726585468271451651 ) ) ;
#22081 = VERTEX_POINT ( 'NONE', #73418 ) ;
#22082 = CARTESIAN_POINT ( 'NONE',  ( 0.000000000000000000, 14.48154074412737202, -12.00000000000000178 ) ) ;
#22083 = CARTESIAN_POINT ( 'NONE',  ( 4.545333244533083850, 1.760332640988309993, -0.8834868730601146414 ) ) ;
#22084 = CARTESIAN_POINT ( 'NONE',  ( 0.04082682177056726897, -1.500436592000290670, -1.232479804542076618 ) ) ;
#22085 = VERTEX_POINT ( 'NONE', #8419 ) ;
#22086 = CARTESIAN_POINT ( 'NONE',  ( -5.743814354044916470, 6.730146830254374990, -1.199719254218453823 ) ) ;
#22087 = CARTESIAN_POINT ( 'NONE',  ( -6.861835142292179057, 9.098836647464588978, 1.443375672974064550 ) ) ;
#22089 = CARTESIAN_POINT ( 'NONE',  ( 6.983858524370782916, 7.320458831286981827, 0.7216878364870328300 ) ) ;
#22088 = CARTESIAN_POINT ( 'NONE',  ( 6.760712154708803823, 11.03924794713562818, 1.040834085586084257E-14 ) ) ;
#22091 = ORIENTED_EDGE ( 'NONE', *, *, #182300, .F. ) ;
#22090 = CARTESIAN_POINT ( 'NONE',  ( 4.969353466749234727, -1.617520173792227567, -1.019718193788564209 ) ) ;
#22092 = ADVANCED_FACE ( 'NONE', ( #154687 ), #74505, .F. ) ;
#22093 = CARTESIAN_POINT ( 'NONE',  ( 0.4466624375424713689, 2.201045718399210038, 0.1599725512250807224 ) ) ;
#22094 = DIRECTION ( 'NONE',  ( -0.000000000000000000, -1.000000000000000000, -0.000000000000000000 ) ) ;
#22095 = CARTESIAN_POINT ( 'NONE',  ( 5.848296790250511634, 0.9903421736442417078, -1.752559156024376508 ) ) ;
#22096 = CARTESIAN_POINT ( 'NONE',  ( 0.07680821025391608436, 6.948789780205374633, -2.405840108717867132 ) ) ;
#22097 = CARTESIAN_POINT ( 'NONE',  ( -5.911293591272317904, 7.247452768069575058, 1.263797332732160106 ) ) ;
#22098 = CARTESIAN_POINT ( 'NONE',  ( -6.429544252029797846, -6.709867743870402634, -6.981856502304072620 ) ) ;
#22099 = CARTESIAN_POINT ( 'NONE',  ( 3.227070907399377298, -1.911900318415656441, -0.7948586591664740242 ) ) ;
#22100 = CARTESIAN_POINT ( 'NONE',  ( -6.307567778855718288, 8.381915046796901692, -1.599625672291263179 ) ) ;
#22101 = CARTESIAN_POINT ( 'NONE',  ( -4.665006653791238911, 8.307176129776033591, 0.4851093158183654719 ) ) ;
#22103 = CARTESIAN_POINT ( 'NONE',  ( 0.6026772488060898603, -0.7295331166810551382, -2.035022307366324945 ) ) ;
#22102 = CARTESIAN_POINT ( 'NONE',  ( -4.277761160311629673, 4.949475094240346706, 1.199719254218462483 ) ) ;
#22104 = CARTESIAN_POINT ( 'NONE',  ( -11.06955610715284166, 7.104274754441156858, 4.637919682314346481 ) ) ;
#22105 = EDGE_CURVE ( 'NONE', #186231, #53161, #20347, .T. ) ;
#22106 = CARTESIAN_POINT ( 'NONE',  ( 5.560252395380215873, 6.619954228432645138, 1.082531754730549078 ) ) ;
#22107 = CARTESIAN_POINT ( 'NONE',  ( 7.846302513400016387, -6.700642373080272662, -7.709579522695857889 ) ) ;
#22108 = CARTESIAN_POINT ( 'NONE',  ( -1.364683531250000748, 13.17187500034139980, 0.000000000000000000 ) ) ;
#22110 = CARTESIAN_POINT ( 'NONE',  ( -3.969505113751027547, 7.853116076009993840, 1.214306433183764966E-14 ) ) ;
#22109 = CARTESIAN_POINT ( 'NONE',  ( 6.825078400183550720, 7.629137130509051623, 2.355651831298340326 ) ) ;
#22111 = ADVANCED_FACE ( 'NONE', ( #208744 ), #175220, .T. ) ;
#22112 = CARTESIAN_POINT ( 'NONE',  ( 4.307042110543488178, 1.062484115506344473, -1.370455642081182646 ) ) ;
#22113 = COLOUR_RGB ( '', 0.40784314, 0.44705882, 0.49803922) ;
#22114 = CARTESIAN_POINT ( 'NONE',  ( -2.767835915484202047, 6.380892334706859792, -0.7998128361456281477 ) ) ;
#22115 = CARTESIAN_POINT ( 'NONE',  ( 3.871986384844767315, -2.040452582458017083, 0.3490408808229996662 ) ) ;
#22116 = CARTESIAN_POINT ( 'NONE',  ( 4.517270869736185190, -1.935087425045402654, 0.8595401143802297028 ) ) ;
#22117 = CARTESIAN_POINT ( 'NONE',  ( 5.601490020740366838, 9.686822124172440596, 1.040834085586084257E-14 ) ) ;
#22118 = CARTESIAN_POINT ( 'NONE',  ( -1.201851678989727383E-14, 4.071875000341425022, 1.575800808251672791 ) ) ;
#22119 = CARTESIAN_POINT ( 'NONE',  ( 1.305442304231837714, -1.549127766076626056, -1.215949579239549161 ) ) ;
#22120 = CARTESIAN_POINT ( 'NONE',  ( 0.4570967503451648373, -1.639016809899789040, 0.9851245988263114262 ) ) ;
#22121 = CARTESIAN_POINT ( 'NONE',  ( 5.261813964552005451, 1.126222290254262015, 1.996463630829442337 ) ) ;
#22122 = CARTESIAN_POINT ( 'NONE',  ( 1.822601884235462766, 1.703052241681313861, 0.6583118566880485911 ) ) ;
#22123 = CARTESIAN_POINT ( 'NONE',  ( 4.179656494762836516, 8.098292687190454586, -0.7998128361456362523 ) ) ;
#22124 = CARTESIAN_POINT ( 'NONE',  ( 4.134873662043553111, 7.767843672452050541, -0.7216878364870197293 ) ) ;
#22125 = CARTESIAN_POINT ( 'NONE',  ( -6.832419346282942563, 10.05857410638369487, 1.199719254218453823 ) ) ;
#22126 = CARTESIAN_POINT ( 'NONE',  ( 3.164317521226766239, 2.013376229028215558, -0.004237188189804701709 ) ) ;
#22127 = CARTESIAN_POINT ( 'NONE',  ( 3.186327686730246800, 1.093712407854827706, -1.628379936052851917 ) ) ;
#22128 = CARTESIAN_POINT ( 'NONE',  ( -8.044065211609668253, 8.279164256499745633, 0.7998128361456602331 ) ) ;
#22129 = CARTESIAN_POINT ( 'NONE',  ( -5.494078562035765501, 7.432844293840273231, -1.599625672291256295 ) ) ;
#22130 = CARTESIAN_POINT ( 'NONE',  ( 0.1753634416057740786, 1.334841368177059895, -2.397339160348281428 ) ) ;
#22132 = CARTESIAN_POINT ( 'NONE',  ( 4.381574371570028603, 1.156860168461280036, 1.339510341777202074 ) ) ;
#22131 = CARTESIAN_POINT ( 'NONE',  ( 5.789036971029382528, 1.582348866732422810, 1.366464223246833809 ) ) ;
#22133 = CARTESIAN_POINT ( 'NONE',  ( -0.6125000000000349054, 2.208333333333325932, -1.060881119635983083 ) ) ;
#22134 = CARTESIAN_POINT ( 'NONE',  ( 0.3225714733509216781, 2.098294765757203528, 0.6321472216322538973 ) ) ;
#22135 = CARTESIAN_POINT ( 'NONE',  ( 0.2216635874392547945, 1.664573546290064598, 0.5083179512348577900 ) ) ;
#22136 = CARTESIAN_POINT ( 'NONE',  ( 7.935599982700328958, 8.152621489438862667, 0.7998128361456481317 ) ) ;
#22137 = CARTESIAN_POINT ( 'NONE',  ( -2.398572866711294438, 5.287202466803545775, -0.8077998227820496480 ) ) ;
#22138 = CARTESIAN_POINT ( 'NONE',  ( 5.731119460814408484, 2.295830932937119595, 0.1164615576392889484 ) ) ;
#22139 = FACE_OUTER_BOUND ( 'NONE', #132445, .T. ) ;
#22140 = CARTESIAN_POINT ( 'NONE',  ( 6.468101748929986350, 1.443884034049055298, 0.9595089302780019924 ) ) ;
#22141 = CARTESIAN_POINT ( 'NONE',  ( 1.823171247573553311, 2.059948494222668014, 0.7922594597074559264 ) ) ;
#22142 = CARTESIAN_POINT ( 'NONE',  ( 0.5851434883720012525, 2.077150299251043553, 0.6315224188822368134 ) ) ;
#22143 = CARTESIAN_POINT ( 'NONE',  ( 11.04536101718726293, 0.000000000000000000, 1.099999999999996758 ) ) ;
#22144 = CARTESIAN_POINT ( 'NONE',  ( 1.130240340503264829, 2.115179321838219551, 0.09787962981822571906 ) ) ;
#22145 = CARTESIAN_POINT ( 'NONE',  ( 4.156250000000002665, -1.895863743163992199, 0.7852924748302037017 ) ) ;
#22146 = DIRECTION ( 'NONE',  ( 0.000000000000000000, -1.000000000000000000, 0.000000000000000000 ) ) ;
#22147 = CARTESIAN_POINT ( 'NONE',  ( 4.752910067621118451, -1.547527511699481106, 1.147055677608086466 ) ) ;
#22148 = ORIENTED_EDGE ( 'NONE', *, *, #75556, .F. ) ;
#22150 = CARTESIAN_POINT ( 'NONE',  ( 1.364683531249986537, -0.8239583329919186738, 0.7879004041258500513 ) ) ;
#22149 = CARTESIAN_POINT ( 'NONE',  ( 1.874976642369927005, -0.1173453557595251634, -2.289501271392534676 ) ) ;
#22151 = CARTESIAN_POINT ( 'NONE',  ( 6.145923705696426431, 6.064665832934283962, 0.7998128361456341429 ) ) ;
#22152 = CARTESIAN_POINT ( 'NONE',  ( 4.645640190976921602, 8.571663989448405019, 1.040834085586084257E-14 ) ) ;
#22153 = CARTESIAN_POINT ( 'NONE',  ( 3.791809789012908549, 2.091298394358314550, -0.7490737107957652352 ) ) ;
#22154 = CARTESIAN_POINT ( 'NONE',  ( -9.164948653158003111, 9.794787638213568570, -0.7216878364870267237 ) ) ;
#22155 = DIRECTION ( 'NONE',  ( 0.000000000000000000, 0.000000000000000000, 1.000000000000000000 ) ) ;
#22156 = CARTESIAN_POINT ( 'NONE',  ( 7.144783764721768904, 7.437928601704619780, 1.040834085586084257E-14 ) ) ;
#22157 = CARTESIAN_POINT ( 'NONE',  ( -8.310784975052685652, 9.758632561392040827, -1.082531754730543083 ) ) ;
#22158 = AXIS2_PLACEMENT_3D ( 'NONE', #195117, #110734, #212405 ) ;
#22159 = CARTESIAN_POINT ( 'NONE',  ( 6.427974226654860956, 7.632296364919712417, -1.082531754730548412 ) ) ;
#22160 = ORIENTED_EDGE ( 'NONE', *, *, #214308, .T. ) ;
#22161 = CARTESIAN_POINT ( 'NONE',  ( 1.723279953462612202, 1.994870059565261755, 0.2930690452552578429 ) ) ;
#22163 = CARTESIAN_POINT ( 'NONE',  ( 6.777782349474076540, -2.001779569883685106, 0.4972090909861492936 ) ) ;
#22162 = CARTESIAN_POINT ( 'NONE',  ( 8.263858322729371153, 9.599921783727809910, -1.199719254218446718 ) ) ;
#22164 =( LENGTH_UNIT ( ) NAMED_UNIT ( * ) SI_UNIT ( .MILLI., .METRE. ) );
#22165 = CARTESIAN_POINT ( 'NONE',  ( 6.495764994278809823, 7.711385593814346073, 1.082531754730549967 ) ) ;
#22166 = AXIS2_PLACEMENT_3D ( 'NONE', #156619, #11401, #205334 ) ;
#22167 = CARTESIAN_POINT ( 'NONE',  ( 6.515217664332146441, -1.685650512211306129, 0.4329046258050253670 ) ) ;
#22168 = CARTESIAN_POINT ( 'NONE',  ( -3.923301836239767137, 8.994671190470434397, 0.7749999999999996891 ) ) ;
#22169 = CARTESIAN_POINT ( 'NONE',  ( -0.6823417656250003738, 2.967708333674754062, -1.181850606188749264 ) ) ;
#22170 = CARTESIAN_POINT ( 'NONE',  ( 1.405125766016354305, -0.4367768486257683769, 1.714848201936822525 ) ) ;
#22171 = CARTESIAN_POINT ( 'NONE',  ( 0.2994542103806375200, 1.388483683912977495, -1.462447666687356485 ) ) ;
#22172 = CARTESIAN_POINT ( 'NONE',  ( 6.550362485727940332, -1.338708790221679656, 1.112040286498132025 ) ) ;
#22173 = CARTESIAN_POINT ( 'NONE',  ( 4.634495141935854434, 0.3908333592176889137, 2.258673302944668837 ) ) ;
#22174 = CARTESIAN_POINT ( 'NONE',  ( 3.450948914068392881, 0.4461466885457600062, -1.786139022923169506 ) ) ;
#22175 = EDGE_CURVE ( 'NONE', #119302, #182623, #180980, .T. ) ;
#22176 = CARTESIAN_POINT ( 'NONE',  ( 7.411503528164766763, 11.79850454950093841, 1.040834085586084257E-14 ) ) ;
#22177 =( NAMED_UNIT ( * ) SI_UNIT ( $, .STERADIAN. ) SOLID_ANGLE_UNIT ( ) );
#22178 = CARTESIAN_POINT ( 'NONE',  ( 4.032112419961201510, 0.9767663869549062516, -1.542106374223570775 ) ) ;
#22179 = CARTESIAN_POINT ( 'NONE',  ( 5.414685466650038137, -1.281359335986744341, -1.556910257834144051 ) ) ;
#22180 = CARTESIAN_POINT ( 'NONE',  ( -8.696665468161981494, 12.23352791524263239, -1.199719254218446718 ) ) ;
#22182 = CARTESIAN_POINT ( 'NONE',  ( -5.932574734431526942, 9.079031735882207244, 1.199719254218454489 ) ) ;
#22181 = CARTESIAN_POINT ( 'NONE',  ( 3.819400769403025198, -0.1694044215128273911, 2.256236840065691585 ) ) ;
#22183 = CARTESIAN_POINT ( 'NONE',  ( 0.2058769709349675681, -0.5595275159893696726, 2.030311192619388638 ) ) ;
#22184 = CARTESIAN_POINT ( 'NONE',  ( 9.262488864310135739, 13.63671387857608508, 6.830742452943137089 ) ) ;
#22185 =( BOUNDED_CURVE ( )  B_SPLINE_CURVE ( 2, ( #78018, #210135, #14061, #113793, #10869, #13005, #63900 ),
 .UNSPECIFIED., .F., .T. ) 
 B_SPLINE_CURVE_WITH_KNOTS ( ( 3, 2, 2, 3 ),
 ( 0.3605655240965703334, 0.3630952380952380820, 0.3690476190476190688, 0.3715773330463134627 ),
 .UNSPECIFIED. ) 
 CURVE ( )  GEOMETRIC_REPRESENTATION_ITEM ( )  RATIONAL_B_SPLINE_CURVE ( ( 0.9345202395942613371, 0.9430618748659225226, 1.000000000000000000, 0.8660254037844387076, 1.000000000000000000, 0.9430618748653227801, 0.9345202395940813700 ) ) 
 REPRESENTATION_ITEM ( '' )  );
#22186 = CARTESIAN_POINT ( 'NONE',  ( 4.018080225218490398, 2.055083638104511223, -0.2504045000601487492 ) ) ;
#22187 = CARTESIAN_POINT ( 'NONE',  ( 9.083072846151447166, 12.68433652289702884, 1.199719254218450271 ) ) ;
#22188 = CARTESIAN_POINT ( 'NONE',  ( 0.6801582343749917881, 1.255208333674727506, 1.178068619123834759 ) ) ;
#22189 = CARTESIAN_POINT ( 'NONE',  ( 5.531924462405465981, -2.068776410037334479, 0.4646945096876684556 ) ) ;
#22190 = CONTEXT_DEPENDENT_SHAPE_REPRESENTATION ( #103179, #78284 ) ;
#22192 = CARTESIAN_POINT ( 'NONE',  ( 2.156748612084181005, -1.489394325481137260, 1.221923121036755600 ) ) ;
#22191 = CARTESIAN_POINT ( 'NONE',  ( -9.775592450653132204, 11.36361159963886891, -1.199719254218441611 ) ) ;
#22193 = B_SPLINE_CURVE_WITH_KNOTS ( 'NONE', 3,
 ( #89068, #154057, #73867, #41390 ),
 .UNSPECIFIED., .F., .F.,
 ( 4, 4 ),
 ( 0.000000000000000000, 6.033646489354490427E-05 ),
 .UNSPECIFIED. ) ;
#22194 = DIRECTION ( 'NONE',  ( 0.000000000000000000, 0.1992968566527040242, 0.9799391628710180102 ) ) ;
#22195 = CARTESIAN_POINT ( 'NONE',  ( 0.1859136753566691391, -1.208741973239912726, -1.555490313720475415 ) ) ;
#22196 = CARTESIAN_POINT ( 'NONE',  ( 5.383996397958233260, 5.453953017138946535, -0.7216878364870458196 ) ) ;
#22197 = CARTESIAN_POINT ( 'NONE',  ( 5.886971415934090679, 5.980320297827544707, -0.1280069804882408846 ) ) ;
#22198 = CARTESIAN_POINT ( 'NONE',  ( 1.284279953904119864, 3.296639714193937198, -0.7749999999999910294 ) ) ;
#22199 = CARTESIAN_POINT ( 'NONE',  ( -5.101945877444165944, 4.846691699973280976, 0.000000000000000000 ) ) ;
#22200 = CARTESIAN_POINT ( 'NONE',  ( 0.2291713999985908190, 1.525799623841477493, -1.614749986458098974 ) ) ;
#22201 = CARTESIAN_POINT ( 'NONE',  ( 3.909285118862667829, 1.805215983022747439, 1.084321332058492571 ) ) ;
#22202 = CARTESIAN_POINT ( 'NONE',  ( -3.871735385154307263, 6.674719161725423788, -1.199719254218450271 ) ) ;
#22203 = CARTESIAN_POINT ( 'NONE',  ( 7.623762449586013901, 7.788811034138823253, 1.040834085586084257E-14 ) ) ;
#22204 = CARTESIAN_POINT ( 'NONE',  ( 0.2032580500000652490, -1.434579632348313982, -1.185340245312079377 ) ) ;
#22205 = CARTESIAN_POINT ( 'NONE',  ( 5.615048174354031474, 9.702639970055050966, 0.7998128361456462443 ) ) ;
#22206 = EDGE_CURVE ( 'NONE', #211791, #63320, #93168, .T. ) ;
#22207 = CARTESIAN_POINT ( 'NONE',  ( -6.861835142292179057, 9.098836647464588978, 1.443375672974064550 ) ) ;
#22208 = CARTESIAN_POINT ( 'NONE',  ( -8.595506201384022660, 11.05117653974661529, 1.443375672974064550 ) ) ;
#22209 = CARTESIAN_POINT ( 'NONE',  ( 1.635180430577408028, 1.980530345366804834, 0.7584260845197098311 ) ) ;
#22210 = CARTESIAN_POINT ( 'NONE',  ( -5.752402313948099533, 9.933162809573264695, -0.7998128361456362523 ) ) ;
#22212 = CARTESIAN_POINT ( 'NONE',  ( 3.279693232472491893, -1.891448704997201302, 0.5207070127687256633 ) ) ;
#22211 = CARTESIAN_POINT ( 'NONE',  ( -1.225000000000042277, 0.9791666666666765106, -0.7072540797572898219 ) ) ;
#22213 = CARTESIAN_POINT ( 'NONE',  ( 2.254944280175336324, -1.671361177491991201, 1.370965666894090385 ) ) ;
#22214 = CARTESIAN_POINT ( 'NONE',  ( 2.173174093899932657, 1.133995793187540180, 1.450494936146892622 ) ) ;
#22216 = CARTESIAN_POINT ( 'NONE',  ( -5.013591113304329383, 6.604120902668014992, -1.237928687022475494 ) ) ;
#22215 = CARTESIAN_POINT ( 'NONE',  ( -4.930325137224961907, 5.781076077297750970, -1.199719254218453823 ) ) ;
#22217 = CARTESIAN_POINT ( 'NONE',  ( 3.749730547248275148, 0.6284987560769598192, 1.623061768561576468 ) ) ;
#22218 = CARTESIAN_POINT ( 'NONE',  ( 4.799223189557548785, 7.582548906917042864, -1.082531754730549078 ) ) ;
#22219 = CARTESIAN_POINT ( 'NONE',  ( -10.78237064342727791, 6.270194388237658956, -4.501389708959286473 ) ) ;
#22220 = CARTESIAN_POINT ( 'NONE',  ( 0.9542513359644848592, 2.159166806557303531, -0.1069676271590186134 ) ) ;
#22221 = CARTESIAN_POINT ( 'NONE',  ( 2.970077202574809228, 1.701686883299750264, 1.080900613174784475 ) ) ;
#22222 = CARTESIAN_POINT ( 'NONE',  ( -0.09924927195301232186, -9.920000000000094076, -10.99955234463955556 ) ) ;
#22223 = CARTESIAN_POINT ( 'NONE',  ( 0.3038912542124502236, -0.5749842496362895794, 2.083749421223294540 ) ) ;
#22224 = CARTESIAN_POINT ( 'NONE',  ( 2.272288244244465627, -1.214158342444570327, 1.553133305774859974 ) ) ;
#22225 = CIRCLE ( 'NONE', #119114, 1.224999999999996980 ) ;
#22226 = CARTESIAN_POINT ( 'NONE',  ( 6.509000000000014552, 2.444259026362519904, 2.383015625331697862 ) ) ;
#22227 = CARTESIAN_POINT ( 'NONE',  ( 2.683070245604711523, 1.375115853580029635, 1.371619177916082011 ) ) ;
#22231 = ORIENTED_EDGE ( 'NONE', *, *, #208628, .F. ) ;
#22230 = EDGE_CURVE ( 'NONE', #130986, #24518, #209809, .T. ) ;
#22229 = CARTESIAN_POINT ( 'NONE',  ( -5.492461627311929995, 5.580495784718250363, 0.000000000000000000 ) ) ;
#22228 = SURFACE_SIDE_STYLE ('',( #74226 ) ) ;
#22232 = CARTESIAN_POINT ( 'NONE',  ( -3.634994581795317536, 7.254927755487573293, 0.000000000000000000 ) ) ;
#22233 = CARTESIAN_POINT ( 'NONE',  ( -0.2106854629475244378, -0.004120941679102134263, -1.996958217618934661 ) ) ;
#22234 = CARTESIAN_POINT ( 'NONE',  ( 5.387385936583818591, 7.378645907471495846, -1.599625672291283607 ) ) ;
#22235 = CIRCLE ( 'NONE', #171004, 11.09999999999999964 ) ;
#22236 = CARTESIAN_POINT ( 'NONE',  ( -6.306477729012051725, 7.386587434382707151, 1.199719254218452047 ) ) ;
#22237 = CARTESIAN_POINT ( 'NONE',  ( -7.119966945832006289, 8.335658187339330283, 1.199719254218452047 ) ) ;
#22238 = CARTESIAN_POINT ( 'NONE',  ( -6.397211430516217767, 6.896709913541772430, -0.8587214783020010733 ) ) ;
#22239 = EDGE_CURVE ( 'NONE', #36876, #213748, #164278, .T. ) ;
#22240 = CARTESIAN_POINT ( 'NONE',  ( 6.756845507909216231, -1.789895876690169585, 1.456048205946461005 ) ) ;
#22241 = LINE ( 'NONE', #189041, #28887 ) ;
#22242 = CARTESIAN_POINT ( 'NONE',  ( 3.942202469084721272, -0.9707516781715104237, 1.704694321266352786 ) ) ;
#22243 = CARTESIAN_POINT ( 'NONE',  ( 7.796102023057898123, 9.054206100777749455, -1.199719254218441611 ) ) ;
#22244 = CARTESIAN_POINT ( 'NONE',  ( 1.565077508395201988, -1.076315722900993643, 1.704939445326451475 ) ) ;
#22245 = ORIENTED_EDGE ( 'NONE', *, *, #57679, .F. ) ;
#22246 = CARTESIAN_POINT ( 'NONE',  ( 2.677094534585529928, 1.813448998079300489, -1.092781719356890946 ) ) ;
#22247 = CARTESIAN_POINT ( 'NONE',  ( -1.500000000000013101, 1.452083334016150085, 0.8660254037844403729 ) ) ;
#22249 = CARTESIAN_POINT ( 'NONE',  ( -6.612626235163205024, 8.737816579155630592, -1.599625672291263179 ) ) ;
#22248 = CARTESIAN_POINT ( 'NONE',  ( 0.000000000000000000, 13.49999999999999822, -1.500000000000000222 ) ) ;
#22250 = CARTESIAN_POINT ( 'NONE',  ( 2.782953997937851920, 1.302219384484751830, 1.301801165952347628 ) ) ;
#22251 = ORIENTED_EDGE ( 'NONE', *, *, #167500, .F. ) ;
#22252 = CARTESIAN_POINT ( 'NONE',  ( -8.272446282632566650, 12.80293776304669962, 0.7998128361456481317 ) ) ;
#22253 = CARTESIAN_POINT ( 'NONE',  ( -15.75000000000000000, 13.40000000000000036, -3.200000000000001510 ) ) ;
#22254 = CARTESIAN_POINT ( 'NONE',  ( 3.691739789689612472, 1.995538565534977549, -0.7177698711837015022 ) ) ;
#22255 = CARTESIAN_POINT ( 'NONE',  ( 0.2691533882960769897, 1.057504993221158873, 1.506941669042777265 ) ) ;
#22256 = CARTESIAN_POINT ( 'NONE',  ( 1.499999999999989120, 5.577083334016153415, -0.8660254037844323793 ) ) ;
#22257 = CARTESIAN_POINT ( 'NONE',  ( 6.317209508963599340, 9.457495962844502557, 1.199719254218462483 ) ) ;
#22258 = CARTESIAN_POINT ( 'NONE',  ( 4.288392841435205938, -2.037809284099707074, -0.3060936983758227870 ) ) ;
#22259 = ADVANCED_FACE ( 'NONE', ( #112398 ), #16934, .T. ) ;
#22261 = CARTESIAN_POINT ( 'NONE',  ( 1.276629239279066574, 1.701104413791530767, -0.7050613402737049284 ) ) ;
#22260 = CARTESIAN_POINT ( 'NONE',  ( -7.711890448074853133, 7.891627032375787998, -0.7998128361456291469 ) ) ;
#22262 = CARTESIAN_POINT ( 'NONE',  ( 6.015607636943825831, 6.078019264660407650, -0.5714835875584244329 ) ) ;
#22263 = CARTESIAN_POINT ( 'NONE',  ( -1.445103857046265317, 8.688264192038502642, 2.625611233228785313 ) ) ;
#22264 = CARTESIAN_POINT ( 'NONE',  ( 10.93053916617009413, -8.254340240174414589, -0.1907932708458892346 ) ) ;
#22265 = CARTESIAN_POINT ( 'NONE',  ( 0.8212658843103730621, 2.040464674744349338, 0.8412164853940640175 ) ) ;
#22266 = CARTESIAN_POINT ( 'NONE',  ( 4.218261219551087571, -1.158436920226207034, -1.943184041606202950 ) ) ;
#22267 = CARTESIAN_POINT ( 'NONE',  ( -6.724481002698115439, 10.78905223654906109, -0.7216878364870267237 ) ) ;
#22268 = CARTESIAN_POINT ( 'NONE',  ( 4.060681591697304249, 0.4892206165460743494, 1.744179128828279302 ) ) ;
#22269 = CARTESIAN_POINT ( 'NONE',  ( 3.819475811356612738, -1.325201190313522792, -1.383632964731799531 ) ) ;
#22270 = CARTESIAN_POINT ( 'NONE',  ( 5.635237798060349412, -0.04710594754482424346, -2.069988403558701062 ) ) ;
#22271 = CARTESIAN_POINT ( 'NONE',  ( 0.6823417656249899377, 3.988541667008085767, -1.181850606188754593 ) ) ;
#22272 = CARTESIAN_POINT ( 'NONE',  ( 3.590661340855735961, -0.3832702008734929500, -1.933690442540521470 ) ) ;
#22273 = CARTESIAN_POINT ( 'NONE',  ( 1.430555067506549483, 1.855864167146383581, 0.5162276523679990570 ) ) ;
#22274 = CARTESIAN_POINT ( 'NONE',  ( 3.572993900519233712, 0.04689164532409998559, -1.870237235490713079 ) ) ;
#22275 = CARTESIAN_POINT ( 'NONE',  ( 3.000898454221593958, -0.6702494718498009929, -2.208213912191819617 ) ) ;
#22276 = CARTESIAN_POINT ( 'NONE',  ( 3.472968545230222581, 1.681562272349636622, 0.7977436208898255332 ) ) ;
#22277 = CARTESIAN_POINT ( 'NONE',  ( -0.6823417656250212460, 4.051041667008085767, 1.181850606188767472 ) ) ;
#22278 = DIRECTION ( 'NONE',  ( 7.993605777301127091E-15, 0.000000000000000000, 1.000000000000000000 ) ) ;
#22279 = CARTESIAN_POINT ( 'NONE',  ( 1.998786363724443182, -0.5629491194198692483, -2.029361489363819882 ) ) ;
#22280 = CARTESIAN_POINT ( 'NONE',  ( 2.521453382017309952, 5.885520012421409319, 0.000000000000000000 ) ) ;
#22282 = DIRECTION ( 'NONE',  ( -0.000000000000000000, -1.000000000000000000, -0.000000000000000000 ) ) ;
#22281 = CARTESIAN_POINT ( 'NONE',  ( 7.065207446497155708, 9.336104335703744539, 0.000000000000000000 ) ) ;
#22283 = CARTESIAN_POINT ( 'NONE',  ( 3.340189922722580196, -1.266226476691566738, -1.700888996046201029 ) ) ;
#22284 = CARTESIAN_POINT ( 'NONE',  ( 3.006787879153326681, 6.373552747333731006, -0.4818892653130519843 ) ) ;
#22285 = CARTESIAN_POINT ( 'NONE',  ( 0.8264327134144221487, -0.9118592345104499231, -1.802339519251413780 ) ) ;
#22286 = CARTESIAN_POINT ( 'NONE',  ( -1.364683531250000748, 0.7593750003414210248, 0.000000000000000000 ) ) ;
#22287 = CARTESIAN_POINT ( 'NONE',  ( -2.480778921620681921, 5.838066475291996404, 1.040834085586084257E-14 ) ) ;
#22288 = CARTESIAN_POINT ( 'NONE',  ( 6.173040012923759257, 6.096301524699504704, -0.7998128361456281477 ) ) ;
#22289 = ORIENTED_EDGE ( 'NONE', *, *, #26436, .F. ) ;
#22290 = CARTESIAN_POINT ( 'NONE',  ( 0.7730135719010817752, -2.035059957909639561, -0.7290066412228360937 ) ) ;
#22291 = DIRECTION ( 'NONE',  ( 0.5038915848679205167, -0.5182601445718857391, 0.6910135260959974213 ) ) ;
#22294 = CARTESIAN_POINT ( 'NONE',  ( 3.714570900464285064, 4.396382807705524698, 1.082531754730560403 ) ) ;
#22293 = CARTESIAN_POINT ( 'NONE',  ( 6.825078400183550720, 7.629137130509051623, 2.555651831298339616 ) ) ;
#22292 = CARTESIAN_POINT ( 'NONE',  ( 5.468734858265785093, 7.473552982767158070, 1.599625672291269396 ) ) ;
#22295 = DIRECTION ( 'NONE',  ( -0.2150645590070936197, 0.8781765503997437383, 0.4272624273056206401 ) ) ;
#22296 = CARTESIAN_POINT ( 'NONE',  ( 5.981657729715996297, -0.6748525008196132324, 1.900413905137773529 ) ) ;
#22297 = CARTESIAN_POINT ( 'NONE',  ( -7.537970219518075332, 10.77775377520434574, -1.082531754730543971 ) ) ;
#22298 = EDGE_CURVE ( 'NONE', #142643, #5559, #60371, .T. ) ;
#22300 = B_SPLINE_CURVE_WITH_KNOTS ( 'NONE', 3,
 ( #69457, #135562, #71589, #153940, #4444, #203718, #120443, #156075 ),
 .UNSPECIFIED., .F., .F.,
 ( 4, 2, 2, 4 ),
 ( 0.000000000000000000, 0.0001671579969091580335, 0.0003343159938183160669, 0.0006686319876366318086 ),
 .UNSPECIFIED. ) ;
#22299 = CARTESIAN_POINT ( 'NONE',  ( -0.02351032182101517320, -2.127384168920816165, -0.5261613093957145937 ) ) ;
#22301 = CARTESIAN_POINT ( 'NONE',  ( -9.617648866954029430, -9.063431457505044975, 0.6035590660249372519 ) ) ;
#22303 = CARTESIAN_POINT ( 'NONE',  ( -1.364683531250000748, 12.10937500034139980, 0.000000000000000000 ) ) ;
#22302 = CARTESIAN_POINT ( 'NONE',  ( 0.7962373781299083575, -0.8115885651059464578, 2.112105989495225877 ) ) ;
#22304 = CARTESIAN_POINT ( 'NONE',  ( -9.996439331977562404, 10.55693406359564790, 0.7998128361456462443 ) ) ;
#22306 = CARTESIAN_POINT ( 'NONE',  ( 0.8959254483255777446, -0.8623397379431455567, -1.710623486014851480 ) ) ;
#22305 = CARTESIAN_POINT ( 'NONE',  ( -5.165293336682207581, 8.009630745229104676, 1.082531754730548412 ) ) ;
#22307 = CARTESIAN_POINT ( 'NONE',  ( 0.6823417656249882723, 1.488541667008083547, -1.181850606188749264 ) ) ;
#22308 = CARTESIAN_POINT ( 'NONE',  ( 1.224999999999971223, 2.708333334016145066, -0.7072540797573039217 ) ) ;
#22309 = CARTESIAN_POINT ( 'NONE',  ( 1.499999999999997113, 9.895833333333335702, -0.8660254037844378194 ) ) ;
#22310 = CARTESIAN_POINT ( 'NONE',  ( 3.158550911874979938, -1.305529951647845355, 1.127390448682374924 ) ) ;
#22311 = CARTESIAN_POINT ( 'NONE',  ( 3.881377115262159894, 7.750300077773022878, 0.7998128361456271485 ) ) ;
#22312 = CARTESIAN_POINT ( 'NONE',  ( 2.020411781336392210, 1.649200945362235826, 0.6424177339450982682 ) ) ;
#22313 = CARTESIAN_POINT ( 'NONE',  ( 2.543610208494262892, -1.877569574052952328, 0.7265587727790027150 ) ) ;
#22314 = CARTESIAN_POINT ( 'NONE',  ( 9.480175724453529185, 12.08329098332774265, 1.599625672291279388 ) ) ;
#22315 = CARTESIAN_POINT ( 'NONE',  ( 5.139771110516938357, -1.557344429106276573, -1.563758303505815572 ) ) ;
#22316 = ORIENTED_EDGE ( 'NONE', *, *, #129911, .F. ) ;
#22317 = CARTESIAN_POINT ( 'NONE',  ( 4.359631895039292715, -1.563893385546542003, -1.278231166955777764 ) ) ;
#22318 = CARTESIAN_POINT ( 'NONE',  ( -6.129167961829681488, 9.308390501180058507, -1.199719254218452047 ) ) ;
#22320 = CARTESIAN_POINT ( 'NONE',  ( 4.218375177057286152, 1.978055892313890229, 0.3905773888849966013 ) ) ;
#22319 = CARTESIAN_POINT ( 'NONE',  ( 4.196021508500130004, 1.385991406618786836, 1.604897850144955340 ) ) ;
#22322 = VERTEX_POINT ( 'NONE', #163225 ) ;
#22321 = CARTESIAN_POINT ( 'NONE',  ( 4.447391390197759975, -1.653601938829275975, 0.7403539279892316083 ) ) ;
#22323 = CARTESIAN_POINT ( 'NONE',  ( 4.278479993564246797, 7.149254538203735798, 1.199719254218452047 ) ) ;
#22324 = VERTEX_POINT ( 'NONE', #14807 ) ;
#22325 = CARTESIAN_POINT ( 'NONE',  ( 0.8834254411415434216, 1.253375741028007084, 1.388844808110502038 ) ) ;
#22326 = CIRCLE ( 'NONE', #84509, 0.08000000000000050127 ) ;
#22327 = CARTESIAN_POINT ( 'NONE',  ( 6.692070433991195166, -0.7751425012093198230, 1.651373049820707317 ) ) ;
#22328 = CARTESIAN_POINT ( 'NONE',  ( -0.1583346312582509796, -1.114004300041637974, -1.428896152673633013 ) ) ;
#22329 = CARTESIAN_POINT ( 'NONE',  ( -4.223528545856940042, 4.886203710709899006, -1.199719254218446718 ) ) ;
#22330 = CARTESIAN_POINT ( 'NONE',  ( -10.30104275384242740, 4.689840931292195592, -5.506867539468097483 ) ) ;
#22331 = CARTESIAN_POINT ( 'NONE',  ( -3.931431380944478082, 2.807600633707135529, 0.7750000000000135669 ) ) ;
#22332 = PRESENTATION_LAYER_ASSIGNMENT (  '', '', ( #198748 ) ) ;
#22333 = CARTESIAN_POINT ( 'NONE',  ( -1.201851678989727383E-14, 2.759375000341417916, -1.575800808251660134 ) ) ;
#22334 = CARTESIAN_POINT ( 'NONE',  ( 0.4219365929402639215, -1.902980170924161385, 0.1897552588234762416 ) ) ;
#22335 = ORIENTED_EDGE ( 'NONE', *, *, #201684, .T. ) ;
#22336 = CARTESIAN_POINT ( 'NONE',  ( 7.851580356089786328, 8.332800968292465527, 0.000000000000000000 ) ) ;
#22337 = CARTESIAN_POINT ( 'NONE',  ( -3.024877669624710386, 6.543124691288523920, 0.000000000000000000 ) ) ;
#22338 = CARTESIAN_POINT ( 'NONE',  ( -6.622231685632140596, 6.690634819517756959, 0.000000000000000000 ) ) ;
#22339 = CARTESIAN_POINT ( 'NONE',  ( 4.711248855110969913, 1.761570823303935551, -1.180294879073326308 ) ) ;
#22341 = DIRECTION ( 'NONE',  ( 0.000000000000000000, -1.000000000000000000, -0.000000000000000000 ) ) ;
#22340 = CARTESIAN_POINT ( 'NONE',  ( -0.1294898018152200736, 7.629137130509059617, -2.526516153123930852 ) ) ;
#22342 = B_SPLINE_CURVE_WITH_KNOTS ( 'NONE', 3,
 ( #145167, #146221, #30319, #164573, #194938, #47654 ),
 .UNSPECIFIED., .F., .F.,
 ( 4, 2, 4 ),
 ( 7.273049277091636640E-18, 9.878339706010669664E-05, 0.0001975667941202061020 ),
 .UNSPECIFIED. ) ;
#22343 = CARTESIAN_POINT ( 'NONE',  ( 5.887953105907347329, -0.8888255776743571035, 1.759709591642463433 ) ) ;
#22344 = CARTESIAN_POINT ( 'NONE',  ( -0.6823417656250212460, 1.801041667008083991, 1.181850606188755259 ) ) ;
#22346 = CARTESIAN_POINT ( 'NONE',  ( 0.6154903249990024694, 1.648289601840571938, 1.155678142064648917 ) ) ;
#22345 = AXIS2_PLACEMENT_3D ( 'NONE', #96853, #63254, #82693 ) ;
#22347 = VERTEX_POINT ( 'NONE', #213006 ) ;
#22348 = CARTESIAN_POINT ( 'NONE',  ( 6.315624676198635434, -1.384492656466195681, -1.602007840318976584 ) ) ;
#22349 = CARTESIAN_POINT ( 'NONE',  ( 10.88471284811786077, 8.294291839072673866, 4.944671277826161671 ) ) ;
#22350 = CARTESIAN_POINT ( 'NONE',  ( 2.031770498437397876, 1.981864486777328294, -0.5989037013024376410 ) ) ;
#22351 = ORIENTED_EDGE ( 'NONE', *, *, #175516, .F. ) ;
#22352 = CARTESIAN_POINT ( 'NONE',  ( 4.016958651398847557, 7.908478536599129249, -0.7998128361456362523 ) ) ;
#22353 = CARTESIAN_POINT ( 'NONE',  ( 6.073126464278658432, 6.050012061272033392, 0.000000000000000000 ) ) ;
#22354 = ORIENTED_EDGE ( 'NONE', *, *, #23613, .T. ) ;
#22356 = CARTESIAN_POINT ( 'NONE',  ( 5.681030059326015014, 6.586622143090519188, -1.199719254218445830 ) ) ;
#22355 = CARTESIAN_POINT ( 'NONE',  ( 4.470703160837229184, 0.0002547659985942945528, -2.090823719324691687 ) ) ;
#22359 = ORIENTED_EDGE ( 'NONE', *, *, #121776, .T. ) ;
#22358 = CARTESIAN_POINT ( 'NONE',  ( 1.699580558467077118, 1.249458034614457702, 1.311817296177042902 ) ) ;
#22357 = CARTESIAN_POINT ( 'NONE',  ( 3.645350208285046634, -1.381898811119431691, -1.193016960613018096 ) ) ;
#22360 = CARTESIAN_POINT ( 'NONE',  ( 6.727182134110200273, -0.004969159814478123736, 2.189081792362323586 ) ) ;
#22361 = DIRECTION ( 'NONE',  ( 0.000000000000000000, 0.000000000000000000, -1.000000000000000000 ) ) ;
#22362 = CARTESIAN_POINT ( 'NONE',  ( 3.733602637680955905, -2.039903990487581087, 0.8422819887162477093 ) ) ;
#22363 = CARTESIAN_POINT ( 'NONE',  ( 6.435316467980822353, 10.65961964595298817, 1.040834085586084257E-14 ) ) ;
#22364 = CARTESIAN_POINT ( 'NONE',  ( -1.364683531250010740, 8.692708333674730170, 0.7879004041258445001 ) ) ;
#22365 = CARTESIAN_POINT ( 'NONE',  ( 2.684119430630255820, 1.024705199231435993, 1.614373862881289590 ) ) ;
#22366 = CARTESIAN_POINT ( 'NONE',  ( 7.248805684800777804, 11.60869039890961218, 1.040834085586084257E-14 ) ) ;
#22367 = CARTESIAN_POINT ( 'NONE',  ( 6.197728532230423859, -1.496850047335227085, -1.430563974149069661 ) ) ;
#22368 = AXIS2_PLACEMENT_3D ( 'NONE', #58863, #26351, #159565 ) ;
#22369 = CARTESIAN_POINT ( 'NONE',  ( 1.360316468749957597, 0.3177083336747154596, -0.7853790794158961308 ) ) ;
#22370 = CARTESIAN_POINT ( 'NONE',  ( 5.636325218313963603, 0.4264374063192889475, 2.149501299143250055 ) ) ;
#22371 = CARTESIAN_POINT ( 'NONE',  ( 5.620636616140949116, 7.477306742562066511, -1.332712173395997013 ) ) ;
#22372 = CARTESIAN_POINT ( 'NONE',  ( -7.116787994678793972, 15.51980677385493124, -9.672274627470516251 ) ) ;
#22373 = ORIENTED_EDGE ( 'NONE', *, *, #119838, .T. ) ;
#22374 = EDGE_LOOP ( 'NONE', ( #47204, #11456 ) ) ;
#22375 = ADVANCED_FACE ( 'NONE', ( #32146 ), #182852, .F. ) ;
#22376 = PLANE ( 'NONE',  #58063 ) ;
#22377 = CARTESIAN_POINT ( 'NONE',  ( 4.112460492241882370, 1.324567223757302514, -1.321038939096484066 ) ) ;
#22378 = CARTESIAN_POINT ( 'NONE',  ( 1.642778471875001811, -1.480208332855375453, 2.845375778867859751 ) ) ;
#22379 = FACE_OUTER_BOUND ( 'NONE', #81214, .T. ) ;
#22380 = B_SPLINE_CURVE_WITH_KNOTS ( 'NONE', 3,
 ( #117514, #18860, #84945, #186704, #152090, #102260, #118577 ),
 .UNSPECIFIED., .F., .F.,
 ( 4, 3, 4 ),
 ( 0.0001932293135873427547, 0.0009000000018422016053, 0.002089330742406778334 ),
 .UNSPECIFIED. ) ;
#22381 = CARTESIAN_POINT ( 'NONE',  ( -6.860062538834774237, 10.94723069537516302, 0.7216878364870458196 ) ) ;
#22382 = CARTESIAN_POINT ( 'NONE',  ( 5.110497557708379546, 4.926945003606695295, -0.7998128361456481317 ) ) ;
#22383 = CARTESIAN_POINT ( 'NONE',  ( 0.2507523796677147421, -0.4231762011769435450, -1.930160340004604569 ) ) ;
#22385 = CARTESIAN_POINT ( 'NONE',  ( 0.6500178175347063325, 0.9963223104369984817, 1.753020061881370051 ) ) ;
#22384 = B_SPLINE_CURVE_WITH_KNOTS ( 'NONE', 3,
 ( #114443, #33121, #133855, #199865, #16843, #82925, #148998, #205192 ),
 .UNSPECIFIED., .F., .F.,
 ( 4, 2, 2, 4 ),
 ( 1.138412281109825108E-18, 0.0002224730689913802315, 0.0004449461379827593247, 0.0008898922759655175652 ),
 .UNSPECIFIED. ) ;
#22386 = CARTESIAN_POINT ( 'NONE',  ( -10.30827686509187835, 10.92074451889568643, 1.040834085586084257E-14 ) ) ;
#22387 = CARTESIAN_POINT ( 'NONE',  ( 5.494797395288433250, 9.632623737803665875, 0.000000000000000000 ) ) ;
#22388 = CARTESIAN_POINT ( 'NONE',  ( 1.254151665356119549, 0.8908215700371600043, 2.002402562943622844 ) ) ;
#22389 = CARTESIAN_POINT ( 'NONE',  ( 4.652862234063231739, -1.464609733205827879, 1.089778014065109657 ) ) ;
#22390 = CARTESIAN_POINT ( 'NONE',  ( -3.978428010606240850, 6.728917548094202949, -1.199719254218452047 ) ) ;
#22391 = AXIS2_PLACEMENT_3D ( 'NONE', #142876, #208878, #107202 ) ;
#22392 = CARTESIAN_POINT ( 'NONE',  ( 4.556949027968946631, 8.330541276023501140, -0.7216878364870357165 ) ) ;
#22393 = CARTESIAN_POINT ( 'NONE',  ( 3.267151830768944443, 4.834763107362302748, -1.443375672974058777 ) ) ;
#22394 = ADVANCED_FACE ( 'NONE', ( #194639 ), #162160, .F. ) ;
#22395 = CARTESIAN_POINT ( 'NONE',  ( -6.143779885648060102, 7.196773283791382703, 1.199719254218452047 ) ) ;
#22396 = CARTESIAN_POINT ( 'NONE',  ( 4.487912541323413329, 5.194651705420806564, 1.199719254218462483 ) ) ;
#22397 = CARTESIAN_POINT ( 'NONE',  ( 3.715816618597135523, 6.492813934075403637, -1.199719254218453823 ) ) ;
#22398 = ORIENTED_EDGE ( 'NONE', *, *, #188204, .F. ) ;
#22400 = CARTESIAN_POINT ( 'NONE',  ( 0.04752084976851479736, -1.839644132637440865, 0.8178810061007844023 ) ) ;
#22399 = CARTESIAN_POINT ( 'NONE',  ( 3.245484093776138668, 1.841430844176932480, -0.003062914905635482320 ) ) ;
#22401 = CARTESIAN_POINT ( 'NONE',  ( 1.634533438177967923, 0.1689203749893586071, -2.292248917674902575 ) ) ;
#22403 = CARTESIAN_POINT ( 'NONE',  ( 0.2857036466711966316, -1.138303949996006148, -1.472634861895638636 ) ) ;
#22402 = CARTESIAN_POINT ( 'NONE',  ( 4.690757960648231695, 5.535267711253469614, 1.082531754730560403 ) ) ;
#22404 = CARTESIAN_POINT ( 'NONE',  ( -3.795392936821753604, 6.515376628678959392, -1.199719254218452047 ) ) ;
#22405 = CARTESIAN_POINT ( 'NONE',  ( -5.731716152730447433, 6.325271568888634732, -0.8228651010004313093 ) ) ;
#22406 = CARTESIAN_POINT ( 'NONE',  ( 3.199369407753744454, 1.726971514772487559, -0.8218122705464236954 ) ) ;
#22407 = CARTESIAN_POINT ( 'NONE',  ( -8.947491310014823895, 12.52615806407091803, 1.199719254218462483 ) ) ;
#22408 = CARTESIAN_POINT ( 'NONE',  ( 6.426609430950597890, 6.789993649951097332, 0.4362094596595481599 ) ) ;
#22409 = CARTESIAN_POINT ( 'NONE',  ( -7.322812365156824654, 8.676274193172000437, 1.082531754730549078 ) ) ;
#22411 = CARTESIAN_POINT ( 'NONE',  ( 1.375632740723360836, 1.111493989511678881, 1.504490780774490499 ) ) ;
#22410 = CARTESIAN_POINT ( 'NONE',  ( 2.683241491500857556, 1.480437668936212869, 1.476589516890645104 ) ) ;
#22412 = CARTESIAN_POINT ( 'NONE',  ( 2.477888549845189470, 1.799646572043178683, 0.9090068759892779848 ) ) ;
#22413 = CARTESIAN_POINT ( 'NONE',  ( 7.456621297836061757, 11.64321591421002644, 0.7216878364870438212 ) ) ;
#22414 = CARTESIAN_POINT ( 'NONE',  ( -1.201851678989727383E-14, 3.759375000341423245, -1.575800808251660134 ) ) ;
#22415 = CARTESIAN_POINT ( 'NONE',  ( 3.509068237933731016, -1.713987098263862086, 0.3013083454645076875 ) ) ;
#22416 = CARTESIAN_POINT ( 'NONE',  ( 4.147904930777053245, 6.926640621626830807, -1.199719254218452047 ) ) ;
#22417 = CARTESIAN_POINT ( 'NONE',  ( -6.784185045882110465, -8.038658175288270868, 6.650326532587137685 ) ) ;
#22418 = CARTESIAN_POINT ( 'NONE',  ( 3.861678741103656165, 1.711552447172806968, -0.2133835738165473228 ) ) ;
#22419 = CARTESIAN_POINT ( 'NONE',  ( 3.948915171154475878, -1.822730400009948237, -1.216494452853926322 ) ) ;
#22420 = CARTESIAN_POINT ( 'NONE',  ( 4.705825944637973990, -0.5905853116198942487, 2.126329296355852883 ) ) ;
#22421 = CARTESIAN_POINT ( 'NONE',  ( -11.60136562008509387, 4.149718911762417584, -5.313756115068398067 ) ) ;
#22422 = CARTESIAN_POINT ( 'NONE',  ( 4.135715461124009451, 2.046248213957535089, -0.7259774245699932571 ) ) ;
#22423 = CARTESIAN_POINT ( 'NONE',  ( 2.648829494986388422, -1.517897411861212076, 1.014145048410304284 ) ) ;
#22424 = DIRECTION ( 'NONE',  ( -0.6507913734559642727, -0.7592566023653003482, -2.775557561562895049E-17 ) ) ;
#22425 = CARTESIAN_POINT ( 'NONE',  ( 4.645784029343587918, 2.093824292288968270, -0.3141051717527267861 ) ) ;
#22426 = CARTESIAN_POINT ( 'NONE',  ( 6.639320575229255006, 4.696066290934245657, 2.559399261709224049 ) ) ;
#22427 = VERTEX_POINT ( 'NONE', #177338 ) ;
#22429 = CARTESIAN_POINT ( 'NONE',  ( 1.364683531249988535, 2.176041667008087543, 0.7879004041258500513 ) ) ;
#22428 = CARTESIAN_POINT ( 'NONE',  ( 4.669621734427405357, 1.318897967798425608, 1.874777261101326920 ) ) ;
#22430 = CARTESIAN_POINT ( 'NONE',  ( 6.720655732516647163, 0.6055996050860124047, 1.780393570709505546 ) ) ;
#22431 = CARTESIAN_POINT ( 'NONE',  ( 10.05353459973327368, 11.68787744023238417, -1.199719254218440723 ) ) ;
#22432 = CARTESIAN_POINT ( 'NONE',  ( 0.7684181764250408442, 2.117871390293009526, -0.1079879263860619443 ) ) ;
#22433 = CARTESIAN_POINT ( 'NONE',  ( -5.260200412422208593, 7.159986452624450770, -1.443375672974053447 ) ) ;
#22434 = CARTESIAN_POINT ( 'NONE',  ( 4.216222584169931231, 4.021273891060765493, 1.214306433183764966E-14 ) ) ;
#22435 = CARTESIAN_POINT ( 'NONE',  ( -5.300874872818844175, 7.207439989753867238, 1.443375672974064550 ) ) ;
#22436 = CARTESIAN_POINT ( 'NONE',  ( 6.883263157960404222, 3.695221384915627905, 2.468000959490519897 ) ) ;
#22437 = ORIENTED_EDGE ( 'NONE', *, *, #152281, .F. ) ;
#22438 = CARTESIAN_POINT ( 'NONE',  ( 5.748672702226536479, 1.986101125435947301, -0.3474646712962395911 ) ) ;
#22440 = CARTESIAN_POINT ( 'NONE',  ( 3.625881544801349055, 2.013384979781565942, -0.4471371585693607598 ) ) ;
#22439 = CARTESIAN_POINT ( 'NONE',  ( 4.961394147597008697, 7.875711374583454827, -1.199719254218452047 ) ) ;
#22442 = CARTESIAN_POINT ( 'NONE',  ( -0.1408020194049912077, 0.6951682901239358836, -2.180991432481160341 ) ) ;
#22441 = CARTESIAN_POINT ( 'NONE',  ( -2.965583170617148046, 6.450339737514259930, -0.2656679274986517014 ) ) ;
#22443 = CARTESIAN_POINT ( 'NONE',  ( 5.027041095616958444, 9.086908054853605421, 0.000000000000000000 ) ) ;
#22444 = CARTESIAN_POINT ( 'NONE',  ( -3.285556943750000514, -1.538541666188708357, -1.896917185911906500 ) ) ;
#22445 = DIRECTION ( 'NONE',  ( -0.9629532593499512405, -0.2632023826131885680, 0.05869860385091355687 ) ) ;
#22446 = CARTESIAN_POINT ( 'NONE',  ( 5.753911783233988331, 0.8852683131516884130, 2.004867968450708915 ) ) ;
#22447 = CARTESIAN_POINT ( 'NONE',  ( 3.867814693791224112, -0.2004342644464084944, -2.006446243107910199 ) ) ;
#22448 = CARTESIAN_POINT ( 'NONE',  ( 3.473999211503727036, -1.775402473473717935, -0.4878004006634574230 ) ) ;
#22449 = EDGE_CURVE ( 'NONE', #86628, #54687, #193576, .T. ) ;
#22450 = CARTESIAN_POINT ( 'NONE',  ( 5.900823170445728572, 7.907379670318584353, 1.599625672291267398 ) ) ;
#22451 = PRESENTATION_STYLE_ASSIGNMENT (( #58180 ) ) ;
#22452 = CARTESIAN_POINT ( 'NONE',  ( 0.1996746939399509924, -1.724222465425511386, -0.05034706749046553159 ) ) ;
#22453 = CARTESIAN_POINT ( 'NONE',  ( -2.279742385392243165, 5.811449882932888222, -0.7998128361456281477 ) ) ;
#22454 = CARTESIAN_POINT ( 'NONE',  ( 1.407308937662318460, -1.282028150163934122, -1.907831638372993410 ) ) ;
#22455 = CARTESIAN_POINT ( 'NONE',  ( -6.039267359883488950, 9.133230122250985517, 1.199719254218452047 ) ) ;
#22456 = CARTESIAN_POINT ( 'NONE',  ( 0.2810632938833834693, -2.195003449849114663, -0.5476492663787374537 ) ) ;
#22457 = CARTESIAN_POINT ( 'NONE',  ( 2.684315897010148610, -1.081986827455215572, 1.806733699029156259 ) ) ;
#22458 = CARTESIAN_POINT ( 'NONE',  ( -4.098307573080856692, 8.003385611894792362, 0.7998128361456352531 ) ) ;
#22459 = CARTESIAN_POINT ( 'NONE',  ( 6.414979237560321401, 10.63589287712906462, 1.040834085586084257E-14 ) ) ;
#22460 = CARTESIAN_POINT ( 'NONE',  ( 5.139949632912227173, 8.050339434155988627, -1.082531754730548412 ) ) ;
#22461 = DIRECTION ( 'NONE',  ( 0.000000000000000000, 0.000000000000000000, 1.000000000000000000 ) ) ;
#22462 = CARTESIAN_POINT ( 'NONE',  ( -5.982172092127739482, 8.002286745614243912, -1.599625672291263179 ) ) ;
#22463 = CARTESIAN_POINT ( 'NONE',  ( 6.195713011320782115, 8.251417818006149929, -1.443375672974057666 ) ) ;
#22464 = CARTESIAN_POINT ( 'NONE',  ( 5.379472278790374595, 6.509029678566758292, 1.321781506194243727 ) ) ;
#22465 = CARTESIAN_POINT ( 'NONE',  ( -4.791917227426195858, 7.677988301050826969, -1.199719254218452047 ) ) ;
#22467 = CARTESIAN_POINT ( 'NONE',  ( 3.990652734535464319, -1.277060150153148221, 1.817470393784472948 ) ) ;
#22466 = CARTESIAN_POINT ( 'NONE',  ( 2.373420902723611725, -1.847293605357634982, -1.041186957106011723 ) ) ;
#22468 = CARTESIAN_POINT ( 'NONE',  ( 2.572451567087580493, -2.097416440861415321, -0.6350555677336400251 ) ) ;
#22469 = CARTESIAN_POINT ( 'NONE',  ( -6.738566041191992539, 7.820414121934134322, 1.199719254218450271 ) ) ;
#22470 = CARTESIAN_POINT ( 'NONE',  ( -6.120580001926503755, 6.105374521861167914, -0.7998128361456362523 ) ) ;
#22471 = CARTESIAN_POINT ( 'NONE',  ( 5.107842384611220865, 0.6171798735227496113, -1.862306164846748491 ) ) ;
#22472 = CARTESIAN_POINT ( 'NONE',  ( -1.364683531250014514, 1.488541667008084435, -0.7879004041258289570 ) ) ;
#22473 = CARTESIAN_POINT ( 'NONE',  ( -2.862179826260718762, 6.353310540697199471, 0.000000000000000000 ) ) ;
#22475 = ORIENTED_EDGE ( 'NONE', *, *, #17805, .F. ) ;
#22474 = CARTESIAN_POINT ( 'NONE',  ( -6.155038550924159857, 8.203964280876741455, 1.443375672974078761 ) ) ;
#22476 = CARTESIAN_POINT ( 'NONE',  ( 4.500305224345508393, -0.9970752094022590217, 1.871535012320741265 ) ) ;
#22477 = CARTESIAN_POINT ( 'NONE',  ( -5.320648938720212051, 5.172121614787156929, 0.000000000000000000 ) ) ;
#22478 = ORIENTED_EDGE ( 'NONE', *, *, #46917, .T. ) ;
#22479 = CARTESIAN_POINT ( 'NONE',  ( 5.805597153138060129, -0.5296426447994294628, 2.095691122003799478 ) ) ;
#22480 = CARTESIAN_POINT ( 'NONE',  ( 6.494519276145969577, 7.535692896047149425, -1.199719254218446718 ) ) ;
#22481 = CARTESIAN_POINT ( 'NONE',  ( 4.810013364240863787, 1.265987717737980134, -1.337210144835267345 ) ) ;
#22482 = CARTESIAN_POINT ( 'NONE',  ( -5.912409256564314930, 5.999956524776160371, -0.009440138123966573813 ) ) ;
#22483 = CARTESIAN_POINT ( 'NONE',  ( -1.364683531250000748, 1.071875000341421247, 0.000000000000000000 ) ) ;
#22484 = CARTESIAN_POINT ( 'NONE',  ( 0.1162408695623952659, -0.08860816971513819917, 1.738289989025374016 ) ) ;
#22485 = CARTESIAN_POINT ( 'NONE',  ( 6.727182134110243794, 2.977085856046020051, 2.364561739503980853 ) ) ;
#22486 = CARTESIAN_POINT ( 'NONE',  ( -0.08635228504281292072, 7.011029804986348424, 1.999717945518313611 ) ) ;
#22487 = CARTESIAN_POINT ( 'NONE',  ( 0.000000000000000000, 0.9200000000000041478, 0.000000000000000000 ) ) ;
#22488 = CARTESIAN_POINT ( 'NONE',  ( 3.766626874709140704, -1.453462046928340579, 1.600284095077113333 ) ) ;
#22489 = CARTESIAN_POINT ( 'NONE',  ( -5.135841261478327979, 4.886236314679810455, 0.7998128361456341429 ) ) ;
#22490 = CARTESIAN_POINT ( 'NONE',  ( -6.168596704093453731, 10.14052055484361325, 0.7216878364870458196 ) ) ;
#22491 = CARTESIAN_POINT ( 'NONE',  ( 3.116266767097406909, -1.064116542966097922, -1.881565754655416756 ) ) ;
#22492 = CARTESIAN_POINT ( 'NONE',  ( 4.710209360279286273, -0.8403073340159574744, -1.783404427212876842 ) ) ;
#22493 = CARTESIAN_POINT ( 'NONE',  ( 4.340949964944015527, -0.9985633389030469376, 1.417159075928013046 ) ) ;
#22494 = AXIS2_PLACEMENT_3D ( 'NONE', #123476, #201400, #90896 ) ;
#22495 = CARTESIAN_POINT ( 'NONE',  ( 1.171705676731093604, 1.309414992938146893, 1.757219779060022580 ) ) ;
#22496 = CARTESIAN_POINT ( 'NONE',  ( 1.501454852758288494, 1.885366349659310048, -1.330307493247370410 ) ) ;
#22497 = CARTESIAN_POINT ( 'NONE',  ( 4.007146649590315413, 1.765602988722612565, 1.062546815679512369 ) ) ;
#22498 = CARTESIAN_POINT ( 'NONE',  ( 6.022988683830415191, -1.827201308531730017, 0.6583088893449047241 ) ) ;
#22501 = VERTEX_POINT ( 'NONE', #93976 ) ;
#22500 = EDGE_CURVE ( 'NONE', #11347, #121606, #103548, .T. ) ;
#22499 = CARTESIAN_POINT ( 'NONE',  ( -7.117667457050096402, 10.28740055232499984, 1.082531754730549967 ) ) ;
#22502 = CARTESIAN_POINT ( 'NONE',  ( -5.061990249855848667, 6.999017606288844284, -1.599625672291271394 ) ) ;
#22503 = DIRECTION ( 'NONE',  ( 0.04888523518676873847, 0.000000000000000000, 0.9988044021632734859 ) ) ;
#22505 = ORIENTED_EDGE ( 'NONE', *, *, #49103, .F. ) ;
#22504 = CARTESIAN_POINT ( 'NONE',  ( 1.423015351387224570E-15, 0.9706168436483911810, -11.90408086427858692 ) ) ;
#22506 = CARTESIAN_POINT ( 'NONE',  ( -6.629573926958124197, 9.717958100551031819, 1.082531754730548412 ) ) ;
#22507 = CARTESIAN_POINT ( 'NONE',  ( 3.364504783244476993, 0.9904720576699842516, 1.972067388187691339 ) ) ;
#22508 = CARTESIAN_POINT ( 'NONE',  ( -3.285556943750000070, -4.046874999522040106, 0.000000000000000000 ) ) ;
#22509 = ORIENTED_EDGE ( 'NONE', *, *, #110743, .F. ) ;
#22510 = CARTESIAN_POINT ( 'NONE',  ( 0.6196752394443981737, 1.841814893205738102, -0.2651871859581377833 ) ) ;
#22511 = CARTESIAN_POINT ( 'NONE',  ( -0.1290005225502433017, 7.629137130509076492, -2.773995091683974401 ) ) ;
#22512 = FACE_OUTER_BOUND ( 'NONE', #134740, .T. ) ;
#22513 = CARTESIAN_POINT ( 'NONE',  ( -9.492905263954453332, -8.233136995002796610, 0.3773006915670363282 ) ) ;
#22514 = CARTESIAN_POINT ( 'NONE',  ( 6.825078400183554272, 2.951006455646578264, 2.596623860847916188 ) ) ;
#22515 = CARTESIAN_POINT ( 'NONE',  ( 6.333933918656591722, 1.821832875601756774, 0.2651207078676054429 ) ) ;
#22516 = VERTEX_POINT ( 'NONE', #79820 ) ;
#22517 = CARTESIAN_POINT ( 'NONE',  ( 2.430605206563386300, 1.998658846558550195, 0.5020661504441750189 ) ) ;
#22518 = CARTESIAN_POINT ( 'NONE',  ( 0.6801582343749900117, 0.05729166700808169255, -1.178068619123848526 ) ) ;
#22519 = EDGE_CURVE ( 'NONE', #101381, #30345, #145932, .T. ) ;
#22520 = CARTESIAN_POINT ( 'NONE',  ( -5.994676475536691029, 10.14553965476814845, 0.7998128361456481317 ) ) ;
#22521 = PRESENTATION_STYLE_ASSIGNMENT (( #170924 ) ) ;
#22522 = PRESENTATION_STYLE_ASSIGNMENT (( #70201 ) ) ;
#22523 = CARTESIAN_POINT ( 'NONE',  ( 3.337278367258157630, 7.045241861776501580, 0.7998128361456341429 ) ) ;
#22524 = CARTESIAN_POINT ( 'NONE',  ( 0.8485939591743509869, 0.5976917523492016882, 1.972322469454860672 ) ) ;
#22526 = CARTESIAN_POINT ( 'NONE',  ( -0.6823417656250003738, 13.15104166700806232, 1.181850606188754593 ) ) ;
#22525 = CARTESIAN_POINT ( 'NONE',  ( -3.449547071718257030, 5.999999999999998224, 2.025000000000002576 ) ) ;
#22527 = CARTESIAN_POINT ( 'NONE',  ( 6.817052309572890323, 6.847649204123507083, 0.7998128361456341429 ) ) ;
#22528 = CARTESIAN_POINT ( 'NONE',  ( -5.173318132066234476, 8.193232366456022930, -1.199719254218453823 ) ) ;
#22529 = CARTESIAN_POINT ( 'NONE',  ( 5.345219749365309525, 4.708221922860561293, 2.500000000000000444 ) ) ;
#22530 = CIRCLE ( 'NONE', #29372, 9.479622692290801567 ) ;
#22531 = CARTESIAN_POINT ( 'NONE',  ( 6.094375512030342001, -2.195847865938059140, -0.2203403561373064590 ) ) ;
#22532 = CARTESIAN_POINT ( 'NONE',  ( 6.907534427287327361, -0.5096537312613695914, 2.212693016512882416 ) ) ;
#22533 = CARTESIAN_POINT ( 'NONE',  ( -5.938108093105513241, 6.030140318152288792, 0.7216878364870317197 ) ) ;
#22534 = CARTESIAN_POINT ( 'NONE',  ( 0.5098338327763075606, -0.6861045072398126443, 1.785269576063217567 ) ) ;
#22535 = CARTESIAN_POINT ( 'NONE',  ( 0.7082206942033396624, 1.197301205363930254, -1.622488844446705381 ) ) ;
#22536 = EDGE_CURVE ( 'NONE', #22857, #53554, #210687, .T. ) ;
#22537 = CARTESIAN_POINT ( 'NONE',  ( 6.278834536460164983, 9.379038488295265097, -1.082531754730548412 ) ) ;
#22538 = CARTESIAN_POINT ( 'NONE',  ( 9.355700869302610911, 13.88187516316259895, -7.515225910968625023 ) ) ;
#22539 = CARTESIAN_POINT ( 'NONE',  ( 1.500000000000001332, 12.15625000068279427, 0.000000000000000000 ) ) ;
#22540 = CARTESIAN_POINT ( 'NONE',  ( 7.752014238602739730E-16, 0.03624871340549007392, 6.329999999999995630 ) ) ;
#22541 = ADVANCED_FACE ( 'NONE', ( #132874 ), #53679, .F. ) ;
#22542 = CARTESIAN_POINT ( 'NONE',  ( 1.445950363956361340, 1.868363765441739099, 0.09516058986362013750 ) ) ;
#22543 = VECTOR ( 'NONE', #24749, 1000.000000000000000 ) ;
#22544 = CARTESIAN_POINT ( 'NONE',  ( 2.800017839408690090, -0.9981255096969069429, -1.752139039461996006 ) ) ;
#22546 = DIRECTION ( 'NONE',  ( -1.000000000000000000, 7.109522442527899011E-16, 0.000000000000000000 ) ) ;
#22545 = CARTESIAN_POINT ( 'NONE',  ( -0.6823417656250246877, 0.5510416670080897639, 1.181850606188755259 ) ) ;
#22548 = CARTESIAN_POINT ( 'NONE',  ( 5.356126594405285601, 2.103725632816171309, -0.1020696835895683885 ) ) ;
#22547 = CARTESIAN_POINT ( 'NONE',  ( -8.474009703741204547, 9.845098394908269768, -1.199719254218446718 ) ) ;
#22549 = CARTESIAN_POINT ( 'NONE',  ( 6.747154001095143627, 11.02343010125301959, -0.7998128361456291469 ) ) ;
#22551 = CARTESIAN_POINT ( 'NONE',  ( -6.877010230629689858, 9.046264573866535486, 1.599625672291283607 ) ) ;
#22550 = CARTESIAN_POINT ( 'NONE',  ( 3.223806664999388172, 6.983134552466421674, -0.7998128361456362523 ) ) ;
#22552 = CARTESIAN_POINT ( 'NONE',  ( -0.01083140255525823388, -7.162053774861992572, -9.500385102287555839 ) ) ;
#22553 = CARTESIAN_POINT ( 'NONE',  ( 4.359631895039292715, -1.563893385546542003, -1.278231166955777764 ) ) ;
#22554 = CARTESIAN_POINT ( 'NONE',  ( 0.6823417656249899377, 5.176041667008086655, -1.181850606188754593 ) ) ;
#22555 = AXIS2_PLACEMENT_3D ( 'NONE', #16558, #149795, #183345 ) ;
#22556 = CARTESIAN_POINT ( 'NONE',  ( 5.951645758832087907, 1.559603009536973284, 1.349993227703372156 ) ) ;
#22557 = CARTESIAN_POINT ( 'NONE',  ( 9.734391104931951588, 11.41950637958454706, 1.082531754730548412 ) ) ;
#22558 = CARTESIAN_POINT ( 'NONE',  ( 6.063787883973515314, 2.130759124531961923, -0.3628933549372145295 ) ) ;
#22559 = CARTESIAN_POINT ( 'NONE',  ( 6.119526231721748033, 8.232809585132461194, 1.599625672291269396 ) ) ;
#22560 = CARTESIAN_POINT ( 'NONE',  ( 1.364683531249988757, -0.8031249996585804185, 0.000000000000000000 ) ) ;
#22562 = FILL_AREA_STYLE_COLOUR ( '', #27621 ) ;
#22561 = CARTESIAN_POINT ( 'NONE',  ( 4.369470645354133431, 8.319742529546998000, 0.7998128361456271485 ) ) ;
#22563 = CARTESIAN_POINT ( 'NONE',  ( 7.578644679914713578, 8.904468883731073703, 1.082531754730558626 ) ) ;
#22565 = CARTESIAN_POINT ( 'NONE',  ( -2.300257893000399623, 2.674526321726193867, -2.456405337815161793 ) ) ;
#22564 = CARTESIAN_POINT ( 'NONE',  ( 1.592468369012179918, 1.070935286220242366, -1.888628467986789738 ) ) ;
#22567 = CARTESIAN_POINT ( 'NONE',  ( 2.208333698829296310, 1.645431377724184463, 0.8263914577605266931 ) ) ;
#22566 = CARTESIAN_POINT ( 'NONE',  ( -6.290620087060847965, 7.401773525401500464, 1.082531754730549967 ) ) ;
#22568 = CARTESIAN_POINT ( 'NONE',  ( -1.364683531250012516, 2.738541667008090208, -0.7879004041258289570 ) ) ;
#22569 = CARTESIAN_POINT ( 'NONE',  ( 2.859115728684503477, 0.3189004193784421015, -2.168101852914063876 ) ) ;
#22570 = CARTESIAN_POINT ( 'NONE',  ( 6.983263157960362122, 2.430545403621493072, 2.435370848939223620 ) ) ;
#22571 = CARTESIAN_POINT ( 'NONE',  ( 3.520660345214459586, 1.437014610000959314, -1.747548891452437081 ) ) ;
#22572 = CARTESIAN_POINT ( 'NONE',  ( -5.018489415352746619, 9.006654751220198207, 0.7998128361456481317 ) ) ;
#22573 = CARTESIAN_POINT ( 'NONE',  ( -11.84668730067608600, 10.19999999999998153, 1.399999999999998579 ) ) ;
#22574 = CARTESIAN_POINT ( 'NONE',  ( 6.457572779797339457, 6.769951385671206801, 0.3193968722623799494 ) ) ;
#22575 = CARTESIAN_POINT ( 'NONE',  ( -1.402160292154681736E-14, 14.31250000000000355, 1.732050807568881190 ) ) ;
#22576 = CARTESIAN_POINT ( 'NONE',  ( 4.746763178560241769, 8.551991118380046331, 0.7216878364870328300 ) ) ;
#22577 = CARTESIAN_POINT ( 'NONE',  ( 5.378098658424382172, -0.9825891054615911724, 1.471664417823245197 ) ) ;
#22578 = CARTESIAN_POINT ( 'NONE',  ( 9.284636267260101050, 9.726497154758602548, -0.7998128361456281477 ) ) ;
#22579 = CARTESIAN_POINT ( 'NONE',  ( 1.501149451381103672, 1.721883814275385616, -1.212229816669802895 ) ) ;
#22581 = CARTESIAN_POINT ( 'NONE',  ( -0.7500000000000215383, 2.441666666666689078, 1.299038105676671107 ) ) ;
#22580 = CARTESIAN_POINT ( 'NONE',  ( 1.364683531249997417, 11.23437500034139802, 2.602085213965210642E-15 ) ) ;
#22582 = CARTESIAN_POINT ( 'NONE',  ( 1.398812336859527550, 0.3809602064741451355, 1.932172009363951837 ) ) ;
#22583 = CARTESIAN_POINT ( 'NONE',  ( -2.959422669532919326, 6.674686557755516780, 0.7998128361456352531 ) ) ;
#22584 = CARTESIAN_POINT ( 'NONE',  ( -0.7499999999999972244, 5.389583334016151639, -1.299038105676652899 ) ) ;
#22586 = ORIENTED_EDGE ( 'NONE', *, *, #169387, .F. ) ;
#22585 = CARTESIAN_POINT ( 'NONE',  ( 6.310821775929002619, -0.4926439853468951857, -1.743236492463080767 ) ) ;
#22587 = CARTESIAN_POINT ( 'NONE',  ( 5.938108093105483931, 8.911247961056314892, -1.082531754730537088 ) ) ;
#22588 = CARTESIAN_POINT ( 'NONE',  ( -1.364683531250014514, -0.4072916663252447167, 0.7879004041258379498 ) ) ;
#22589 = CARTESIAN_POINT ( 'NONE',  ( 4.469519713540137218, 1.814478506493341969, -0.4545110902946307152 ) ) ;
#22590 = CARTESIAN_POINT ( 'NONE',  ( 3.460355519985863548, 5.060167411448709629, 1.599625672291267398 ) ) ;
#22591 = ORIENTED_EDGE ( 'NONE', *, *, #42234, .F. ) ;
#22592 = CARTESIAN_POINT ( 'NONE',  ( 5.805552407531882508, -1.628464769346991581, -1.278160613847306504 ) ) ;
#22593 = CARTESIAN_POINT ( 'NONE',  ( 0.6125000000000071498, 1.583333333333325488, 1.060881119635915359 ) ) ;
#22594 = CARTESIAN_POINT ( 'NONE',  ( -4.462041952228942954, 8.219816354326809460, -0.7216878364870338292 ) ) ;
#22595 = CARTESIAN_POINT ( 'NONE',  ( 0.1509401653462701109, -0.4529219869476922011, -2.027634260368789576 ) ) ;
#22596 = CARTESIAN_POINT ( 'NONE',  ( -1.500000000000001332, -0.5999999999999755529, 0.000000000000000000 ) ) ;
#22597 = CARTESIAN_POINT ( 'NONE',  ( 7.344766530301147789, 9.591980256816594164, 1.599625672291281386 ) ) ;
#22598 = CARTESIAN_POINT ( 'NONE',  ( -10.15235809853472126, 10.73883929124566983, -0.7998128361456291469 ) ) ;
#22599 = CARTESIAN_POINT ( 'NONE',  ( 6.855582950365507244, 8.027210192628430718, -1.199719254218452047 ) ) ;
#22600 = CARTESIAN_POINT ( 'NONE',  ( 1.364683531249988757, 0.3843750003414206362, 0.000000000000000000 ) ) ;
#22601 = CARTESIAN_POINT ( 'NONE',  ( 1.499999999999987121, 0.7541666666666868579, 0.8660254037844524744 ) ) ;
#22603 = CARTESIAN_POINT ( 'NONE',  ( 6.335737856287750880, 6.286115675290828264, -0.7998128361456281477 ) ) ;
#22602 = CARTESIAN_POINT ( 'NONE',  ( 4.598074495912658044, 0.8407358649686399454, -1.772743347989129692 ) ) ;
#22604 = CARTESIAN_POINT ( 'NONE',  ( 2.196638537759632470, -1.314794530490107638, -1.528507974810841219 ) ) ;
#22605 = DIRECTION ( 'NONE',  ( 0.000000000000000000, -1.000000000000000000, 0.000000000000000000 ) ) ;
#22606 = CARTESIAN_POINT ( 'NONE',  ( 0.3631484714031462668, 0.2087870660046411420, -2.181583536649676525 ) ) ;
#22607 = CARTESIAN_POINT ( 'NONE',  ( -11.89839339040395139, 9.771225315960876401, 1.560885614203548100 ) ) ;
#22608 = CARTESIAN_POINT ( 'NONE',  ( 2.073319367481298858, 1.791407343212477077, -0.5384048943791116537 ) ) ;
#22609 = CARTESIAN_POINT ( 'NONE',  ( -1.364683531250010295, 5.280208333674758059, 0.7879004041258379498 ) ) ;
#22610 = CARTESIAN_POINT ( 'NONE',  ( 3.691655806294301900, 1.894216563707728396, -0.6821535943304660732 ) ) ;
#22611 = CARTESIAN_POINT ( 'NONE',  ( -7.320512876374914768, 10.62801655815766999, 1.199719254218453823 ) ) ;
#22613 = CARTESIAN_POINT ( 'NONE',  ( 3.286815299386883549, 1.667571603535710434, -1.304429798788673267 ) ) ;
#22612 = CARTESIAN_POINT ( 'NONE',  ( -5.178851490740209229, 7.065079377328788546, 1.443375672974064550 ) ) ;
#22614 = CARTESIAN_POINT ( 'NONE',  ( -4.094259397040477033, 3.811769539471001167, -2.445515378722424860 ) ) ;
#22615 = CARTESIAN_POINT ( 'NONE',  ( 6.426242046702522082, 1.060841730010402495, 1.777776562702712226 ) ) ;
#22617 = CARTESIAN_POINT ( 'NONE',  ( 6.720655732516626735, 6.034942950145537388, 2.668627893128409756 ) ) ;
#22616 = CARTESIAN_POINT ( 'NONE',  ( 0.7321124197560413549, 2.060462595713075995, 0.3535659584654736731 ) ) ;
#22619 = ORIENTED_EDGE ( 'NONE', *, *, #182631, .T. ) ;
#22618 = CARTESIAN_POINT ( 'NONE',  ( 6.739283625173963621, -1.628968703954777553, 0.8242606506234579911 ) ) ;
#22620 = CARTESIAN_POINT ( 'NONE',  ( 8.288111976655649471, 8.563885482386732306, -0.7998128361456291469 ) ) ;
#22621 = CARTESIAN_POINT ( 'NONE',  ( 7.952857047017175773, -6.836289462023034780, -7.401194801147395808 ) ) ;
#22622 = CARTESIAN_POINT ( 'NONE',  ( -10.81659190237994395, 5.544392656652913587, 6.534142543513654644 ) ) ;
#22624 =( BOUNDED_SURFACE ( )  B_SPLINE_SURFACE ( 3, 2, ( 
 ( #113739, #35600, #18276 ),
 ( #946, #69149, #97438 ),
 ( #67011, #133147, #199149 ),
 ( #50794, #15076, #31362 ),
 ( #84358, #182922, #34537 ),
 ( #101676, #3079, #47629 ),
 ( #167746, #100608, #19346 ),
 ( #81166, #131054, #170939 ),
 ( #73436, #135268, #156851 ),
 ( #139539, #86495, #203415 ) ),
 .UNSPECIFIED., .F., .F., .F. ) 
 B_SPLINE_SURFACE_WITH_KNOTS ( ( 4, 2, 2, 2, 4 ),
 ( 3, 3 ),
 ( 0.001823043507466968506, 0.002278804384346605483, 0.002734565261226242026, 0.003190326138105878569, 0.003646087014985515545 ),
 ( 0.000000000000000000, 1.000000000000000000 ),
 .UNSPECIFIED. ) 
 GEOMETRIC_REPRESENTATION_ITEM ( )  RATIONAL_B_SPLINE_SURFACE ( (
 ( 1.000000000000000000, 0.8267197332287864464, 1.000000000000000000),
 ( 1.000000000000000000, 0.8323584916099276976, 1.000000000000000000),
 ( 1.000000000000000000, 0.8280586474256576013, 1.000000000000000000),
 ( 1.000000000000000000, 0.7975649039268305485, 1.000000000000000000),
 ( 1.000000000000000000, 0.7708027761888249785, 1.000000000000000000),
 ( 1.000000000000000000, 0.7027005163579342906, 1.000000000000000000),
 ( 1.000000000000000000, 0.6615630608851112981, 1.000000000000000000),
 ( 1.000000000000000000, 0.5955151780456100497, 1.000000000000000000),
 ( 1.000000000000000000, 0.5705924789361177529, 1.000000000000000000),
 ( 1.000000000000000000, 0.5626093260850774103, 1.000000000000000000) ) ) 
 REPRESENTATION_ITEM ( '' )  SURFACE ( )  );
#22623 = CARTESIAN_POINT ( 'NONE',  ( -1.364683531250010740, 12.69270833367473550, 0.7879004041258445001 ) ) ;
#22625 = CARTESIAN_POINT ( 'NONE',  ( 6.410809557875646547, -0.5148348048229570706, -1.841598127471068658 ) ) ;
#22626 = CARTESIAN_POINT ( 'NONE',  ( -7.426115451983156923, 9.686887332112256388, -1.599625672291263179 ) ) ;
#22627 = CARTESIAN_POINT ( 'NONE',  ( 4.710568305744190276, 7.583081225755162968, 1.199719254218462483 ) ) ;
#22628 = FACE_OUTER_BOUND ( 'NONE', #194163, .T. ) ;
#22629 = DIRECTION ( 'NONE',  ( 0.6507913734559651608, 0.7592566023652994600, 1.725633230170963543E-31 ) ) ;
#22630 = CARTESIAN_POINT ( 'NONE',  ( 4.708759422647839976, 4.387974169377582001, -0.7998128361456211532 ) ) ;
#22631 = ORIENTED_EDGE ( 'NONE', *, *, #65958, .F. ) ;
#22632 = EDGE_CURVE ( 'NONE', #74610, #143389, #61964, .T. ) ;
#22633 = CARTESIAN_POINT ( 'NONE',  ( 5.554314605481814660, -1.277030258849481736, 1.560512323070535112 ) ) ;
#22634 = CARTESIAN_POINT ( 'NONE',  ( 0.6453774867190856801, 0.1600191834128759094, 2.114519675249281416 ) ) ;
#22635 = STYLED_ITEM ( 'NONE', ( #29335 ), #121837 ) ;
#22636 = CARTESIAN_POINT ( 'NONE',  ( 0.1071175833137206629, -7.075894077951318707E-15, -1.231310646603006376 ) ) ;
#22637 = FACE_OUTER_BOUND ( 'NONE', #98082, .T. ) ;
#22638 = CARTESIAN_POINT ( 'NONE',  ( -5.775410249741523394, 5.840326167560965231, 0.7216878364870317197 ) ) ;
#22639 = VECTOR ( 'NONE', #140517, 1000.000000000000000 ) ;
#22640 = CARTESIAN_POINT ( 'NONE',  ( 2.184835310096557404, 5.700724961754617404, 1.040834085586084257E-14 ) ) ;
#22641 = CARTESIAN_POINT ( 'NONE',  ( 3.819166351039466001, -1.734870831597424612, -0.9322225710242746377 ) ) ;
#22642 = CARTESIAN_POINT ( 'NONE',  ( 4.956657736208940790, -1.899625167328807374, -0.6766988040120130998 ) ) ;
#22643 = CARTESIAN_POINT ( 'NONE',  ( -6.775324078527193983, 8.927630729746953264, -1.599625672291263179 ) ) ;
#22644 = CYLINDRICAL_SURFACE ( 'NONE', #73522, 0.08000000000000041800 ) ;
#22645 = CARTESIAN_POINT ( 'NONE',  ( 4.699289266375740404, -0.5861454505808120219, 2.111544493182772708 ) ) ;
#22646 = CARTESIAN_POINT ( 'NONE',  ( 2.889578633693023590, 1.361086032938205070, 1.363490106525049317 ) ) ;
#22647 = CARTESIAN_POINT ( 'NONE',  ( -6.669721502918952716, 9.868759955792373972, 1.199719254218452047 ) ) ;
#22648 = CARTESIAN_POINT ( 'NONE',  ( -0.02988540731096045455, 2.895077309840556445, -2.215427197800499570 ) ) ;
#22649 = LINE ( 'NONE', #86610, #18934 ) ;
#22650 = CARTESIAN_POINT ( 'NONE',  ( -9.086228366407658186, 14.48154074263858604, 7.851304407759048587 ) ) ;
#22651 = CARTESIAN_POINT ( 'NONE',  ( 5.148345644887269756, 7.029489223833707001, -1.599625672291256295 ) ) ;
#22652 = ORIENTED_EDGE ( 'NONE', *, *, #5514, .F. ) ;
#22653 = CARTESIAN_POINT ( 'NONE',  ( 3.580761967785000888, 7.191656372475549119, -0.7216878364870338292 ) ) ;
#22654 = CARTESIAN_POINT ( 'NONE',  ( 5.225436369306192930, 0.1968503305618974075, -1.959608170402066696 ) ) ;
#22656 = CARTESIAN_POINT ( 'NONE',  ( 3.633450831153079541, -0.1460068579729571769, 2.007839618615501642 ) ) ;
#22655 = CARTESIAN_POINT ( 'NONE',  ( 0.2220789341932476180, 1.858810982918417620, 0.5625763381651854855 ) ) ;
#22657 = CARTESIAN_POINT ( 'NONE',  ( 5.343244854357415363, -1.283103863925443955, 1.906741504182138502 ) ) ;
#22659 = CARTESIAN_POINT ( 'NONE',  ( 3.748742453178009360, -0.3589989779783793744, -1.825800159725386118 ) ) ;
#22658 = CARTESIAN_POINT ( 'NONE',  ( 10.56514123924917392, 9.841080455211937306, -3.404988257269842222 ) ) ;
#22660 = CARTESIAN_POINT ( 'NONE',  ( -3.285556943750000070, -0.1093749995220438809, 0.000000000000000000 ) ) ;
#22661 = CARTESIAN_POINT ( 'NONE',  ( -9.837588353263715391, -6.372041098637188483, 1.678902898539189045E-12 ) ) ;
#22662 = CARTESIAN_POINT ( 'NONE',  ( 6.363533315466952445, -1.540175188624912650, -1.133462061071670579 ) ) ;
#22663 = CARTESIAN_POINT ( 'NONE',  ( -6.989391883044787868, 8.113044270762433285, -1.199719254218446718 ) ) ;
#22664 = CARTESIAN_POINT ( 'NONE',  ( -4.990809943606281607, 6.915973915664348937, -1.443375672974066548 ) ) ;
#22665 = CARTESIAN_POINT ( 'NONE',  ( 5.618719695961268634, -0.05021595884377753893, 2.090305304898040006 ) ) ;
#22666 = CARTESIAN_POINT ( 'NONE',  ( 5.260200412422194383, 7.159986452624450770, -1.443375672974051449 ) ) ;
#22667 = ORIENTED_EDGE ( 'NONE', *, *, #100462, .F. ) ;
#22668 = DIRECTION ( 'NONE',  ( -0.000000000000000000, -1.000000000000000000, 0.000000000000000000 ) ) ;
#22669 = CARTESIAN_POINT ( 'NONE',  ( 0.7326872660318053398, 0.1314506862302306234, 1.821024990000128518 ) ) ;
#22670 = CARTESIAN_POINT ( 'NONE',  ( -3.737243898861318137, 7.511868315313511069, 0.7998128361456341429 ) ) ;
#22671 = CARTESIAN_POINT ( 'NONE',  ( 3.058897358425614055, -1.030606816589432873, 1.394497854932384762 ) ) ;
#22672 = DIRECTION ( 'NONE',  ( 3.330669073875479482E-16, -3.330669073875479482E-16, -1.000000000000000000 ) ) ;
#22674 = CARTESIAN_POINT ( 'NONE',  ( -5.530836599371015794, 8.540060901653093950, 1.199719254218452047 ) ) ;
#22673 = AXIS2_PLACEMENT_3D ( 'NONE', #39160, #102025, #167030 ) ;
#22675 = CARTESIAN_POINT ( 'NONE',  ( 3.649297074908570321E-15, -6.789018801444764277E-15, 0.2598076211376221800 ) ) ;
#22676 = CARTESIAN_POINT ( 'NONE',  ( 6.983263157960363010, -0.009046620988246899253, 2.153544821522495489 ) ) ;
#22677 = CARTESIAN_POINT ( 'NONE',  ( 5.479063914364931343, -0.04889757770590653918, -1.825204647902956889 ) ) ;
#22678 = CARTESIAN_POINT ( 'NONE',  ( 3.080854412065773928, 1.845568107317007822, 0.6654098317215583203 ) ) ;
#22679 = CARTESIAN_POINT ( 'NONE',  ( 1.224999999999971001, -0.08333333265048434302, 0.7072540797572797189 ) ) ;
#22680 = CARTESIAN_POINT ( 'NONE',  ( -8.829384350997580455, 11.32403438096243775, 1.599625672291269396 ) ) ;
#22681 = CARTESIAN_POINT ( 'NONE',  ( 7.775764792637399836, 9.030479331953833011, -1.199719254218441611 ) ) ;
#22682 = CARTESIAN_POINT ( 'NONE',  ( 3.949941927655271190, -1.463281269271698770, -1.534908012577620440 ) ) ;
#22683 = CARTESIAN_POINT ( 'NONE',  ( -2.480778921620681921, 5.838066475291996404, 1.040834085586084257E-14 ) ) ;
#22684 = CARTESIAN_POINT ( 'NONE',  ( -7.784352752540590004, 12.23349531127272094, 0.7998128361456481317 ) ) ;
#22685 = CARTESIAN_POINT ( 'NONE',  ( 2.342711862795249012, -2.029470198211943632, -0.4080651701656515251 ) ) ;
#22686 = CARTESIAN_POINT ( 'NONE',  ( -11.89942855770814134, 11.29999999999999893, 0.6999999999999992895 ) ) ;
#22688 = ORIENTED_EDGE ( 'NONE', *, *, #20771, .F. ) ;
#22687 = CARTESIAN_POINT ( 'NONE',  ( 4.108218931252209494, -0.8498058027226679245, 2.052504409502105442 ) ) ;
#22689 = CARTESIAN_POINT ( 'NONE',  ( 2.180727191476996563, 1.779927251244978192, 1.454631630963822309 ) ) ;
#22691 = CARTESIAN_POINT ( 'NONE',  ( 0.4440980561614649158, -0.9299495107331550159, 1.727370323332158897 ) ) ;
#22690 = CARTESIAN_POINT ( 'NONE',  ( 8.080296364064698977, 12.37083682481011060, -0.7216878364870328300 ) ) ;
#22693 = CARTESIAN_POINT ( 'NONE',  ( 1.001543065824772753E-15, -0.2624999999999988454, 4.012584370867899430 ) ) ;
#22692 = CARTESIAN_POINT ( 'NONE',  ( 7.349928672384119288, 8.707909884937221179, 1.082531754730549967 ) ) ;
#22694 = DIRECTION ( 'NONE',  ( 0.000000000000000000, 8.546850786086437571E-32, 1.000000000000000000 ) ) ;
#22695 = CARTESIAN_POINT ( 'NONE',  ( 6.497600353373155002, -1.840680978339729545, 0.05264081064878384231 ) ) ;
#22696 = VERTEX_POINT ( 'NONE', #2805 ) ;
#22698 = CARTESIAN_POINT ( 'NONE',  ( -10.75000000000000000, 0.000000000000000000, 0.000000000000000000 ) ) ;
#22697 = AXIS2_PLACEMENT_3D ( 'NONE', #27581, #93679, #159721 ) ;
#22699 = CARTESIAN_POINT ( 'NONE',  ( 3.181800181368432678, 1.864768544494728175, -0.4233684943922080834 ) ) ;
#22700 = CARTESIAN_POINT ( 'NONE',  ( -0.1106727585415863135, 6.947232144882324434, -2.598525652753637782 ) ) ;
#22701 = CARTESIAN_POINT ( 'NONE',  ( 3.574969364760666846, 0.04275877055364904478, -1.724416222950067690 ) ) ;
#22702 = CARTESIAN_POINT ( 'NONE',  ( 2.712125330650519750, 1.116209241849321465, -1.679223868463100233 ) ) ;
#22703 = CARTESIAN_POINT ( 'NONE',  ( 3.797728626882245884, 1.624942816722572125, -1.626123495085467496 ) ) ;
#22704 = CARTESIAN_POINT ( 'NONE',  ( 3.515140014801207524, 2.043520737213794458, 0.9711500472536734874 ) ) ;
#22705 = CARTESIAN_POINT ( 'NONE',  ( 6.059223728125719965, -1.805531155315470926, -1.083989359861557533 ) ) ;
#22706 = CARTESIAN_POINT ( 'NONE',  ( -5.722950238744243023, 7.770137593325314285, 1.443375672974058777 ) ) ;
#22707 = ORIENTED_EDGE ( 'NONE', *, *, #142558, .T. ) ;
#22708 = CARTESIAN_POINT ( 'NONE',  ( 4.938602502702000407, 0.3022688342860947452, 1.743538433004296673 ) ) ;
#22710 = CARTESIAN_POINT ( 'NONE',  ( 0.6918693526153978368, -0.8198495674218098106, 2.140808456117601732 ) ) ;
#22709 = CARTESIAN_POINT ( 'NONE',  ( 5.203297092594585393, 9.292540051327542017, 0.7998128361456341429 ) ) ;
#22711 = B_SPLINE_CURVE_WITH_KNOTS ( 'NONE', 3,
 ( #166807, #1070, #183042, #202464, #19464, #35721, #200340, #115979, #201401, #169984 ),
 .UNSPECIFIED., .F., .F.,
 ( 4, 3, 3, 4 ),
 ( 2.763748478102358283E-14, 6.251571079173980452E-05, 0.0001250313277099753971, 0.0002424569244162144992 ),
 .UNSPECIFIED. ) ;
#22712 = CARTESIAN_POINT ( 'NONE',  ( 6.122987604524110949, -1.732013368603693593, 0.6248225064409973495 ) ) ;
#22713 = CARTESIAN_POINT ( 'NONE',  ( -4.081167932913447594, 4.720116328942494555, -1.199719254218452047 ) ) ;
#22714 = CARTESIAN_POINT ( 'NONE',  ( 5.472676780243426187, -0.05103125619924236966, -2.191024458042860168 ) ) ;
#22715 = CARTESIAN_POINT ( 'NONE',  ( -6.303615075710993665, 6.318915441276411471, -0.7998128361456362523 ) ) ;
#22716 = CARTESIAN_POINT ( 'NONE',  ( -4.457933580795036654, 4.095344020549286590, -0.7998128361456221525 ) ) ;
#22717 = CARTESIAN_POINT ( 'NONE',  ( -4.750201942159842261, 15.44698457193027785, 10.98078241047744186 ) ) ;
#22718 = CARTESIAN_POINT ( 'NONE',  ( 6.250451049865752395, -2.060019788584551481, -0.2068627631737207651 ) ) ;
#22719 = CARTESIAN_POINT ( 'NONE',  ( 0.3566581422463632189, -1.900417414521380133, -0.6748426577906708745 ) ) ;
#22720 = CARTESIAN_POINT ( 'NONE',  ( -1.402160292154681736E-14, -0.8812499993171809543, -1.732050807568870754 ) ) ;
#22721 = CARTESIAN_POINT ( 'NONE',  ( 3.932187577746598883, 1.029727551008235320, -1.628035494724868970 ) ) ;
#22722 = CARTESIAN_POINT ( 'NONE',  ( -1.402160292154681736E-14, 9.671875000341399797, 1.575800808251682339 ) ) ;
#22723 = CARTESIAN_POINT ( 'NONE',  ( 0.8443251495477720470, -1.414827328263716266, -1.712562173056450643 ) ) ;
#22725 = ORIENTED_EDGE ( 'NONE', *, *, #117255, .T. ) ;
#22724 = FACE_BOUND ( 'NONE', #165825, .T. ) ;
#22727 = CARTESIAN_POINT ( 'NONE',  ( -7.649321060469629785, -7.336076765398686028, 6.992767129439145357 ) ) ;
#22726 = CARTESIAN_POINT ( 'NONE',  ( -11.78331023100045627, 12.21999999999998288, 1.799999999999999600 ) ) ;
#22728 = CARTESIAN_POINT ( 'NONE',  ( 4.390142812726693045, 4.016254791136236513, 1.214306433183764966E-14 ) ) ;
#22729 = CARTESIAN_POINT ( 'NONE',  ( -6.441468915117185112, 6.687670953824438769, 0.7183096694902652013 ) ) ;
#22730 = CARTESIAN_POINT ( 'NONE',  ( 1.284279953904119864, 3.046639714193936754, -0.7749999999999910294 ) ) ;
#22731 = CARTESIAN_POINT ( 'NONE',  ( 2.558977423257744022, 1.577441344615847951, -1.166261179026031547 ) ) ;
#22733 = CARTESIAN_POINT ( 'NONE',  ( -1.364683531250012516, 3.051041667008083547, -0.7879004041258289570 ) ) ;
#22732 = CARTESIAN_POINT ( 'NONE',  ( 5.473741331615251227, 7.409117525016355010, -1.599625672291262513 ) ) ;
#22734 = DIRECTION ( 'NONE',  ( -5.551115123125764829E-17, 0.000000000000000000, 1.000000000000000000 ) ) ;
#22735 = CARTESIAN_POINT ( 'NONE',  ( 6.549272904993657995, 1.707534169505098953, -0.9658701945045378157 ) ) ;
#22736 = CARTESIAN_POINT ( 'NONE',  ( -7.323375529675950624, 11.69568855126397011, -0.7998128361456291469 ) ) ;
#22737 = CARTESIAN_POINT ( 'NONE',  ( -3.904385050611244079, 7.498940292447679568, 1.040834085586084257E-14 ) ) ;
#22738 = CARTESIAN_POINT ( 'NONE',  ( 0.3919815047150644327, 1.678997099660347603, 1.516718289441946199 ) ) ;
#22740 = EDGE_LOOP ( 'NONE', ( #120498, #27691 ) ) ;
#22739 = CARTESIAN_POINT ( 'NONE',  ( -5.422371370461663176, 8.413518134592214537, -1.199719254218446718 ) ) ;
#22741 = CARTESIAN_POINT ( 'NONE',  ( -1.364683531249997417, 5.259375000341425022, 1.214306433183764966E-14 ) ) ;
#22742 = CARTESIAN_POINT ( 'NONE',  ( 1.036156370570060270, 1.841834720703208639, 0.3256331921374157057 ) ) ;
#22743 = CARTESIAN_POINT ( 'NONE',  ( 0.2813449273042024079, 1.443300801228193153, -0.9609375900588543740 ) ) ;
#22745 = CARTESIAN_POINT ( 'NONE',  ( 4.300438532332786501, 1.693616701070689956, -1.390861761948622766 ) ) ;
#22744 = CARTESIAN_POINT ( 'NONE',  ( 0.6801582343749796866, 1.723958333674766141, 1.178068619123784355 ) ) ;
#22746 = CARTESIAN_POINT ( 'NONE',  ( 5.262836394871557744, -1.675821390925121168, 1.586616667910417888 ) ) ;
#22747 = CARTESIAN_POINT ( 'NONE',  ( 0.6552379465495603572, -1.740689658905628878, -1.102993579323052753 ) ) ;
#22748 = CARTESIAN_POINT ( 'NONE',  ( 2.150241637240562831, -1.501185980473922488, 1.231905181128474691 ) ) ;
#22749 = CARTESIAN_POINT ( 'NONE',  ( -4.351804119862249465, 7.060559992272473551, 1.082531754730560403 ) ) ;
#22750 = FILL_AREA_STYLE_COLOUR ( '', #185503 ) ;
#22751 = CARTESIAN_POINT ( 'NONE',  ( 3.757017964762656703, 7.397288368949487491, -1.734723475976807094E-15 ) ) ;
#22752 = CARTESIAN_POINT ( 'NONE',  ( -3.956095110007851991E-14, 0.3281250003414356020, -1.570758158831788265 ) ) ;
#22753 = CARTESIAN_POINT ( 'NONE',  ( 3.762342404062005041, 1.897698010425369786, -0.6819954029829021769 ) ) ;
#22754 = CARTESIAN_POINT ( 'NONE',  ( -3.741687207247254676, 7.309126141856352454, 1.040834085586084257E-14 ) ) ;
#22755 = CARTESIAN_POINT ( 'NONE',  ( -7.391130018105325661, 8.652015104991543026, -1.199719254218452047 ) ) ;
#22756 = B_SPLINE_CURVE_WITH_KNOTS ( 'NONE', 3,
 ( #192703, #96317, #193781, #95253 ),
 .UNSPECIFIED., .F., .F.,
 ( 4, 4 ),
 ( 0.000000000000000000, 8.505390838610418455E-05 ),
 .UNSPECIFIED. ) ;
#22757 = CARTESIAN_POINT ( 'NONE',  ( 3.673896439623286714, 4.156855427197417185, -2.419999999999995044 ) ) ;
#22759 = CARTESIAN_POINT ( 'NONE',  ( 7.747753938335137924, -5.575271019048081200, -7.808923410443490809 ) ) ;
#22758 = CARTESIAN_POINT ( 'NONE',  ( 0.6447967512687136082, -1.567379569643694515, 0.9359695128687425258 ) ) ;
#22760 = CARTESIAN_POINT ( 'NONE',  ( -4.599959256786493533, 8.588645909551377855, 0.000000000000000000 ) ) ;
#22761 = CARTESIAN_POINT ( 'NONE',  ( -9.569358774149643310, 3.553052365627049625, 7.167287524840453727 ) ) ;
#22762 = CARTESIAN_POINT ( 'NONE',  ( -10.96276904610368597, 4.385383195573210102, 6.374211443005175504 ) ) ;
#22763 = ORIENTED_EDGE ( 'NONE', *, *, #178800, .F. ) ;
#22764 = CARTESIAN_POINT ( 'NONE',  ( 5.594623806460828241, -0.4985412361782278201, -1.999555476978178703 ) ) ;
#22765 = CARTESIAN_POINT ( 'NONE',  ( -7.119440060507479018, 8.439006504414422238, 1.082531754730549078 ) ) ;
#22766 = EDGE_CURVE ( 'NONE', #121840, #148633, #160275, .T. ) ;
#22767 = CARTESIAN_POINT ( 'NONE',  ( 1.931788062848141441E-13, 7.054063922337705073, -3.955400951015614730 ) ) ;
#22768 = CARTESIAN_POINT ( 'NONE',  ( -4.711622075948912247, 5.455646162483875017, -1.199719254218446718 ) ) ;
#22769 = CARTESIAN_POINT ( 'NONE',  ( -9.809487834687324437, 11.40315621434539395, 1.199719254218462483 ) ) ;
#22770 = CARTESIAN_POINT ( 'NONE',  ( 5.197918162715867929, 1.358090353789550342, 1.495039904793266095 ) ) ;
#22771 = CARTESIAN_POINT ( 'NONE',  ( 5.918639493159310483, -0.7970842504121906646, -2.073522590485813666 ) ) ;
#22772 = CARTESIAN_POINT ( 'NONE',  ( -3.142457743317409680, 6.888227477170756785, 0.7998128361456352531 ) ) ;
#22773 = CARTESIAN_POINT ( 'NONE',  ( 5.144429221381498607, 8.089252293998699272, -1.199719254218452047 ) ) ;
#22774 = CARTESIAN_POINT ( 'NONE',  ( 5.471578299931997513, 1.986755592664890324, -0.5475478416450995089 ) ) ;
#22775 = CARTESIAN_POINT ( 'NONE',  ( 4.324842380567116784, 0.8596320953860696612, -1.824118450417112847 ) ) ;
#22776 = ORIENTED_EDGE ( 'NONE', *, *, #31576, .T. ) ;
#22777 = CARTESIAN_POINT ( 'NONE',  ( 3.867100128395839942, 5.534702787927018974, -1.599625672291255185 ) ) ;
#22778 = B_SPLINE_CURVE_WITH_KNOTS ( 'NONE', 3,
 ( #154546, #171855, #23450, #89562, #57043, #106918 ),
 .UNSPECIFIED., .F., .F.,
 ( 4, 2, 4 ),
 ( 0.001263516168593488680, 0.001315211845502643750, 0.001366907522411799037 ),
 .UNSPECIFIED. ) ;
#22780 = ORIENTED_EDGE ( 'NONE', *, *, #34390, .F. ) ;
#22779 = CARTESIAN_POINT ( 'NONE',  ( -5.824109505522200081, 8.952488968821326054, -1.199719254218452047 ) ) ;
#22781 = CARTESIAN_POINT ( 'NONE',  ( 5.910429572389825026, 7.145202977605201511, -1.123150837922413547 ) ) ;
#22782 = CARTESIAN_POINT ( 'NONE',  ( 4.007185349139028574, 2.006139037694018690, 0.2004037502189442987 ) ) ;
#22783 = CARTESIAN_POINT ( 'NONE',  ( 4.031074566243696644, -1.271087849624694233, -1.332192834049110486 ) ) ;
#22784 = CARTESIAN_POINT ( 'NONE',  ( 2.494940289813108780, 3.447199233515649386, -11.73777120880564695 ) ) ;
#22785 = CARTESIAN_POINT ( 'NONE',  ( 2.139721691919532098, -2.060220725375282225, 1.039829281875967570 ) ) ;
#22786 = CARTESIAN_POINT ( 'NONE',  ( 4.167152111353856547, 5.955039778036558040, 1.599625672291262513 ) ) ;
#22787 = CARTESIAN_POINT ( 'NONE',  ( 3.550220938608072085, 2.161773192003491495, 0.003901938047633223515 ) ) ;
#22788 = CARTESIAN_POINT ( 'NONE',  ( 8.284195553149872993, 9.623648552551724578, -1.199719254218445830 ) ) ;
#22789 = CARTESIAN_POINT ( 'NONE',  ( -5.786632634934295361, 5.645492917045106473, 0.7998128361456341429 ) ) ;
#22790 = CARTESIAN_POINT ( 'NONE',  ( 3.691010296293754323, -1.365721494773973754, -1.848513781679576251 ) ) ;
#22791 = AXIS2_PLACEMENT_3D ( 'NONE', #192194, #65384, #47056 ) ;
#22792 = CARTESIAN_POINT ( 'NONE',  ( 1.499999999999990896, 4.056250000682819490, 1.214306433183764966E-14 ) ) ;
#22793 = CARTESIAN_POINT ( 'NONE',  ( 2.166681600665042229, -1.709288833360942617, -0.7604731621856930524 ) ) ;
#22794 = EDGE_CURVE ( 'NONE', #117081, #56620, #133947, .T. ) ;
#22795 = CARTESIAN_POINT ( 'NONE',  ( 6.420779677996255153, 1.839401344301737184, 0.7098503129845078474 ) ) ;
#22796 = MECHANICAL_DESIGN_GEOMETRIC_PRESENTATION_REPRESENTATION (  '', ( #29641 ), #71185 ) ;
#22798 = CARTESIAN_POINT ( 'NONE',  ( -5.399890319992785237, 9.521898816625391504, 0.7998128361456291469 ) ) ;
#22797 = CARTESIAN_POINT ( 'NONE',  ( -1.201851678989727383E-14, 4.946875000341420581, -1.575800808251660134 ) ) ;
#22799 = B_SPLINE_CURVE_WITH_KNOTS ( 'NONE', 3,
 ( #178918, #96613, #99784, #196225 ),
 .UNSPECIFIED., .F., .F.,
 ( 4, 4 ),
 ( 0.0004855182311547751126, 0.001091960318275098660 ),
 .UNSPECIFIED. ) ;
#22801 = CARTESIAN_POINT ( 'NONE',  ( 1.594636444620714633, -2.196503929104542951, -0.2137616909994101977 ) ) ;
#22800 = CARTESIAN_POINT ( 'NONE',  ( -6.410307701162927252, 6.373113827645189744, -0.7998128361456291469 ) ) ;
#22802 = CARTESIAN_POINT ( 'NONE',  ( -3.719872605471121751, 6.605953636083950364, -2.499999999999998668 ) ) ;
#22803 = CARTESIAN_POINT ( 'NONE',  ( 4.222474775652216294, 7.013638773981186958, 1.199719254218462483 ) ) ;
#22804 = CARTESIAN_POINT ( 'NONE',  ( -3.978428010606240850, 6.728917548094202949, -1.199719254218452047 ) ) ;
#22805 = CARTESIAN_POINT ( 'NONE',  ( -7.721398836998369042, -5.907420853759296264, 7.721398836998396575 ) ) ;
#22806 = CARTESIAN_POINT ( 'NONE',  ( 6.403199630258991526, 1.638877779571865423, 1.095505698648422177 ) ) ;
#22807 = CARTESIAN_POINT ( 'NONE',  ( 5.338606043529401823, 2.272755431710461238, 0.3992410602531944464 ) ) ;
#22808 = CARTESIAN_POINT ( 'NONE',  ( 0.4495626703563436743, 1.451167377975391304, 1.320406988977901985 ) ) ;
#22809 = CARTESIAN_POINT ( 'NONE',  ( 2.518489969072700507, 0.8780072382167501965, 1.866465334303254897 ) ) ;
#22810 = CARTESIAN_POINT ( 'NONE',  ( 7.632877294813741109, 8.007371053478589573, 1.040834085586084257E-14 ) ) ;
#22811 = CARTESIAN_POINT ( 'NONE',  ( 4.598150373690133463, 5.393538853173795111, -1.199719254218452047 ) ) ;
#22812 =( BOUNDED_CURVE ( )  B_SPLINE_CURVE ( 2, ( #83134, #144991, #114652, #82071, #214165, #162277, #46398 ),
 .UNSPECIFIED., .F., .T. ) 
 B_SPLINE_CURVE_WITH_KNOTS ( ( 3, 2, 2, 3 ),
 ( 0.3784226669537131271, 0.3809523809523809312, 0.3869047619047619180, 0.3894344759034563674 ),
 .UNSPECIFIED. ) 
 CURVE ( )  GEOMETRIC_REPRESENTATION_ITEM ( )  RATIONAL_B_SPLINE_CURVE ( ( 0.9345202395942608931, 0.9430618748659213013, 1.000000000000000000, 0.8660254037844387076, 1.000000000000000000, 0.9430618748653214478, 0.9345202395940808149 ) ) 
 REPRESENTATION_ITEM ( '' )  );
#22813 = CARTESIAN_POINT ( 'NONE',  ( 5.761852095683461350, 9.665985178365305686, -0.7216878364870267237 ) ) ;
#22814 = CARTESIAN_POINT ( 'NONE',  ( 1.364683531249990311, 3.946875000341417028, 1.214306433183764966E-14 ) ) ;
#22815 = FACE_OUTER_BOUND ( 'NONE', #160969, .T. ) ;
#22816 = CARTESIAN_POINT ( 'NONE',  ( 4.270455198180219902, 6.965652916976816655, -1.082531754730548412 ) ) ;
#22817 = CARTESIAN_POINT ( 'NONE',  ( 0.2687526973377635797, -0.9260139170579514412, -1.961338766822422919 ) ) ;
#22819 = CARTESIAN_POINT ( 'NONE',  ( 5.354971380013192395, 0.3533838956982695567, -1.806849549699687696 ) ) ;
#22818 = CARTESIAN_POINT ( 'NONE',  ( -11.35605497252127094, 9.985818540483544226, -3.553547709190210124 ) ) ;
#22820 = CARTESIAN_POINT ( 'NONE',  ( 6.620655732516683045, 6.038298567659169613, 2.521170675138622475 ) ) ;
#22821 = CARTESIAN_POINT ( 'NONE',  ( 6.720655732516647163, -0.004400176169771369272, 2.173773060281408931 ) ) ;
#22822 = CARTESIAN_POINT ( 'NONE',  ( 0.2626887844769665303, -1.667795467377327423, -0.8471929967568125885 ) ) ;
#22823 = CARTESIAN_POINT ( 'NONE',  ( 6.543838037463636681, 0.8733170268561093463, -2.087377253365163110 ) ) ;
#22824 = CARTESIAN_POINT ( 'NONE',  ( -5.364460139690476304, 6.514416944181776081, 1.355983593732257741 ) ) ;
#22825 = CARTESIAN_POINT ( 'NONE',  ( -0.1904212755198937679, 3.362625042665647879, -2.069931805936022329 ) ) ;
#22826 = CARTESIAN_POINT ( 'NONE',  ( 6.257994703896152089, 7.000112715747270009, 0.9732540237740094913 ) ) ;
#22827 = CARTESIAN_POINT ( 'NONE',  ( 0.4692111731946085884, -1.615589042895089200, -1.022764193708516789 ) ) ;
#22828 = CARTESIAN_POINT ( 'NONE',  ( 1.586397006687990885, -0.2552452650203296813, -1.751205042619798258 ) ) ;
#22829 = VECTOR ( 'NONE', #108296, 1000.000000000000000 ) ;
#22830 = CARTESIAN_POINT ( 'NONE',  ( 6.322908177684296582, 1.490210921086480234, -1.353605025193492128 ) ) ;
#22832 = CARTESIAN_POINT ( 'NONE',  ( 3.145994354733801845, 0.8638979756431870438, 1.709836580976647813 ) ) ;
#22831 = CARTESIAN_POINT ( 'NONE',  ( -7.818248136574758256, 12.27303992597924420, 0.000000000000000000 ) ) ;
#22833 = CARTESIAN_POINT ( 'NONE',  ( -5.602498012743508227, 5.726462300312828546, -0.1687859242097844992 ) ) ;
#22834 = CARTESIAN_POINT ( 'NONE',  ( 4.000420421810535032, 1.959860935258441517, 0.1952677912114946512 ) ) ;
#22835 = CARTESIAN_POINT ( 'NONE',  ( 0.2113915902133572944, 1.759560880827226947, -1.183302968686468226 ) ) ;
#22836 = CARTESIAN_POINT ( 'NONE',  ( -3.216308754939891212, 4.775446185561722956, -1.599625672291262513 ) ) ;
#22837 = CARTESIAN_POINT ( 'NONE',  ( 3.115926070338378207, -0.9207206926411042325, -1.628290677324291780 ) ) ;
#22839 = VERTEX_POINT ( 'NONE', #118781 ) ;
#22838 = CARTESIAN_POINT ( 'NONE',  ( 6.059189007909253633, -1.483166448586000774, -0.8803546789384365523 ) ) ;
#22841 = CARTESIAN_POINT ( 'NONE',  ( 4.704316114261903436, 4.590716342834741504, 1.214306433183764966E-14 ) ) ;
#22840 = CARTESIAN_POINT ( 'NONE',  ( 2.578998426009218470, -2.112161100990978202, -0.6396139477699357423 ) ) ;
#22842 = CARTESIAN_POINT ( 'NONE',  ( -0.6823417656249969321, 3.530208333674754506, -1.181850606188749264 ) ) ;
#22843 = CARTESIAN_POINT ( 'NONE',  ( 1.170463292146912915, -0.9257924050831314311, -1.843294045186917085 ) ) ;
#22844 = CARTESIAN_POINT ( 'NONE',  ( 5.764187864104357573, 9.876636274763768597, 1.040834085586084257E-14 ) ) ;
#22845 = LINE ( 'NONE', #204794, #191991 ) ;
#22846 = CARTESIAN_POINT ( 'NONE',  ( -1.874158809982213958, 3.299964346911606228, -0.4000000000000374922 ) ) ;
#22847 = CARTESIAN_POINT ( 'NONE',  ( -5.091250377131585125, 5.898545847196970726, 1.199719254218450271 ) ) ;
#22848 = VECTOR ( 'NONE', #31488, 1000.000000000000000 ) ;
#22849 = CARTESIAN_POINT ( 'NONE',  ( -4.505562513083238407, 8.245961809465203629, -0.2033783863445335349 ) ) ;
#22850 = ORIENTED_EDGE ( 'NONE', *, *, #66705, .F. ) ;
#22851 = CARTESIAN_POINT ( 'NONE',  ( 3.209495720308676248, -1.691010085789945716, -1.194244797349801157 ) ) ;
#22852 = CARTESIAN_POINT ( 'NONE',  ( 0.7499999999999902300, 5.066666666666684193, -1.299038105676658228 ) ) ;
#22853 = CARTESIAN_POINT ( 'NONE',  ( 5.671388329218120639, 5.511041227042920099, 1.040834085586084257E-14 ) ) ;
#22854 = CARTESIAN_POINT ( 'NONE',  ( -6.480235040494578769, 6.771487114559836762, -0.2501488059577141598 ) ) ;
#22855 = CARTESIAN_POINT ( 'NONE',  ( 0.5748750247985534578, -1.461244816878112029, 1.394459567027491076 ) ) ;
#22856 = CARTESIAN_POINT ( 'NONE',  ( 1.364683531249990311, 4.134375000341417028, 1.214306433183764966E-14 ) ) ;
#22857 = VERTEX_POINT ( 'NONE', #115581 ) ;
#22858 = AXIS2_PLACEMENT_3D ( 'NONE', #5638, #25119, #202787 ) ;
#22860 = CARTESIAN_POINT ( 'NONE',  ( 8.920901888111989919, 11.43080484092926241, 1.443375672974076540 ) ) ;
#22859 = CARTESIAN_POINT ( 'NONE',  ( 0.07459516483344308391, 2.893589955008399883, -2.244599473808198020 ) ) ;
#22861 = CARTESIAN_POINT ( 'NONE',  ( 5.202499893966790800, -1.423744420606623429, -1.427717849564233532 ) ) ;
#22862 = CARTESIAN_POINT ( 'NONE',  ( 5.876186789644119557, -1.907177742178717716, -0.1804351137127818694 ) ) ;
#22863 = FACE_BOUND ( 'NONE', #69702, .T. ) ;
#22864 = CARTESIAN_POINT ( 'NONE',  ( 4.177398808104064720, 1.432170664236757540, 1.658919600136643524 ) ) ;
#22865 = CARTESIAN_POINT ( 'NONE',  ( -0.7500000000000215383, 1.472916667349486008, 1.299038105676659116 ) ) ;
#22866 = CARTESIAN_POINT ( 'NONE',  ( 2.056764645581514728, 0.4224895836346024280, 1.864965418913032913 ) ) ;
#22867 = CARTESIAN_POINT ( 'NONE',  ( -4.530395885260773525, 8.437212299446219532, 0.7998128361456481317 ) ) ;
#22868 = CARTESIAN_POINT ( 'NONE',  ( 4.161989969270892153, 6.839110149915929249, 1.082531754730558626 ) ) ;
#22869 = CARTESIAN_POINT ( 'NONE',  ( 0.9488424731869498086, -1.824129051820524205, -0.8596123018156722750 ) ) ;
#22870 = CARTESIAN_POINT ( 'NONE',  ( 0.6823417656249934904, 10.75520833367472839, 1.181850606188764807 ) ) ;
#22872 = CARTESIAN_POINT ( 'NONE',  ( -6.656127069666307072, 6.730179434224282886, 0.7998128361456341429 ) ) ;
#22871 = CARTESIAN_POINT ( 'NONE',  ( 6.603104432341277530, -0.4828188497946246382, 2.145653685147373313 ) ) ;
#22874 = ORIENTED_EDGE ( 'NONE', *, *, #174144, .F. ) ;
#22873 = CARTESIAN_POINT ( 'NONE',  ( 3.416762500535154068, 1.558979225792535006, 0.7381585831351898941 ) ) ;
#22875 =( LENGTH_UNIT ( ) NAMED_UNIT ( * ) SI_UNIT ( .MILLI., .METRE. ) );
#22876 = CARTESIAN_POINT ( 'NONE',  ( 6.421758314367153275, 10.64380180007036891, -0.7998128361456291469 ) ) ;
#22877 = CARTESIAN_POINT ( 'NONE',  ( 5.820528018968444961, 5.685037531751635953, 0.7998128361456341429 ) ) ;
#22878 = DIRECTION ( 'NONE',  ( 5.176899690512889097E-31, -0.6000000000000018652, 0.7999999999999984901 ) ) ;
#22879 = FACE_OUTER_BOUND ( 'NONE', #204899, .T. ) ;
#22880 = CARTESIAN_POINT ( 'NONE',  ( 5.733910645827320351, 5.654260273078802079, -0.3844519940494390831 ) ) ;
#22881 = CARTESIAN_POINT ( 'NONE',  ( 5.361359679200154105, 8.342337828120466980, 1.199719254218462483 ) ) ;
#22882 = CARTESIAN_POINT ( 'NONE',  ( -0.4019237886466933696, 10.80133545031537068, 1.500000000000005995 ) ) ;
#22883 = ORIENTED_EDGE ( 'NONE', *, *, #105983, .F. ) ;
#22884 = DIRECTION ( 'NONE',  ( 0.000000000000000000, 0.4225363771131893098, 0.9063459659622591369 ) ) ;
#22885 = ORIENTED_EDGE ( 'NONE', *, *, #144093, .T. ) ;
#22886 = CARTESIAN_POINT ( 'NONE',  ( 3.281707762122548555, 1.766655041338391907, -0.3996267988317265818 ) ) ;
#22887 = ORIENTED_EDGE ( 'NONE', *, *, #97582, .F. ) ;
#22888 = CARTESIAN_POINT ( 'NONE',  ( 10.53876547652418338, 11.18964789890005918, 0.7998128361456462443 ) ) ;
#22889 = CARTESIAN_POINT ( 'NONE',  ( 0.000000000000000000, -2.000000000000001776, 10.91999999999999105 ) ) ;
#22890 = CARTESIAN_POINT ( 'NONE',  ( 4.318897000252651885, 1.397372457865418083, -1.152701029936139099 ) ) ;
#22891 = CARTESIAN_POINT ( 'NONE',  ( 0.01387835396682936609, -7.030163990561721477, 9.597420367780074457 ) ) ;
#22892 = DIRECTION ( 'NONE',  ( 0.7592566023653004592, 0.6507913734559639396, -0.000000000000000000 ) ) ;
#22893 = CARTESIAN_POINT ( 'NONE',  ( 5.543269800280802073, 6.196057874731542015, 0.9238780061134096444 ) ) ;
#22894 = EDGE_CURVE ( 'NONE', #178259, #184579, #127154, .T. ) ;
#22896 = CARTESIAN_POINT ( 'NONE',  ( 0.6823417656249934904, 14.94270833367473195, 1.181850606188764807 ) ) ;
#22895 = CARTESIAN_POINT ( 'NONE',  ( 4.808966763405270406, -1.495079835775798838, 1.108065441546413288 ) ) ;
#22897 = CARTESIAN_POINT ( 'NONE',  ( 2.267068109148970834, 1.750504415394140922, -0.7784415599910772254 ) ) ;
#22898 = DIRECTION ( 'NONE',  ( 0.9366510587354612838, 0.000000000000000000, -0.3502638921866474409 ) ) ;
#22899 = CARTESIAN_POINT ( 'NONE',  ( -11.37834099079384487, 6.126291437673294205, 3.408052918099385931 ) ) ;
#22900 = CARTESIAN_POINT ( 'NONE',  ( 5.968508390656825036, 7.206245191706623032, 1.226434852180135149 ) ) ;
#22901 = DIRECTION ( 'NONE',  ( 0.06183953750878252997, 0.9962285034897218061, 0.06086575749408946329 ) ) ;
#22902 = CARTESIAN_POINT ( 'NONE',  ( 6.925078400183575233, 2.022016365062285104, 2.447829694591229899 ) ) ;
#22903 = CARTESIAN_POINT ( 'NONE',  ( 6.561783159334121152, 8.678499657355050800, -1.443375672974057666 ) ) ;
#22904 = CARTESIAN_POINT ( 'NONE',  ( -4.603156847039612920, 5.329103395422994716, 1.199719254218462483 ) ) ;
#22905 = CARTESIAN_POINT ( 'NONE',  ( -1.499999999999963141, 7.750000000000000000, 10.86128356754324820 ) ) ;
#22906 = EDGE_CURVE ( 'NONE', #53788, #47983, #27465, .T. ) ;
#22907 = CARTESIAN_POINT ( 'NONE',  ( 1.552797837233742095, -1.793874147449931344, -1.073420256486889324 ) ) ;
#22908 = CARTESIAN_POINT ( 'NONE',  ( 6.879836604291781121, 6.991173891287354003, -0.7998128361456341429 ) ) ;
#22909 = CARTESIAN_POINT ( 'NONE',  ( 6.176777841581622575, -1.829441475422811436, -0.6035904912435466896 ) ) ;
#22910 = CARTESIAN_POINT ( 'NONE',  ( -3.906720819032141190, 7.709591388846142479, -0.7998128361456281477 ) ) ;
#22911 = CARTESIAN_POINT ( 'NONE',  ( 2.221465439867484903, -1.771451409125622600, 0.4407646962370226351 ) ) ;
#22912 = CARTESIAN_POINT ( 'NONE',  ( 11.94651559118242190, 12.44869344121029009, 1.135242698369639980 ) ) ;
#22913 = CARTESIAN_POINT ( 'NONE',  ( 1.037202349414727109, -0.04413313863061394532, 1.912034500058952036 ) ) ;
#22914 = CARTESIAN_POINT ( 'NONE',  ( 1.240603756995876772, -1.920774042053990494, -0.4348295819559512831 ) ) ;
#22915 = CARTESIAN_POINT ( 'NONE',  ( 3.843253449720198667, 0.6512379428032251116, -1.829756300597375596 ) ) ;
#22916 = CIRCLE ( 'NONE', #9029, 0.4000000000000001332 ) ;
#22917 = ORIENTED_EDGE ( 'NONE', *, *, #185885, .T. ) ;
#22918 = DIRECTION ( 'NONE',  ( 1.000000000000000000, -0.000000000000000000, -0.000000000000000000 ) ) ;
#22920 = CARTESIAN_POINT ( 'NONE',  ( 0.2032580500000652490, -1.434579632348313982, -1.185340245312079377 ) ) ;
#22919 = CARTESIAN_POINT ( 'NONE',  ( -4.329849954717889915, 6.144853928627882489, 1.599625672291270506 ) ) ;
#22921 = CARTESIAN_POINT ( 'NONE',  ( 7.991605200612358573, 8.288237253661408843, 0.7998128361456281477 ) ) ;
#22922 = CARTESIAN_POINT ( 'NONE',  ( 6.653311379900189948, -6.675176078274398961, 6.940534579975176754 ) ) ;
#22923 = CARTESIAN_POINT ( 'NONE',  ( 7.235247531187115833, 11.59287255302699648, -0.7998128361456291469 ) ) ;
#22924 = CARTESIAN_POINT ( 'NONE',  ( -6.231907884136888676, 7.299589282028351001, -1.199719254218453823 ) ) ;
#22925 = CARTESIAN_POINT ( 'NONE',  ( 2.684151225825664788, 5.114964949229812596, -1.082531754730543083 ) ) ;
#22926 = VERTEX_POINT ( 'NONE', #66730 ) ;
#22927 = CARTESIAN_POINT ( 'NONE',  ( 7.374709211190586089, 7.568525266002632534, 0.000000000000000000 ) ) ;
#22928 = DIRECTION ( 'NONE',  ( 0.000000000000000000, 0.000000000000000000, -1.000000000000000000 ) ) ;
#22929 = CARTESIAN_POINT ( 'NONE',  ( 3.984828715814022981, -0.1808549858164226476, -1.816707794649790708 ) ) ;
#22930 = CARTESIAN_POINT ( 'NONE',  ( 0.000000000000000000, 1.000000000000000888, 0.000000000000000000 ) ) ;
#22931 = CARTESIAN_POINT ( 'NONE',  ( -9.408995418203979000, 12.00024729270324286, 1.443375672974076540 ) ) ;
#22932 = CARTESIAN_POINT ( 'NONE',  ( -4.936046011350697427, 8.098431898006973384, 1.075429046246343612 ) ) ;
#22933 = DIRECTION ( 'NONE',  ( 0.000000000000000000, 1.000000000000000000, 0.000000000000000000 ) ) ;
#22934 = CARTESIAN_POINT ( 'NONE',  ( 4.381629165553334815, 1.221847395770376377, 1.416585496670008659 ) ) ;
#22935 = CARTESIAN_POINT ( 'NONE',  ( 6.903072767652295383, 11.20533532890304684, 1.040834085586084257E-14 ) ) ;
#22937 = EDGE_CURVE ( 'NONE', #174805, #131565, #116647, .T. ) ;
#22936 = CARTESIAN_POINT ( 'NONE',  ( 1.611812915071403784, -1.911997954552616008, 0.2354761707349817823 ) ) ;
#22938 = CARTESIAN_POINT ( 'NONE',  ( 6.948121807170864805, -0.8414398651286276731, 1.770450887113049099 ) ) ;
#22939 = CARTESIAN_POINT ( 'NONE',  ( -1.500000000000008216, 15.50000000000000000, 3.469446951953614189E-15 ) ) ;
#22940 = CARTESIAN_POINT ( 'NONE',  ( -4.889686956022917919, 8.856385215335397021, 1.214306433183764966E-14 ) ) ;
#22941 = CARTESIAN_POINT ( 'NONE',  ( 5.007038802148489509, 4.735966778795008381, 0.7998128361456341429 ) ) ;
#22942 = CARTESIAN_POINT ( 'NONE',  ( -5.628043163004235794, 5.738674243025936761, 0.7216878364870257245 ) ) ;
#22943 = VECTOR ( 'NONE', #98808, 1000.000000000000227 ) ;
#22944 = CARTESIAN_POINT ( 'NONE',  ( 6.491443032814855130, -0.4656331456187530748, 2.073361762655197893 ) ) ;
#22945 = CARTESIAN_POINT ( 'NONE',  ( 9.541187415715040032, 12.15447128979948310, -1.599625672291262513 ) ) ;
#22947 = ADVANCED_FACE ( 'NONE', ( #199955 ), #53723, .F. ) ;
#22946 = CARTESIAN_POINT ( 'NONE',  ( -1.499912825862921073, 4.449810153648276589, 0.08469158891784515919 ) ) ;
#22948 = CARTESIAN_POINT ( 'NONE',  ( 4.715722526854881913, 0.4587184135333640111, -2.018627749927892179 ) ) ;
#22950 = CARTESIAN_POINT ( 'NONE',  ( 0.6823417656249882723, 2.988541667008084879, -1.181850606188754593 ) ) ;
#22949 = CARTESIAN_POINT ( 'NONE',  ( 0.1339853816830008371, 0.3136495386693045062, 1.814181566856580607 ) ) ;
#22951 = CARTESIAN_POINT ( 'NONE',  ( 5.414730038718025718, -1.455890720088355961, -1.778839290973016629 ) ) ;
#22952 = CARTESIAN_POINT ( 'NONE',  ( 7.632877294813741109, 8.007371053478589573, 1.040834085586084257E-14 ) ) ;
#22954 = CARTESIAN_POINT ( 'NONE',  ( 3.621833129746810265, 4.096114899008192367, -2.419999999999995044 ) ) ;
#22953 = CARTESIAN_POINT ( 'NONE',  ( 4.421367491832282504, 5.291255174293369556, 1.082531754730549078 ) ) ;
#22955 = CARTESIAN_POINT ( 'NONE',  ( 0.7797068561936998377, 1.543341569868655450, 1.695032692825575005 ) ) ;
#22956 = DIRECTION ( 'NONE',  ( 0.000000000000000000, 1.000000000000000000, 0.000000000000000000 ) ) ;
#22957 = CARTESIAN_POINT ( 'NONE',  ( -5.250750630242457362, 9.347902511916677426, 0.000000000000000000 ) ) ;
#22958 = CARTESIAN_POINT ( 'NONE',  ( 5.472584303614713264, -0.04973451981254246174, -1.941474127069875433 ) ) ;
#22959 = ORIENTED_EDGE ( 'NONE', *, *, #110772, .T. ) ;
#22960 = CARTESIAN_POINT ( 'NONE',  ( 7.741342523278686549, 11.97539067722642869, 0.7216878364870438212 ) ) ;
#22961 = ORIENTED_EDGE ( 'NONE', *, *, #202925, .T. ) ;
#22962 = CARTESIAN_POINT ( 'NONE',  ( 5.818603510220927255, -0.6945032022064903110, -1.782003016414166474 ) ) ;
#22963 = CARTESIAN_POINT ( 'NONE',  ( 5.788296071918774821, -0.7303023681345042206, -1.879805717804765353 ) ) ;
#22965 = CARTESIAN_POINT ( 'NONE',  ( -1.249999999999964695, 8.500000000000000000, -10.97907099895069294 ) ) ;
#22964 = CARTESIAN_POINT ( 'NONE',  ( -7.669108446824431269, 12.09904362127053545, -0.7998128361456291469 ) ) ;
#22966 = CARTESIAN_POINT ( 'NONE',  ( 3.285556943750000514, -2.501041666188708046, 1.896917185911906500 ) ) ;
#22968 = CARTESIAN_POINT ( 'NONE',  ( 0.7250502862299773588, -1.682426168213309703, 0.5495948440489316633 ) ) ;
#22967 = CARTESIAN_POINT ( 'NONE',  ( 2.431682593473180276, 0.9845738105917539729, -1.844271946693208708 ) ) ;
#22969 = CARTESIAN_POINT ( 'NONE',  ( 1.040949779275250140E-15, 7.250000000000006217, 8.500000000000000000 ) ) ;
#22970 = CARTESIAN_POINT ( 'NONE',  ( 3.925942518080671739, 1.227467849647005282, -1.935749465030587313 ) ) ;
#22971 = CARTESIAN_POINT ( 'NONE',  ( 1.991783209624857331, -0.4627563367010344986, -1.677588981799936541 ) ) ;
#22972 = CARTESIAN_POINT ( 'NONE',  ( 3.005103603723342953, 6.657704637652544832, -0.7998128361456291469 ) ) ;
#22973 = CARTESIAN_POINT ( 'NONE',  ( -2.679285714285713826, -0.4970443252110337551, -0.09999999999999592548 ) ) ;
#22974 = CARTESIAN_POINT ( 'NONE',  ( 2.213800448916534158, -1.389428533404401422, -1.036884654713841725 ) ) ;
#22975 = CARTESIAN_POINT ( 'NONE',  ( 0.6801582343749952297, 2.255208333674735499, 1.178068619123839866 ) ) ;
#22976 = CARTESIAN_POINT ( 'NONE',  ( 2.013881029938934919, 1.856366682828480608, -0.1327402387825328822 ) ) ;
#22977 = CARTESIAN_POINT ( 'NONE',  ( 1.996751263802678533, 2.147379752972265354, 0.3199099038852480370 ) ) ;
#22978 = CARTESIAN_POINT ( 'NONE',  ( 5.717788096661236885, 7.693838750903348789, 1.599625672291267398 ) ) ;
#22979 = CARTESIAN_POINT ( 'NONE',  ( 4.311732611912100666, -1.244383703160652610, -1.586670621409623116 ) ) ;
#22980 = CARTESIAN_POINT ( 'NONE',  ( 3.031250000000001776, -0.7852924748301450819, -1.895863743164018400 ) ) ;
#22981 = CARTESIAN_POINT ( 'NONE',  ( 0.7499999999999885647, 3.097916667349487341, -1.299038105676658228 ) ) ;
#22982 = CARTESIAN_POINT ( 'NONE',  ( 0.5692023642799119987, 0.1922812221162081003, -1.916781067358761748 ) ) ;
#22983 = CARTESIAN_POINT ( 'NONE',  ( 1.364683531249996529, 14.96354166700806410, 0.7879004041258405033 ) ) ;
#22984 = CARTESIAN_POINT ( 'NONE',  ( 4.711300293261502681, 1.846222065370630050, -1.235088439349934841 ) ) ;
#22985 = ORIENTED_EDGE ( 'NONE', *, *, #51647, .T. ) ;
#22986 = SURFACE_STYLE_USAGE ( .BOTH. , #27269 ) ;
#22987 = CARTESIAN_POINT ( 'NONE',  ( -0.7500000000000006661, 0.6083333333333564852, -1.299038105676652011 ) ) ;
#22988 = CARTESIAN_POINT ( 'NONE',  ( 6.751070424600909448, 9.963667031088037973, -1.199719254218441611 ) ) ;
#22989 = CARTESIAN_POINT ( 'NONE',  ( 1.364683531249986537, -0.3447916663252443836, -0.7879004041258309554 ) ) ;
#22990 = CARTESIAN_POINT ( 'NONE',  ( 0.1182595804350913826, -0.5859369620430117109, 2.142582832819041716 ) ) ;
#22992 = CARTESIAN_POINT ( 'NONE',  ( 5.881297811770386019, -0.04968318840743202180, 1.961410508136133712 ) ) ;
#22991 = AXIS2_PLACEMENT_3D ( 'NONE', #142719, #44131, #8401 ) ;
#22993 = CARTESIAN_POINT ( 'NONE',  ( 8.378575743565351175, 11.75846021992619406, -1.082531754730543083 ) ) ;
#22994 = CARTESIAN_POINT ( 'NONE',  ( -11.89942855770813956, 12.22000000000000064, -0.7000000000000009548 ) ) ;
#22995 = CARTESIAN_POINT ( 'NONE',  ( 6.292268727954291485, -2.250598158220047385, -0.2311834041341890578 ) ) ;
#22996 = CARTESIAN_POINT ( 'NONE',  ( -3.526529353330350336, 7.128384988945109413, -0.7216878364870458196 ) ) ;
#22997 = CARTESIAN_POINT ( 'NONE',  ( 3.016140967954855423, 2.052969616667064123, -0.1997095218184695709 ) ) ;
#22998 = CARTESIAN_POINT ( 'NONE',  ( -7.054319997812058318, 7.124461507069184130, 1.040834085586084257E-14 ) ) ;
#22999 = CARTESIAN_POINT ( 'NONE',  ( 0.7499999999999902300, 2.514583334016148974, 1.299038105676669330 ) ) ;
#23000 = CARTESIAN_POINT ( 'NONE',  ( 0.6823417656249917140, 5.655208333674749177, 1.181850606188765695 ) ) ;
#23001 = CARTESIAN_POINT ( 'NONE',  ( 4.446469999505775483, 0.4968273501132040026, 1.803309644091706021 ) ) ;
#23002 = CARTESIAN_POINT ( 'NONE',  ( 3.480872026922664286, -1.732388960670039113, -0.08070120533314528721 ) ) ;
#23003 = CARTESIAN_POINT ( 'NONE',  ( 3.702475415089864441, 1.494950309154385426, 0.8909294612347866682 ) ) ;
#23004 = CARTESIAN_POINT ( 'NONE',  ( 1.330038945030669995, 1.124775647945252643, -1.997386028781794387 ) ) ;
#23005 = CARTESIAN_POINT ( 'NONE',  ( -0.6823417656249969321, 3.780208333674754506, -1.181850606188749264 ) ) ;
#23006 = CARTESIAN_POINT ( 'NONE',  ( 4.194928683902748645, 1.680244682056671879, 1.243991948001839543 ) ) ;
#23007 = CARTESIAN_POINT ( 'NONE',  ( 6.193304230345664685, -0.6518728838521523627, 1.829399646200319252 ) ) ;
#23008 = CIRCLE ( 'NONE', #150924, 4.500000000000000000 ) ;
#23010 = ORIENTED_EDGE ( 'NONE', *, *, #135967, .T. ) ;
#23009 = CARTESIAN_POINT ( 'NONE',  ( -4.916039773278787273, 4.881957280557857715, 0.5603013081572870702 ) ) ;
#23011 = CARTESIAN_POINT ( 'NONE',  ( 0.8267963299631932994, 0.8146243292815741333, -1.844710905833810255 ) ) ;
#23012 = CARTESIAN_POINT ( 'NONE',  ( 0.5102161431939798986, -0.7575819503438313562, 1.980855387931411915 ) ) ;
#23013 = FACE_OUTER_BOUND ( 'NONE', #135708, .T. ) ;
#23014 = CARTESIAN_POINT ( 'NONE',  ( -3.129460678718345878, 6.444905630999884671, -0.7687999843507524744 ) ) ;
#23015 = CARTESIAN_POINT ( 'NONE',  ( -6.503107236049161521, 10.73870887536603291, 0.7998128361456481317 ) ) ;
#23016 = CARTESIAN_POINT ( 'NONE',  ( 6.662942426112080874, 9.860851032851066122, 1.199719254218460707 ) ) ;
#23017 = CARTESIAN_POINT ( 'NONE',  ( 2.192179715818479036, 1.306768369893403170, 1.669877806752372740 ) ) ;
#23018 = CARTESIAN_POINT ( 'NONE',  ( 1.154700538379228147, -4.295408888568413630, -1.734723475976807094E-15 ) ) ;
#23019 = CARTESIAN_POINT ( 'NONE',  ( 4.775911370473768791, 1.053640644303525331, 1.490772598166143048 ) ) ;
#23020 = EDGE_LOOP ( 'NONE', ( #22776, #65052, #109177, #14397 ) ) ;
#23021 = CARTESIAN_POINT ( 'NONE',  ( -3.648552735408990166, 6.310376387068841630, -1.082531754730546636 ) ) ;
#23022 = EDGE_CURVE ( 'NONE', #22085, #61771, #113523, .T. ) ;
#23023 = UNCERTAINTY_MEASURE_WITH_UNIT (LENGTH_MEASURE( 1.000000000000000082E-05 ), #88293, 'distance_accuracy_value', 'NONE');
#23024 = CARTESIAN_POINT ( 'NONE',  ( 2.273349394227877074, 5.683342515206170731, 0.4597581080974435519 ) ) ;
#23025 = CARTESIAN_POINT ( 'NONE',  ( -3.285556943750000514, -0.5760416661887087786, -1.896917185911906500 ) ) ;
#23026 = CARTESIAN_POINT ( 'NONE',  ( -5.845536785786364931, 9.971543350059432598, 0.000000000000000000 ) ) ;
#23027 = CARTESIAN_POINT ( 'NONE',  ( 2.461199802766162570, -1.676885983773316990, 1.125551603727361627 ) ) ;
#23028 = CARTESIAN_POINT ( 'NONE',  ( 5.790102700048295858, -0.9971039342967463748, 1.968745932239771568 ) ) ;
#23029 = CARTESIAN_POINT ( 'NONE',  ( -3.935609729716867289, 7.813571461303467913, 0.7998128361456352531 ) ) ;
#23030 = CARTESIAN_POINT ( 'NONE',  ( 3.309261503611124144, -1.518638105539332317, -1.075258281928012094 ) ) ;
#23031 = CARTESIAN_POINT ( 'NONE',  ( 10.55232363013785246, 11.20546574478267132, 0.000000000000000000 ) ) ;
#23032 = CARTESIAN_POINT ( 'NONE',  ( 4.407809338218622308, 8.156544971314787063, 0.000000000000000000 ) ) ;
#23033 = VERTEX_POINT ( 'NONE', #54790 ) ;
#23034 = CARTESIAN_POINT ( 'NONE',  ( -3.632695093457760649, 6.325562478087638496, -1.199719254218452047 ) ) ;
#23035 = CARTESIAN_POINT ( 'NONE',  ( -8.158255747121117452, 10.54105100977322174, 1.599625672291295375 ) ) ;
#23036 = CARTESIAN_POINT ( 'NONE',  ( 5.373610676068619973, 1.758448663713826132, -0.4906839848310071139 ) ) ;
#23038 = CARTESIAN_POINT ( 'NONE',  ( -3.976739547089790161, 7.847837856468413698, 0.08243740857501527519 ) ) ;
#23037 = CARTESIAN_POINT ( 'NONE',  ( -3.169574050544739841, 6.919863168935977527, -0.7998128361456481317 ) ) ;
#23039 = CARTESIAN_POINT ( 'NONE',  ( 6.304162555737000240, 6.968127521147626346, -0.9177210060461529206 ) ) ;
#23040 = CARTESIAN_POINT ( 'NONE',  ( 0.8601780606121096628, -0.6315397308106798224, 1.614934579331471998 ) ) ;
#23041 = CARTESIAN_POINT ( 'NONE',  ( 6.720655732516648939, 0.005566325962592238129, 1.826293863978686538 ) ) ;
#23042 = CARTESIAN_POINT ( 'NONE',  ( 6.024106105913028308, -1.276746162841462695, -1.922164112325924989 ) ) ;
#23043 = CARTESIAN_POINT ( 'NONE',  ( 5.564695703766185275, 5.456842840674144490, 0.000000000000000000 ) ) ;
#23044 = CARTESIAN_POINT ( 'NONE',  ( 0.4212572661226633985, -0.1035701926632242170, 2.058322702938982562 ) ) ;
#23045 = CARTESIAN_POINT ( 'NONE',  ( 6.602984505055297326, 7.662235663108029726, 1.199719254218462483 ) ) ;
#23046 = CARTESIAN_POINT ( 'NONE',  ( 6.098996632684510644, 1.141130774408656068, -1.995064312872560697 ) ) ;
#23047 = CARTESIAN_POINT ( 'NONE',  ( -2.900957617708239678, -3.232243495192087757, 1.542507481629953103 ) ) ;
#23048 = CARTESIAN_POINT ( 'NONE',  ( -6.947627372360122955, 7.070263120700404968, 0.000000000000000000 ) ) ;
#23049 = CARTESIAN_POINT ( 'NONE',  ( 5.875831987524620992, 1.115552982110395330, 1.501486808359139946 ) ) ;
#23051 = CARTESIAN_POINT ( 'NONE',  ( -3.363304624641834106, 6.081549941127532222, -1.199719254218452047 ) ) ;
#23050 = CARTESIAN_POINT ( 'NONE',  ( 4.060738401289211374, 0.5150538496448524572, 1.841637258418599155 ) ) ;
#23052 = CARTESIAN_POINT ( 'NONE',  ( 4.934293700819583073, 1.136511309699510308, -1.891595316245115788 ) ) ;
#23053 = CARTESIAN_POINT ( 'NONE',  ( 4.136029606254186142, 2.116781002543933088, -0.05581379417103624063 ) ) ;
#23054 = B_SPLINE_CURVE_WITH_KNOTS ( 'NONE', 3,
 ( #59456, #125614, #94123, #60517, #43236, #175364, #10692, #76763, #208886, #126678 ),
 .UNSPECIFIED., .F., .F.,
 ( 4, 3, 3, 4 ),
 ( 8.033417195976369988E-16, 3.125154781590810406E-05, 6.537904841941566522E-05, 9.952318552807673643E-05 ),
 .UNSPECIFIED. ) ;
#23055 = CARTESIAN_POINT ( 'NONE',  ( 0.6124999999999723999, 1.145833334016146843, 1.060881119635889380 ) ) ;
#23056 = CARTESIAN_POINT ( 'NONE',  ( 6.983263157960404754, 7.052265632007776119, 2.644342174942279744 ) ) ;
#23057 = CARTESIAN_POINT ( 'NONE',  ( 4.868786560638896255, 5.813244087901094481, 1.082531754730549078 ) ) ;
#23058 = CARTESIAN_POINT ( 'NONE',  ( -5.763624699140894592, 5.896852701852039580, -0.7216878364870338292 ) ) ;
#23059 = CARTESIAN_POINT ( 'NONE',  ( 5.496778590849229040, -2.068848325035842706, -0.4644329061709790429 ) ) ;
#23060 = ADVANCED_FACE ( 'NONE', ( #104618 ), #125884, .T. ) ;
#23061 = CARTESIAN_POINT ( 'NONE',  ( 2.468180027558197320, 2.263118346622743360, -0.4500467933809069176 ) ) ;
#23062 = CARTESIAN_POINT ( 'NONE',  ( 3.965250677406896962, 1.681448970545707855, 1.010551734412237446 ) ) ;
#23063 = CARTESIAN_POINT ( 'NONE',  ( 6.855650617048460127, -7.357813805523313988, 6.855650617048437923 ) ) ;
#23064 = CARTESIAN_POINT ( 'NONE',  ( 0.8484012048698870156, -1.946262134508335739, -0.2457884297097159831 ) ) ;
#23065 = CARTESIAN_POINT ( 'NONE',  ( 3.877268743828270470, 5.546566172598190292, 1.443375672974062551 ) ) ;
#23066 = CARTESIAN_POINT ( 'NONE',  ( 3.878514461961128479, 6.682628084666728085, -1.199719254218448494 ) ) ;
#23067 = ORIENTED_EDGE ( 'NONE', *, *, #84896, .F. ) ;
#23068 = CARTESIAN_POINT ( 'NONE',  ( 5.524625123954316486, 0.3981063221985549072, 1.976670730632006601 ) ) ;
#23069 = CARTESIAN_POINT ( 'NONE',  ( -8.971744963941075568, 11.49012176272984931, 1.599625672291269396 ) ) ;
#23070 = FACE_OUTER_BOUND ( 'NONE', #202158, .T. ) ;
#23071 = CARTESIAN_POINT ( 'NONE',  ( 10.50000000000000178, 0.000000000000000000, -3.600000000000002309 ) ) ;
#23072 = CARTESIAN_POINT ( 'NONE',  ( 3.327178260015594802, -2.004142704238300876, -0.8352945444606455494 ) ) ;
#23073 = DIRECTION ( 'NONE',  ( 0.000000000000000000, 1.000000000000000000, 0.000000000000000000 ) ) ;
#23074 = CARTESIAN_POINT ( 'NONE',  ( 0.5277791401020451856, -0.3051165123582540994, 2.098401203810342786 ) ) ;
#23075 = CARTESIAN_POINT ( 'NONE',  ( -1.402160292154681736E-14, 1.368750000682821710, -1.732050807568863648 ) ) ;
#23076 = SURFACE_SIDE_STYLE ('',( #107622 ) ) ;
#23077 = DIRECTION ( 'NONE',  ( -0.9989735196462988798, 0.000000000000000000, 0.04529798058948708572 ) ) ;
#23078 = CARTESIAN_POINT ( 'NONE',  ( 4.842126824027952026, 8.201492973507317430, 0.9351865777775794086 ) ) ;
#23079 = CARTESIAN_POINT ( 'NONE',  ( 0.9134385407369073340, -0.3049482027854091837, 2.037980195292460550 ) ) ;
#23081 = CARTESIAN_POINT ( 'NONE',  ( -3.701970883082869701, 7.364863713882350282, -2.499999999999995559 ) ) ;
#23080 = CARTESIAN_POINT ( 'NONE',  ( -10.34217224912604571, 10.96028913360221502, 0.7998128361456462443 ) ) ;
#23082 = CARTESIAN_POINT ( 'NONE',  ( -1.402160292154681736E-14, 1.196875000341419026, -1.575800808251659024 ) ) ;
#23083 = FACE_OUTER_BOUND ( 'NONE', #61280, .T. ) ;
#23084 = ORIENTED_EDGE ( 'NONE', *, *, #82890, .T. ) ;
#23085 = CARTESIAN_POINT ( 'NONE',  ( 2.859904825981678833, 0.6862549603197342085, -1.785085608301796523 ) ) ;
#23086 = CARTESIAN_POINT ( 'NONE',  ( 5.418734442855144273, 1.636401904928608042, 0.6746929113052438920 ) ) ;
#23087 = CARTESIAN_POINT ( 'NONE',  ( 6.387826650694035990, 7.481494509678370264, -1.199719254218452047 ) ) ;
#23088 = CARTESIAN_POINT ( 'NONE',  ( -3.093231602212184850, 6.760520635889515795, -0.7998128361456281477 ) ) ;
#23089 = CARTESIAN_POINT ( 'NONE',  ( 0.1229364404080907497, 1.576183056183463993, 0.8927909362536170512 ) ) ;
#23091 = CARTESIAN_POINT ( 'NONE',  ( 0.3916159773660661259, -1.906239802237769787, 0.1905982916604181676 ) ) ;
#23090 = CARTESIAN_POINT ( 'NONE',  ( 4.132297641190314508, 7.622816840561035256, -0.7610026044957002300 ) ) ;
#23092 = CARTESIAN_POINT ( 'NONE',  ( 2.523957353938070192, 2.030885678308389952, -0.4015143504868187718 ) ) ;
#23093 = CARTESIAN_POINT ( 'NONE',  ( 1.364683531249988757, 0.4468750003414206917, 0.000000000000000000 ) ) ;
#23094 = CARTESIAN_POINT ( 'NONE',  ( 6.244977087980838171, -1.579202250953464670, 1.002420361074819688 ) ) ;
#23095 = CARTESIAN_POINT ( 'NONE',  ( 2.894927146036041510, 1.565677646668685696, -0.9388022922067614795 ) ) ;
#23096 = ADVANCED_FACE ( 'NONE', ( #107877 ), #186561, .T. ) ;
#23098 = CARTESIAN_POINT ( 'NONE',  ( 5.638349000628050334, 7.351887578364292075, 1.232751772250343381 ) ) ;
#23097 = CARTESIAN_POINT ( 'NONE',  ( 6.217417563691929772, -0.2743312036321900460, 2.189694890431858276 ) ) ;
#23099 = CARTESIAN_POINT ( 'NONE',  ( -1.364683531250000748, 0.5093750003414208027, 0.000000000000000000 ) ) ;
#23100 = CARTESIAN_POINT ( 'NONE',  ( 4.545415624535277921, 1.843838458276589209, -0.9247144854665176883 ) ) ;
#23101 = CARTESIAN_POINT ( 'NONE',  ( -7.552055258011950656, 8.769484874890757453, 1.199719254218462483 ) ) ;
#23102 = CARTESIAN_POINT ( 'NONE',  ( 10.07778825365955733, 10.65184113889131012, -0.7998128361456281477 ) ) ;
#23103 = CARTESIAN_POINT ( 'NONE',  ( 3.845709127770629010, 7.638411082374393146, 0.7998128361456321445 ) ) ;
#23104 = CARTESIAN_POINT ( 'NONE',  ( 0.9136071317731933039, -0.3180670004044767740, 2.137961049616762921 ) ) ;
#23105 = STYLED_ITEM ( 'NONE', ( #52011 ), #197622 ) ;
#23106 = CARTESIAN_POINT ( 'NONE',  ( 6.443811375169310907, 1.424792453395683500, 1.502365266013883538 ) ) ;
#23107 = CARTESIAN_POINT ( 'NONE',  ( 1.364683531249988535, 1.426041667008083991, 0.7879004041258500513 ) ) ;
#23108 = CARTESIAN_POINT ( 'NONE',  ( 4.147864318636265146, 0.7325676050485959712, -2.033789780341701547 ) ) ;
#23109 = CARTESIAN_POINT ( 'NONE',  ( 4.547524150180999314, -1.845711718722802486, 0.8204608018674663938 ) ) ;
#23110 = DIRECTION ( 'NONE',  ( 0.000000000000000000, -1.000000000000000000, 0.000000000000000000 ) ) ;
#23113 = CARTESIAN_POINT ( 'NONE',  ( 5.666945020832167224, 8.594891043404107478, 1.082531754730558626 ) ) ;
#23112 = CARTESIAN_POINT ( 'NONE',  ( 0.000000000000000000, -0.08749999999999961975, -4.012584370867899430 ) ) ;
#23111 = CARTESIAN_POINT ( 'NONE',  ( 0.000000000000000000, 0.000000000000000000, 0.000000000000000000 ) ) ;
#23114 = CARTESIAN_POINT ( 'NONE',  ( -5.745623237141265882, 9.925253886631958622, 0.7998128361456291469 ) ) ;
#23115 = CARTESIAN_POINT ( 'NONE',  ( 2.079314900164643820, 1.561883299538204151, 1.275554356156020308 ) ) ;
#23117 = CARTESIAN_POINT ( 'NONE',  ( 0.6823417656249899377, 3.155208333674754062, 1.181850606188765695 ) ) ;
#23116 = CARTESIAN_POINT ( 'NONE',  ( -3.903858165731105778, 6.641919395739846799, 1.199719254218464037 ) ) ;
#23118 = DIRECTION ( 'NONE',  ( -0.9999655912483514930, 0.000000000000000000, 0.008295560218254021193 ) ) ;
#23119 = CARTESIAN_POINT ( 'NONE',  ( 5.730699431777452446, 1.279516236652695316, -1.421498520143074540 ) ) ;
#23120 = CARTESIAN_POINT ( 'NONE',  ( -11.89942855770813956, 12.30000000000000071, 0.6999999999999992895 ) ) ;
#23121 = CARTESIAN_POINT ( 'NONE',  ( 6.141480396866128899, 6.267408005873028820, -0.7216878364870257245 ) ) ;
#23123 = CARTESIAN_POINT ( 'NONE',  ( 4.165638788432171502, 1.319243065725501873, 1.525032742243138451 ) ) ;
#23122 = CARTESIAN_POINT ( 'NONE',  ( -7.443063143778079649, 10.66702885350765584, 1.082531754730549967 ) ) ;
#23124 = CARTESIAN_POINT ( 'NONE',  ( 0.7499999999999902300, 4.316666666666691299, -1.299038105676658228 ) ) ;
#23125 = CARTESIAN_POINT ( 'NONE',  ( -0.6823417656250039265, 14.63020833367473195, -1.181850606188755259 ) ) ;
#23126 = CARTESIAN_POINT ( 'NONE',  ( 6.282236785375785892, -0.9178991178065436518, 1.460045492214437246 ) ) ;
#23127 = CARTESIAN_POINT ( 'NONE',  ( 4.376249722160992839, 8.327651452488305850, 0.000000000000000000 ) ) ;
#23128 = CARTESIAN_POINT ( 'NONE',  ( 8.595506201384008449, 11.05117653974661529, 1.443375672974076540 ) ) ;
#23129 = CARTESIAN_POINT ( 'NONE',  ( 4.446469999505775483, 0.4968273501132040026, 1.803309644091706021 ) ) ;
#23130 = DIRECTION ( 'NONE',  ( 5.551115123125766062E-17, 0.000000000000000000, -1.000000000000000000 ) ) ;
#23131 = AXIS2_PLACEMENT_3D ( 'NONE', #23437, #88473, #24506 ) ;
#23132 = CARTESIAN_POINT ( 'NONE',  ( 2.061466481998303735, 1.718891244229248105, 1.153550331455879707 ) ) ;
#23133 = CARTESIAN_POINT ( 'NONE',  ( -8.041394506236766659, 8.554250810130591631, -0.7216878364870338292 ) ) ;
#23134 = ORIENTED_EDGE ( 'NONE', *, *, #6116, .F. ) ;
#23135 = CARTESIAN_POINT ( 'NONE',  ( 4.309512724297349884, 6.121127159803966933, 1.599625672291261402 ) ) ;
#23136 = CARTESIAN_POINT ( 'NONE',  ( 0.5269705342763851830, -1.727990693721896287, 1.039014695730144933 ) ) ;
#23137 = CARTESIAN_POINT ( 'NONE',  ( 1.617148605665112537, 1.507408818846365017, 1.004416837792695194 ) ) ;
#23138 = EDGE_CURVE ( 'NONE', #168364, #78193, #214187, .T. ) ;
#23139 = CARTESIAN_POINT ( 'NONE',  ( 4.217995187182920880, 6.974725914138481642, 1.082531754730549078 ) ) ;
#23140 = DIRECTION ( 'NONE',  ( -8.638326563840814399E-31, 0.000000000000000000, -1.000000000000000000 ) ) ;
#23141 = CIRCLE ( 'NONE', #203114, 0.09999999999999982514 ) ;
#23142 = CARTESIAN_POINT ( 'NONE',  ( 7.199016378732056687, 10.38230762762066384, -1.082531754730537976 ) ) ;
#23143 = ADVANCED_FACE ( 'NONE', ( #73146 ), #201678, .T. ) ;
#23144 = CARTESIAN_POINT ( 'NONE',  ( 7.401861798056875053, 10.72292363345333399, -1.199719254218441611 ) ) ;
#23146 = CARTESIAN_POINT ( 'NONE',  ( 6.398046686924231174, -0.9077857338794625974, -1.686868998638735073 ) ) ;
#23145 = CARTESIAN_POINT ( 'NONE',  ( -5.194745412330402878, 9.212286747694129474, 0.000000000000000000 ) ) ;
#23147 = FACE_OUTER_BOUND ( 'NONE', #54163, .T. ) ;
#23148 = CARTESIAN_POINT ( 'NONE',  ( -1.580000000000022276, 8.758163473637745611, 2.500000000000011102 ) ) ;
#23149 = CARTESIAN_POINT ( 'NONE',  ( 6.954969613686092345, 7.216478758829655504, -0.7216878364870257245 ) ) ;
#23150 = CARTESIAN_POINT ( 'NONE',  ( -10.99970480893082403, -6.221252899067775566, -0.08058608058607830138 ) ) ;
#23152 = VERTEX_POINT ( 'NONE', #82762 ) ;
#23151 = CARTESIAN_POINT ( 'NONE',  ( 3.212919216758630014, 6.692230152952963529, 0.000000000000000000 ) ) ;
#23153 = CARTESIAN_POINT ( 'NONE',  ( -6.561783159334121152, 10.59923808595773664, -0.7216878364870278340 ) ) ;
#23154 = CIRCLE ( 'NONE', #36941, 9.499999999999992895 ) ;
#23155 = CARTESIAN_POINT ( 'NONE',  ( 3.538091169922503276, 0.9737216987566952309, -1.930062384640649054 ) ) ;
#23156 = CARTESIAN_POINT ( 'NONE',  ( -6.238160076063538284, 9.331584951165851294, 1.082531754730549967 ) ) ;
#23157 = EDGE_CURVE ( 'NONE', #14896, #157191, #75824, .T. ) ;
#23158 = CARTESIAN_POINT ( 'NONE',  ( 6.536439455564164724, 7.758839131980592718, 1.082531754730549967 ) ) ;
#23159 = CARTESIAN_POINT ( 'NONE',  ( 0.3344391967911933272, -1.139684030083350841, -1.788147294700337397 ) ) ;
#23160 = CARTESIAN_POINT ( 'NONE',  ( 6.352569596097208837, 0.5757234290239590102, 1.732508359437078482 ) ) ;
#23161 = CARTESIAN_POINT ( 'NONE',  ( 2.583225839741074115, 1.803852637447726392, -0.7955871043755156080 ) ) ;
#23162 = CARTESIAN_POINT ( 'NONE',  ( 4.517770118113122457, -0.5046507728132009207, 1.844564425022446885 ) ) ;
#23163 = CARTESIAN_POINT ( 'NONE',  ( -8.150368799117956087, 14.48038083418904698, -8.818837747985245556 ) ) ;
#23164 = CARTESIAN_POINT ( 'NONE',  ( 5.090277013941287620, 1.014100869069594291, -1.688273828314874825 ) ) ;
#23165 = CARTESIAN_POINT ( 'NONE',  ( 0.07597880344310371792, -1.883441279811811642, -0.4727451468593062422 ) ) ;
#23166 = VERTEX_POINT ( 'NONE', #102216 ) ;
#23167 = CARTESIAN_POINT ( 'NONE',  ( -3.949167883330528372, 7.829389307186077396, 1.214306433183764966E-14 ) ) ;
#23169 = CARTESIAN_POINT ( 'NONE',  ( 6.796618584847125000, -7.026643280347811604, -6.776593369755265606 ) ) ;
#23168 = CARTESIAN_POINT ( 'NONE',  ( -3.959863383643135393, 6.777535159962392086, 1.199719254218452935 ) ) ;
#23171 = CARTESIAN_POINT ( 'NONE',  ( 5.302647476276220573, 8.240153584747313076, -1.082531754730548412 ) ) ;
#23170 = CARTESIAN_POINT ( 'NONE',  ( 8.294891053462476904, 8.571794405328034827, 1.040834085586084257E-14 ) ) ;
#23173 = ORIENTED_EDGE ( 'NONE', *, *, #55279, .F. ) ;
#23172 = CARTESIAN_POINT ( 'NONE',  ( 4.811142580195256535, 1.587781804131962682, -1.065416552848017284 ) ) ;
#23174 = CARTESIAN_POINT ( 'NONE',  ( 0.6927435329204565395, -2.190372518412486702, -0.2681103625320201411 ) ) ;
#23175 = CARTESIAN_POINT ( 'NONE',  ( 7.547231044119296683, -5.251137252134833844, 7.967649405165770915 ) ) ;
#23176 = CARTESIAN_POINT ( 'NONE',  ( 6.621754286443582771, -0.4424289334611238300, 1.971349943050800801 ) ) ;
#23177 = CARTESIAN_POINT ( 'NONE',  ( 10.98194350564910415, -7.666862915010147717, -0.6300133639306100264 ) ) ;
#23178 = DIRECTION ( 'NONE',  ( 0.000000000000000000, 0.000000000000000000, -1.000000000000000000 ) ) ;
#23179 = CARTESIAN_POINT ( 'NONE',  ( 2.031770498437397876, 1.981864486777328294, -0.5989037013024376410 ) ) ;
#23180 = CARTESIAN_POINT ( 'NONE',  ( -6.925517538482230506, 6.974191971184389160, 0.7998128361456341429 ) ) ;
#23181 = CARTESIAN_POINT ( 'NONE',  ( -4.646665375593996394, 8.329970469126573462, 0.4085986083085801912 ) ) ;
#23183 = CARTESIAN_POINT ( 'NONE',  ( 0.4444780689869810564, 2.156031605563761833, 0.1575401717312311101 ) ) ;
#23182 = CARTESIAN_POINT ( 'NONE',  ( -5.766295404513795297, 5.621766148221195358, 0.7998128361456341429 ) ) ;
#23184 = CARTESIAN_POINT ( 'NONE',  ( -15.75000000000000000, 10.89999999999998259, 1.399999999999998579 ) ) ;
#23185 = CARTESIAN_POINT ( 'NONE',  ( 3.580761967785000888, 7.191656372475549119, -0.7216878364870338292 ) ) ;
#23186 = CARTESIAN_POINT ( 'NONE',  ( 0.01424860406314341042, -7.025535116234668642, 9.597801448741886787 ) ) ;
#23187 = CARTESIAN_POINT ( 'NONE',  ( -0.6823417656250003738, 12.46354166700806765, 1.181850606188754593 ) ) ;
#23189 = CARTESIAN_POINT ( 'NONE',  ( -5.257529707049291900, 9.355811434857983500, 0.7998128361456291469 ) ) ;
#23188 = CARTESIAN_POINT ( 'NONE',  ( -0.02319159430947624612, 7.629137130509076492, -2.410989586153564623 ) ) ;
#23190 = CARTESIAN_POINT ( 'NONE',  ( 4.641094080744356809, 0.6698209448141523303, 1.599790421982680400 ) ) ;
#23191 = CARTESIAN_POINT ( 'NONE',  ( -3.684065054611367351, 5.321161868511784299, -1.599625672291256295 ) ) ;
#23192 = CARTESIAN_POINT ( 'NONE',  ( 2.694261129275489886, 0.9798316074655871732, -1.823736424811234658 ) ) ;
#23193 =( BOUNDED_CURVE ( )  B_SPLINE_CURVE ( 3, ( #6321, #138495, #201314, #106034 ),
 .UNSPECIFIED., .F., .T. ) 
 B_SPLINE_CURVE_WITH_KNOTS ( ( 4, 4 ),
 ( 1.430804639040423654, 1.438015327900961982 ),
 .UNSPECIFIED. ) 
 CURVE ( )  GEOMETRIC_REPRESENTATION_ITEM ( )  RATIONAL_B_SPLINE_CURVE ( ( 1.000000000000000000, 0.9999956671685397147, 0.9999956671685397147, 1.000000000000000000 ) ) 
 REPRESENTATION_ITEM ( '' )  );
#23194 = CARTESIAN_POINT ( 'NONE',  ( 4.956716356600668227, -1.994036693836033658, -0.7120731657841266049 ) ) ;
#23195 = CARTESIAN_POINT ( 'NONE',  ( 7.613066949273408213, 8.840665181362512115, -1.199719254218441611 ) ) ;
#23197 = ADVANCED_FACE ( 'NONE', ( #164038 ), #208646, .T. ) ;
#23196 = CARTESIAN_POINT ( 'NONE',  ( -1.364683531250012516, 3.530208333674758059, 0.7879004041258379498 ) ) ;
#23198 = CARTESIAN_POINT ( 'NONE',  ( 2.078894642590666031, 1.835759051837970945, 0.7136754054878727827 ) ) ;
#23199 = CARTESIAN_POINT ( 'NONE',  ( 6.114332400817464652, 6.016105027659348181, -0.05221600309115309591 ) ) ;
#23200 = CARTESIAN_POINT ( 'NONE',  ( -0.2049973002360427898, -0.1418364932926942379, -1.881151990943498387 ) ) ;
#23201 = CARTESIAN_POINT ( 'NONE',  ( 4.382983890270373273, 2.048579214610211530, -1.028644635605566959 ) ) ;
#23202 = CARTESIAN_POINT ( 'NONE',  ( 1.312830284664792790, 1.609138963534262778, 0.8624270714618911260 ) ) ;
#23203 = ADVANCED_FACE ( 'NONE', ( #3611 ), #72444, .T. ) ;
#23204 = CARTESIAN_POINT ( 'NONE',  ( 6.391743074199808916, 6.421731439513382433, -0.7998128361456481317 ) ) ;
#23205 = CARTESIAN_POINT ( 'NONE',  ( 5.626270559546821204, 6.626699076635176766, 1.082531754730560403 ) ) ;
#23206 = CARTESIAN_POINT ( 'NONE',  ( -7.320512876374914768, 10.62801655815766999, 1.199719254218453823 ) ) ;
#23207 = CARTESIAN_POINT ( 'NONE',  ( 3.269792347016476697, 0.4849277011088357070, -1.953833955329455696 ) ) ;
#23208 =( BOUNDED_CURVE ( )  B_SPLINE_CURVE ( 3, ( #87851, #23894, #55348, #138747 ),
 .UNSPECIFIED., .F., .T. ) 
 B_SPLINE_CURVE_WITH_KNOTS ( ( 4, 4 ),
 ( 0.4999999999999992784, 1.000000000000000000 ),
 .UNSPECIFIED. ) 
 CURVE ( )  GEOMETRIC_REPRESENTATION_ITEM ( )  RATIONAL_B_SPLINE_CURVE ( ( 1.000000000000000888, 0.3333333333333333148, 0.3333333333333323711, 1.000000000000000000 ) ) 
 REPRESENTATION_ITEM ( '' )  );
#23209 = CARTESIAN_POINT ( 'NONE',  ( 3.432423435979839343, -1.172226468724973936, 1.572839002276872566 ) ) ;
#23210 = CARTESIAN_POINT ( 'NONE',  ( -7.751511138711140170, 10.06651563329490529, -1.599625672291263179 ) ) ;
#23211 = CARTESIAN_POINT ( 'NONE',  ( -7.009729113465285266, 8.136771039586342624, -1.199719254218446718 ) ) ;
#23212 = CYLINDRICAL_SURFACE ( 'NONE', #175138, 0.08000000000000020983 ) ;
#23214 = CARTESIAN_POINT ( 'NONE',  ( 4.697990591988738807, -1.769527177957382680, -0.04185004791794690038 ) ) ;
#23213 = CARTESIAN_POINT ( 'NONE',  ( 6.509723796436136745, -0.9841294377065135102, -1.844520550012812565 ) ) ;
#23215 = CARTESIAN_POINT ( 'NONE',  ( 4.901740149399201663, 4.849955969763177777, 0.6350953998956505586 ) ) ;
#23216 = CARTESIAN_POINT ( 'NONE',  ( 0.8850414913617115076, 1.931072968267994794, -1.036053359626129877 ) ) ;
#23217 = CARTESIAN_POINT ( 'NONE',  ( 5.683501733545419654, -0.7767583057271000291, 1.557453612149447775 ) ) ;
#23218 = CARTESIAN_POINT ( 'NONE',  ( 8.372323551638698902, 9.726464550788689323, 1.199719254218462483 ) ) ;
#23219 = CARTESIAN_POINT ( 'NONE',  ( -10.62873463776380056, 11.29999999999999893, -3.200000000000001510 ) ) ;
#23220 = CARTESIAN_POINT ( 'NONE',  ( 6.311202115008078373, 1.327223183623595704, -1.876690649992603044 ) ) ;
#23221 =( BOUNDED_SURFACE ( )  B_SPLINE_SURFACE ( 3, 2, ( 
 ( #199504, #51147, #117271 ),
 ( #184326, #19698, #189667 ),
 ( #106347, #25031, #172369 ),
 ( #39164, #42388, #59671 ),
 ( #7706, #91131, #107426 ),
 ( #143105, #76979, #23959 ) ),
 .UNSPECIFIED., .F., .F., .F. ) 
 B_SPLINE_SURFACE_WITH_KNOTS ( ( 4, 2, 4 ),
 ( 3, 3 ),
 ( 0.000000000000000000, 0.0003831327362561333209, 0.0007662654725122666419 ),
 ( 0.000000000000000000, 1.000000000000000000 ),
 .UNSPECIFIED. ) 
 GEOMETRIC_REPRESENTATION_ITEM ( )  RATIONAL_B_SPLINE_SURFACE ( (
 ( 1.000000000000000000, 0.5879095031487548972, 1.000000000000000000),
 ( 1.000000000000000000, 0.5873691247580630215, 1.000000000000000000),
 ( 1.000000000000000000, 0.6054349545494872586, 1.000000000000000000),
 ( 1.000000000000000000, 0.6533334602768978705, 1.000000000000000000),
 ( 1.000000000000000000, 0.6828746263149312323, 1.000000000000000000),
 ( 1.000000000000000000, 0.7071067811865475727, 1.000000000000000000) ) ) 
 REPRESENTATION_ITEM ( '' )  SURFACE ( )  );
#23222 = CARTESIAN_POINT ( 'NONE',  ( -3.475000000000000533, -1.356249999044083943, 0.000000000000000000 ) ) ;
#23223 = CARTESIAN_POINT ( 'NONE',  ( 5.202368031388965974, -1.227288160380139548, -1.225006654371106452 ) ) ;
#23224 = CARTESIAN_POINT ( 'NONE',  ( 1.787996309160574837, 1.523479866092191548, 1.596893430481533649 ) ) ;
#23225 = DIRECTION ( 'NONE',  ( -0.7613463080411786432, 0.000000000000000000, -0.6483454320283800199 ) ) ;
#23226 = CARTESIAN_POINT ( 'NONE',  ( 5.881339278728036746, -0.05926448915108929044, 2.170540009233146606 ) ) ;
#23227 = CARTESIAN_POINT ( 'NONE',  ( -0.4356160240586524068, -9.063431457505059186, 9.626717610576628559 ) ) ;
#23228 = CARTESIAN_POINT ( 'NONE',  ( 0.6907973960054912821, 1.599150545848356364, -1.387813827701115610 ) ) ;
#23229 = CARTESIAN_POINT ( 'NONE',  ( 2.718750000000001332, -0.7852924748298429902, 1.895863743164144744 ) ) ;
#23230 = CARTESIAN_POINT ( 'NONE',  ( 6.727182134110181622, 6.034673098952469950, 2.683942742083842425 ) ) ;
#23231 = CARTESIAN_POINT ( 'NONE',  ( 4.840804290916858932, 0.3290424097142484738, 1.897927756555679801 ) ) ;
#23232 = CARTESIAN_POINT ( 'NONE',  ( 1.243189324034719823, 2.142110494306264101, 0.5876511989056328877 ) ) ;
#23233 = ORIENTED_EDGE ( 'NONE', *, *, #77263, .F. ) ;
#23235 = CARTESIAN_POINT ( 'NONE',  ( -0.7499999999999972244, 4.358333333333352932, -1.299038105676652011 ) ) ;
#23234 = CARTESIAN_POINT ( 'NONE',  ( 1.277341847617214476, 2.115720621435190907, -0.8829085993839781432 ) ) ;
#23236 = CARTESIAN_POINT ( 'NONE',  ( 5.522248639467795428, 5.337044922334209573, -0.7998128361456231517 ) ) ;
#23237 = CARTESIAN_POINT ( 'NONE',  ( 6.063521013809720195, 8.097193820909906137, 1.599625672291281386 ) ) ;
#23238 = CARTESIAN_POINT ( 'NONE',  ( 4.231244787023562992, 2.030907777374240997, 0.9001406952713184584 ) ) ;
#23239 = CARTESIAN_POINT ( 'NONE',  ( -7.199016379176422120, 11.34267684244042584, 0.000000000000000000 ) ) ;
#23240 = CARTESIAN_POINT ( 'NONE',  ( 6.887178846062110615, 9.058127958537705027, -1.443375672974057666 ) ) ;
#23241 = CARTESIAN_POINT ( 'NONE',  ( -9.788623718942277563, 10.52240854829523187, 1.040834085586084257E-14 ) ) ;
#23242 = CARTESIAN_POINT ( 'NONE',  ( 6.455090533882185788, 8.624301270986276080, -1.443375672974078761 ) ) ;
#23243 = ORIENTED_EDGE ( 'NONE', *, *, #127684, .T. ) ;
#23244 = CARTESIAN_POINT ( 'NONE',  ( 2.215470409936692420, 1.956561601830292485, 0.4872017847364697452 ) ) ;
#23246 = CARTESIAN_POINT ( 'NONE',  ( 6.180145878880094479, -1.142753862412404509, -1.717008129757614077 ) ) ;
#23245 = CARTESIAN_POINT ( 'NONE',  ( 8.749089199520284410, 9.101692242395490240, 0.7998128361456481317 ) ) ;
#23247 = CARTESIAN_POINT ( 'NONE',  ( -11.33772463945037146, 10.89999999999998259, 3.599999999999999201 ) ) ;
#23248 = CARTESIAN_POINT ( 'NONE',  ( 5.668717623845194176, 9.627604637879139560, 0.000000000000000000 ) ) ;
#23249 = CARTESIAN_POINT ( 'NONE',  ( 6.269106929289325336, 1.662610211318481301, -0.5146825814001282362 ) ) ;
#23250 = CARTESIAN_POINT ( 'NONE',  ( -0.6823417656250003738, 1.967708333674753174, -1.181850606188749264 ) ) ;
#23251 = CARTESIAN_POINT ( 'NONE',  ( 1.159032429170350653, 0.3524738178620877571, -1.734097463706934183 ) ) ;
#23252 = CARTESIAN_POINT ( 'NONE',  ( 0.7213275451133926985, 1.987047012402185731, 0.3419330716275259530 ) ) ;
#23253 = CARTESIAN_POINT ( 'NONE',  ( 6.532745107981281940, -1.550057735787165214, 0.7916670675358824516 ) ) ;
#23254 = CARTESIAN_POINT ( 'NONE',  ( 4.493851497812589635, -2.291808737193799406, -0.05710960328321466883 ) ) ;
#23255 = CARTESIAN_POINT ( 'NONE',  ( 3.099365256270599112, -1.839010575856118823, 0.09107247011905240941 ) ) ;
#23256 = CARTESIAN_POINT ( 'NONE',  ( 7.639129486296027061, 10.99973593639901814, 1.199719254218460707 ) ) ;
#23257 = CARTESIAN_POINT ( 'NONE',  ( 9.412584077552686779, 11.54679772643938307, 7.460083846873735602 ) ) ;
#23258 = CARTESIAN_POINT ( 'NONE',  ( 2.643341535394112984, -1.351257319430071657, -1.227710988083303478 ) ) ;
#23259 = CARTESIAN_POINT ( 'NONE',  ( 4.043592392309851569, -1.492256208629010761, 1.356298961253152413 ) ) ;
#23260 = CARTESIAN_POINT ( 'NONE',  ( -8.306341666666730461, 12.84248237775322643, 1.040834085586084257E-14 ) ) ;
#23262 = CARTESIAN_POINT ( 'NONE',  ( 8.305220197644215929, 14.86737089724833893, -9.585679967850639471 ) ) ;
#23261 = CARTESIAN_POINT ( 'NONE',  ( 3.204270770158343939, -2.259979215032235977, 0.1094169825565076415 ) ) ;
#23263 = CARTESIAN_POINT ( 'NONE',  ( 5.315496758875870142, -0.3119175628578441661, 2.082610458907033557 ) ) ;
#23264 = CARTESIAN_POINT ( 'NONE',  ( 9.216403166322994167, 13.91905933883010249, 6.904314279704210300 ) ) ;
#23265 = CARTESIAN_POINT ( 'NONE',  ( 4.105968538015460467, 0.7004154448949986289, -1.948405661837959713 ) ) ;
#23266 = CARTESIAN_POINT ( 'NONE',  ( 3.891353782322113375, 4.498666486585943147, -1.199719254218446718 ) ) ;
#23267 = CARTESIAN_POINT ( 'NONE',  ( -0.6801582343750438575, 0.6302083336747199560, -1.178068619123869398 ) ) ;
#23268 = CARTESIAN_POINT ( 'NONE',  ( 5.303433364654349447, 1.869980213031800398, -0.9998494819224086338 ) ) ;
#23269 = APPLICATION_PROTOCOL_DEFINITION ( 'draft international standard', 'automotive_design', 1998, #132313 ) ;
#23271 = CARTESIAN_POINT ( 'NONE',  ( 1.049297559255836010, -1.518254527582623359, -1.185787014772927916 ) ) ;
#23270 = CARTESIAN_POINT ( 'NONE',  ( -7.804689982961090955, 12.25722208009664094, 0.7998128361456481317 ) ) ;
#23272 = UNCERTAINTY_MEASURE_WITH_UNIT (LENGTH_MEASURE( 1.000000000000000082E-05 ), #80900, 'distance_accuracy_value', 'NONE');
#23273 = CARTESIAN_POINT ( 'NONE',  ( -5.191846479390389568, 5.021852078902356631, 0.7998128361456281477 ) ) ;
#23274 = CARTESIAN_POINT ( 'NONE',  ( 7.584896871841365851, 10.93646455286856956, -1.199719254218446718 ) ) ;
#23275 = CARTESIAN_POINT ( 'NONE',  ( 5.411112705185558092, 6.445957923205511086, -1.082531754730548412 ) ) ;
#23276 = CARTESIAN_POINT ( 'NONE',  ( 5.681948419994366617, 6.106813310819505070, 0.7427411415691799190 ) ) ;
#23277 = CARTESIAN_POINT ( 'NONE',  ( 1.500000000000053291, 7.750000000000000000, 15.74999999999999289 ) ) ;
#23278 = CARTESIAN_POINT ( 'NONE',  ( -4.253507506385335368, 5.985511395581417204, 1.599625672291267398 ) ) ;
#23279 = CARTESIAN_POINT ( 'NONE',  ( 0.5279477311770188752, -0.3182371573221299266, 2.198381937975202760 ) ) ;
#23280 = CARTESIAN_POINT ( 'NONE',  ( 2.133940825901488481, -1.375048162780323935, -1.595187971101755364 ) ) ;
#23281 = CARTESIAN_POINT ( 'NONE',  ( -4.167152111353897403, 5.955039778036558040, 1.599625672291270506 ) ) ;
#23282 = CARTESIAN_POINT ( 'NONE',  ( 9.237182729612253951, 9.671134694169463586, 0.7998128361456462443 ) ) ;
#23283 = CARTESIAN_POINT ( 'NONE',  ( 6.526204204079649962, 0.9558936715202811518, 1.596491800297286545 ) ) ;
#23284 = CARTESIAN_POINT ( 'NONE',  ( 6.588372581236919601, 9.773852880496709972, -1.199719254218440723 ) ) ;
#23285 = DIRECTION ( 'NONE',  ( 0.000000000000000000, 1.000000000000000000, 0.000000000000000000 ) ) ;
#23286 = CARTESIAN_POINT ( 'NONE',  ( -6.780486220610186798, 8.043560357867583832, -1.082531754730549967 ) ) ;
#23288 = CARTESIAN_POINT ( 'NONE',  ( -9.680158490477310806, 10.39586578175276266, 0.7216878364870438212 ) ) ;
#23287 = VECTOR ( 'NONE', #113715, 1000.000000000000000 ) ;
#23289 =( BOUNDED_CURVE ( )  B_SPLINE_CURVE ( 2, ( #183035, #181960, #99661, #66058, #115971, #114909, #192071, #148426, #33589 ),
 .UNSPECIFIED., .F., .T. ) 
 B_SPLINE_CURVE_WITH_KNOTS ( ( 3, 2, 2, 2, 3 ),
 ( 0.6041666666666667407, 0.6111111111111111605, 0.6250000000000000000, 0.6388888888888888395, 0.6458333333333333703 ),
 .UNSPECIFIED. ) 
 CURVE ( )  GEOMETRIC_REPRESENTATION_ITEM ( )  RATIONAL_B_SPLINE_CURVE ( ( 0.9330127018922192983, 0.9330127018922198534, 1.000000000000000000, 0.8660254037844387076, 1.000000000000000000, 0.8660254037844387076, 1.000000000000000000, 0.9330127018922187432, 0.9330127018922192983 ) ) 
 REPRESENTATION_ITEM ( '' )  );
#23290 = CARTESIAN_POINT ( 'NONE',  ( 0.2465380642357860586, 1.084720387836759725, -1.822023332652397354 ) ) ;
#23291 = CARTESIAN_POINT ( 'NONE',  ( -7.208094944320834863, 8.438474185576302133, -1.199719254218452047 ) ) ;
#23293 = CARTESIAN_POINT ( 'NONE',  ( 3.297265573180406584, -1.731424309613574852, 0.9225008839797432802 ) ) ;
#23292 = CARTESIAN_POINT ( 'NONE',  ( 0.6124999999999846123, -0.08333333333329639991, -1.060881119635962211 ) ) ;
#23294 = CARTESIAN_POINT ( 'NONE',  ( 1.657319961134783748, -1.854130675604428902, -1.111159678259740602 ) ) ;
#23295 = CARTESIAN_POINT ( 'NONE',  ( 1.083273795380396143, -0.8277460070302902206, 1.644747122058511035 ) ) ;
#23297 = CARTESIAN_POINT ( 'NONE',  ( -5.219871119622601086, 6.450327202623305389, -1.173442693870077935 ) ) ;
#23296 = CARTESIAN_POINT ( 'NONE',  ( -5.472651281771599763, 6.413789912602166687, 1.199719254218452935 ) ) ;
#23298 = CARTESIAN_POINT ( 'NONE',  ( 3.257457426684560620, 0.7833967258410595713, 1.554110229252920528 ) ) ;
#23299 = CARTESIAN_POINT ( 'NONE',  ( 6.236387472606139681, 8.298871356172400127, -1.443375672974057666 ) ) ;
#23300 = CARTESIAN_POINT ( 'NONE',  ( -10.85762644215163775, 5.701980886241464042, -6.452002860825420960 ) ) ;
#23301 = VECTOR ( 'NONE', #2328, 1000.000000000000000 ) ;
#23302 = CARTESIAN_POINT ( 'NONE',  ( 1.253037233087474611, -1.703760181015579134, 1.330383891403746688 ) ) ;
#23303 = CARTESIAN_POINT ( 'NONE',  ( 2.266953675890924558, -2.015725231744563306, 0.04666741021024794350 ) ) ;
#23304 = DIRECTION ( 'NONE',  ( 0.000000000000000000, 8.546850786086437571E-32, 1.000000000000000000 ) ) ;
#23305 = CARTESIAN_POINT ( 'NONE',  ( 0.1984014031938194922, -2.161264429664040421, -0.05129915172277095536 ) ) ;
#23306 = CARTESIAN_POINT ( 'NONE',  ( 2.342595614570395668, 0.4301288016448929774, 1.923825502367804141 ) ) ;
#23307 = CARTESIAN_POINT ( 'NONE',  ( 6.609000000000009756, 0.005669918681722520802, 1.900160851458796873 ) ) ;
#23308 = CARTESIAN_POINT ( 'NONE',  ( 2.067823894287325714, -1.192992258377950865, 1.532381367046357523 ) ) ;
#23311 = ORIENTED_EDGE ( 'NONE', *, *, #85916, .T. ) ;
#23310 = CARTESIAN_POINT ( 'NONE',  ( -4.611181642423629157, 7.433443445252599702, 1.082531754730549967 ) ) ;
#23309 = PRESENTATION_STYLE_ASSIGNMENT (( #55831 ) ) ;
#23312 = AXIS2_PLACEMENT_3D ( 'NONE', #29126, #129909, #179649 ) ;
#23313 = CARTESIAN_POINT ( 'NONE',  ( -4.706088717274938382, 6.583799151611112954, 1.443375672974058777 ) ) ;
#23314 = CARTESIAN_POINT ( 'NONE',  ( -0.1110810684432986112, 0.002541288824218449188, -1.796853612742685513 ) ) ;
#23315 = CARTESIAN_POINT ( 'NONE',  ( 4.278479993564246797, 7.149254538203735798, 1.199719254218452047 ) ) ;
#23316 = CARTESIAN_POINT ( 'NONE',  ( -4.633854640820660009, 8.628190524257904670, -0.7998128361456362523 ) ) ;
#23317 = CARTESIAN_POINT ( 'NONE',  ( -6.095272577795516789, 9.268845886473535245, 1.199719254218452047 ) ) ;
#23318 = CARTESIAN_POINT ( 'NONE',  ( -9.612367721964606204, 12.23751498042398289, -1.443375672974058777 ) ) ;
#23319 = CARTESIAN_POINT ( 'NONE',  ( 6.124106107054944736, -1.275020473110911157, -1.923184551904693507 ) ) ;
#23320 = DIRECTION ( 'NONE',  ( 0.9829311923673916818, -0.1839735607939843032, 0.000000000000000000 ) ) ;
#23321 = CARTESIAN_POINT ( 'NONE',  ( 3.625789200213443753, 1.914935786268581852, -0.4253726038727227432 ) ) ;
#23322 = CARTESIAN_POINT ( 'NONE',  ( 9.108380270282433244, 9.520865158284665952, 1.040834085586084257E-14 ) ) ;
#23323 = CARTESIAN_POINT ( 'NONE',  ( 0.4576579978108759050, -1.899619568183811058, -0.6767110947205197125 ) ) ;
#23324 = VERTEX_POINT ( 'NONE', #141169 ) ;
#23325 = CARTESIAN_POINT ( 'NONE',  ( 1.815762809344774187, -1.387149605378830586, -1.599721994570136197 ) ) ;
#23326 = CARTESIAN_POINT ( 'NONE',  ( 1.499999999999987121, 1.827083334016151861, -0.8660254037844253849 ) ) ;
#23327 = CARTESIAN_POINT ( 'NONE',  ( -7.366157530926372488, 7.488271962369228874, -0.7998128361456291469 ) ) ;
#23328 = CARTESIAN_POINT ( 'NONE',  ( 3.398233898566359823, 1.450718870894672330, -1.133551952132209717 ) ) ;
#23329 = ORIENTED_EDGE ( 'NONE', *, *, #117424, .T. ) ;
#23330 = CARTESIAN_POINT ( 'NONE',  ( -8.296699936558862731, 11.76690146170562201, 1.199719254218453823 ) ) ;
#23331 = CARTESIAN_POINT ( 'NONE',  ( 3.902672080109194752, -2.098000727953463151, -0.3078000538283761078 ) ) ;
#23332 = CARTESIAN_POINT ( 'NONE',  ( 0.3922017905241963476, 1.532332584989907653, -1.020347975915262939 ) ) ;
#23333 = CARTESIAN_POINT ( 'NONE',  ( -1.201851678989727383E-14, 5.368750000682816825, -1.732050807568863648 ) ) ;
#23334 = CARTESIAN_POINT ( 'NONE',  ( 5.829115978871627135, 8.888053511070525659, 1.199719254218462483 ) ) ;
#23335 = CARTESIAN_POINT ( 'NONE',  ( 7.472478939787284169, 8.746922180287201698, 1.199719254218452935 ) ) ;
#23336 = CARTESIAN_POINT ( 'NONE',  ( 4.429017379523855880, 0.09708327650245980600, 2.058604088861961667 ) ) ;
#23338 = CARTESIAN_POINT ( 'NONE',  ( 1.452429406588066740, -1.579491434881035827, -0.9459884711465746943 ) ) ;
#23337 = CARTESIAN_POINT ( 'NONE',  ( -7.660520486921249983, 8.896027641951645748, -1.199719254218446718 ) ) ;
#23339 = CARTESIAN_POINT ( 'NONE',  ( 0.6823417656249917140, 5.092708333674749177, 1.181850606188765695 ) ) ;
#23340 = FACE_BOUND ( 'NONE', #173290, .T. ) ;
#23341 = CARTESIAN_POINT ( 'NONE',  ( -9.499633409936905082, -9.910600865424404660, 0.08345703571627748063 ) ) ;
#23342 = CARTESIAN_POINT ( 'NONE',  ( 10.99931799034184365, -8.075210796978272043, -0.1485693272543584520 ) ) ;
#23343 = CARTESIAN_POINT ( 'NONE',  ( 0.8739773845415178544, 2.125910683164092152, -0.5920798734769525673 ) ) ;
#23344 = CARTESIAN_POINT ( 'NONE',  ( 3.638171750181828035, 1.021205778115843010, -2.018914226005202206 ) ) ;
#23345 = CARTESIAN_POINT ( 'NONE',  ( -8.839552966430023417, 9.415159337030921449, -0.7216878364870267237 ) ) ;
#23346 = CARTESIAN_POINT ( 'NONE',  ( 3.937629537800376500, -1.731762593766679403, 0.5317277010480087052 ) ) ;
#23347 = CARTESIAN_POINT ( 'NONE',  ( 3.837047941109549054, -1.595840754823075303, -1.059516945425369450 ) ) ;
#23348 = ADVANCED_FACE ( 'NONE', ( #137930 ), #148549, .T. ) ;
#23349 = CARTESIAN_POINT ( 'NONE',  ( 5.494608840674215955, 2.039112051642687717, 0.3575134270455831986 ) ) ;
#23350 = CARTESIAN_POINT ( 'NONE',  ( 0.6823417656249899377, 4.488541667008086655, -1.181850606188754593 ) ) ;
#23351 = CARTESIAN_POINT ( 'NONE',  ( 2.940257707442377022, 1.956376729411358095, 0.2430245213203632293 ) ) ;
#23352 = CARTESIAN_POINT ( 'NONE',  ( 1.184454412485607344, -1.878822398200689525, -0.4247803175085519412 ) ) ;
#23353 = CARTESIAN_POINT ( 'NONE',  ( 3.977312496258199825, 1.761605600429091201, -0.6297503393934977822 ) ) ;
#23354 = EDGE_CURVE ( 'NONE', #193316, #182484, #145013, .T. ) ;
#23355 = CARTESIAN_POINT ( 'NONE',  ( 2.948224681477436881, 0.8299853515197992415, -2.153443412361542020 ) ) ;
#23356 = CARTESIAN_POINT ( 'NONE',  ( 4.158551126772993989, -0.5825245785200537929, -1.767622772031415490 ) ) ;
#23357 = CARTESIAN_POINT ( 'NONE',  ( -1.001543065824772872E-14, 4.821875000341419693, 1.575800808251672791 ) ) ;
#23358 = CARTESIAN_POINT ( 'NONE',  ( -5.461236948206312114, 5.265864615862458464, 0.7998128361456341429 ) ) ;
#23359 = CARTESIAN_POINT ( 'NONE',  ( 5.615048174354031474, 9.702639970055050966, 0.7998128361456462443 ) ) ;
#23360 = DIRECTION ( 'NONE',  ( 2.168404344971003188E-14, -1.000000000000000000, 0.000000000000000000 ) ) ;
#23361 = CARTESIAN_POINT ( 'NONE',  ( 0.4168064962662480499, 1.450752768847368257, -1.526948433937134197 ) ) ;
#23362 = CARTESIAN_POINT ( 'NONE',  ( 4.826339496340538382, 4.733076955259818419, 1.040834085586084257E-14 ) ) ;
#23364 = CARTESIAN_POINT ( 'NONE',  ( 3.469446951953614189E-15, 0.7598076211376182387, 6.938893903907228378E-15 ) ) ;
#23363 = CARTESIAN_POINT ( 'NONE',  ( 0.6823417656249917140, 5.155208333674749177, 1.181850606188765695 ) ) ;
#23365 = CARTESIAN_POINT ( 'NONE',  ( -1.845237968648473448, 8.937006183319889274, -0.7749999999999996891 ) ) ;
#23366 = CARTESIAN_POINT ( 'NONE',  ( 1.775790443353560732, 0.3575140072833470906, -2.090081039791711337 ) ) ;
#23367 = CARTESIAN_POINT ( 'NONE',  ( 2.982962183914244836, 6.465010346290775978, -0.5414090736701422379 ) ) ;
#23368 = CARTESIAN_POINT ( 'NONE',  ( 0.5627676185161786249, 0.5905471060306236586, 1.931493850173772397 ) ) ;
#23369 = CARTESIAN_POINT ( 'NONE',  ( -0.6823417656250246877, 0.5510416670080897639, 1.181850606188755259 ) ) ;
#23370 = CARTESIAN_POINT ( 'NONE',  ( -4.121315508874280553, 3.910548969882488901, -0.7216878364870207285 ) ) ;
#23371 = CARTESIAN_POINT ( 'NONE',  ( 4.310602774141044868, 7.116454772218158809, -1.199719254218452047 ) ) ;
#23372 = ORIENTED_EDGE ( 'NONE', *, *, #33483, .T. ) ;
#23373 = CARTESIAN_POINT ( 'NONE',  ( 0.6851285477917113953, -0.2638797801631336259, -2.145333599305146333 ) ) ;
#23374 = CARTESIAN_POINT ( 'NONE',  ( 6.610000000000006537, 0.6121396118998356783, 1.775466344933520846 ) ) ;
#23377 = CARTESIAN_POINT ( 'NONE',  ( 4.880572111239557920, 4.796348339308675435, -0.7216878364870197293 ) ) ;
#23376 = CARTESIAN_POINT ( 'NONE',  ( 6.825078400183590688, 2.971555572656236599, 2.408956600524428282 ) ) ;
#23375 = CARTESIAN_POINT ( 'NONE',  ( 4.538947565524982686, 8.517465603079630299, 0.000000000000000000 ) ) ;
#23378 = DIRECTION ( 'NONE',  ( 0.000000000000000000, 1.000000000000000000, 0.000000000000000000 ) ) ;
#23379 = CARTESIAN_POINT ( 'NONE',  ( 5.841029835422532734, -1.731992920607817288, -1.032484497598872064 ) ) ;
#23380 = CARTESIAN_POINT ( 'NONE',  ( -8.839552966430023417, 9.415159337030921449, -0.7216878364870267237 ) ) ;
#23381 = CARTESIAN_POINT ( 'NONE',  ( 0.1698123575781598782, 1.266975945507025081, 1.788028528876134393 ) ) ;
#23383 = CARTESIAN_POINT ( 'NONE',  ( 0.6823417656249934904, 11.19270833367473550, 1.181850606188764807 ) ) ;
#23382 = CARTESIAN_POINT ( 'NONE',  ( 6.684453901184132185, -2.118919246787358102, -0.4271090584619871566 ) ) ;
#23384 = CARTESIAN_POINT ( 'NONE',  ( -8.947491310014823895, 12.52615806407091803, 1.199719254218462483 ) ) ;
#23386 = CARTESIAN_POINT ( 'NONE',  ( 1.089294787249419194, -0.4641297292061612456, 1.858405954227143386 ) ) ;
#23385 = CARTESIAN_POINT ( 'NONE',  ( -5.599154252319524794, 6.595063384869953360, 1.082531754730546636 ) ) ;
#23387 = CARTESIAN_POINT ( 'NONE',  ( 0.6823417656249882723, 0.1552083336747514530, 1.181850606188755259 ) ) ;
#23388 = B_SPLINE_CURVE_WITH_KNOTS ( 'NONE', 3,
 ( #193811, #128905, #177584, #207927, #161336, #194886, #93150, #140849, #159187, #141915, #76863, #126779, #142982, #13984, #18253, #164526, #50772, #64882, #98462 ),
 .UNSPECIFIED., .F., .F.,
 ( 4, 3, 3, 3, 3, 3, 4 ),
 ( 0.000000000000000000, 4.552787399504174405E-05, 9.164501444053742372E-05, 0.0001336247809766562765, 0.0001748474261958513174, 0.0002334031072667115464, 0.0002737127687883765038 ),
 .UNSPECIFIED. ) ;
#23389 = CARTESIAN_POINT ( 'NONE',  ( -0.7500000000000006661, 9.958333333333332149, -1.299038105676657340 ) ) ;
#23390 = CARTESIAN_POINT ( 'NONE',  ( 2.560839114378242076, -1.500511350262800470, -0.8505237462590549136 ) ) ;
#23391 = CARTESIAN_POINT ( 'NONE',  ( 4.797606254389322089, 6.690569611577942943, 1.599625672291268286 ) ) ;
#23392 = CARTESIAN_POINT ( 'NONE',  ( 2.002845679596281681, 1.468101958376843985, 0.9879206967360052438 ) ) ;
#23393 = CARTESIAN_POINT ( 'NONE',  ( 4.928867898441261275, 2.110505041808665716, 0.6446608841527908806 ) ) ;
#23394 = VERTEX_POINT ( 'NONE', #24146 ) ;
#23395 = CARTESIAN_POINT ( 'NONE',  ( 4.219013726799848207, 1.558537513506755845, -1.284668789120123833 ) ) ;
#23396 = CARTESIAN_POINT ( 'NONE',  ( -6.749980374757255319, 8.968339418673846097, 1.599625672291269396 ) ) ;
#23398 = CARTESIAN_POINT ( 'NONE',  ( 3.673453983005552814, 1.462458373076291673, 1.388474078538141754 ) ) ;
#23397 = CARTESIAN_POINT ( 'NONE',  ( 4.705793326368500118, 1.571798730262342181, 1.423547657546264000 ) ) ;
#23400 = VERTEX_POINT ( 'NONE', #90249 ) ;
#23399 = CARTESIAN_POINT ( 'NONE',  ( 4.007922362044618048, -0.6876924770315288038, 1.676191166192544157 ) ) ;
#23401 = CARTESIAN_POINT ( 'NONE',  ( 5.747730777550676073, 5.670383760089384495, 0.000000000000000000 ) ) ;
#23402 = ORIENTED_EDGE ( 'NONE', *, *, #51328, .T. ) ;
#23403 = CARTESIAN_POINT ( 'NONE',  ( 1.621729638615863944, -1.036547396872866678, -1.557007864774778705 ) ) ;
#23404 = CARTESIAN_POINT ( 'NONE',  ( 3.294945724223596883, 7.655198976062512983, -2.499999999999994671 ) ) ;
#23405 = CARTESIAN_POINT ( 'NONE',  ( 6.305303276254960565, 1.572402219250234268, -0.8993151100721032964 ) ) ;
#23406 = FACE_OUTER_BOUND ( 'NONE', #41125, .T. ) ;
#23408 =( GEOMETRIC_REPRESENTATION_CONTEXT ( 3 ) GLOBAL_UNCERTAINTY_ASSIGNED_CONTEXT ( ( #183658 ) ) GLOBAL_UNIT_ASSIGNED_CONTEXT ( ( #205447, #70095, #204360 ) ) REPRESENTATION_CONTEXT ( 'NONE', 'WORKASPACE' ) );
#23407 = CIRCLE ( 'NONE', #61468, 2.750000000000000444 ) ;
#23409 = CARTESIAN_POINT ( 'NONE',  ( 0.000000000000000000, 3.900000000000000799, 0.000000000000000000 ) ) ;
#23410 =( LENGTH_UNIT ( ) NAMED_UNIT ( * ) SI_UNIT ( .MILLI., .METRE. ) );
#23411 = CARTESIAN_POINT ( 'NONE',  ( -1.364683531250012516, 3.551041667008086211, -0.7879004041258300672 ) ) ;
#23412 = ORIENTED_EDGE ( 'NONE', *, *, #37914, .T. ) ;
#23413 = CARTESIAN_POINT ( 'NONE',  ( 7.865138509703455405, 8.348618814175074121, -0.7216878364870317197 ) ) ;
#23414 = CARTESIAN_POINT ( 'NONE',  ( -4.855228407469635243, 4.837057028235559386, 0.7216878364870257245 ) ) ;
#23415 = EDGE_CURVE ( 'NONE', #172991, #155330, #176228, .T. ) ;
#23416 = CARTESIAN_POINT ( 'NONE',  ( -6.017840079619296567, 8.114175741012878973, -1.599625672291271394 ) ) ;
#23417 = CARTESIAN_POINT ( 'NONE',  ( 4.060867369437678676, 0.5686956411946364476, 2.042824496258560441 ) ) ;
#23419 = CARTESIAN_POINT ( 'NONE',  ( -11.24554764128284035, 7.016280722987462859, -5.611469924715791535 ) ) ;
#23418 = CARTESIAN_POINT ( 'NONE',  ( -0.1296875068448125334, 4.095146142119266308, -2.381513845672214913 ) ) ;
#23420 = CARTESIAN_POINT ( 'NONE',  ( 5.395764264914824970, -0.7120431519804657494, 1.838431125455505688 ) ) ;
#23421 = CARTESIAN_POINT ( 'NONE',  ( 1.364683531249988757, 1.134375000341421247, 0.000000000000000000 ) ) ;
#23422 = CARTESIAN_POINT ( 'NONE',  ( 0.4045417950784445105, -1.998468379361338698, -0.2424310749817460697 ) ) ;
#23423 = ORIENTED_EDGE ( 'NONE', *, *, #61552, .T. ) ;
#23424 = CARTESIAN_POINT ( 'NONE',  ( 6.509000000000050967, 0.001920477310565076989, 2.100274754360692331 ) ) ;
#23425 = CARTESIAN_POINT ( 'NONE',  ( 8.790098660144254339, 13.29414747594431923, 8.101455065885637907 ) ) ;
#23426 = CARTESIAN_POINT ( 'NONE',  ( 1.170471352854907776, -0.9292243337341490328, -1.850172451097586990 ) ) ;
#23427 = ORIENTED_EDGE ( 'NONE', *, *, #93121, .F. ) ;
#23428 = CARTESIAN_POINT ( 'NONE',  ( 5.285699784481295183, 7.260012063351913625, 1.599625672291268286 ) ) ;
#23429 = CARTESIAN_POINT ( 'NONE',  ( 6.412080304620304538, 6.445458208337293549, -0.7998128361456481317 ) ) ;
#23431 = CARTESIAN_POINT ( 'NONE',  ( 4.819033534653518025, 7.709623992816043270, -1.199719254218452047 ) ) ;
#23430 = CARTESIAN_POINT ( 'NONE',  ( 5.226549702048478352, 0.1529751191454275516, 2.085101625929087099 ) ) ;
#23432 = CARTESIAN_POINT ( 'NONE',  ( 7.388267364804250725, 7.584343111885245570, -0.7998128361456341429 ) ) ;
#23435 = VERTEX_POINT ( 'NONE', #206105 ) ;
#23434 = CARTESIAN_POINT ( 'NONE',  ( 2.033590728242135715, -1.756817081591253604, 0.4409998202260062006 ) ) ;
#23433 = CARTESIAN_POINT ( 'NONE',  ( 2.678497062878131718, -1.746332412481563567, -0.5319975912557314279 ) ) ;
#23436 = DIRECTION ( 'NONE',  ( -0.3085202182251676195, 0.000000000000000000, 0.9512177852344304574 ) ) ;
#23437 = CARTESIAN_POINT ( 'NONE',  ( 0.000000000000000000, 4.999999999999997335, 0.000000000000000000 ) ) ;
#23438 = CARTESIAN_POINT ( 'NONE',  ( 4.770673279661371780, -1.444480529215144804, 1.668407551275403300 ) ) ;
#23439 = CARTESIAN_POINT ( 'NONE',  ( 8.145751363712157911, 8.397798100619326078, -0.7998128361456281477 ) ) ;
#23440 = FACE_OUTER_BOUND ( 'NONE', #124220, .T. ) ;
#23441 = EDGE_CURVE ( 'NONE', #52099, #105328, #110574, .T. ) ;
#23442 = CARTESIAN_POINT ( 'NONE',  ( 3.387273370026026686, 0.04433669930821101945, -1.911926451916061476 ) ) ;
#23443 = CIRCLE ( 'NONE', #144580, 9.499999999999992895 ) ;
#23444 = CARTESIAN_POINT ( 'NONE',  ( 6.909851844459134362, 11.21324425184434936, -0.7998128361456291469 ) ) ;
#23445 = CARTESIAN_POINT ( 'NONE',  ( 6.180147188013234150, -1.146869210499700920, -1.723488058659912392 ) ) ;
#23446 = CARTESIAN_POINT ( 'NONE',  ( -3.040408649313822931, 6.452285303259204241, 0.6472276285178559796 ) ) ;
#23447 = CARTESIAN_POINT ( 'NONE',  ( 6.023007056224171762, -2.064090639567913499, 0.7368321019862942300 ) ) ;
#23448 = CARTESIAN_POINT ( 'NONE',  ( 5.396826230253299883, 7.665096674459883630, -1.326205021280580265 ) ) ;
#23449 = AXIS2_PLACEMENT_3D ( 'NONE', #61813, #127981, #193934 ) ;
#23450 = CARTESIAN_POINT ( 'NONE',  ( 0.3988961525413015075, 2.965604040240178652, 2.024173287229360074 ) ) ;
#23451 = CARTESIAN_POINT ( 'NONE',  ( 4.411198876399872404, 6.239761003923544713, -1.599625672291273171 ) ) ;
#23452 = CARTESIAN_POINT ( 'NONE',  ( 1.642778471875001811, -1.130208332855375808, 2.845375778867859751 ) ) ;
#23453 = CARTESIAN_POINT ( 'NONE',  ( -1.500000000000008216, 12.53125000068279427, 3.469446951953614189E-15 ) ) ;
#23454 = B_SPLINE_CURVE_WITH_KNOTS ( 'NONE', 3,
 ( #133469, #147562, #199472, #181111, #48995, #134530, #116173, #200536, #182159, #100918, #151826, #33789, #47951, #82536, #51114, #114065, #117239, #52182, #213583, #167006, #180057, #32729, #18597, #84676, #115115, #131359, #118307, #98809, #184294, #31679, #163815, #35919, #101995, #168063, #15393, #19665, #38068, #153952, #4455, #86811, #169123, #5520, #187501, #91100, #73758, #204796 ),
 .UNSPECIFIED., .F., .F.,
 ( 4, 3, 3, 3, 3, 3, 3, 3, 3, 3, 3, 3, 3, 3, 3, 4 ),
 ( 0.000000000000000000, 0.0002001208021641467678, 0.0002987350495539372935, 0.0003974608682140796023, 0.0004175935870586608640, 0.0004226419832867753202, 0.0004238941922970896193, 0.0004244411037539569343, 0.0004249975721417096437, 0.0004254804695417831119, 0.0004261174966295773058, 0.0004273003274780872687, 0.0004324025126211059077, 0.0004525445321848968277, 0.0005326990625275228493, 0.0005514034162145647726 ),
 .UNSPECIFIED. ) ;
#23455 = CARTESIAN_POINT ( 'NONE',  ( -8.405692050792730186, 9.869357483088723626, 1.082531754730558626 ) ) ;
#23456 = CARTESIAN_POINT ( 'NONE',  ( 4.492547798081839794, 6.334668079219206049, 1.599625672291262513 ) ) ;
#23457 = CARTESIAN_POINT ( 'NONE',  ( 5.629760504653214426, 1.996728726787128538, -0.5467053113129491937 ) ) ;
#23458 = CARTESIAN_POINT ( 'NONE',  ( 4.248602273900093707, 0.5149172349826669493, 1.856347322705960146 ) ) ;
#23459 = CARTESIAN_POINT ( 'NONE',  ( 1.546500145565053108, -1.423948579484592747, 1.427951870166991544 ) ) ;
#23460 = CARTESIAN_POINT ( 'NONE',  ( -8.435144125996554720, 12.99275191363802229, 0.7998128361456341429 ) ) ;
#23461 = CARTESIAN_POINT ( 'NONE',  ( 6.210516883511641772, 9.403297576475722508, 1.199719254218452047 ) ) ;
#23463 = ADVANCED_FACE ( 'NONE', ( #8981 ), #189865, .T. ) ;
#23462 = CARTESIAN_POINT ( 'NONE',  ( -15.75000000000000000, 13.39999999999998259, 1.399999999999998579 ) ) ;
#23464 = B_SPLINE_CURVE_WITH_KNOTS ( 'NONE', 3,
 ( #210014, #128868, #174366, #45424, #61656, #107274, #60583, #8630, #10755, #192701 ),
 .UNSPECIFIED., .F., .F.,
 ( 4, 2, 2, 2, 4 ),
 ( 0.000000000000000000, 0.0002216178067634668662, 0.0004432356135269337324, 0.0006648534202904005444, 0.0008864712270538674648 ),
 .UNSPECIFIED. ) ;
#23465 = CARTESIAN_POINT ( 'NONE',  ( 1.060776890969020059, -1.982532595227912475, -0.9341070725938580566 ) ) ;
#23466 = CARTESIAN_POINT ( 'NONE',  ( 5.162654993523497993, -1.319871331358621447, 1.261628347558926944 ) ) ;
#23467 = CARTESIAN_POINT ( 'NONE',  ( -5.108724954250998707, 4.854600622914589714, -0.7998128361456221525 ) ) ;
#23468 = EDGE_CURVE ( 'NONE', #76787, #29424, #13554, .T. ) ;
#23469 = CARTESIAN_POINT ( 'NONE',  ( 5.885648082108199119, 6.999582529615296700, 1.082531754730549967 ) ) ;
#23470 = CARTESIAN_POINT ( 'NONE',  ( 9.935427640716063991, 10.48575375712389679, -0.7998128361456281477 ) ) ;
#23471 = CARTESIAN_POINT ( 'NONE',  ( -5.875479466675803231, 7.948088359245467416, -1.599625672291271394 ) ) ;
#23472 = CARTESIAN_POINT ( 'NONE',  ( 3.344057444064992168, 7.053150784717805877, 1.040834085586084257E-14 ) ) ;
#23473 = CARTESIAN_POINT ( 'NONE',  ( 5.388439706788500594, 5.251210844200210559, 0.7998128361456352531 ) ) ;
#23474 =( BOUNDED_CURVE ( )  B_SPLINE_CURVE ( 2, ( #156716, #91732, #26692 ),
 .UNSPECIFIED., .F., .T. ) 
 B_SPLINE_CURVE_WITH_KNOTS ( ( 3, 3 ),
 ( 0.2750000000000000777, 0.2780234451730101974 ),
 .UNSPECIFIED. ) 
 CURVE ( )  GEOMETRIC_REPRESENTATION_ITEM ( )  RATIONAL_B_SPLINE_CURVE ( ( 0.9999999999999982236, 0.9027844369038582339, 0.9466533178002750626 ) ) 
 REPRESENTATION_ITEM ( '' )  );
#23475 = ORIENTED_EDGE ( 'NONE', *, *, #191590, .F. ) ;
#23477 = CARTESIAN_POINT ( 'NONE',  ( 6.521754290436940771, -0.4404898795188401106, 1.971875975034496742 ) ) ;
#23476 = CARTESIAN_POINT ( 'NONE',  ( 2.507154105146496725, -1.820902139252629448, 0.2722148935128121394 ) ) ;
#23478 = CARTESIAN_POINT ( 'NONE',  ( 2.091588275066556868, 1.323615364194903554, -1.878831054484223495 ) ) ;
#23479 = CARTESIAN_POINT ( 'NONE',  ( 0.2329586101569866563, 0.008238550247445517935, -1.845944905557160398 ) ) ;
#23480 = CARTESIAN_POINT ( 'NONE',  ( -6.728924311084075960, 6.744833205886536120, 1.040834085586084257E-14 ) ) ;
#23481 = DIRECTION ( 'NONE',  ( -0.9999980456341537316, 0.000000000000000000, -0.001977050295949950038 ) ) ;
#23482 = CARTESIAN_POINT ( 'NONE',  ( 3.322422747544371280, -0.7792853099402965444, -1.746611395919236642 ) ) ;
#23483 = CARTESIAN_POINT ( 'NONE',  ( -8.462260433223891098, 13.02438760540324481, -0.7998128361456281477 ) ) ;
#23484 = CYLINDRICAL_SURFACE ( 'NONE', #5472, 0.07999999999999998779 ) ;
#23485 = CARTESIAN_POINT ( 'NONE',  ( -7.932929277771797238, 8.427708043588125975, 0.000000000000000000 ) ) ;
#23487 = CARTESIAN_POINT ( 'NONE',  ( 1.516246529245099284, 1.258767711876613848, -1.383943980506313398 ) ) ;
#23486 = CARTESIAN_POINT ( 'NONE',  ( 2.120754239039924549, 0.003043923042475667976, 2.090933975095090158 ) ) ;
#23488 = CARTESIAN_POINT ( 'NONE',  ( 2.214220036344019871, -1.617569417291262690, -1.203170845901546215 ) ) ;
#23489 = CARTESIAN_POINT ( 'NONE',  ( 8.812436659202669276, 10.34389285956704363, -1.082531754730543083 ) ) ;
#23490 = VERTEX_POINT ( 'NONE', #203951 ) ;
#23491 = CARTESIAN_POINT ( 'NONE',  ( -1.364683531249997417, 4.571875000341417028, 1.214306433183764966E-14 ) ) ;
#23492 = CARTESIAN_POINT ( 'NONE',  ( 2.630072014739594177, 0.2149344560898290013, 1.727053582138169618 ) ) ;
#23493 = CARTESIAN_POINT ( 'NONE',  ( 3.472859903394816872, 7.203420320602605287, -0.7998128361456291469 ) ) ;
#23495 = CARTESIAN_POINT ( 'NONE',  ( 0.1975679859324476761, 2.638084932213505152, -1.992869612520775213 ) ) ;
#23494 = CARTESIAN_POINT ( 'NONE',  ( 6.959052028703007764, 5.167241622962437830, 1.214306433183764966E-14 ) ) ;
#23496 = CARTESIAN_POINT ( 'NONE',  ( 2.490480453433571384, -0.2941264275767330183, -1.699438164531028583 ) ) ;
#23497 = CARTESIAN_POINT ( 'NONE',  ( 2.806388347806953121, 1.585463108415147149, -1.513251884624075672 ) ) ;
#23498 = CARTESIAN_POINT ( 'NONE',  ( 4.916741810085082598, 1.523553907054091328, -1.596827639139485777 ) ) ;
#23499 = CARTESIAN_POINT ( 'NONE',  ( -9.917242840447775265, 4.174869238508773783, -6.172972641688763140 ) ) ;
#23500 = CARTESIAN_POINT ( 'NONE',  ( 3.907220266852969637, -1.778082601562074094, 1.245552836545896769 ) ) ;
#23501 = CARTESIAN_POINT ( 'NONE',  ( 2.156629195875509719, -1.411784796728832392, 1.157573153174975111 ) ) ;
#23502 =( NAMED_UNIT ( * ) PLANE_ANGLE_UNIT ( ) SI_UNIT ( $, .RADIAN. ) );
#23503 = CARTESIAN_POINT ( 'NONE',  ( 4.540305813605725938, 0.8135460886731570307, 1.954998174167394520 ) ) ;
#23504 = CARTESIAN_POINT ( 'NONE',  ( 6.639320575229236354, 1.260096212659385984, 2.110683211146132443 ) ) ;
#23505 = VERTEX_POINT ( 'NONE', #107621 ) ;
#23506 = AXIS2_PLACEMENT_3D ( 'NONE', #196842, #213073, #163287 ) ;
#23508 = CARTESIAN_POINT ( 'NONE',  ( -1.364683531250012516, 0.8427083336747532849, 0.7879004041258379498 ) ) ;
#23507 = CARTESIAN_POINT ( 'NONE',  ( 4.388395349243869425, -0.5016406811718626679, -2.236657869423730460 ) ) ;
#23509 = CARTESIAN_POINT ( 'NONE',  ( 11.48243876534946217, 11.29999999999998117, 3.199999999999997957 ) ) ;
#23510 = CARTESIAN_POINT ( 'NONE',  ( 2.920892028740289081, 5.495125569250587816, 1.199719254218452047 ) ) ;
#23511 = CARTESIAN_POINT ( 'NONE',  ( 0.03014954708456181465, -2.078685333231004684, 0.4181070283913386199 ) ) ;
#23512 = CARTESIAN_POINT ( 'NONE',  ( -6.588899466561478846, 6.789396920517583922, 0.7216878364870317197 ) ) ;
#23513 = CARTESIAN_POINT ( 'NONE',  ( 3.714570900464278846, 5.356752022006865843, 1.443375672974062551 ) ) ;
#23514 = CARTESIAN_POINT ( 'NONE',  ( -5.368665640887164692, 9.207267647769599606, 0.000000000000000000 ) ) ;
#23515 = CARTESIAN_POINT ( 'NONE',  ( 4.312902262922978736, 5.164712407232485702, -1.082531754730548412 ) ) ;
#23516 = EDGE_LOOP ( 'NONE', ( #202803, #156643 ) ) ;
#23517 = CARTESIAN_POINT ( 'NONE',  ( 4.975232503164924935, -2.001511053420693020, -0.2440319332882301961 ) ) ;
#23519 = CARTESIAN_POINT ( 'NONE',  ( 3.063389470891558997, 1.739959455442946279, 1.107334787568447165 ) ) ;
#23518 = CARTESIAN_POINT ( 'NONE',  ( 5.834086172582112262, 5.700855377634248100, 1.040834085586084257E-14 ) ) ;
#23521 = CARTESIAN_POINT ( 'NONE',  ( -0.1409997244345879697, 0.2375178066936211585, -2.034344168881811132 ) ) ;
#23520 = CARTESIAN_POINT ( 'NONE',  ( 6.481679955784983349, 9.719654494127929922, -1.199719254218452047 ) ) ;
#23522 = CARTESIAN_POINT ( 'NONE',  ( 7.014364370223726830, 9.276787413384745662, -1.599625672291269396 ) ) ;
#23523 = CARTESIAN_POINT ( 'NONE',  ( 3.285556943749998737, -2.005208332855377140, -1.896917185911906500 ) ) ;
#23524 = CARTESIAN_POINT ( 'NONE',  ( 5.736325210887869730, 0.4244523575273988492, 2.149783713274712404 ) ) ;
#23525 = CARTESIAN_POINT ( 'NONE',  ( 3.358046224211252095, 0.04667712216412447934, -2.016033814150198999 ) ) ;
#23526 = CARTESIAN_POINT ( 'NONE',  ( 3.122423488780329492, 0.04808623196613136253, 1.840796284283818585 ) ) ;
#23527 = CARTESIAN_POINT ( 'NONE',  ( 5.952193131599331721, 6.902979060742733708, 1.199719254218462483 ) ) ;
#23528 = CARTESIAN_POINT ( 'NONE',  ( 6.651389018303578204, -1.468406013062272253, -1.084454090978362428 ) ) ;
#23529 = CARTESIAN_POINT ( 'NONE',  ( -7.562750758324527922, 7.717630727667075696, 1.040834085586084257E-14 ) ) ;
#23530 = CARTESIAN_POINT ( 'NONE',  ( 6.543838037463636681, 0.8733170268561093463, -2.087377253365163110 ) ) ;
#23531 = CARTESIAN_POINT ( 'NONE',  ( 1.383574010005955701, 1.945322680536746063, -0.8074913105669545565 ) ) ;
#23532 = CARTESIAN_POINT ( 'NONE',  ( -4.599959256786493533, 8.588645909551377855, 0.000000000000000000 ) ) ;
#23533 = CARTESIAN_POINT ( 'NONE',  ( 6.856673000209174695, 9.022537805042615489, 1.599625672291281386 ) ) ;
#23534 = CARTESIAN_POINT ( 'NONE',  ( 7.160114521348466710, 7.526090827760914870, 0.000000000000000000 ) ) ;
#23535 = CARTESIAN_POINT ( 'NONE',  ( -6.201965203247477909, 9.323044272842313518, 1.199719254218452047 ) ) ;
#23536 = CARTESIAN_POINT ( 'NONE',  ( 6.602457619730760285, 8.725953194484466380, 1.443375672974076540 ) ) ;
#23537 = CARTESIAN_POINT ( 'NONE',  ( 5.430717995911492402, 6.471920874811950775, 1.294091166901890633 ) ) ;
#23538 = CARTESIAN_POINT ( 'NONE',  ( -5.949330478298285207, 5.835307067636438028, 0.7998128361456341429 ) ) ;
#23539 = CARTESIAN_POINT ( 'NONE',  ( 3.973042321754824524, -1.644474126697339944, 1.493583396047935219 ) ) ;
#23540 = CARTESIAN_POINT ( 'NONE',  ( 2.853686581259745836, 2.180823047698337902, -0.2155538573413370296 ) ) ;
#23541 = CARTESIAN_POINT ( 'NONE',  ( -6.144869935491728441, 8.192100896205577243, -1.599625672291263179 ) ) ;
#23542 = CARTESIAN_POINT ( 'NONE',  ( 6.883263157960393563, 1.268976584491373183, 2.060807272249213451 ) ) ;
#23543 = CARTESIAN_POINT ( 'NONE',  ( -5.418418667316934112, 6.350518529071726981, -1.199719254218453823 ) ) ;
#23544 = CARTESIAN_POINT ( 'NONE',  ( 5.406682003534418079, 0.5678430586343993225, 1.877905798087247335 ) ) ;
#23545 = DIRECTION ( 'NONE',  ( -1.000000000000000000, 0.000000000000000000, 0.000000000000000000 ) ) ;
#23546 = CARTESIAN_POINT ( 'NONE',  ( -1.201851678989727383E-14, 2.321875000341416584, 1.575800808251672791 ) ) ;
#23547 = EDGE_CURVE ( 'NONE', #182455, #155586, #17079, .T. ) ;
#23548 = CARTESIAN_POINT ( 'NONE',  ( -4.014622883422336308, 5.777089012116397804, -1.443375672974066548 ) ) ;
#23550 = ORIENTED_EDGE ( 'NONE', *, *, #42077, .T. ) ;
#23549 = CARTESIAN_POINT ( 'NONE',  ( -6.399085315970151733, 7.528316292462387871, -1.082531754730544860 ) ) ;
#23552 = CARTESIAN_POINT ( 'NONE',  ( 5.062787373817618786, 0.6179034821891697948, 2.028544477791139222 ) ) ;
#23551 = CIRCLE ( 'NONE', #189467, 0.09999999999999982514 ) ;
#23553 = CARTESIAN_POINT ( 'NONE',  ( -2.972980823146582186, 6.690504403638126263, 0.000000000000000000 ) ) ;
#23554 = ORIENTED_EDGE ( 'NONE', *, *, #196415, .F. ) ;
#23555 = CARTESIAN_POINT ( 'NONE',  ( 5.911032513020411550, 1.904272706209766630, 1.023102869888978583 ) ) ;
#23556 = CARTESIAN_POINT ( 'NONE',  ( 6.993308306550549247, 7.053281200597435685, 1.040834085586084257E-14 ) ) ;
#23557 = CARTESIAN_POINT ( 'NONE',  ( 4.546344060013487898, -1.475942220874026489, 1.100600019281534836 ) ) ;
#23558 = CARTESIAN_POINT ( 'NONE',  ( -5.894595317363360287, 6.010551413984606128, 0.2245382864616944640 ) ) ;
#23559 = CARTESIAN_POINT ( 'NONE',  ( 1.364683531249988757, 1.946875000341415030, 0.000000000000000000 ) ) ;
#23560 = CARTESIAN_POINT ( 'NONE',  ( 0.2744473674479709913, 1.625014162249105443, -0.6237133657705071776 ) ) ;
#23561 = CARTESIAN_POINT ( 'NONE',  ( 6.727182134110196721, 3.701357331967893405, 2.425430364167603603 ) ) ;
#23562 = CARTESIAN_POINT ( 'NONE',  ( 4.704316114261903436, 4.590716342834741504, 1.214306433183764966E-14 ) ) ;
#23563 = DIRECTION ( 'NONE',  ( 0.000000000000000000, 1.000000000000000000, 0.000000000000000000 ) ) ;
#23564 = CARTESIAN_POINT ( 'NONE',  ( 4.258765444007106105, -1.603684720688375975, 1.449730421305382544 ) ) ;
#23565 = CARTESIAN_POINT ( 'NONE',  ( -5.623934791570306402, 5.455678766453782913, 0.7998128361456341429 ) ) ;
#23566 = CARTESIAN_POINT ( 'NONE',  ( 6.854846703925610463, -0.8643618726141141240, 1.819651424301058640 ) ) ;
#23567 = CARTESIAN_POINT ( 'NONE',  ( -8.812436658758329600, 9.383523644747281622, 1.040834085586084257E-14 ) ) ;
#23569 = STYLED_ITEM ( 'NONE', ( #161685 ), #5413 ) ;
#23568 = AXIS2_PLACEMENT_3D ( 'NONE', #28306, #93337, #159373 ) ;
#23570 = CARTESIAN_POINT ( 'NONE',  ( 3.819328725847204620, -0.1613130240520690706, 2.155748724213396361 ) ) ;
#23571 = CARTESIAN_POINT ( 'NONE',  ( 4.341064969683814390, -1.716640784620737659, 0.9690559893368445588 ) ) ;
#23572 = CARTESIAN_POINT ( 'NONE',  ( 3.444447550215405052, 1.098527548611628601, 1.341433071544478217 ) ) ;
#23573 = CARTESIAN_POINT ( 'NONE',  ( 1.277182604683280598, 2.023070758711601691, -0.8431670391453591762 ) ) ;
#23574 = CARTESIAN_POINT ( 'NONE',  ( 1.343279689680024536, 0.4525242940816387449, 2.262625540901804122 ) ) ;
#23575 = CARTESIAN_POINT ( 'NONE',  ( 4.182927011504236070, -0.1980092267137799622, -2.051220347156012647 ) ) ;
#23576 = CARTESIAN_POINT ( 'NONE',  ( 5.759312517635055251, 1.912593682650292060, -0.3362288579709416525 ) ) ;
#23578 = ORIENTED_EDGE ( 'NONE', *, *, #101879, .F. ) ;
#23577 = CARTESIAN_POINT ( 'NONE',  ( -7.171900071504738072, 10.35067193585544665, -1.082531754730543083 ) ) ;
#23579 = CARTESIAN_POINT ( 'NONE',  ( -6.629010762438975135, 6.698543742459062145, -0.7998128361456362523 ) ) ;
#23580 = CARTESIAN_POINT ( 'NONE',  ( 1.316495309083404618E-15, 0.5000000000000000000, -10.75000000000000000 ) ) ;
#23582 = VERTEX_POINT ( 'NONE', #87029 ) ;
#23581 = CARTESIAN_POINT ( 'NONE',  ( -5.164730172163054966, 4.990216387137135889, -0.7998128361456362523 ) ) ;
#23583 = CARTESIAN_POINT ( 'NONE',  ( -7.415946836550729948, 9.675023947441092176, 1.443375672974090751 ) ) ;
#23584 = CARTESIAN_POINT ( 'NONE',  ( 3.241465689944766915, -1.947025830926933043, 1.038692105600529159 ) ) ;
#23585 = CARTESIAN_POINT ( 'NONE',  ( -3.285556943749998737, -3.317708332855375808, 1.896917185911908499 ) ) ;
#23586 = ORIENTED_EDGE ( 'NONE', *, *, #50194, .T. ) ;
#23587 = CARTESIAN_POINT ( 'NONE',  ( 0.5142147075538996415, 0.7048593813003102282, 1.722512033545370080 ) ) ;
#23588 = CARTESIAN_POINT ( 'NONE',  ( -0.02919842301646497981, 5.720960850909259321, -2.667883601355185430 ) ) ;
#23589 =( LENGTH_UNIT ( ) NAMED_UNIT ( * ) SI_UNIT ( .MILLI., .METRE. ) );
#23590 = CARTESIAN_POINT ( 'NONE',  ( 4.612443543746578278, 7.139628114692022187, -1.342220757880496995 ) ) ;
#23591 = CARTESIAN_POINT ( 'NONE',  ( -5.346851039111045978, 6.199209027673978412, -1.060622344683157747 ) ) ;
#23592 = CARTESIAN_POINT ( 'NONE',  ( 6.298766309436587996, 1.533505995929709487, 1.018591839899836371 ) ) ;
#23593 = ORIENTED_EDGE ( 'NONE', *, *, #66049, .F. ) ;
#23594 = CARTESIAN_POINT ( 'NONE',  ( 2.026313557074521210, 1.187556641299570614, -1.684123726253353492 ) ) ;
#23595 = CARTESIAN_POINT ( 'NONE',  ( 0.6801582343749917881, 0.7239583336747443809, 1.178068619123793015 ) ) ;
#23596 = CARTESIAN_POINT ( 'NONE',  ( -7.043624497499477499, 8.176315654292865887, 1.199719254218450271 ) ) ;
#23597 =( NAMED_UNIT ( * ) PLANE_ANGLE_UNIT ( ) SI_UNIT ( $, .RADIAN. ) );
#23598 = FILL_AREA_STYLE_COLOUR ( '', #192762 ) ;
#23599 = CARTESIAN_POINT ( 'NONE',  ( 4.681643115420508039, 4.356338477612361260, 0.7998128361456341429 ) ) ;
#23600 = EDGE_CURVE ( 'NONE', #183890, #116379, #24566, .T. ) ;
#23601 = CARTESIAN_POINT ( 'NONE',  ( 0.9892191112199534286, 1.817966452439750968, -0.9706697534878678812 ) ) ;
#23603 = CARTESIAN_POINT ( 'NONE',  ( 5.108874002337426390, -0.2646564886703614006, 1.822002613180016883 ) ) ;
#23602 = CARTESIAN_POINT ( 'NONE',  ( 1.250000000000033973, 8.500000000000000000, 9.921567416492207414 ) ) ;
#23604 = CARTESIAN_POINT ( 'NONE',  ( 7.091078035147269532, 8.231678114882006625, 1.199719254218462483 ) ) ;
#23605 = AXIS2_PLACEMENT_3D ( 'NONE', #197930, #132979, #116752 ) ;
#23606 = CARTESIAN_POINT ( 'NONE',  ( -4.606738333593328072, 8.596554832492683929, 0.7998128361456281477 ) ) ;
#23607 = CARTESIAN_POINT ( 'NONE',  ( 4.442132104469964204, 0.9450947508268662256, -1.994404356956205326 ) ) ;
#23608 = CARTESIAN_POINT ( 'NONE',  ( 0.7905619602705875604, -2.145198653374354336, -0.2653712149464776959 ) ) ;
#23609 = CARTESIAN_POINT ( 'NONE',  ( -6.236387472606158333, 7.338502141871059870, -1.082531754730544860 ) ) ;
#23610 = CARTESIAN_POINT ( 'NONE',  ( 0.6153073421325053749, 1.564839666810373231, 1.099065937236625157 ) ) ;
#23611 = CARTESIAN_POINT ( 'NONE',  ( 0.8664231474371618669, -1.968446048378743152, -0.4370742218882398000 ) ) ;
#23613 = EDGE_CURVE ( 'NONE', #58716, #180119, #138195, .T. ) ;
#23612 = COLOUR_RGB ( '', 0.09019608, 0.27058824, 0.51372549) ;
#23614 = CARTESIAN_POINT ( 'NONE',  ( 6.658462837642789012, 9.821938173008357253, 1.082531754730549078 ) ) ;
#23615 = CARTESIAN_POINT ( 'NONE',  ( 1.318156941596902998, -1.811358654967555104, 1.414711894558273730 ) ) ;
#23616 = CARTESIAN_POINT ( 'NONE',  ( 11.41381675112453387, 13.39999999999998259, 3.704697986577180746 ) ) ;
#23617 = CARTESIAN_POINT ( 'NONE',  ( 0.7500000000000006661, 12.19791666734946389, -1.299038105676657340 ) ) ;
#23618 = CARTESIAN_POINT ( 'NONE',  ( 11.48243876534946217, 12.30000000000000071, -3.200000000000001510 ) ) ;
#23619 = CARTESIAN_POINT ( 'NONE',  ( 1.727212824277712944, -1.762453432929488528, 0.6273722324065673650 ) ) ;
#23620 = CARTESIAN_POINT ( 'NONE',  ( 2.764861550476094276, -0.1531697945360478985, -2.010801143277194392 ) ) ;
#23622 = CARTESIAN_POINT ( 'NONE',  ( 6.639320575229257670, 2.427506520031021520, 2.484945200759064665 ) ) ;
#23621 = CARTESIAN_POINT ( 'NONE',  ( -1.364683531250014514, 0.9885416670080898749, -0.7879004041258289570 ) ) ;
#23624 = CARTESIAN_POINT ( 'NONE',  ( 3.985071343692931034, -0.2060594512321256011, -2.095964026187596918 ) ) ;
#23623 = CARTESIAN_POINT ( 'NONE',  ( -8.097244055859620815, 10.46987070330147063, -1.599625672291263179 ) ) ;
#23625 = B_SPLINE_CURVE_WITH_KNOTS ( 'NONE', 3,
 ( #119420, #22891, #186475, #54363, #103109, #170232, #21817, #5564 ),
 .UNSPECIFIED., .F., .F.,
 ( 4, 2, 2, 4 ),
 ( 0.000000000000000000, 0.0003954713701971529841, 0.0005932070552957304519, 0.0007909427403943080281 ),
 .UNSPECIFIED. ) ;
#23626 = CARTESIAN_POINT ( 'NONE',  ( 8.308449207076147758, 8.587612251210650527, -0.7998128361456281477 ) ) ;
#23628 = CARTESIAN_POINT ( 'NONE',  ( -8.528242318195895066, 9.908369778438709474, 1.199719254218462483 ) ) ;
#23627 = CARTESIAN_POINT ( 'NONE',  ( 3.739016502318667445, 7.584212696005614873, 0.7998128361456271485 ) ) ;
#23629 = PRESENTATION_STYLE_ASSIGNMENT (( #188265 ) ) ;
#23630 = CARTESIAN_POINT ( 'NONE',  ( 3.920179414529322504, -2.014104250368133453, 0.1526392722818684933 ) ) ;
#23631 = CARTESIAN_POINT ( 'NONE',  ( -1.364683531250010295, 4.280208333674753618, 0.7879004041258379498 ) ) ;
#23632 = CARTESIAN_POINT ( 'NONE',  ( 6.531690654341108626, 1.975040822251827644, -0.5949189890239890977 ) ) ;
#23633 = CARTESIAN_POINT ( 'NONE',  ( 7.931156674314368438, 12.19684052010138586, 1.040834085586084257E-14 ) ) ;
#23634 = CARTESIAN_POINT ( 'NONE',  ( 4.552137767457805850, 2.161219302129935738, -0.04802546048104232301 ) ) ;
#23635 = CARTESIAN_POINT ( 'NONE',  ( 7.361151057576892143, 7.552707420120024828, 0.7998128361456291469 ) ) ;
#23636 = CARTESIAN_POINT ( 'NONE',  ( 1.364683531249986537, -0.07395833299191513499, 0.7879004041258500513 ) ) ;
#23638 = DIRECTION ( 'NONE',  ( 1.000000000000000000, -6.165071176878339540E-16, 0.000000000000000000 ) ) ;
#23637 = CARTESIAN_POINT ( 'NONE',  ( 6.638652492546827766, 7.774124658506663010, 1.199719254218452047 ) ) ;
#23639 = CARTESIAN_POINT ( 'NONE',  ( 6.426201622753093368, 10.44105962661321563, 1.040834085586084257E-14 ) ) ;
#23641 = CARTESIAN_POINT ( 'NONE',  ( 0.000000000000000000, 4.400000000000001243, 0.000000000000000000 ) ) ;
#23640 = CARTESIAN_POINT ( 'NONE',  ( 2.172564162468085147, -1.022266837292043595, -1.915435327925461229 ) ) ;
#23643 = CARTESIAN_POINT ( 'NONE',  ( 1.311775528174640604, 1.236260529797410301, -1.364685630449238740 ) ) ;
#23642 = CARTESIAN_POINT ( 'NONE',  ( -4.094199201646926412, 7.720390135322642067, 0.7216878364870317197 ) ) ;
#23644 = CARTESIAN_POINT ( 'NONE',  ( -1.364683531250012516, 1.530208333674756505, 0.7879004041258379498 ) ) ;
#23645 = CARTESIAN_POINT ( 'NONE',  ( 3.034921719543516971, -1.931671641359738567, 1.035203715903771915 ) ) ;
#23646 = CARTESIAN_POINT ( 'NONE',  ( 6.983263157960365675, 7.629137130509066722, 2.753810918356710769 ) ) ;
#23647 = CARTESIAN_POINT ( 'NONE',  ( 3.889755562772099662, 1.636703778197702075, 1.562332884182315196 ) ) ;
#23648 = CARTESIAN_POINT ( 'NONE',  ( -4.882907879216086933, 8.848476292394087395, -0.7998128361456281477 ) ) ;
#23650 = AXIS2_PLACEMENT_3D ( 'NONE', #81982, #31127, #64669 ) ;
#23649 = CARTESIAN_POINT ( 'NONE',  ( -11.80248046418316044, 9.799999999999982947, 1.695421849633139466 ) ) ;
#23651 = CARTESIAN_POINT ( 'NONE',  ( 6.272547281004660746, 6.891683285556123195, -0.7655605874731727933 ) ) ;
#23652 = CARTESIAN_POINT ( 'NONE',  ( -1.500000000000008216, 13.49999999999999822, 3.469446951953614189E-15 ) ) ;
#23653 = CARTESIAN_POINT ( 'NONE',  ( 4.733205024946604667, 8.536173272497439513, 0.000000000000000000 ) ) ;
#23654 = CARTESIAN_POINT ( 'NONE',  ( 5.044116495868207650, 1.765035602982415242, 0.1300806658623629153 ) ) ;
#23655 = CARTESIAN_POINT ( 'NONE',  ( 8.959240580532112475, 9.346868853575953651, -0.7998128361456221525 ) ) ;
#23656 = CARTESIAN_POINT ( 'NONE',  ( 1.852698501422584298, 0.6601115537133980249, 1.999908888789264649 ) ) ;
#23658 = CARTESIAN_POINT ( 'NONE',  ( -1.500000000000015099, 0.8791666666666874130, -0.8660254037844313801 ) ) ;
#23657 = CARTESIAN_POINT ( 'NONE',  ( -1.402160292154681736E-14, 10.92187500034139802, 1.575800808251682339 ) ) ;
#23659 = CARTESIAN_POINT ( 'NONE',  ( 0.8187300819318241718, -1.428952508342665517, 1.355707701654704112 ) ) ;
#23660 = PRESENTATION_LAYER_ASSIGNMENT (  '', '', ( #99744 ) ) ;
#23661 = CARTESIAN_POINT ( 'NONE',  ( 0.000000000000000000, 12.30000000000000071, 0.000000000000000000 ) ) ;
#23662 = CARTESIAN_POINT ( 'NONE',  ( -1.499999999999997780, 5.431250000682820378, 1.214306433183764966E-14 ) ) ;
#23664 = ORIENTED_EDGE ( 'NONE', *, *, #81050, .T. ) ;
#23663 = CARTESIAN_POINT ( 'NONE',  ( 5.343967111402722736, -1.155686419774919704, -1.395051459885946699 ) ) ;
#23665 = CARTESIAN_POINT ( 'NONE',  ( 6.968527767744104651, 8.192665819532020777, 1.082531754730558626 ) ) ;
#23666 = CARTESIAN_POINT ( 'NONE',  ( 5.260568668178753349, -1.354309965608934352, 1.290672426560689035 ) ) ;
#23667 = ORIENTED_EDGE ( 'NONE', *, *, #11443, .F. ) ;
#23668 = CARTESIAN_POINT ( 'NONE',  ( 4.469627305733424372, -0.3590069766891256231, 2.038746214588673666 ) ) ;
#23669 = CARTESIAN_POINT ( 'NONE',  ( 0.6124999999999898304, 1.916666666666677621, -1.060881119635962211 ) ) ;
#23670 = CARTESIAN_POINT ( 'NONE',  ( -4.733205024502264102, 7.575804057677677505, 1.082531754730549967 ) ) ;
#23671 = DIRECTION ( 'NONE',  ( 0.000000000000000000, 0.000000000000000000, 1.000000000000000000 ) ) ;
#23672 = CARTESIAN_POINT ( 'NONE',  ( 6.252281394196331554, 10.44607872653774372, 1.040834085586084257E-14 ) ) ;
#23673 = CARTESIAN_POINT ( 'NONE',  ( -7.343712760096452463, 11.71941532008788833, -0.7998128361456291469 ) ) ;
#23674 = DIRECTION ( 'NONE',  ( 0.000000000000000000, -1.000000000000000000, -1.804652791718263484E-16 ) ) ;
#23675 = CARTESIAN_POINT ( 'NONE',  ( 5.075973375179646752, 4.911903417823547002, -0.2129554534070592919 ) ) ;
#23676 = CARTESIAN_POINT ( 'NONE',  ( 1.364683531249986537, -0.5947916663252456049, -0.7879004041258309554 ) ) ;
#23677 = CARTESIAN_POINT ( 'NONE',  ( -1.201851678989727383E-14, 0.7125000000000225597, 1.732050807568877637 ) ) ;
#23679 = CARTESIAN_POINT ( 'NONE',  ( 3.974511587100456822, 7.788680618259193444, 1.040834085586084257E-14 ) ) ;
#23678 = CARTESIAN_POINT ( 'NONE',  ( 3.455471728117681440, 1.544996161402897528, 1.208956721487665087 ) ) ;
#23680 = CARTESIAN_POINT ( 'NONE',  ( 2.126327167286511166, 0.3474154575464418748, -1.985796285822030383 ) ) ;
#23681 = EDGE_CURVE ( 'NONE', #83914, #204424, #109762, .T. ) ;
#23682 = CARTESIAN_POINT ( 'NONE',  ( 11.43204722947019825, 13.65592754026173594, -3.649275849833183649 ) ) ;
#23683 = CARTESIAN_POINT ( 'NONE',  ( -1.772826578343107640, 3.949999999999974420, 0.4499999999999487188 ) ) ;
#23684 = SURFACE_STYLE_USAGE ( .BOTH. , #190447 ) ;
#23685 = CARTESIAN_POINT ( 'NONE',  ( 2.284254421533092216, -1.833544361078912388, -0.3693468884775341077 ) ) ;
#23686 = CARTESIAN_POINT ( 'NONE',  ( 1.364683531249990311, 4.884375000341417916, 1.214306433183764966E-14 ) ) ;
#23687 = CARTESIAN_POINT ( 'NONE',  ( 4.412362193956616885, -2.012844744014946841, -0.04520991500436136873 ) ) ;
#23688 = CARTESIAN_POINT ( 'NONE',  ( -7.832860060393135093, 10.16142270859057462, 1.599625672291295375 ) ) ;
#23690 = CARTESIAN_POINT ( 'NONE',  ( 3.761412437133329068, 1.992871936191454418, -0.7152352101782408766 ) ) ;
#23689 = CARTESIAN_POINT ( 'NONE',  ( -5.802526556968872207, 6.832331073627524454, 1.082531754730548412 ) ) ;
#23691 = DIRECTION ( 'NONE',  ( 0.000000000000000000, 0.000000000000000000, 1.000000000000000000 ) ) ;
#23692 = CARTESIAN_POINT ( 'NONE',  ( 4.475093801846619535, 1.891600172242546840, 0.8420093967692193759 ) ) ;
#23693 = CARTESIAN_POINT ( 'NONE',  ( 5.692444392891300886, 7.734547439830227411, -1.599625672291281386 ) ) ;
#23695 = CARTESIAN_POINT ( 'NONE',  ( 6.620655732516651071, 4.689394895873098434, 2.736297475404291024 ) ) ;
#23694 = CARTESIAN_POINT ( 'NONE',  ( 0.8551579053767807137, 0.4041549552570160575, -2.051131941465775821 ) ) ;
#23697 = ORIENTED_EDGE ( 'NONE', *, *, #192598, .T. ) ;
#23696 = CARTESIAN_POINT ( 'NONE',  ( 6.581069972421211389, -0.09314021972051110543, -1.823315219958022482 ) ) ;
#23698 = CARTESIAN_POINT ( 'NONE',  ( 8.274553823041976841, 8.548067636504127265, 1.040834085586084257E-14 ) ) ;
#23699 = CARTESIAN_POINT ( 'NONE',  ( 0.008622031262369225790, 14.55347103577515000, 11.95585889282743253 ) ) ;
#23700 = CARTESIAN_POINT ( 'NONE',  ( 2.889785579457927245, 6.440540434672811898, -0.3822207396134719715 ) ) ;
#23701 = CARTESIAN_POINT ( 'NONE',  ( -10.97061778408437505, 3.255139717175850933, 6.407648009301818881 ) ) ;
#23702 = CARTESIAN_POINT ( 'NONE',  ( 6.873620692004076105, 10.00267932643801672, -1.082531754730537976 ) ) ;
#23703 = CARTESIAN_POINT ( 'NONE',  ( -1.911686719268548496, 3.274494700676831904, 0.4236673858377323909 ) ) ;
#23704 = CARTESIAN_POINT ( 'NONE',  ( -0.07596920688733227456, -0.7732221873907207943, -1.636987988057141852 ) ) ;
#23705 = CARTESIAN_POINT ( 'NONE',  ( -8.833300774503376473, 10.26427131079744193, 1.199719254218462483 ) ) ;
#23706 = CIRCLE ( 'NONE', #158552, 10.97656854249491509 ) ;
#23707 = CARTESIAN_POINT ( 'NONE',  ( 6.505214776458575265, 6.483838748823460563, 1.040834085586084257E-14 ) ) ;
#23708 = CARTESIAN_POINT ( 'NONE',  ( 8.326672684688649401E-17, 4.400000000000001243, -1.500000000000000222 ) ) ;
#23709 = CARTESIAN_POINT ( 'NONE',  ( 2.507895228403643539, 5.869702166538802501, -0.7216878364870267237 ) ) ;
#23710 = CARTESIAN_POINT ( 'NONE',  ( 3.834746474454188013E-15, 12.34375000068279959, 1.500000000000001554 ) ) ;
#23711 = CARTESIAN_POINT ( 'NONE',  ( 3.171717870593107058, 5.787755718078879674, -1.199719254218446718 ) ) ;
#23712 = ORIENTED_EDGE ( 'NONE', *, *, #204878, .T. ) ;
#23713 = CARTESIAN_POINT ( 'NONE',  ( 6.415638736316127577, -1.319241173714128745, -1.525034172108488573 ) ) ;
#23714 = CARTESIAN_POINT ( 'NONE',  ( -3.131570295076647525, 6.597323077657299528, 1.040834085586084257E-14 ) ) ;
#23715 = CARTESIAN_POINT ( 'NONE',  ( 10.95632728729436067, -7.911711732698780253, -0.3221646467111924927 ) ) ;
#23716 = CARTESIAN_POINT ( 'NONE',  ( -0.1405533004718676759, 7.629137130509054288, -2.320277334263821434 ) ) ;
#23717 = CARTESIAN_POINT ( 'NONE',  ( -4.392478581147607031, 7.108013530438723748, 1.082531754730560403 ) ) ;
#23718 = CARTESIAN_POINT ( 'NONE',  ( 3.708318708537623021, 4.285125567170706695, -1.199719254218446718 ) ) ;
#23719 = CARTESIAN_POINT ( 'NONE',  ( 2.307411487444132270, -1.578694758215667404, -1.177220170345204098 ) ) ;
#23720 = CARTESIAN_POINT ( 'NONE',  ( 4.780875152847498200, 1.674876996157638187, -1.122516304564516565 ) ) ;
#23721 = CARTESIAN_POINT ( 'NONE',  ( -5.585069213825653023, 8.603332285183535433, -1.199719254218440723 ) ) ;
#23723 = EDGE_CURVE ( 'NONE', #187426, #209493, #194736, .T. ) ;
#23722 = CARTESIAN_POINT ( 'NONE',  ( -0.4019237886467001974, 10.30133545031537246, 1.500000000000001998 ) ) ;
#23724 = CARTESIAN_POINT ( 'NONE',  ( 4.927760762764835434, 1.128268568998530563, -1.878541326455762661 ) ) ;
#23725 = DIRECTION ( 'NONE',  ( 0.000000000000000000, 0.000000000000000000, 1.000000000000000000 ) ) ;
#23726 = CARTESIAN_POINT ( 'NONE',  ( 2.713793335149127905, -1.905670363949378165, 0.2809714450454863233 ) ) ;
#23727 = CARTESIAN_POINT ( 'NONE',  ( -7.296259222448620463, 11.66405285949874759, 0.7998128361456481317 ) ) ;
#23728 = CARTESIAN_POINT ( 'NONE',  ( -0.1298852118744256712, 1.416581902219627542, -1.986715197202136185 ) ) ;
#23729 = CARTESIAN_POINT ( 'NONE',  ( 0.3642759247451561322, 2.182245240920151375, -0.3280614795862640820 ) ) ;
#23730 = CARTESIAN_POINT ( 'NONE',  ( -7.116787983951523344, 15.51980677384556984, -9.672274635395138986 ) ) ;
#23731 = CARTESIAN_POINT ( 'NONE',  ( 0.6823417656249934904, 13.19270833367473195, 1.181850606188764807 ) ) ;
#23732 = CARTESIAN_POINT ( 'NONE',  ( 4.123651276850781144, 7.962676922967908411, -0.7998128361456221525 ) ) ;
#23733 = CARTESIAN_POINT ( 'NONE',  ( -6.932145363377542502, -8.169775483750512990, 6.496114076516009916 ) ) ;
#23734 = CARTESIAN_POINT ( 'NONE',  ( 5.261973015879598314, 5.311592404713873172, -0.7216878364870458196 ) ) ;
#23736 = CARTESIAN_POINT ( 'NONE',  ( 3.123692395903770347, -0.3905211382968387102, 1.974689860881967407 ) ) ;
#23735 = CARTESIAN_POINT ( 'NONE',  ( 5.970224376651540155, -1.750504005202535796, -0.5711807346103907612 ) ) ;
#23737 = CARTESIAN_POINT ( 'NONE',  ( 4.886215977948979550, -0.1196125283245419307, 2.295398719017431866 ) ) ;
#23739 = CARTESIAN_POINT ( 'NONE',  ( 2.940123752802700885, -0.9609217279343595930, 1.593531096896059873 ) ) ;
#23738 = PLANE ( 'NONE',  #185521 ) ;
#23740 = CARTESIAN_POINT ( 'NONE',  ( 3.285556943750000070, -0.9843749995220412163, 0.000000000000000000 ) ) ;
#23742 = EDGE_CURVE ( 'NONE', #114098, #88263, #200308, .T. ) ;
#23741 = LINE ( 'NONE', #205688, #147056 ) ;
#23743 = CARTESIAN_POINT ( 'NONE',  ( -5.181187258716735577, 9.196468901811520880, 0.7998128361456481317 ) ) ;
#23744 = CARTESIAN_POINT ( 'NONE',  ( -5.167065940583949413, 5.200867483535597913, 0.000000000000000000 ) ) ;
#23745 = CARTESIAN_POINT ( 'NONE',  ( 6.444877668667830406, -1.679477184941297496, -1.245029935506683838 ) ) ;
#23746 = CARTESIAN_POINT ( 'NONE',  ( 6.493992391265805075, 6.678671999339316656, 1.040834085586084257E-14 ) ) ;
#23747 = VERTEX_POINT ( 'NONE', #209290 ) ;
#23748 = STYLED_ITEM ( 'NONE', ( #3027 ), #21023 ) ;
#23749 = CARTESIAN_POINT ( 'NONE',  ( 10.41114276008972617, -8.296408557652583227, -0.1817271728525790275 ) ) ;
#23750 = CARTESIAN_POINT ( 'NONE',  ( 7.065207446497155708, 9.336104335703744539, 0.000000000000000000 ) ) ;
#23751 = CARTESIAN_POINT ( 'NONE',  ( 6.428329371266205072, 0.9864720512241608175, -1.414751289540659318 ) ) ;
#23752 = CARTESIAN_POINT ( 'NONE',  ( -5.250031796989778066, 7.148123067953287446, 1.599625672291267398 ) ) ;
#23753 = CARTESIAN_POINT ( 'NONE',  ( 2.056849044198369114, -1.066344721839644460, 1.367450411802049182 ) ) ;
#23754 = CARTESIAN_POINT ( 'NONE',  ( 0.2887529476172369103, 1.000000000000000888, -11.89119375935163880 ) ) ;
#23755 = CARTESIAN_POINT ( 'NONE',  ( 3.895595285070167169, 2.800000000000017586, -0.7749999999999935829 ) ) ;
#23756 = CARTESIAN_POINT ( 'NONE',  ( -7.366157530926372488, 7.488271962369228874, -0.7998128361456291469 ) ) ;
#23757 = LINE ( 'NONE', #89862, #53502 ) ;
#23758 = CARTESIAN_POINT ( 'NONE',  ( 6.825048293896172957, -1.981324744236719004, -0.8880960284254543202 ) ) ;
#23759 = CARTESIAN_POINT ( 'NONE',  ( 5.408770660633122063, 1.379882519126625295, -1.195542987486551301 ) ) ;
#23760 = CARTESIAN_POINT ( 'NONE',  ( 2.905073028004667712, -1.633678134795817583, 1.085783093053994453 ) ) ;
#23761 = CARTESIAN_POINT ( 'NONE',  ( 0.6124999999999637401, -0.3541666659838821341, 1.060881119635891157 ) ) ;
#23762 = FACE_OUTER_BOUND ( 'NONE', #36121, .T. ) ;
#23763 = CARTESIAN_POINT ( 'NONE',  ( 7.019370843573166319, 9.212351955633947043, 1.599625672291281386 ) ) ;
#23764 = CARTESIAN_POINT ( 'NONE',  ( 4.231183009085410340, 1.939187816756043237, 0.8583030597293441755 ) ) ;
#23765 = CARTESIAN_POINT ( 'NONE',  ( 6.827182134110223011, 1.235230467647760566, 2.302354205009625954 ) ) ;
#23766 = EDGE_CURVE ( 'NONE', #100853, #149695, #34269, .T. ) ;
#23767 = CARTESIAN_POINT ( 'NONE',  ( 1.762639944428091576, -0.7413553172891698129, -1.933158369416078770 ) ) ;
#23769 = FACE_OUTER_BOUND ( 'NONE', #212598, .T. ) ;
#23768 = DIRECTION ( 'NONE',  ( -1.084202172485508576E-15, 0.5005768354468290715, 0.8656921114426525676 ) ) ;
#23771 = ORIENTED_EDGE ( 'NONE', *, *, #110855, .F. ) ;
#23770 = CARTESIAN_POINT ( 'NONE',  ( 3.211816561499138523, 1.752256602034316213, 1.365123760953767418 ) ) ;
#23772 = CARTESIAN_POINT ( 'NONE',  ( 1.565480925793379274, -1.225038264044479686, 1.944918359529357543 ) ) ;
#23774 = CARTESIAN_POINT ( 'NONE',  ( 0.2390249890181182224, -0.1369461163322066299, -1.930431041017650395 ) ) ;
#23773 = CARTESIAN_POINT ( 'NONE',  ( 8.920901888111989919, 11.43080484092926241, 1.443375672974076540 ) ) ;
#23776 = CARTESIAN_POINT ( 'NONE',  ( 1.001543065824772753E-15, -0.9624999999999998002, 4.012584370867899430 ) ) ;
#23775 = CARTESIAN_POINT ( 'NONE',  ( 5.564695703766185275, 5.456842840674144490, 0.000000000000000000 ) ) ;
#23777 = DIRECTION ( 'NONE',  ( 0.000000000000000000, -1.000000000000000000, 0.000000000000000000 ) ) ;
#23778 = CARTESIAN_POINT ( 'NONE',  ( 6.550350952284553330, -1.418464805562440922, 1.173678288350611609 ) ) ;
#23779 = CARTESIAN_POINT ( 'NONE',  ( -3.240269673027908137, 6.421702286726624465, 0.6780825091596647258 ) ) ;
#23780 = CARTESIAN_POINT ( 'NONE',  ( 2.882959773793275726, -1.768624019741386277, -0.7279546805132871556 ) ) ;
#23781 = CARTESIAN_POINT ( 'NONE',  ( -0.2104748580754391973, 0.7011259924453935310, -2.185273273056092425 ) ) ;
#23782 = CARTESIAN_POINT ( 'NONE',  ( 4.576996085227628797, -0.001753933126501586170, -1.724958192235986232 ) ) ;
#23783 = CARTESIAN_POINT ( 'NONE',  ( 2.483611571103707227, -0.6279893487078170855, 1.916353726171161398 ) ) ;
#23784 = CARTESIAN_POINT ( 'NONE',  ( 3.920743334446879835, -1.585418671752996334, -1.664648107385821030 ) ) ;
#23785 = CARTESIAN_POINT ( 'NONE',  ( 3.655803326253406649, 0.5538646471104657909, -2.193435612772106413 ) ) ;
#23786 = CARTESIAN_POINT ( 'NONE',  ( 5.883451020920152708, 1.946514763749309429, -0.8046133670899023871 ) ) ;
#23787 = CARTESIAN_POINT ( 'NONE',  ( -6.129694847154220305, 8.244672969803623630, -1.443375672974066548 ) ) ;
#23788 = CARTESIAN_POINT ( 'NONE',  ( 5.132005351226563761, 0.9095619001311354701, -1.517971549226182715 ) ) ;
#23790 = CARTESIAN_POINT ( 'NONE',  ( 0.8148889116572692881, 2.119938092393148565, 0.8724386107587696060 ) ) ;
#23789 = CARTESIAN_POINT ( 'NONE',  ( 7.014364370223726830, 9.276787413384745662, -1.599625672291269396 ) ) ;
#23791 = CARTESIAN_POINT ( 'NONE',  ( 6.087831982560696353, -1.832735460234231617, -0.1757473516527594259 ) ) ;
#23792 = CARTESIAN_POINT ( 'NONE',  ( -3.948449050077848632, 5.629609863222681199, 1.599625672291267398 ) ) ;
#23793 = VECTOR ( 'NONE', #128143, 1000.000000000000000 ) ;
#23794 = UNCERTAINTY_MEASURE_WITH_UNIT (LENGTH_MEASURE( 1.000000000000000082E-05 ), #120191, 'distance_accuracy_value', 'NONE');
#23795 = CARTESIAN_POINT ( 'NONE',  ( 6.070311387754347088, -2.079788119406985825, -0.6908379657195939938 ) ) ;
#23796 = CARTESIAN_POINT ( 'NONE',  ( -2.785310492603665367, 5.336947110424484109, 1.199719254218462483 ) ) ;
#23797 = CARTESIAN_POINT ( 'NONE',  ( -7.105996805615566458, 15.47012406969961518, 9.680156245089420963 ) ) ;
#23798 = CARTESIAN_POINT ( 'NONE',  ( 6.268043187460373922, -2.055199631210803624, 0.2494731385529954104 ) ) ;
#23799 = CARTESIAN_POINT ( 'NONE',  ( 0.4445464637146989695, -1.457232572767804379, 1.394089106691732693 ) ) ;
#23800 = CARTESIAN_POINT ( 'NONE',  ( -1.500000000000001332, -1.318749999317178734, 0.000000000000000000 ) ) ;
#23801 = CARTESIAN_POINT ( 'NONE',  ( 4.863854859025781074, 1.905264070129700782, -0.2845116402651908794 ) ) ;
#23802 = CARTESIAN_POINT ( 'NONE',  ( -1.364683531250014514, 10.58854166700806765, -0.7879004041258335089 ) ) ;
#23803 = CARTESIAN_POINT ( 'NONE',  ( -3.633221978782304351, 4.301475732409860697, -1.082531754730549967 ) ) ;
#23804 = CARTESIAN_POINT ( 'NONE',  ( 1.512303732575480675, -0.7424040314494853021, 2.093836701676012879 ) ) ;
#23806 = VERTEX_POINT ( 'NONE', #14293 ) ;
#23805 = CARTESIAN_POINT ( 'NONE',  ( 4.913904330310220558, 4.697586238308844919, 0.000000000000000000 ) ) ;
#23807 = CARTESIAN_POINT ( 'NONE',  ( -3.526529353330355221, 6.168015774643768268, -1.082531754730546636 ) ) ;
#23808 = CARTESIAN_POINT ( 'NONE',  ( 2.530568227245037605, 6.104080031761181857, 0.000000000000000000 ) ) ;
#23809 = CARTESIAN_POINT ( 'NONE',  ( -0.1108833634136767443, 0.0002062650063822807356, -1.896853557917008271 ) ) ;
#23810 = LINE ( 'NONE', #89915, #83681 ) ;
#23811 = VECTOR ( 'NONE', #173429, 1000.000000000000000 ) ;
#23812 = CARTESIAN_POINT ( 'NONE',  ( 0.000000000000000000, 11.29999999999999893, 0.000000000000000000 ) ) ;
#23813 = CARTESIAN_POINT ( 'NONE',  ( 1.419999999999989049, 6.280000000000042881, -2.579999999999995630 ) ) ;
#23814 = CARTESIAN_POINT ( 'NONE',  ( 1.135121963537696566, -0.04462593873827064989, -1.961518378280776354 ) ) ;
#23815 = CARTESIAN_POINT ( 'NONE',  ( -0.6823417656250003738, 2.530208333674753618, -1.181850606188749264 ) ) ;
#23816 = PLANE ( 'NONE',  #95825 ) ;
#23817 = CARTESIAN_POINT ( 'NONE',  ( 6.268018250734934682, -1.947192974725008963, 0.2387856323943157166 ) ) ;
#23818 = CARTESIAN_POINT ( 'NONE',  ( -9.267161690140662600, 10.77044237904097734, -1.199719254218441611 ) ) ;
#23819 = CARTESIAN_POINT ( 'NONE',  ( -5.897433631820158340, 5.982686779986042147, 0.7216878364870317197 ) ) ;
#23820 = CARTESIAN_POINT ( 'NONE',  ( 0.2337813496832439053, -2.066932786716439541, 0.9205801711329018033 ) ) ;
#23822 = EDGE_LOOP ( 'NONE', ( #131877, #85770, #102643, #82449 ) ) ;
#23821 = CARTESIAN_POINT ( 'NONE',  ( -5.530836599371015794, 8.540060901653093950, 1.199719254218452047 ) ) ;
#23823 = CARTESIAN_POINT ( 'NONE',  ( -1.500000000000001332, -1.068749999317178290, 0.000000000000000000 ) ) ;
#23824 = CARTESIAN_POINT ( 'NONE',  ( 0.9482695043977107385, 0.5371953702461745861, 1.791772314883005146 ) ) ;
#23825 = CARTESIAN_POINT ( 'NONE',  ( 0.6681306116654138760, 1.163384174638517177, 1.286150249643343901 ) ) ;
#23827 = CARTESIAN_POINT ( 'NONE',  ( 4.124703146219878214, 0.1084699374758208573, 2.189010777610411740 ) ) ;
#23826 = CARTESIAN_POINT ( 'NONE',  ( 1.360316468749992236, 2.015625000341400685, -1.040834085586084257E-14 ) ) ;
#23828 = CARTESIAN_POINT ( 'NONE',  ( 4.032480619008128819, 1.237564890788948269, -1.947499633988438061 ) ) ;
#23829 = CARTESIAN_POINT ( 'NONE',  ( 0.5146158036630330557, 1.421672375139692246, -1.492246178604545115 ) ) ;
#23830 = CARTESIAN_POINT ( 'NONE',  ( 2.466655979050590197, 0.09513121245676225968, -1.939734245173969640 ) ) ;
#23831 = CARTESIAN_POINT ( 'NONE',  ( -4.080641047588902559, 7.704572288921609058, -0.7216878364870257245 ) ) ;
#23832 = CARTESIAN_POINT ( 'NONE',  ( 5.642871316567687145, 2.044259226470702462, 0.5637153772257290640 ) ) ;
#23833 = CYLINDRICAL_SURFACE ( 'NONE', #150451, 0.3999999999999997446 ) ;
#23834 = CARTESIAN_POINT ( 'NONE',  ( 3.199842427594956185, 1.824118962040650604, 0.8596310190432245868 ) ) ;
#23835 = CARTESIAN_POINT ( 'NONE',  ( -4.026408433134269771, 6.680931691089825541, 1.082531754730560403 ) ) ;
#23836 = CARTESIAN_POINT ( 'NONE',  ( -7.781453819600577582, 8.043060642480948985, 0.000000000000000000 ) ) ;
#23837 = CARTESIAN_POINT ( 'NONE',  ( 8.401248741962376698, 12.95320729893149370, 0.7998128361456462443 ) ) ;
#23838 = CARTESIAN_POINT ( 'NONE',  ( 1.066719475142905216, -1.649486405746130258, -0.7827983987617056494 ) ) ;
#23839 = CARTESIAN_POINT ( 'NONE',  ( -6.286140498591554326, 7.362860665558790707, 1.199719254218452047 ) ) ;
#23840 = CARTESIAN_POINT ( 'NONE',  ( -5.605310199005481664, 5.702455421404705405, 0.3560189469562446973 ) ) ;
#23841 = CARTESIAN_POINT ( 'NONE',  ( -11.30310531956832598, 5.150576456239967627, 5.742040133384030298 ) ) ;
#23842 = ORIENTED_EDGE ( 'NONE', *, *, #214308, .F. ) ;
#23843 = CARTESIAN_POINT ( 'NONE',  ( 5.963760128287220574, 2.030816783491296906, -0.3497918165830601334 ) ) ;
#23845 = MANIFOLD_SOLID_BREP ( 'Fillet2', #4953 ) ;
#23844 = CARTESIAN_POINT ( 'NONE',  ( -6.170369307550858551, 8.292126506933035657, 1.443375672974058777 ) ) ;
#23846 = CARTESIAN_POINT ( 'NONE',  ( -4.009460741339347045, 5.700790169694431420, -1.599625672291256295 ) ) ;
#23847 = CARTESIAN_POINT ( 'NONE',  ( -8.299562589859897699, 12.83457345481192036, -0.7998128361456281477 ) ) ;
#23848 = CARTESIAN_POINT ( 'NONE',  ( 5.320965550519270337, 1.527853097053995191, -1.320967980168601175 ) ) ;
#23850 = ORIENTED_EDGE ( 'NONE', *, *, #121129, .T. ) ;
#23849 = CARTESIAN_POINT ( 'NONE',  ( 5.760436963792294307, 2.218610086356072930, 0.1113587401332209043 ) ) ;
#23851 = CARTESIAN_POINT ( 'NONE',  ( -4.329849954717889915, 6.144853928627882489, 1.599625672291270506 ) ) ;
#23852 = CARTESIAN_POINT ( 'NONE',  ( 6.667912619822566000, 6.673652899414787676, 1.040834085586084257E-14 ) ) ;
#23853 = CARTESIAN_POINT ( 'NONE',  ( 4.592684518728709975, -0.4495978358524716501, -2.011083796685923630 ) ) ;
#23854 = CARTESIAN_POINT ( 'NONE',  ( 4.465470312728934132, -1.956561007648183192, -0.4872041746135646889 ) ) ;
#23855 = EDGE_LOOP ( 'NONE', ( #164371, #62047, #136118, #39169 ) ) ;
#23856 = CARTESIAN_POINT ( 'NONE',  ( 4.539282502477016479, 4.190251095844947926, 0.7998128361456341429 ) ) ;
#23857 = AXIS2_PLACEMENT_3D ( 'NONE', #77589, #176177, #29921 ) ;
#23859 = ORIENTED_EDGE ( 'NONE', *, *, #105774, .T. ) ;
#23858 = CARTESIAN_POINT ( 'NONE',  ( -5.610041701004606196, 9.767075427805856691, -0.7998128361456362523 ) ) ;
#23860 = CARTESIAN_POINT ( 'NONE',  ( 4.771426152247889796, 8.279957873513081879, -0.8122977234717634332 ) ) ;
#23861 = CARTESIAN_POINT ( 'NONE',  ( 3.743517394402117837, -1.942243990624907823, -0.5404084370827856310 ) ) ;
#23862 = CARTESIAN_POINT ( 'NONE',  ( 3.222423357234117436, 0.04607595322191247733, 1.840729346561786661 ) ) ;
#23863 = CARTESIAN_POINT ( 'NONE',  ( 6.387350227241329392, 6.552219065289217603, 2.499999999999828582 ) ) ;
#23864 = CARTESIAN_POINT ( 'NONE',  ( 1.260874316716424470, 0.9392902264234997967, 2.108064829403846208 ) ) ;
#23865 = CARTESIAN_POINT ( 'NONE',  ( 8.167861197590044142, 8.493869250135347215, 0.000000000000000000 ) ) ;
#23866 = CARTESIAN_POINT ( 'NONE',  ( 3.286554482555790191, -2.129011082553730727, -0.3730605165198074835 ) ) ;
#23867 = CARTESIAN_POINT ( 'NONE',  ( 7.397945374551106568, 11.78268670361832093, -0.7998128361456291469 ) ) ;
#23868 = CARTESIAN_POINT ( 'NONE',  ( -5.494078562035765501, 7.432844293840273231, -1.599625672291256295 ) ) ;
#23869 = EDGE_CURVE ( 'NONE', #198793, #28237, #30901, .T. ) ;
#23870 = CARTESIAN_POINT ( 'NONE',  ( -0.003376046620571447263, -7.161464053357565973, -9.586610838029429260 ) ) ;
#23871 = CARTESIAN_POINT ( 'NONE',  ( 2.412791964582483129, 1.669947582624079274, 0.8431454209596804805 ) ) ;
#23872 = AXIS2_PLACEMENT_3D ( 'NONE', #76220, #192085, #174821 ) ;
#23873 = CARTESIAN_POINT ( 'NONE',  ( 6.332890595682218127, 0.1930081403669886009, 1.961983401381848457 ) ) ;
#23875 = CARTESIAN_POINT ( 'NONE',  ( -6.064239847062411926, 10.29697326487330500, 0.000000000000000000 ) ) ;
#23874 = CARTESIAN_POINT ( 'NONE',  ( 1.364683531249990311, 5.113541667008084879, 0.7879004041258500513 ) ) ;
#23877 = CARTESIAN_POINT ( 'NONE',  ( 1.489210700298746692, -0.3264265768355456010, -2.182489157894373033 ) ) ;
#23876 = CARTESIAN_POINT ( 'NONE',  ( -6.196239896645333367, 7.187700286629718605, -1.199719254218446718 ) ) ;
#23878 = LINE ( 'NONE', #140886, #202616 ) ;
#23879 = CARTESIAN_POINT ( 'NONE',  ( 4.599240423533799138, 6.388866465587984322, 1.599625672291267398 ) ) ;
#23880 = CARTESIAN_POINT ( 'NONE',  ( -5.412729640353771465, 7.337937218544611895, 1.599625672291269396 ) ) ;
#23881 = CARTESIAN_POINT ( 'NONE',  ( 11.97929049433705551, 13.80000000000000071, 0.7046979865771805240 ) ) ;
#23882 = CARTESIAN_POINT ( 'NONE',  ( 5.682488568729203493, -1.923295458312636264, -0.4324549907560610307 ) ) ;
#23883 = CARTESIAN_POINT ( 'NONE',  ( 6.076872578159392191, -2.189301982996785245, -0.7299270095633101363 ) ) ;
#23884 = CARTESIAN_POINT ( 'NONE',  ( 6.654761307663171976, -0.4979203083825957110, -1.793151784937331961 ) ) ;
#23885 = CARTESIAN_POINT ( 'NONE',  ( 3.010651042449908221, 0.6904807078514271224, 1.943715162320960088 ) ) ;
#23886 = CARTESIAN_POINT ( 'NONE',  ( 6.155038550924139429, 9.164333495178082600, 1.082531754730558626 ) ) ;
#23887 = ADVANCED_FACE ( 'NONE', ( #16427 ), #164379, .T. ) ;
#23888 = CARTESIAN_POINT ( 'NONE',  ( 7.180978637093494044, 8.406838493811077839, -1.199719254218452047 ) ) ;
#23889 = CARTESIAN_POINT ( 'NONE',  ( 7.605760987142057061, 7.975735361194951523, -0.7216878364870267237 ) ) ;
#23890 = CARTESIAN_POINT ( 'NONE',  ( -0.6823417656250212460, 3.113541667008084879, 1.181850606188767472 ) ) ;
#23891 = CARTESIAN_POINT ( 'NONE',  ( -8.148189797612232610, 14.48010055955566244, 8.855677698438045198 ) ) ;
#23892 = CARTESIAN_POINT ( 'NONE',  ( 4.487385655998873624, 7.218738451098584363, 1.082531754730558626 ) ) ;
#23893 = CARTESIAN_POINT ( 'NONE',  ( 5.863789056686759871, -0.5331677977272324398, 2.104577851170267078 ) ) ;
#23895 = CARTESIAN_POINT ( 'NONE',  ( 4.880324068823122197, -0.2306306682541107433, -1.826696389425507938 ) ) ;
#23894 = CARTESIAN_POINT ( 'NONE',  ( 6.639320575229258559, 0.002292789353198345943, 1.996863816985874118 ) ) ;
#23897 = CARTESIAN_POINT ( 'NONE',  ( 9.549252947205625119, -7.850763007174478503, -0.06856108760741426444 ) ) ;
#23896 = DIRECTION ( 'NONE',  ( -1.000000000000000000, 7.771561172376097755E-16, 4.440892098500627148E-16 ) ) ;
#23898 = CARTESIAN_POINT ( 'NONE',  ( 6.750000000000007994, 7.629137130509070275, 2.600000000000001421 ) ) ;
#23899 = CARTESIAN_POINT ( 'NONE',  ( 0.2634263733268344398, -2.021796075192600295, -1.015562799429880814 ) ) ;
#23900 = CARTESIAN_POINT ( 'NONE',  ( -5.391143034427437364, 6.494952464278877180, 1.342996321926675396 ) ) ;
#23901 = DIRECTION ( 'NONE',  ( 0.000000000000000000, 1.000000000000000000, 0.000000000000000000 ) ) ;
#23902 = CARTESIAN_POINT ( 'NONE',  ( 6.308853223578811509, 6.964933332891984463, 0.9108697706533327443 ) ) ;
#23903 = VECTOR ( 'NONE', #134997, 1000.000000000000000 ) ;
#23904 = CARTESIAN_POINT ( 'NONE',  ( -3.757017964318317471, 6.436919154129725484, 1.082531754730549967 ) ) ;
#23905 = CARTESIAN_POINT ( 'NONE',  ( -1.382866120668046372, 3.383804033233791309, 0.2144190051505676931 ) ) ;
#23906 =( BOUNDED_SURFACE ( )  B_SPLINE_SURFACE ( 1, 2, ( 
 ( #47775, #193982, #110680, #129087, #31508, #45630, #128028, #94387, #80242, #46698, #97583, #81312, #197182, #212354, #15222, #114935, #111747, #12032, #177753, #95463, #147388, #178829, #112815, #211294, #60792, #32555, #13093, #179884, #79173, #65037, #180933, #62919, #30441, #96526, #162574, #146340, #63994, #130146, #196136, #98631, #143159, #176680, #164691, #77030, #126951, #103961, #186249, #37884, #149507, #70351, #185180, #18421, #119194, #100745, #136468, #201421, #20, #16277, #67153, #183062, #134356, #198236, #34675, #150586, #118135, #102887, #165759, #117064, #167884, #19484, #1091, #202487, #200361, #82361, #84496, #166827, #17344, #83426, #53059, #132227, #152699, #148451, #133289, #49873, #54139, #68225, #181986, #66084, #35741, #36804, #115998, #120275, #199295, #33618, #20548, #99688, #151649, #50940, #184121, #2149, #52009, #101816, #3219, #85560, #69286, #168946, #135398, #86632, #4280, #206768, #6424, #141829, #158051, #42172, #38954, #107215, #191576, #72498, #153771, #22670, #88782, #139677, #204620, #5339, #125617, #138597, #43239, #56272, #207831, #154839, #170004, #58402, #59459, #75715, #122430, #21592, #188387, #124557, #40024, #87696, #71422, #171074, #156983, #190515, #137533, #106136, #105036, #9637, #205700, #8572, #74652, #172159, #203549, #23752, #173237, #57335, #140757, #24817, #89856, #123499, #55204, #121349, #155907, #187325, #7492, #73576, #108288, #90919, #174307, #189463, #41106, #25882, #91992, #44296, #77838, #12820, #111479, #130926, #109356, #60520, #177486, #146071, #176421, #11764, #14946, #196919, #175367, #10695, #29100, #145017, #76766, #208889, #81043, #110418, #211022, #126681, #142888, #195863, #13888, #192643, #212084, #64784, #161233, #163371, #160164, #63722, #97312, #128805, #26949, #194787, #28028, #93057, #159095, #95184, #94126, #147128, #213154, #143960, #209955, #62646, #78894, #61592, #127763, #193719, #45362, #96250, #79967, #46423, #112540, #178552, #129880, #30162, #162303, #47504, #113613, #179618, #31238, #167627, #2962, #150326, #815, #118944, #33351, #131965, #115730, #99433, #181721, #180670, #165486, #82096, #117878, #32296, #1893, #182797, #17083, #65818, #98362, #18152, #116799, #83160, #67952, #197977, #149240, #49606, #148189, #48558, #201166, #52806, #35483, #85306, #114677, #66883, #164427, #133027, #16011, #199026, #214191, #50673, #34416, #100488, #19228, #166563, #135150, #84239, #134097, #200105, #183868, #51756, #101560, #151392, #69033, #193361, #111116, #78541, #98024, #129524, #79611, #95896, #11398, #197615, #210673, #212796, #45006, #130578, #31940, #28736, #62301, #94821, #29811, #112190, #177119, #179262, #14594, #161949, #93756, #127388, #30884, #128460, #144658, #115380, #49259, #27661, #160872, #81746, #196568, #13541, #48210, #178194, #147828, #64434, #77476, #159795, #194428, #46069, #145730, #209587, #211730, #63368, #195504, #114322, #12466, #47140, #96963, #163011, #113257, #213847, #80690, #143595, #146781, #180320, #164079, #15659, #65465, #61233, #131616, #136908, #34054, #148880, #20978, #18855, #132664, #181374, #200797, #135838, #202935, #70795, #166189, #4720, #185627, #153145, #102257, #198669, #134790, #17778, #100127, #54578, #168331, #99075, #1526, #201863, #67590, #19926, #83866, #3656, #149957, #32998, #169393, #53509, #50316, #118574, #165128, #133735, #16719, #199742, #51388, #151028, #117509, #82804, #453, #183502, #66521, #37260, #116434, #86012, #182427, #52448, #35110, #101181, #167270, #152086, #84939, #2597, #119644, #68666, #69734, #184560, #103330, #36181, #87075, #202651, #22831, #169104, #19649, #104120, #6584, #20701, #119358, #3382, #55361, #21755, #72663, #56432, #172319, #187485, #120438, #139837, #86794, #185346, #103051, #152861, #4439, #35903, #70509, #69451, #154999, #101978, #121513, #87863, #136624, #201581, #168047, #203713, #153935, #54300, #39115, #53227, #186412, #36968, #135557, #52164, #156069, #7656, #138761, #188554, #105198, #88945, #73740, #38049, #170167, #106298, #5504, #171235, #204778, #71584, #118291, #137693, #122591, #40185, #23909, #90013, #184277 ),
 ( #85722, #151809, #112445, #210927, #15917, #205865, #157145, #62553, #31144, #58562, #111384, #114580, #82000, #57499, #107377, #128716, #30067, #173400, #91085, #180571, #206933, #96157, #8738, #24982, #80942, #113516, #74819, #97218, #164327, #46330, #124716, #45264, #29001, #177387, #189621, #161136, #140919, #163270, #41269, #63630, #162208, #95088, #190675, #12724, #145977, #178458, #78797, #129784, #144920, #194688, #13794, #79868, #123658, #98269, #211989, #14852, #130831, #195765, #147034, #47404, #179524, #213056, #48465, #64686, #196823, #32193, #116693, #214092, #132920, #151285, #183767, #201059, #85201, #182692, #117776, #103596, #65720, #100386, #181622, #131868, #202117, #168584, #2856, #20184, #197876, #84135, #86271, #166457, #83058, #34310, #51653, #150223, #169653, #148087, #99335, #1793, #184817, #715, #50571, #53777, #21238, #49507, #115627, #67850, #35377, #33251, #165384, #119910, #149134, #101452, #16977, #66780, #152342, #52700, #198925, #36447, #18048, #200004, #185886, #133998, #102522, #136101, #167524, #19122, #68925, #135046, #118831, #3920, #69989, #37520, #141473, #207480, #137174, #203198, #123150, #139309, #75361, #24449, #74298, #173957, #23385, #58037, #204255, #54845, #205338, #41819, #55906, #154484, #38594, #90562, #56976, #107932, #91638, #59100, #8213, #155551, #175010, #122063, #72133, #156623, #189107, #140394, #206413, #188027, #40740, #42884, #153411, #39657, #120995, #4981, #125260, #25530, #124201, #157690, #71058, #89497, #9288, #105765, #22305, #171790, #106846, #7131, #108993, #87344, #104671, #73203, #190165, #6063, #172877, #191220, #186962, #170719, #88417, #138241, #62309, #208531, #126324, #146789, #27669, #128468, #192283, #60167, #113266, #145738, #43943, #129532, #196576, #78550, #80698, #77484, #63376, #14601, #46077, #48218, #112197, #93764, #26597, #10338, #94828, #114331, #212805, #64442, #76412, #142522, #194436, #144667, #130586, #178203, #13547, #179270, #177127, #211738, #143603, #110059, #210680, #195513, #209596, #159803, #176071, #29820, #95904, #47149, #30894, #92698, #161957, #160880, #158744, #61240, #11407, #127397, #193369, #45014, #111124, #28744, #12475, #96971, #79619, #163019, #1534, #148888, #115388, #81754, #117515, #149965, #461, #101188, #181382, #66530, #33005, #131624, #180326, #69739, #135844, #134796, #102262, #167277, #2604, #201867, #132672, #99084, #19932, #67596, #18862, #84946, #198678, #31948, #165136, #16727, #50323, #82811, #164086, #116441, #197623, #68673, #15667, #35117, #133742, #182435, #34062, #147836, #183508, #199750, #100133, #151035, #166195, #17786, #83873, #49267, #98032, #53515, #213853, #200802, #168337, #52453, #118578, #65474, #51395, #184566, #86018, #36186, #152091, #3662, #88155, #185633, #104410, #122890, #155290, #172617, #56722, #154223, #89239, #75107, #37266, #71872, #153151, #103336, #173702, #140132, #188849, #206158, #169398, #55648, #57786, #137982, #54585, #5795, #23122, #121804, #141218, #119649, #70801, #187771, #156366, #186705, #22044, #25277, #207228, #20984, #87081, #39403, #6873, #4726, #136914, #91379, #120732, #72951, #202941, #38333, #123946, #24193, #170459, #7950, #203999, #171529, #157439, #105497, #74042, #107673, #139053, #205080, #40485, #106589, #90296, #189915, #41560, #9033, #113012, #179021, #108740, #174767, #94579, #110871, #46897, #210423, #45827, #145491, #209341, #29564, #175821, #26342, #109812, #42631, #126071, #192032, #28488, #93512, #92455, #14350, #27414, #80440, #159553, #96723, #43695, #146539, #162772, #63123, #30639, #194182, #10093, #12223, #11150, #77227, #58852, #111948, #190965, #143346, #13299, #60989, #177950, #127142, #129287, #95656, #125008, #44763, #161707, #79372, #193114, #211486, #176876, #158494, #160622, #78296, #144421, #62065, #76167, #142272, #128220, #208283, #195263, #59914, #131379, #19686, #34863, #35938, #118329, #49016, #102018, #98833, #100937, #32751, #184314, #130338, #213602, #84698, #168086, #115135, #163836, #81505, #181130, #68424, #99889, #50075, #66281, #196327, #85764, #164883, #183259, #15415, #167024, #2348, #65228 ) ),
 .UNSPECIFIED., .F., .F., .F. ) 
 B_SPLINE_SURFACE_WITH_KNOTS ( ( 2, 2 ),
 ( 3, 2, 2, 2, 2, 2, 2, 2, 2, 2, 2, 2, 2, 2, 2, 2, 2, 2, 2, 2, 2, 2, 2, 2, 2, 2, 2, 2, 2, 2, 2, 2, 2, 2, 2, 2, 2, 2, 2, 2, 2, 2, 2, 2, 2, 2, 2, 2, 2, 2, 2, 2, 2, 2, 2, 2, 2, 2, 2, 2, 2, 2, 2, 2, 2, 2, 2, 2, 2, 2, 2, 2, 2, 2, 2, 2, 2, 2, 2, 2, 2, 2, 2, 2, 2, 2, 2, 2, 2, 2, 2, 2, 2, 2, 2, 2, 2, 2, 2, 2, 2, 2, 2, 2, 2, 2, 2, 2, 2, 2, 2, 2, 2, 2, 2, 2, 2, 2, 2, 2, 2, 2, 2, 2, 2, 2, 2, 2, 2, 2, 2, 2, 2, 2, 2, 2, 2, 2, 2, 2, 2, 2, 2, 2, 2, 2, 2, 2, 2, 2, 2, 2, 2, 2, 2, 2, 2, 2, 2, 2, 2, 2, 2, 2, 2, 2, 2, 2, 2, 2, 2, 2, 2, 2, 2, 2, 2, 2, 2, 2, 2, 2, 2, 2, 2, 2, 2, 2, 2, 2, 2, 2, 2, 2, 2, 2, 2, 2, 2, 2, 2, 2, 2, 2, 2, 2, 2, 2, 2, 2, 2, 2, 2, 2, 2, 2, 2, 2, 2, 2, 2, 2, 2, 2, 2, 2, 2, 2, 2, 2, 2, 2, 2, 2, 2, 2, 2, 2, 2, 2, 3 ),
 ( 0.000000000000000000, 1.000000000000000000 ),
 ( 0.000000000000000000, 0.004166666666666666609, 0.008333333333333333218, 0.01250000000000000069, 0.01666666666666666644, 0.02083333333333333218, 0.02500000000000000139, 0.02916666666666666713, 0.03333333333333333287, 0.03749999999999999861, 0.04166666666666666435, 0.04583333333333333010, 0.05000000000000000278, 0.05416666666666666852, 0.05833333333333333426, 0.06250000000000000000, 0.06666666666666666574, 0.07083333333333333148, 0.07499999999999999722, 0.07916666666666666297, 0.08333333333333332871, 0.08749999999999999445, 0.09166666666666666019, 0.09583333333333333981, 0.1000000000000000056, 0.1041666666666666713, 0.1083333333333333370, 0.1125000000000000028, 0.1166666666666666685, 0.1208333333333333343, 0.1250000000000000000, 0.1291666666666666796, 0.1333333333333333315, 0.1375000000000000111, 0.1416666666666666630, 0.1458333333333333426, 0.1499999999999999944, 0.1541666666666666741, 0.1583333333333333259, 0.1625000000000000056, 0.1666666666666666574, 0.1708333333333333370, 0.1749999999999999889, 0.1791666666666666685, 0.1833333333333333204, 0.1875000000000000000, 0.1916666666666666796, 0.1958333333333333315, 0.2000000000000000111, 0.2041666666666666630, 0.2083333333333333426, 0.2124999999999999944, 0.2166666666666666741, 0.2208333333333333259, 0.2250000000000000056, 0.2291666666666666574, 0.2333333333333333370, 0.2374999999999999889, 0.2416666666666666685, 0.2458333333333333204, 0.2500000000000000000, 0.2541666666666666519, 0.2583333333333333592, 0.2625000000000000111, 0.2666666666666666630, 0.2708333333333333148, 0.2750000000000000222, 0.2791666666666666741, 0.2833333333333333259, 0.2874999999999999778, 0.2916666666666666852, 0.2958333333333333370, 0.2999999999999999889, 0.3041666666666666408, 0.3083333333333333481, 0.3125000000000000000, 0.3166666666666666519, 0.3208333333333333592, 0.3250000000000000111, 0.3291666666666666630, 0.3333333333333333148, 0.3375000000000000222, 0.3416666666666666741, 0.3458333333333333259, 0.3499999999999999778, 0.3541666666666666852, 0.3583333333333333370, 0.3624999999999999889, 0.3666666666666666408, 0.3708333333333333481, 0.3750000000000000000, 0.3791666666666666519, 0.3833333333333333592, 0.3875000000000000111, 0.3916666666666666630, 0.3958333333333333148, 0.4000000000000000222, 0.4041666666666666741, 0.4083333333333333259, 0.4124999999999999778, 0.4166666666666666852, 0.4208333333333333370, 0.4249999999999999889, 0.4291666666666666408, 0.4333333333333333481, 0.4375000000000000000, 0.4416666666666666519, 0.4458333333333333592, 0.4500000000000000111, 0.4541666666666666630, 0.4583333333333333148, 0.4625000000000000222, 0.4666666666666666741, 0.4708333333333333259, 0.4749999999999999778, 0.4791666666666666852, 0.4833333333333333370, 0.4874999999999999889, 0.4916666666666666408, 0.4958333333333333481, 0.5000000000000000000, 0.5041666666666666519, 0.5083333333333333037, 0.5124999999999999556, 0.5166666666666667185, 0.5208333333333333703, 0.5250000000000000222, 0.5291666666666666741, 0.5333333333333333259, 0.5374999999999999778, 0.5416666666666666297, 0.5458333333333332815, 0.5500000000000000444, 0.5541666666666666963, 0.5583333333333333481, 0.5625000000000000000, 0.5666666666666666519, 0.5708333333333333037, 0.5749999999999999556, 0.5791666666666667185, 0.5833333333333333703, 0.5875000000000000222, 0.5916666666666666741, 0.5958333333333333259, 0.5999999999999999778, 0.6041666666666666297, 0.6083333333333332815, 0.6125000000000000444, 0.6166666666666666963, 0.6208333333333333481, 0.6250000000000000000, 0.6291666666666666519, 0.6333333333333333037, 0.6374999999999999556, 0.6416666666666667185, 0.6458333333333333703, 0.6500000000000000222, 0.6541666666666666741, 0.6583333333333333259, 0.6624999999999999778, 0.6666666666666666297, 0.6708333333333332815, 0.6750000000000000444, 0.6791666666666666963, 0.6833333333333333481, 0.6875000000000000000, 0.6916666666666666519, 0.6958333333333333037, 0.6999999999999999556, 0.7041666666666667185, 0.7083333333333333703, 0.7125000000000000222, 0.7166666666666666741, 0.7208333333333333259, 0.7249999999999999778, 0.7291666666666666297, 0.7333333333333332815, 0.7375000000000000444, 0.7416666666666666963, 0.7458333333333333481, 0.7500000000000000000, 0.7541666666666666519, 0.7583333333333333037, 0.7624999999999999556, 0.7666666666666667185, 0.7708333333333333703, 0.7750000000000000222, 0.7791666666666666741, 0.7833333333333333259, 0.7874999999999999778, 0.7916666666666666297, 0.7958333333333332815, 0.8000000000000000444, 0.8041666666666666963, 0.8083333333333333481, 0.8125000000000000000, 0.8166666666666666519, 0.8208333333333333037, 0.8249999999999999556, 0.8291666666666667185, 0.8333333333333333703, 0.8375000000000000222, 0.8416666666666666741, 0.8458333333333333259, 0.8499999999999999778, 0.8541666666666666297, 0.8583333333333332815, 0.8625000000000000444, 0.8666666666666666963, 0.8708333333333333481, 0.8750000000000000000, 0.8791666666666666519, 0.8833333333333333037, 0.8874999999999999556, 0.8916666666666667185, 0.8958333333333333703, 0.9000000000000000222, 0.9041666666666666741, 0.9083333333333333259, 0.9124999999999999778, 0.9166666666666666297, 0.9208333333333332815, 0.9250000000000000444, 0.9291666666666666963, 0.9333333333333333481, 0.9375000000000000000, 0.9416666666666666519, 0.9458333333333333037, 0.9499999999999999556, 0.9541666666666667185, 0.9583333333333333703, 0.9625000000000000222, 0.9666666666666666741, 0.9708333333333333259, 0.9749999999999999778, 0.9791666666666666297, 0.9833333333333332815, 0.9875000000000000444, 0.9916666666666666963, 0.9958333333333333481, 1.000000000000000000 ),
 .UNSPECIFIED. ) 
 GEOMETRIC_REPRESENTATION_ITEM ( )  RATIONAL_B_SPLINE_SURFACE ( (
 ( 1.000000000000000000, 0.8660254037844387076, 1.000000000000000000, 0.8660254037844387076, 1.000000000000000000, 0.8660254037844387076, 1.000000000000000000, 0.8660254037844387076, 1.000000000000000000, 0.8660254037844387076, 1.000000000000000000, 0.8660254037844387076, 1.000000000000000000, 0.8660254037844387076, 1.000000000000000000, 0.8660254037844387076, 1.000000000000000000, 0.8660254037844387076, 1.000000000000000000, 0.8660254037844387076, 1.000000000000000000, 0.8660254037844387076, 1.000000000000000000, 0.8660254037844387076, 1.000000000000000000, 0.8660254037844387076, 1.000000000000000000, 0.8660254037844387076, 1.000000000000000000, 0.8660254037844387076, 1.000000000000000000, 0.8660254037844387076, 1.000000000000000000, 0.8660254037844387076, 1.000000000000000000, 0.8660254037844387076, 1.000000000000000000, 0.8660254037844387076, 1.000000000000000000, 0.8660254037844387076, 1.000000000000000000, 0.8660254037844387076, 1.000000000000000000, 0.8660254037844387076, 1.000000000000000000, 0.8660254037844387076, 1.000000000000000000, 0.8660254037844387076, 1.000000000000000000, 0.8660254037844387076, 1.000000000000000000, 0.8660254037844387076, 1.000000000000000000, 0.8660254037844387076, 1.000000000000000000, 0.8660254037844387076, 1.000000000000000000, 0.8660254037844387076, 1.000000000000000000, 0.8660254037844387076, 1.000000000000000000, 0.8660254037844387076, 1.000000000000000000, 0.8660254037844387076, 1.000000000000000000, 0.8660254037844387076, 1.000000000000000000, 0.8660254037844387076, 1.000000000000000000, 0.8660254037844387076, 1.000000000000000000, 0.8660254037844387076, 1.000000000000000000, 0.8660254037844387076, 1.000000000000000000, 0.8660254037844387076, 1.000000000000000000, 0.8660254037844387076, 1.000000000000000000, 0.8660254037844387076, 1.000000000000000000, 0.8660254037844387076, 1.000000000000000000, 0.8660254037844387076, 1.000000000000000000, 0.8660254037844387076, 1.000000000000000000, 0.8660254037844387076, 1.000000000000000000, 0.8660254037844387076, 1.000000000000000000, 0.8660254037844387076, 1.000000000000000000, 0.8660254037844387076, 1.000000000000000000, 0.8660254037844387076, 1.000000000000000000, 0.8660254037844387076, 1.000000000000000000, 0.8660254037844387076, 1.000000000000000000, 0.8660254037844387076, 1.000000000000000000, 0.8660254037844387076, 1.000000000000000000, 0.8660254037844387076, 1.000000000000000000, 0.8660254037844387076, 1.000000000000000000, 0.8660254037844387076, 1.000000000000000000, 0.8660254037844387076, 1.000000000000000000, 0.8660254037844387076, 1.000000000000000000, 0.8660254037844387076, 1.000000000000000000, 0.8660254037844387076, 1.000000000000000000, 0.8660254037844387076, 1.000000000000000000, 0.8660254037844387076, 1.000000000000000000, 0.8660254037844387076, 1.000000000000000000, 0.8660254037844387076, 1.000000000000000000, 0.8660254037844387076, 1.000000000000000000, 0.8660254037844387076, 1.000000000000000000, 0.8660254037844387076, 1.000000000000000000, 0.8660254037844387076, 1.000000000000000000, 0.8660254037844387076, 1.000000000000000000, 0.8660254037844387076, 1.000000000000000000, 0.8660254037844387076, 1.000000000000000000, 0.8660254037844387076, 1.000000000000000000, 0.8660254037844387076, 1.000000000000000000, 0.8660254037844387076, 1.000000000000000000, 0.8660254037844387076, 1.000000000000000000, 0.8660254037844387076, 1.000000000000000000, 0.8660254037844387076, 1.000000000000000000, 0.8660254037844387076, 1.000000000000000000, 0.8660254037844387076, 1.000000000000000000, 0.8660254037844387076, 1.000000000000000000, 0.8660254037844387076, 1.000000000000000000, 0.8660254037844387076, 1.000000000000000000, 0.8660254037844387076, 1.000000000000000000, 0.8660254037844387076, 1.000000000000000000, 0.8660254037844387076, 1.000000000000000000, 0.8660254037844387076, 1.000000000000000000, 0.8660254037844387076, 1.000000000000000000, 0.8660254037844387076, 1.000000000000000000, 0.8660254037844387076, 1.000000000000000000, 0.8660254037844387076, 1.000000000000000000, 0.8660254037844387076, 1.000000000000000000, 0.8660254037844387076, 1.000000000000000000, 0.8660254037844387076, 1.000000000000000000, 0.8660254037844387076, 1.000000000000000000, 0.8660254037844387076, 1.000000000000000000, 0.8660254037844387076, 1.000000000000000000, 0.8660254037844387076, 1.000000000000000000, 0.8660254037844387076, 1.000000000000000000, 0.8660254037844387076, 1.000000000000000000, 0.8660254037844387076, 1.000000000000000000, 0.8660254037844387076, 1.000000000000000000, 0.8660254037844387076, 1.000000000000000000, 0.8660254037844387076, 1.000000000000000000, 0.8660254037844387076, 1.000000000000000000, 0.8660254037844387076, 1.000000000000000000, 0.8660254037844387076, 1.000000000000000000, 0.8660254037844387076, 1.000000000000000000, 0.8660254037844387076, 1.000000000000000000, 0.8660254037844387076, 1.000000000000000000, 0.8660254037844387076, 1.000000000000000000, 0.8660254037844387076, 1.000000000000000000, 0.8660254037844387076, 1.000000000000000000, 0.8660254037844387076, 1.000000000000000000, 0.8660254037844387076, 1.000000000000000000, 0.8660254037844387076, 1.000000000000000000, 0.8660254037844387076, 1.000000000000000000, 0.8660254037844387076, 1.000000000000000000, 0.8660254037844387076, 1.000000000000000000, 0.8660254037844387076, 1.000000000000000000, 0.8660254037844387076, 1.000000000000000000, 0.8660254037844387076, 1.000000000000000000, 0.8660254037844387076, 1.000000000000000000, 0.8660254037844387076, 1.000000000000000000, 0.8660254037844387076, 1.000000000000000000, 0.8660254037844387076, 1.000000000000000000, 0.8660254037844387076, 1.000000000000000000, 0.8660254037844387076, 1.000000000000000000, 0.8660254037844387076, 1.000000000000000000, 0.8660254037844387076, 1.000000000000000000, 0.8660254037844387076, 1.000000000000000000, 0.8660254037844387076, 1.000000000000000000, 0.8660254037844387076, 1.000000000000000000, 0.8660254037844387076, 1.000000000000000000, 0.8660254037844387076, 1.000000000000000000, 0.8660254037844387076, 1.000000000000000000, 0.8660254037844387076, 1.000000000000000000, 0.8660254037844387076, 1.000000000000000000, 0.8660254037844387076, 1.000000000000000000, 0.8660254037844387076, 1.000000000000000000, 0.8660254037844387076, 1.000000000000000000, 0.8660254037844387076, 1.000000000000000000, 0.8660254037844387076, 1.000000000000000000, 0.8660254037844387076, 1.000000000000000000, 0.8660254037844387076, 1.000000000000000000, 0.8660254037844387076, 1.000000000000000000, 0.8660254037844387076, 1.000000000000000000, 0.8660254037844387076, 1.000000000000000000, 0.8660254037844387076, 1.000000000000000000, 0.8660254037844387076, 1.000000000000000000, 0.8660254037844387076, 1.000000000000000000, 0.8660254037844387076, 1.000000000000000000, 0.8660254037844387076, 1.000000000000000000, 0.8660254037844387076, 1.000000000000000000, 0.8660254037844387076, 1.000000000000000000, 0.8660254037844387076, 1.000000000000000000, 0.8660254037844387076, 1.000000000000000000, 0.8660254037844387076, 1.000000000000000000, 0.8660254037844387076, 1.000000000000000000, 0.8660254037844387076, 1.000000000000000000, 0.8660254037844387076, 1.000000000000000000, 0.8660254037844387076, 1.000000000000000000, 0.8660254037844387076, 1.000000000000000000, 0.8660254037844387076, 1.000000000000000000, 0.8660254037844387076, 1.000000000000000000, 0.8660254037844387076, 1.000000000000000000, 0.8660254037844387076, 1.000000000000000000, 0.8660254037844387076, 1.000000000000000000, 0.8660254037844387076, 1.000000000000000000, 0.8660254037844387076, 1.000000000000000000, 0.8660254037844387076, 1.000000000000000000, 0.8660254037844387076, 1.000000000000000000, 0.8660254037844387076, 1.000000000000000000, 0.8660254037844387076, 1.000000000000000000, 0.8660254037844387076, 1.000000000000000000, 0.8660254037844387076, 1.000000000000000000, 0.8660254037844387076, 1.000000000000000000, 0.8660254037844387076, 1.000000000000000000, 0.8660254037844387076, 1.000000000000000000, 0.8660254037844387076, 1.000000000000000000, 0.8660254037844387076, 1.000000000000000000, 0.8660254037844387076, 1.000000000000000000, 0.8660254037844387076, 1.000000000000000000, 0.8660254037844387076, 1.000000000000000000, 0.8660254037844387076, 1.000000000000000000, 0.8660254037844387076, 1.000000000000000000, 0.8660254037844387076, 1.000000000000000000, 0.8660254037844387076, 1.000000000000000000, 0.8660254037844387076, 1.000000000000000000, 0.8660254037844387076, 1.000000000000000000, 0.8660254037844387076, 1.000000000000000000, 0.8660254037844387076, 1.000000000000000000, 0.8660254037844387076, 1.000000000000000000, 0.8660254037844387076, 1.000000000000000000, 0.8660254037844387076, 1.000000000000000000, 0.8660254037844387076, 1.000000000000000000, 0.8660254037844387076, 1.000000000000000000, 0.8660254037844387076, 1.000000000000000000, 0.8660254037844387076, 1.000000000000000000, 0.8660254037844387076, 1.000000000000000000, 0.8660254037844387076, 1.000000000000000000, 0.8660254037844387076, 1.000000000000000000, 0.8660254037844387076, 1.000000000000000000, 0.8660254037844387076, 1.000000000000000000, 0.8660254037844387076, 1.000000000000000000, 0.8660254037844387076, 1.000000000000000000, 0.8660254037844387076, 1.000000000000000000, 0.8660254037844387076, 1.000000000000000000, 0.8660254037844387076, 1.000000000000000000, 0.8660254037844387076, 1.000000000000000000, 0.8660254037844387076, 1.000000000000000000, 0.8660254037844387076, 1.000000000000000000, 0.8660254037844387076, 1.000000000000000000, 0.8660254037844387076, 1.000000000000000000, 0.8660254037844387076, 1.000000000000000000, 0.8660254037844387076, 1.000000000000000000, 0.8660254037844387076, 1.000000000000000000, 0.8660254037844387076, 1.000000000000000000, 0.8660254037844387076, 1.000000000000000000, 0.8660254037844387076, 1.000000000000000000, 0.8660254037844387076, 1.000000000000000000, 0.8660254037844387076, 1.000000000000000000, 0.8660254037844387076, 1.000000000000000000, 0.8660254037844387076, 1.000000000000000000, 0.8660254037844387076, 1.000000000000000000, 0.8660254037844387076, 1.000000000000000000, 0.8660254037844387076, 1.000000000000000000, 0.8660254037844387076, 1.000000000000000000, 0.8660254037844387076, 1.000000000000000000, 0.8660254037844387076, 1.000000000000000000, 0.8660254037844387076, 1.000000000000000000, 0.8660254037844387076, 1.000000000000000000, 0.8660254037844387076, 1.000000000000000000, 0.8660254037844387076, 1.000000000000000000, 0.8660254037844387076, 1.000000000000000000, 0.8660254037844387076, 1.000000000000000000, 0.8660254037844387076, 1.000000000000000000, 0.8660254037844387076, 1.000000000000000000, 0.8660254037844387076, 1.000000000000000000, 0.8660254037844387076, 1.000000000000000000, 0.8660254037844387076, 1.000000000000000000, 0.8660254037844387076, 1.000000000000000000),
 ( 1.000000000000000000, 0.8660254037844387076, 1.000000000000000000, 0.8660254037844387076, 1.000000000000000000, 0.8660254037844387076, 1.000000000000000000, 0.8660254037844387076, 1.000000000000000000, 0.8660254037844387076, 1.000000000000000000, 0.8660254037844387076, 1.000000000000000000, 0.8660254037844387076, 1.000000000000000000, 0.8660254037844387076, 1.000000000000000000, 0.8660254037844387076, 1.000000000000000000, 0.8660254037844387076, 1.000000000000000000, 0.8660254037844387076, 1.000000000000000000, 0.8660254037844387076, 1.000000000000000000, 0.8660254037844387076, 1.000000000000000000, 0.8660254037844387076, 1.000000000000000000, 0.8660254037844387076, 1.000000000000000000, 0.8660254037844387076, 1.000000000000000000, 0.8660254037844387076, 1.000000000000000000, 0.8660254037844387076, 1.000000000000000000, 0.8660254037844387076, 1.000000000000000000, 0.8660254037844387076, 1.000000000000000000, 0.8660254037844387076, 1.000000000000000000, 0.8660254037844387076, 1.000000000000000000, 0.8660254037844387076, 1.000000000000000000, 0.8660254037844387076, 1.000000000000000000, 0.8660254037844387076, 1.000000000000000000, 0.8660254037844387076, 1.000000000000000000, 0.8660254037844387076, 1.000000000000000000, 0.8660254037844387076, 1.000000000000000000, 0.8660254037844387076, 1.000000000000000000, 0.8660254037844387076, 1.000000000000000000, 0.8660254037844387076, 1.000000000000000000, 0.8660254037844387076, 1.000000000000000000, 0.8660254037844387076, 1.000000000000000000, 0.8660254037844387076, 1.000000000000000000, 0.8660254037844387076, 1.000000000000000000, 0.8660254037844387076, 1.000000000000000000, 0.8660254037844387076, 1.000000000000000000, 0.8660254037844387076, 1.000000000000000000, 0.8660254037844387076, 1.000000000000000000, 0.8660254037844387076, 1.000000000000000000, 0.8660254037844387076, 1.000000000000000000, 0.8660254037844387076, 1.000000000000000000, 0.8660254037844387076, 1.000000000000000000, 0.8660254037844387076, 1.000000000000000000, 0.8660254037844387076, 1.000000000000000000, 0.8660254037844387076, 1.000000000000000000, 0.8660254037844387076, 1.000000000000000000, 0.8660254037844387076, 1.000000000000000000, 0.8660254037844387076, 1.000000000000000000, 0.8660254037844387076, 1.000000000000000000, 0.8660254037844387076, 1.000000000000000000, 0.8660254037844387076, 1.000000000000000000, 0.8660254037844387076, 1.000000000000000000, 0.8660254037844387076, 1.000000000000000000, 0.8660254037844387076, 1.000000000000000000, 0.8660254037844387076, 1.000000000000000000, 0.8660254037844387076, 1.000000000000000000, 0.8660254037844387076, 1.000000000000000000, 0.8660254037844387076, 1.000000000000000000, 0.8660254037844387076, 1.000000000000000000, 0.8660254037844387076, 1.000000000000000000, 0.8660254037844387076, 1.000000000000000000, 0.8660254037844387076, 1.000000000000000000, 0.8660254037844387076, 1.000000000000000000, 0.8660254037844387076, 1.000000000000000000, 0.8660254037844387076, 1.000000000000000000, 0.8660254037844387076, 1.000000000000000000, 0.8660254037844387076, 1.000000000000000000, 0.8660254037844387076, 1.000000000000000000, 0.8660254037844387076, 1.000000000000000000, 0.8660254037844387076, 1.000000000000000000, 0.8660254037844387076, 1.000000000000000000, 0.8660254037844387076, 1.000000000000000000, 0.8660254037844387076, 1.000000000000000000, 0.8660254037844387076, 1.000000000000000000, 0.8660254037844387076, 1.000000000000000000, 0.8660254037844387076, 1.000000000000000000, 0.8660254037844387076, 1.000000000000000000, 0.8660254037844387076, 1.000000000000000000, 0.8660254037844387076, 1.000000000000000000, 0.8660254037844387076, 1.000000000000000000, 0.8660254037844387076, 1.000000000000000000, 0.8660254037844387076, 1.000000000000000000, 0.8660254037844387076, 1.000000000000000000, 0.8660254037844387076, 1.000000000000000000, 0.8660254037844387076, 1.000000000000000000, 0.8660254037844387076, 1.000000000000000000, 0.8660254037844387076, 1.000000000000000000, 0.8660254037844387076, 1.000000000000000000, 0.8660254037844387076, 1.000000000000000000, 0.8660254037844387076, 1.000000000000000000, 0.8660254037844387076, 1.000000000000000000, 0.8660254037844387076, 1.000000000000000000, 0.8660254037844387076, 1.000000000000000000, 0.8660254037844387076, 1.000000000000000000, 0.8660254037844387076, 1.000000000000000000, 0.8660254037844387076, 1.000000000000000000, 0.8660254037844387076, 1.000000000000000000, 0.8660254037844387076, 1.000000000000000000, 0.8660254037844387076, 1.000000000000000000, 0.8660254037844387076, 1.000000000000000000, 0.8660254037844387076, 1.000000000000000000, 0.8660254037844387076, 1.000000000000000000, 0.8660254037844387076, 1.000000000000000000, 0.8660254037844387076, 1.000000000000000000, 0.8660254037844387076, 1.000000000000000000, 0.8660254037844387076, 1.000000000000000000, 0.8660254037844387076, 1.000000000000000000, 0.8660254037844387076, 1.000000000000000000, 0.8660254037844387076, 1.000000000000000000, 0.8660254037844387076, 1.000000000000000000, 0.8660254037844387076, 1.000000000000000000, 0.8660254037844387076, 1.000000000000000000, 0.8660254037844387076, 1.000000000000000000, 0.8660254037844387076, 1.000000000000000000, 0.8660254037844387076, 1.000000000000000000, 0.8660254037844387076, 1.000000000000000000, 0.8660254037844387076, 1.000000000000000000, 0.8660254037844387076, 1.000000000000000000, 0.8660254037844387076, 1.000000000000000000, 0.8660254037844387076, 1.000000000000000000, 0.8660254037844387076, 1.000000000000000000, 0.8660254037844387076, 1.000000000000000000, 0.8660254037844387076, 1.000000000000000000, 0.8660254037844387076, 1.000000000000000000, 0.8660254037844387076, 1.000000000000000000, 0.8660254037844387076, 1.000000000000000000, 0.8660254037844387076, 1.000000000000000000, 0.8660254037844387076, 1.000000000000000000, 0.8660254037844387076, 1.000000000000000000, 0.8660254037844387076, 1.000000000000000000, 0.8660254037844387076, 1.000000000000000000, 0.8660254037844387076, 1.000000000000000000, 0.8660254037844387076, 1.000000000000000000, 0.8660254037844387076, 1.000000000000000000, 0.8660254037844387076, 1.000000000000000000, 0.8660254037844387076, 1.000000000000000000, 0.8660254037844387076, 1.000000000000000000, 0.8660254037844387076, 1.000000000000000000, 0.8660254037844387076, 1.000000000000000000, 0.8660254037844387076, 1.000000000000000000, 0.8660254037844387076, 1.000000000000000000, 0.8660254037844387076, 1.000000000000000000, 0.8660254037844387076, 1.000000000000000000, 0.8660254037844387076, 1.000000000000000000, 0.8660254037844387076, 1.000000000000000000, 0.8660254037844387076, 1.000000000000000000, 0.8660254037844387076, 1.000000000000000000, 0.8660254037844387076, 1.000000000000000000, 0.8660254037844387076, 1.000000000000000000, 0.8660254037844387076, 1.000000000000000000, 0.8660254037844387076, 1.000000000000000000, 0.8660254037844387076, 1.000000000000000000, 0.8660254037844387076, 1.000000000000000000, 0.8660254037844387076, 1.000000000000000000, 0.8660254037844387076, 1.000000000000000000, 0.8660254037844387076, 1.000000000000000000, 0.8660254037844387076, 1.000000000000000000, 0.8660254037844387076, 1.000000000000000000, 0.8660254037844387076, 1.000000000000000000, 0.8660254037844387076, 1.000000000000000000, 0.8660254037844387076, 1.000000000000000000, 0.8660254037844387076, 1.000000000000000000, 0.8660254037844387076, 1.000000000000000000, 0.8660254037844387076, 1.000000000000000000, 0.8660254037844387076, 1.000000000000000000, 0.8660254037844387076, 1.000000000000000000, 0.8660254037844387076, 1.000000000000000000, 0.8660254037844387076, 1.000000000000000000, 0.8660254037844387076, 1.000000000000000000, 0.8660254037844387076, 1.000000000000000000, 0.8660254037844387076, 1.000000000000000000, 0.8660254037844387076, 1.000000000000000000, 0.8660254037844387076, 1.000000000000000000, 0.8660254037844387076, 1.000000000000000000, 0.8660254037844387076, 1.000000000000000000, 0.8660254037844387076, 1.000000000000000000, 0.8660254037844387076, 1.000000000000000000, 0.8660254037844387076, 1.000000000000000000, 0.8660254037844387076, 1.000000000000000000, 0.8660254037844387076, 1.000000000000000000, 0.8660254037844387076, 1.000000000000000000, 0.8660254037844387076, 1.000000000000000000, 0.8660254037844387076, 1.000000000000000000, 0.8660254037844387076, 1.000000000000000000, 0.8660254037844387076, 1.000000000000000000, 0.8660254037844387076, 1.000000000000000000, 0.8660254037844387076, 1.000000000000000000, 0.8660254037844387076, 1.000000000000000000, 0.8660254037844387076, 1.000000000000000000, 0.8660254037844387076, 1.000000000000000000, 0.8660254037844387076, 1.000000000000000000, 0.8660254037844387076, 1.000000000000000000, 0.8660254037844387076, 1.000000000000000000, 0.8660254037844387076, 1.000000000000000000, 0.8660254037844387076, 1.000000000000000000, 0.8660254037844387076, 1.000000000000000000, 0.8660254037844387076, 1.000000000000000000, 0.8660254037844387076, 1.000000000000000000, 0.8660254037844387076, 1.000000000000000000, 0.8660254037844387076, 1.000000000000000000, 0.8660254037844387076, 1.000000000000000000, 0.8660254037844387076, 1.000000000000000000, 0.8660254037844387076, 1.000000000000000000, 0.8660254037844387076, 1.000000000000000000, 0.8660254037844387076, 1.000000000000000000, 0.8660254037844387076, 1.000000000000000000, 0.8660254037844387076, 1.000000000000000000, 0.8660254037844387076, 1.000000000000000000, 0.8660254037844387076, 1.000000000000000000, 0.8660254037844387076, 1.000000000000000000, 0.8660254037844387076, 1.000000000000000000, 0.8660254037844387076, 1.000000000000000000, 0.8660254037844387076, 1.000000000000000000, 0.8660254037844387076, 1.000000000000000000, 0.8660254037844387076, 1.000000000000000000, 0.8660254037844387076, 1.000000000000000000, 0.8660254037844387076, 1.000000000000000000, 0.8660254037844387076, 1.000000000000000000, 0.8660254037844387076, 1.000000000000000000, 0.8660254037844387076, 1.000000000000000000, 0.8660254037844387076, 1.000000000000000000, 0.8660254037844387076, 1.000000000000000000, 0.8660254037844387076, 1.000000000000000000, 0.8660254037844387076, 1.000000000000000000, 0.8660254037844387076, 1.000000000000000000, 0.8660254037844387076, 1.000000000000000000, 0.8660254037844387076, 1.000000000000000000, 0.8660254037844387076, 1.000000000000000000, 0.8660254037844387076, 1.000000000000000000, 0.8660254037844387076, 1.000000000000000000, 0.8660254037844387076, 1.000000000000000000, 0.8660254037844387076, 1.000000000000000000, 0.8660254037844387076, 1.000000000000000000, 0.8660254037844387076, 1.000000000000000000, 0.8660254037844387076, 1.000000000000000000, 0.8660254037844387076, 1.000000000000000000, 0.8660254037844387076, 1.000000000000000000, 0.8660254037844387076, 1.000000000000000000, 0.8660254037844387076, 1.000000000000000000) ) ) 
 REPRESENTATION_ITEM ( '' )  SURFACE ( )  );
#23907 = CARTESIAN_POINT ( 'NONE',  ( 1.551229123295729373, 0.5181449431543529993, -1.692289574110398931 ) ) ;
#23908 = CARTESIAN_POINT ( 'NONE',  ( -0.02298948590537253436, -1.708053232816408196, -0.8599758793098393195 ) ) ;
#23910 = CARTESIAN_POINT ( 'NONE',  ( 3.339363673285804079, 0.4624358396413058570, -1.858828564233159675 ) ) ;
#23909 = CARTESIAN_POINT ( 'NONE',  ( -9.130526383799315582, 12.73969898348616070, 1.199719254218462483 ) ) ;
#23911 = CARTESIAN_POINT ( 'NONE',  ( -6.116136693540540570, 10.14959355252369910, 0.000000000000000000 ) ) ;
#23912 = CARTESIAN_POINT ( 'NONE',  ( 3.947672784279113500, 1.424866277981166052, 1.359976495918001627 ) ) ;
#23913 = CARTESIAN_POINT ( 'NONE',  ( 6.381118777440311085, -1.848351591093103652, -0.8147283084726087976 ) ) ;
#23914 = CARTESIAN_POINT ( 'NONE',  ( 2.535844406030359544, 0.8837261853790435717, -1.648756255988912400 ) ) ;
#23916 = ORIENTED_EDGE ( 'NONE', *, *, #28302, .F. ) ;
#23915 = CARTESIAN_POINT ( 'NONE',  ( -0.02319159430949970999, 0.003959926571647092407, -1.810968101872318714 ) ) ;
#23918 = CARTESIAN_POINT ( 'NONE',  ( 3.307826292054301121, 4.882216645528547616, -1.443375672974057666 ) ) ;
#23917 = CARTESIAN_POINT ( 'NONE',  ( 2.086817400036289794, -2.164668306305051804, -0.4287355390964405211 ) ) ;
#23919 = CARTESIAN_POINT ( 'NONE',  ( -1.201851678989727383E-14, 3.134375000341420137, 1.575800808251672791 ) ) ;
#23920 = CARTESIAN_POINT ( 'NONE',  ( 6.777797683793751915, -1.903277019102869616, 0.4755351429900215310 ) ) ;
#23922 = AXIS2_PLACEMENT_3D ( 'NONE', #65993, #47683, #198149 ) ;
#23921 = CARTESIAN_POINT ( 'NONE',  ( 6.238723240582662477, 10.43026088065513513, -0.7998128361456291469 ) ) ;
#23923 = CARTESIAN_POINT ( 'NONE',  ( 11.86239285000045918, 11.29999999999998472, 1.812080536912751283 ) ) ;
#23924 = CARTESIAN_POINT ( 'NONE',  ( -8.912450614902597934, 3.507114751586604129, -8.024806578263023127 ) ) ;
#23925 = CARTESIAN_POINT ( 'NONE',  ( -4.172158584703340445, 5.890604320285754980, -1.599625672291256517 ) ) ;
#23926 = CARTESIAN_POINT ( 'NONE',  ( -7.565242077046479885, -6.863172033215950485, -7.985752187169511629 ) ) ;
#23927 = ORIENTED_EDGE ( 'NONE', *, *, #7268, .T. ) ;
#23928 = CARTESIAN_POINT ( 'NONE',  ( 1.557173632797459684, 1.693725193156172315, -1.190412882225246438 ) ) ;
#23929 = CARTESIAN_POINT ( 'NONE',  ( -1.201851678989727383E-14, 3.087500000000026112, -1.732050807568863648 ) ) ;
#23930 = CARTESIAN_POINT ( 'NONE',  ( 4.286349120214771879, 8.152491073559232859, -0.7998128361456221525 ) ) ;
#23931 = CARTESIAN_POINT ( 'NONE',  ( 5.551137550152489553, 5.441024994791534120, 0.7998128361456352531 ) ) ;
#23932 = CARTESIAN_POINT ( 'NONE',  ( 1.330729578248716960, 1.354828421643257119, -1.498027418808007605 ) ) ;
#23933 = CARTESIAN_POINT ( 'NONE',  ( -1.499999999999997780, 5.900000000000023448, 1.214306433183764966E-14 ) ) ;
#23934 = B_SPLINE_CURVE_WITH_KNOTS ( 'NONE', 3,
 ( #155014, #59636, #72680, #205881, #57515, #26062 ),
 .UNSPECIFIED., .F., .F.,
 ( 4, 2, 4 ),
 ( 0.0004044236633723155756, 0.0006920484658239215488, 0.0009796732682755275763 ),
 .UNSPECIFIED. ) ;
#23935 = CARTESIAN_POINT ( 'NONE',  ( 1.364683531249988535, 4.113541667008088432, 0.7879004041258500513 ) ) ;
#23937 = CARTESIAN_POINT ( 'NONE',  ( 10.05978679165993839, 10.83876546646586014, 0.7216878364870438212 ) ) ;
#23936 = CARTESIAN_POINT ( 'NONE',  ( 0.07459516483341446791, 5.726030365519781284, -2.349570391284861781 ) ) ;
#23938 = CARTESIAN_POINT ( 'NONE',  ( 5.993517489292202960, 1.942244631591660164, 0.5404061186519912852 ) ) ;
#23939 = CARTESIAN_POINT ( 'NONE',  ( 5.594928181924037069, 1.692849881775596366, 0.8967378362389683000 ) ) ;
#23940 = CARTESIAN_POINT ( 'NONE',  ( 6.639320575229291421, 7.052573552169272730, 2.601414154538615353 ) ) ;
#23941 = CARTESIAN_POINT ( 'NONE',  ( 3.667680160636753506, 1.218766932906123479, 1.821211977396507198 ) ) ;
#23942 = CARTESIAN_POINT ( 'NONE',  ( 1.499999999999989120, 2.556250000682817713, 1.214306433183764966E-14 ) ) ;
#23943 = CARTESIAN_POINT ( 'NONE',  ( 2.408343312057196872, -1.907530749141531423, -0.1368029246449145864 ) ) ;
#23944 = CARTESIAN_POINT ( 'NONE',  ( -6.338600509588822263, 7.353787668397130162, -1.199719254218446718 ) ) ;
#23945 = CARTESIAN_POINT ( 'NONE',  ( 4.324687812634882000, 7.028924300507257250, 1.082531754730558626 ) ) ;
#23947 = CARTESIAN_POINT ( 'NONE',  ( 6.239883422132978197, 2.111550094393780608, -0.1561052605421053563 ) ) ;
#23946 = DIRECTION ( 'NONE',  ( -1.000000000000000000, 8.673617379884035472E-16, 0.000000000000000000 ) ) ;
#23948 = CARTESIAN_POINT ( 'NONE',  ( -0.6823417656250003738, 11.21354166700806765, 1.181850606188754593 ) ) ;
#23949 = AXIS2_PLACEMENT_3D ( 'NONE', #147510, #131310, #1211 ) ;
#23951 = CARTESIAN_POINT ( 'NONE',  ( -6.794571259104023930, 7.956029886156682274, 1.199719254218452047 ) ) ;
#23950 = CARTESIAN_POINT ( 'NONE',  ( 6.392125918040960642, -0.5824770489515176397, -2.112646119873210271 ) ) ;
#23953 = VERTEX_POINT ( 'NONE', #11362 ) ;
#23952 = CARTESIAN_POINT ( 'NONE',  ( 3.012419478190906830, 1.250452035320260835, -1.188195685136491875 ) ) ;
#23954 = CYLINDRICAL_SURFACE ( 'NONE', #5343, 0.08000000000000020983 ) ;
#23955 = CARTESIAN_POINT ( 'NONE',  ( 7.202405917357655341, 9.425892875049191488, 1.599625672291281386 ) ) ;
#23956 = CARTESIAN_POINT ( 'NONE',  ( 5.118366684358879759, 5.930181538962194132, 1.199719254218462483 ) ) ;
#23957 = DIRECTION ( 'NONE',  ( 0.5773487058764860125, 0.002327115863041261980, 0.8164943700690817652 ) ) ;
#23958 = CARTESIAN_POINT ( 'NONE',  ( -3.475000000000000533, -2.406249999044082877, 0.000000000000000000 ) ) ;
#23959 = CARTESIAN_POINT ( 'NONE',  ( 11.55950211276791428, 9.719999999999998863, -3.221476510067115662 ) ) ;
#23960 = CARTESIAN_POINT ( 'NONE',  ( 4.547870462380197765, 7.393267075163835855, 1.199719254218462483 ) ) ;
#23961 = CARTESIAN_POINT ( 'NONE',  ( -0.4019237886466871523, 10.69866454968463110, -1.499999999999998668 ) ) ;
#23962 = VERTEX_POINT ( 'NONE', #81711 ) ;
#23963 = DIRECTION ( 'NONE',  ( 0.000000000000000000, 0.000000000000000000, 1.000000000000000000 ) ) ;
#23964 = EDGE_LOOP ( 'NONE', ( #87412, #197204, #57427, #3292 ) ) ;
#23965 = CARTESIAN_POINT ( 'NONE',  ( 3.141053669680595739, 0.04696373034178760036, 1.811039086309898627 ) ) ;
#23966 = EDGE_LOOP ( 'NONE', ( #82571, #100656, #100077, #36916 ) ) ;
#23967 = CARTESIAN_POINT ( 'NONE',  ( 10.40318394038753702, 11.03146944007395724, -0.7998128361456281477 ) ) ;
#23968 = CARTESIAN_POINT ( 'NONE',  ( 5.923986774528332333, 5.876015756563318426, -0.7998128361456481317 ) ) ;
#23969 = CARTESIAN_POINT ( 'NONE',  ( 4.354050602105923318, 0.7703955181818689102, -1.639620356061684436 ) ) ;
#23970 = CARTESIAN_POINT ( 'NONE',  ( 6.739811759324814133, 8.956476034002680109, -1.443375672974078761 ) ) ;
#23971 = DIRECTION ( 'NONE',  ( 0.000000000000000000, -1.000000000000000000, 0.000000000000000000 ) ) ;
#23972 = CARTESIAN_POINT ( 'NONE',  ( 5.007133299032078710, 6.576657384445655730, 1.236533897214306066 ) ) ;
#23974 = CARTESIAN_POINT ( 'NONE',  ( 0.6823417656249934904, 14.19270833367473195, 1.181850606188764807 ) ) ;
#23973 = CARTESIAN_POINT ( 'NONE',  ( 5.406657457964442415, 0.5403815791694633885, 1.780887135367102303 ) ) ;
#23975 = CARTESIAN_POINT ( 'NONE',  ( 2.144012975658988740, 0.8210224433658172005, 1.730898686554068311 ) ) ;
#23976 = CARTESIAN_POINT ( 'NONE',  ( 1.360069071312763223, 0.7361036424862777983, 1.670779996689908398 ) ) ;
#23977 = CARTESIAN_POINT ( 'NONE',  ( 4.739226852959141034, 8.198292129125304584, 0.7147376406119988479 ) ) ;
#23978 = CARTESIAN_POINT ( 'NONE',  ( -10.93359526636954193, 4.740328704497578372, 4.433404364989353752 ) ) ;
#23979 = CARTESIAN_POINT ( 'NONE',  ( 6.059270238282111087, 7.038290852966752276, 1.014332888565868229 ) ) ;
#23980 = CARTESIAN_POINT ( 'NONE',  ( 9.672792005750940447, 13.47495944640959920, 8.176450814826708324 ) ) ;
#23981 = CARTESIAN_POINT ( 'NONE',  ( 10.99999999999731060, 1.347111479061759252E-15, -0.4330127018938151884 ) ) ;
#23982 = CARTESIAN_POINT ( 'NONE',  ( 3.475000000000000533, -2.552083332377419023, -2.006292185433951047 ) ) ;
#23983 = CARTESIAN_POINT ( 'NONE',  ( 6.480434237652121787, 9.543961796360731498, 1.082531754730558626 ) ) ;
#23984 = CARTESIAN_POINT ( 'NONE',  ( -4.172158584703340445, 5.890604320285754980, -1.599625672291256295 ) ) ;
#23985 = CARTESIAN_POINT ( 'NONE',  ( 11.86686399458719521, 12.49071270224662555, -1.056461745586973588 ) ) ;
#23986 = CARTESIAN_POINT ( 'NONE',  ( 0.8848510708264365476, 1.842997052242268508, -0.9869714196348714497 ) ) ;
#23987 = CARTESIAN_POINT ( 'NONE',  ( 6.792047303494690880, -0.8216981310003536043, 1.740383667632472875 ) ) ;
#23988 = CARTESIAN_POINT ( 'NONE',  ( -5.880485940025243607, 7.883652901494672349, 1.599625672291269396 ) ) ;
#23989 = CARTESIAN_POINT ( 'NONE',  ( 2.379681254797087586, 1.121034037677430595, 1.440765146680768272 ) ) ;
#23990 = CARTESIAN_POINT ( 'NONE',  ( 3.282038605231399231, 1.400092287458438722, 1.705885466304429166 ) ) ;
#23991 = FACE_OUTER_BOUND ( 'NONE', #71003, .T. ) ;
#23992 = CARTESIAN_POINT ( 'NONE',  ( 1.908593538011025492, 0.6150006609981206740, 1.871157805954210440 ) ) ;
#23993 = CARTESIAN_POINT ( 'NONE',  ( 3.667467498987980967, 1.081383794499408468, 1.612947176984424802 ) ) ;
#23994 = ORIENTED_EDGE ( 'NONE', *, *, #126096, .T. ) ;
#23995 = CYLINDRICAL_SURFACE ( 'NONE', #26274, 3.475000000000000089 ) ;
#23997 = CARTESIAN_POINT ( 'NONE',  ( 6.438329693799461850, -0.9962124079390155540, 1.571646734037221105 ) ) ;
#23996 = CARTESIAN_POINT ( 'NONE',  ( -5.679940009482361774, 5.591294530676332641, 0.7998128361456281477 ) ) ;
#23998 = CARTESIAN_POINT ( 'NONE',  ( 5.574337433874081427, 6.532423756721743580, -1.199719254218452047 ) ) ;
#24000 = ADVANCED_FACE ( 'NONE', ( #77441 ), #112156, .T. ) ;
#23999 = CARTESIAN_POINT ( 'NONE',  ( 1.579999999999991189, 8.674529973577531194, 2.420000000000000373 ) ) ;
#24001 = DIRECTION ( 'NONE',  ( -0.000000000000000000, -1.000000000000000000, -0.000000000000000000 ) ) ;
#24002 = CARTESIAN_POINT ( 'NONE',  ( -5.315678745009726924, 8.359319748223434487, -1.199719254218453823 ) ) ;
#24003 = CARTESIAN_POINT ( 'NONE',  ( 2.384552795368581890, -0.3778730364575392797, -2.158588602542845347 ) ) ;
#24004 = CARTESIAN_POINT ( 'NONE',  ( 2.207884333776653740E-15, 1.500000000682816914, -1.225000000000019851 ) ) ;
#24005 = ORIENTED_EDGE ( 'NONE', *, *, #143969, .F. ) ;
#24006 = CARTESIAN_POINT ( 'NONE',  ( 5.013482942003290255, 9.071090208970993274, -0.7998128361456481317 ) ) ;
#24007 = CARTESIAN_POINT ( 'NONE',  ( 4.214603523450839440, 3.811458953647739900, -0.4421859227901690503 ) ) ;
#24008 = CARTESIAN_POINT ( 'NONE',  ( 4.055160972438559774, -1.518969423100406946, -1.012540670841777013 ) ) ;
#24009 = CARTESIAN_POINT ( 'NONE',  ( 0.000000000000000000, -6.527411821100059797, 0.000000000000000000 ) ) ;
#24010 = CARTESIAN_POINT ( 'NONE',  ( -2.764973262183167968, 5.313220341600567664, 1.199719254218462483 ) ) ;
#24011 = CIRCLE ( 'NONE', #145132, 1.914481421317578258 ) ;
#24012 = CARTESIAN_POINT ( 'NONE',  ( -4.905272163827030241, 8.130510659208837865, -1.040677472382423474 ) ) ;
#24013 = DIRECTION ( 'NONE',  ( -1.000000000000000000, 0.000000000000000000, 0.000000000000000000 ) ) ;
#24014 = CARTESIAN_POINT ( 'NONE',  ( 7.052212457402625922, 11.37933163361175382, -0.7998128361456291469 ) ) ;
#24015 = CARTESIAN_POINT ( 'NONE',  ( 2.332535780611888043, 1.868688736674573247, 0.4679572130895108817 ) ) ;
#24016 = CARTESIAN_POINT ( 'NONE',  ( -0.5569645644277303465, 2.800000000000026468, 1.258719724711860666 ) ) ;
#24017 = CARTESIAN_POINT ( 'NONE',  ( -0.7500000000000006661, 14.45833333333333748, -1.299038105676657340 ) ) ;
#24018 = CARTESIAN_POINT ( 'NONE',  ( -6.521635583373313061, 7.567328587812373719, -1.199719254218446718 ) ) ;
#24019 = CARTESIAN_POINT ( 'NONE',  ( 3.388648328411762556, 6.040841252200647382, 1.199719254218462483 ) ) ;
#24020 = CARTESIAN_POINT ( 'NONE',  ( -6.089020385868876062, 6.276481003034692030, -0.7216878364870338292 ) ) ;
#24021 = ADVANCED_FACE ( 'NONE', ( #111080 ), #207279, .T. ) ;
#24022 = CARTESIAN_POINT ( 'NONE',  ( 6.385961957380775544, -2.116826826188836552, 0.05405687909286471110 ) ) ;
#24023 = CARTESIAN_POINT ( 'NONE',  ( 8.757677159423465696, 12.30470822171437284, 1.199719254218450271 ) ) ;
#24024 = CARTESIAN_POINT ( 'NONE',  ( 4.979381509686323426, -0.1069728651886258930, 2.067640925720988232 ) ) ;
#24026 = CARTESIAN_POINT ( 'NONE',  ( -1.364683531249997417, 3.321875000341423245, 1.214306433183764966E-14 ) ) ;
#24025 = CARTESIAN_POINT ( 'NONE',  ( 0.4855842612344652975, -1.827229208960782447, -0.2260576252584786672 ) ) ;
#24027 = CARTESIAN_POINT ( 'NONE',  ( 5.555437251493606787, -1.460316692103363456, 1.775274546321881530 ) ) ;
#24028 = CARTESIAN_POINT ( 'NONE',  ( 5.816084710582486217, 9.729256562414162701, 1.040834085586084257E-14 ) ) ;
#24030 = CARTESIAN_POINT ( 'NONE',  ( -10.24999999999999822, 0.000000000000000000, 6.123233995736778362E-17 ) ) ;
#24029 = CARTESIAN_POINT ( 'NONE',  ( 4.692530564105613422, 7.528350520548263702, -1.082531754730548412 ) ) ;
#24031 = CARTESIAN_POINT ( 'NONE',  ( 0.5688445697737016804, -2.160344153581617022, -0.7667740616737575010 ) ) ;
#24032 = DIRECTION ( 'NONE',  ( 0.000000000000000000, 0.000000000000000000, 1.000000000000000000 ) ) ;
#24033 = CARTESIAN_POINT ( 'NONE',  ( -6.291865805193673111, 9.498204651771386509, -1.199719254218452047 ) ) ;
#24034 = CARTESIAN_POINT ( 'NONE',  ( 4.576081071864527061, -1.884036987645235417, -0.4702585519323047025 ) ) ;
#24035 = ORIENTED_EDGE ( 'NONE', *, *, #19121, .F. ) ;
#24036 = CARTESIAN_POINT ( 'NONE',  ( 8.500599125643985232, 11.90082083235127008, -1.082531754730543083 ) ) ;
#24037 = VERTEX_POINT ( 'NONE', #2555 ) ;
#24038 = CARTESIAN_POINT ( 'NONE',  ( 6.398695753475230674, -1.876852914212179035, -0.3660984893600614520 ) ) ;
#24039 = CARTESIAN_POINT ( 'NONE',  ( 0.3281590906380106865, 1.648959081962350304, 0.5061492587876709193 ) ) ;
#24040 = CARTESIAN_POINT ( 'NONE',  ( 6.157435431667657610, 1.928259211291092123, -0.5899821858514133766 ) ) ;
#24041 = CARTESIAN_POINT ( 'NONE',  ( -10.16591625214838679, 10.75465713712827487, 1.040834085586084257E-14 ) ) ;
#24042 = CARTESIAN_POINT ( 'NONE',  ( 0.000000000000000000, -2.034374999522043481, -3.793834371823813001 ) ) ;
#24044 = CARTESIAN_POINT ( 'NONE',  ( 1.604008636410862554, -0.6330215999658711512, -1.652955932040809595 ) ) ;
#24043 = CARTESIAN_POINT ( 'NONE',  ( 3.169954053886741008, -1.245012139812958996, 1.679338519663716500 ) ) ;
#24045 = CARTESIAN_POINT ( 'NONE',  ( -1.326716514427061987E-15, 2.999999999999988454, -1.225000000000003864 ) ) ;
#24046 = B_SPLINE_CURVE_WITH_KNOTS ( 'NONE', 3,
 ( #156683, #141534, #208595, #190220, #91700, #41879, #105825, #74358, #60227, #7191, #58102, #209661, #39718, #8274, #76476, #143668, #124261, #140461, #139369, #127464, #61302, #207542, #157752, #24514, #142587 ),
 .UNSPECIFIED., .F., .F.,
 ( 4, 3, 3, 3, 3, 3, 3, 3, 4 ),
 ( 0.000000000000000000, 2.847723191052623255E-05, 6.630505566358953792E-05, 8.958118362427201905E-05, 9.621695898307930904E-05, 0.0001106671188294701110, 0.0001194291616091197475, 0.0001339184197518206642, 0.0001602236158699481391 ),
 .UNSPECIFIED. ) ;
#24048 = CARTESIAN_POINT ( 'NONE',  ( 4.506013928309719141, -0.9778350203078637337, -2.073373472838499598 ) ) ;
#24047 = CARTESIAN_POINT ( 'NONE',  ( 3.061108821635398769, 6.793320401875094561, -0.7998128361456362523 ) ) ;
#24049 = CARTESIAN_POINT ( 'NONE',  ( 2.150002804924430411, -1.345968700644652349, 1.103203096369822056 ) ) ;
#24050 = CARTESIAN_POINT ( 'NONE',  ( 3.194917754314666514, 6.879154480009089134, 0.7998128361456321445 ) ) ;
#24051 = PRESENTATION_LAYER_ASSIGNMENT (  '', '', ( #37991 ) ) ;
#24052 = CARTESIAN_POINT ( 'NONE',  ( 2.777707764728345907, 0.3069055913166895966, -2.098134212408508059 ) ) ;
#24053 = CARTESIAN_POINT ( 'NONE',  ( -2.660307654469991068, -0.4179397774614554417, -0.1320628536826823352 ) ) ;
#24054 = CARTESIAN_POINT ( 'NONE',  ( 2.653305042933405300, -0.2923731341353021373, -1.708803492460549744 ) ) ;
#24055 = CARTESIAN_POINT ( 'NONE',  ( -1.360316468750011332, 2.421875000341397577, -1.387778780781445676E-14 ) ) ;
#24056 = CARTESIAN_POINT ( 'NONE',  ( 1.838117294476193431, -0.9991240133950601843, 1.569924424075196390 ) ) ;
#24057 = CARTESIAN_POINT ( 'NONE',  ( 1.891327416536987105, 0.2117802020594385659, 2.160802721360413070 ) ) ;
#24058 = CARTESIAN_POINT ( 'NONE',  ( 5.473741331615251227, 7.409117525016355010, -1.599625672291262513 ) ) ;
#24059 = CARTESIAN_POINT ( 'NONE',  ( 3.204314817619222211, 1.275555974797081049, -1.561881975048397209 ) ) ;
#24060 = CARTESIAN_POINT ( 'NONE',  ( 2.718750000000001332, -0.7852924748298429902, 1.895863743164144744 ) ) ;
#24061 = CARTESIAN_POINT ( 'NONE',  ( -1.499999999999997780, 2.431250000682817713, 1.214306433183764966E-14 ) ) ;
#24062 = CARTESIAN_POINT ( 'NONE',  ( 1.342661396784496697, 0.3730742192328758144, 1.889760217127177455 ) ) ;
#24063 = CARTESIAN_POINT ( 'NONE',  ( 0.6823417656249969321, 13.77604166700806232, -1.181850606188757036 ) ) ;
#24064 = CARTESIAN_POINT ( 'NONE',  ( 5.045291550738682851, 0.1642389012704112972, 2.215424048113129540 ) ) ;
#24065 = ORIENTED_EDGE ( 'NONE', *, *, #158984, .T. ) ;
#24066 = CARTESIAN_POINT ( 'NONE',  ( -0.2110808730067144090, 0.2462152545684419269, -1.831495465910786269 ) ) ;
#24067 = CARTESIAN_POINT ( 'NONE',  ( -1.201851678989727383E-14, 0.7125000000000225597, 1.732050807568877637 ) ) ;
#24068 = CARTESIAN_POINT ( 'NONE',  ( 8.046927864910717432, 9.346836249606042202, 1.199719254218462483 ) ) ;
#24069 = CARTESIAN_POINT ( 'NONE',  ( 1.364683531249986537, 0.1552083336747499542, -0.7879004041258309554 ) ) ;
#24070 = CARTESIAN_POINT ( 'NONE',  ( 6.082328216444968128, 1.141246503175277205, 1.905736721132505140 ) ) ;
#24071 = CARTESIAN_POINT ( 'NONE',  ( 4.756279191188107269, -1.961398630904508833, -0.05015466537350299348 ) ) ;
#24072 = CARTESIAN_POINT ( 'NONE',  ( 9.463228032658635769, 11.10314946193233965, -1.082531754730543083 ) ) ;
#24073 =( GEOMETRIC_REPRESENTATION_CONTEXT ( 3 ) GLOBAL_UNCERTAINTY_ASSIGNED_CONTEXT ( ( #211888 ) ) GLOBAL_UNIT_ASSIGNED_CONTEXT ( ( #161440, #47699, #27148 ) ) REPRESENTATION_CONTEXT ( 'NONE', 'WORKASPACE' ) );
#24074 = FACE_OUTER_BOUND ( 'NONE', #200429, .T. ) ;
#24075 = CARTESIAN_POINT ( 'NONE',  ( 5.518922325393873507, 2.087324940739025525, 0.8731552084927389767 ) ) ;
#24076 = CARTESIAN_POINT ( 'NONE',  ( -4.502716413514296079, 8.267269892493059658, -0.7216878364870338292 ) ) ;
#24077 = CARTESIAN_POINT ( 'NONE',  ( 3.033693852995589246, 1.959511903404848043, -0.6444255830786119743 ) ) ;
#24078 = CARTESIAN_POINT ( 'NONE',  ( -6.742482464697739708, 6.760651051769146491, 0.7998128361456341429 ) ) ;
#24079 = CARTESIAN_POINT ( 'NONE',  ( 1.499999999999987121, 3.077083334016149863, -0.8660254037844262731 ) ) ;
#24080 = CARTESIAN_POINT ( 'NONE',  ( -1.364683531250010295, 5.592708333674750953, 0.7879004041258379498 ) ) ;
#24081 = CARTESIAN_POINT ( 'NONE',  ( 4.885944009213345929, -0.8832235454491498272, 1.648918812636574804 ) ) ;
#24082 = CARTESIAN_POINT ( 'NONE',  ( 3.955468362790943715, -1.619900715620861131, -0.6195580815930351593 ) ) ;
#24083 = CARTESIAN_POINT ( 'NONE',  ( 2.876183954794831354, -0.1304463317927692101, -1.735623171917876073 ) ) ;
#24084 = CARTESIAN_POINT ( 'NONE',  ( 0.8730959291491724450, -0.06322356207747076295, -2.291674109354911781 ) ) ;
#24085 = CARTESIAN_POINT ( 'NONE',  ( 1.501302152069685425, 1.803625081967351829, -1.271268654958551014 ) ) ;
#24086 = CARTESIAN_POINT ( 'NONE',  ( 5.056232447125663221, -1.513354532948107956, 1.442795048270538727 ) ) ;
#24087 = CARTESIAN_POINT ( 'NONE',  ( 5.507742394360604088, -0.8750994344452074358, -1.733673826448577593 ) ) ;
#24088 = CARTESIAN_POINT ( 'NONE',  ( 7.501149153046521967, 15.44179335589286062, 9.372933691065389539 ) ) ;
#24089 =( LENGTH_UNIT ( ) NAMED_UNIT ( * ) SI_UNIT ( .MILLI., .METRE. ) );
#24090 = CARTESIAN_POINT ( 'NONE',  ( 0.8443752267504719411, 0.3905955241953715795, -1.978051186352240309 ) ) ;
#24091 = FACE_OUTER_BOUND ( 'NONE', #120558, .T. ) ;
#24092 = DIRECTION ( 'NONE',  ( -0.000000000000000000, 1.000000000000000000, 9.023263958591317418E-17 ) ) ;
#24093 = CARTESIAN_POINT ( 'NONE',  ( -8.317037166979361018, 11.79062823052953668, 1.199719254218453823 ) ) ;
#24094 =( BOUNDED_CURVE ( )  B_SPLINE_CURVE ( 2, ( #158557, #44828, #211550, #142340, #59980, #210488, #28555, #78361, #125075, #62125, #195327, #128285, #112012, #79434, #191031, #179081, #101004, #198493, #166017, #114148, #148706, #84763, #98894, #32820, #130402, #99952, #97838, #167093, #163903, #17602, #180140, #2414, #117327, #131437, #83687, #213666, #68491, #116260, #64258, #65290, #212618, #82622, #50137, #162835, #182249, #51205, #164947, #275, #16539, #14414, #197440, #183325, #196391, #115200, #52268, #96784, #49081, #133553, #200621, #181193, #66348, #81563, #149775, #134619, #33874, #132491, #147647, #199561, #67412, #1350, #34931 ),
 .UNSPECIFIED., .F., .T. ) 
 B_SPLINE_CURVE_WITH_KNOTS ( ( 3, 2, 2, 2, 2, 2, 2, 2, 2, 2, 2, 2, 2, 2, 2, 2, 2, 2, 2, 2, 2, 2, 2, 2, 2, 2, 2, 2, 2, 2, 2, 2, 2, 2, 2, 3 ),
 ( 0.1345121972684862333, 0.1375000000000000111, 0.1416666666666666630, 0.1458333333333333426, 0.1499999999999999944, 0.1541666666666666741, 0.1583333333333333259, 0.1625000000000000056, 0.1666666666666666574, 0.1708333333333333370, 0.1749999999999999889, 0.1791666666666666685, 0.1833333333333333204, 0.1875000000000000000, 0.1916666666666666796, 0.1958333333333333315, 0.2000000000000000111, 0.2041666666666666630, 0.2083333333333333426, 0.2124999999999999944, 0.2166666666666666741, 0.2208333333333333259, 0.2250000000000000056, 0.2291666666666666574, 0.2333333333333333370, 0.2374999999999999889, 0.2416666666666666685, 0.2458333333333333204, 0.2500000000000000000, 0.2541666666666666519, 0.2583333333333333592, 0.2625000000000000111, 0.2666666666666666630, 0.2708333333333333148, 0.2750000000000000222, 0.2778825950481893514 ),
 .UNSPECIFIED. ) 
 CURVE ( )  GEOMETRIC_REPRESENTATION_ITEM ( )  RATIONAL_B_SPLINE_CURVE ( ( 0.9456386119408557445, 0.9039304805136860743, 1.000000000000000000, 0.8660254037844387076, 1.000000000000000000, 0.8660254037844387076, 1.000000000000000000, 0.8660254037844387076, 1.000000000000000000, 0.8660254037844387076, 1.000000000000000000, 0.8660254037844387076, 1.000000000000000000, 0.8660254037844387076, 1.000000000000000000, 0.8660254037844387076, 1.000000000000000000, 0.8660254037844387076, 1.000000000000000000, 0.8660254037844387076, 1.000000000000000000, 0.8660254037844387076, 1.000000000000000000, 0.8660254037844387076, 1.000000000000000000, 0.8660254037844387076, 1.000000000000000000, 0.8660254037844387076, 1.000000000000000000, 0.8660254037844387076, 1.000000000000000000, 0.8660254037844387076, 1.000000000000000000, 0.8660254037844387076, 1.000000000000000000, 0.8660254037844387076, 1.000000000000000000, 0.8660254037844387076, 1.000000000000000000, 0.8660254037844387076, 1.000000000000000000, 0.8660254037844387076, 1.000000000000000000, 0.8660254037844387076, 1.000000000000000000, 0.8660254037844387076, 1.000000000000000000, 0.8660254037844387076, 1.000000000000000000, 0.8660254037844387076, 1.000000000000000000, 0.8660254037844387076, 1.000000000000000000, 0.8660254037844387076, 1.000000000000000000, 0.8660254037844387076, 1.000000000000000000, 0.8660254037844387076, 1.000000000000000000, 0.8660254037844387076, 1.000000000000000000, 0.8660254037844387076, 1.000000000000000000, 0.8660254037844387076, 1.000000000000000000, 0.8660254037844387076, 1.000000000000000000, 0.8660254037844387076, 1.000000000000000000, 0.9073133181678055825, 0.9428721579752517012 ) ) 
 REPRESENTATION_ITEM ( '' )  );
#24095 = CARTESIAN_POINT ( 'NONE',  ( 6.388916700537700777, 8.476822122092563916, 1.599625672291281386 ) ) ;
#24096 = ADVANCED_BREP_SHAPE_REPRESENTATION ( '', ( #20283, #19400, #200407 ), #110829 ) ;
#24097 = SURFACE_STYLE_FILL_AREA ( #106484 ) ;
#24098 = CARTESIAN_POINT ( 'NONE',  ( 3.932112477472641920, 0.9751300899686901058, -1.543267412809447681 ) ) ;
#24099 = EDGE_LOOP ( 'NONE', ( #66148, #68249, #133847, #191907 ) ) ;
#24100 = CARTESIAN_POINT ( 'NONE',  ( -4.963693635934603776, 4.963599794778024155, 0.000000000000000000 ) ) ;
#24101 = CARTESIAN_POINT ( 'NONE',  ( 1.642778471875000035, -3.113541666188709200, -2.845375778867859751 ) ) ;
#24102 = CARTESIAN_POINT ( 'NONE',  ( -6.531277313481209212, 8.642909503859968368, 1.599625672291283607 ) ) ;
#24103 = CARTESIAN_POINT ( 'NONE',  ( 1.722921806169195547, 1.493705621373665915, -1.359711205623759023 ) ) ;
#24104 = CARTESIAN_POINT ( 'NONE',  ( 5.438574045396407541, 2.173287242562565780, 0.3821286992964008089 ) ) ;
#24105 = CARTESIAN_POINT ( 'NONE',  ( -3.623772196602547346, 7.449761006003425834, 0.000000000000000000 ) ) ;
#24106 = CARTESIAN_POINT ( 'NONE',  ( 2.553354172538614630, 1.434905519572576171, 1.184926768776579431 ) ) ;
#24107 = CARTESIAN_POINT ( 'NONE',  ( 4.241003122976366058, 3.842258486427521103, -0.7998128361456211532 ) ) ;
#24108 = CYLINDRICAL_SURFACE ( 'NONE', #112877, 2.000000000000000000 ) ;
#24109 = VERTEX_POINT ( 'NONE', #65430 ) ;
#24110 = CARTESIAN_POINT ( 'NONE',  ( -4.578903193113314174, 6.365139696764064325, 1.599625672291267398 ) ) ;
#24111 = CARTESIAN_POINT ( 'NONE',  ( -8.809047120577080392, 11.30030761213851953, 1.599625672291269396 ) ) ;
#24112 = CARTESIAN_POINT ( 'NONE',  ( 4.547361323050268744, -1.413013347330991598, -1.156083184146582177 ) ) ;
#24114 = CARTESIAN_POINT ( 'NONE',  ( -4.119491766144414591, 7.660190618428146081, -0.8001636830725885607 ) ) ;
#24113 = CARTESIAN_POINT ( 'NONE',  ( -8.100070429521727178, 8.414780020722290033, 0.7998128361456341429 ) ) ;
#24115 = CARTESIAN_POINT ( 'NONE',  ( 5.845834525830363226, 7.300097092180095615, -1.274846751706928849 ) ) ;
#24116 = CARTESIAN_POINT ( 'NONE',  ( 0.7371068013607602332, -1.629765380930665364, -0.5920680523868580014 ) ) ;
#24117 = CARTESIAN_POINT ( 'NONE',  ( 0.1459185412583801633, -1.400943258209320863, 1.032289493613134823 ) ) ;
#24118 = CARTESIAN_POINT ( 'NONE',  ( 5.250698995481407394, 0.6654115676409579905, 2.209675006967478428 ) ) ;
#24119 = CARTESIAN_POINT ( 'NONE',  ( 4.553559489343365740, 6.405848385690952718, -1.599625672291269396 ) ) ;
#24120 = CARTESIAN_POINT ( 'NONE',  ( 0.4915707408097417797, 1.525207926881542830, 1.386002245639144981 ) ) ;
#24122 = ADVANCED_FACE ( 'NONE', ( #131580 ), #132628, .T. ) ;
#24121 = MECHANICAL_DESIGN_GEOMETRIC_PRESENTATION_REPRESENTATION (  '', ( #107226 ), #145249 ) ;
#24123 = CARTESIAN_POINT ( 'NONE',  ( 6.063868583556772052, 1.884346855680006261, -1.315804018288849964 ) ) ;
#24124 = CARTESIAN_POINT ( 'NONE',  ( 3.600749563572445133, 3.160087278257350807, 2.499999999999998668 ) ) ;
#24125 = CARTESIAN_POINT ( 'NONE',  ( -7.422162748838431412, 7.623887726591770608, -0.7998128361456362523 ) ) ;
#24126 = CARTESIAN_POINT ( 'NONE',  ( 5.295714669793899709, -0.6724083694377264164, 1.745798414713333413 ) ) ;
#24128 = CARTESIAN_POINT ( 'NONE',  ( -4.065465959251405081, 5.836405933916976707, -1.599625672291271394 ) ) ;
#24127 = CARTESIAN_POINT ( 'NONE',  ( 3.603681638446740720, 1.388520161702249567, 1.315275747533505069 ) ) ;
#24129 = CARTESIAN_POINT ( 'NONE',  ( 5.285833163787800437, 1.479997892162682849, 1.637210856327932618 ) ) ;
#24130 = CARTESIAN_POINT ( 'NONE',  ( 4.417270958439249107, -1.934380516720465959, 0.8614220525851381538 ) ) ;
#24131 = CARTESIAN_POINT ( 'NONE',  ( -0.6125000000000383471, 0.6041666673494219264, 1.060881119635901593 ) ) ;
#24132 = CARTESIAN_POINT ( 'NONE',  ( -10.79305576557562318, 4.699117409047659955, 5.142361589734059990 ) ) ;
#24133 = CARTESIAN_POINT ( 'NONE',  ( 6.495764994278809823, 6.751016379513001375, 0.7216878364870328300 ) ) ;
#24134 = CARTESIAN_POINT ( 'NONE',  ( -5.356880090730904875, 7.343055753976412525, 1.443375672974058777 ) ) ;
#24135 = CARTESIAN_POINT ( 'NONE',  ( 6.199870563505585963, 1.461971410283597894, 1.536153618249151309 ) ) ;
#24136 = CARTESIAN_POINT ( 'NONE',  ( 2.802171680323842118, -0.7245931359087741663, 2.190924829087222303 ) ) ;
#24137 = CARTESIAN_POINT ( 'NONE',  ( 3.666413850373055006, -0.7928392042928497085, -1.794698522912529182 ) ) ;
#24138 = CARTESIAN_POINT ( 'NONE',  ( 5.998899845030374323, 0.3968100507469035643, 2.023884403326465797 ) ) ;
#24139 = CARTESIAN_POINT ( 'NONE',  ( 2.887523530030648988, 6.312601851770308414, 0.000000000000000000 ) ) ;
#24140 = CARTESIAN_POINT ( 'NONE',  ( 5.401997860402196316, 5.267028690082820930, 0.000000000000000000 ) ) ;
#24141 = ORIENTED_EDGE ( 'NONE', *, *, #135864, .F. ) ;
#24142 = CARTESIAN_POINT ( 'NONE',  ( 5.348842313791752900, -1.825074749614737701, -0.8578464102408298597 ) ) ;
#24143 = CARTESIAN_POINT ( 'NONE',  ( -8.565000355531095622, 11.01558638625153286, -1.599625672291263179 ) ) ;
#24144 = CARTESIAN_POINT ( 'NONE',  ( -4.489403031431899116, 8.251676092768461146, -0.01033961207361998313 ) ) ;
#24145 = CARTESIAN_POINT ( 'NONE',  ( 2.114367463569406080, 2.165448829365283157, -0.1565315255437193243 ) ) ;
#24146 = CARTESIAN_POINT ( 'NONE',  ( -5.608757509019071108, 5.629766575892905855, -0.3787719694710602325 ) ) ;
#24147 = CARTESIAN_POINT ( 'NONE',  ( -1.402160292154681736E-14, 2.368750000682818602, -1.732050807568863648 ) ) ;
#24148 = CARTESIAN_POINT ( 'NONE',  ( -8.165975823559877611, 14.52981782405839262, -8.838012710010978878 ) ) ;
#24149 = CARTESIAN_POINT ( 'NONE',  ( -1.420000000000021911, 6.120000000000041851, 2.500000000000011102 ) ) ;
#24150 = CARTESIAN_POINT ( 'NONE',  ( 5.602183562003149042, 7.492195738860313092, 1.335281325244306982 ) ) ;
#24151 = CARTESIAN_POINT ( 'NONE',  ( 1.511086176359067501, 1.816151333767004772, 0.9739060079534812564 ) ) ;
#24153 = CARTESIAN_POINT ( 'NONE',  ( 6.727182134110222478, 3.706444386917655986, 2.325533714637216143 ) ) ;
#24152 = CARTESIAN_POINT ( 'NONE',  ( -10.50487009249003378, 11.15010328419353947, 0.7998128361456462443 ) ) ;
#24154 = CARTESIAN_POINT ( 'NONE',  ( -1.364683531250014514, 0.4885416670080875434, -0.7879004041258289570 ) ) ;
#24155 = CARTESIAN_POINT ( 'NONE',  ( -0.1608832656953863849, 7.629137130509072939, -2.497055476982701361 ) ) ;
#24156 = ORIENTED_EDGE ( 'NONE', *, *, #88143, .F. ) ;
#24157 = CARTESIAN_POINT ( 'NONE',  ( 3.791585636498477463, 1.799617611794877670, -0.6470144256675299799 ) ) ;
#24158 = CARTESIAN_POINT ( 'NONE',  ( 4.926482082969720899, 1.694141084728201907, 0.5120089106541975132 ) ) ;
#24159 = CARTESIAN_POINT ( 'NONE',  ( 5.956828388357757298, 8.042995434541133193, 1.599625672291269396 ) ) ;
#24160 = CARTESIAN_POINT ( 'NONE',  ( -5.101945877444165944, 4.846691699973280976, 0.000000000000000000 ) ) ;
#24161 = CARTESIAN_POINT ( 'NONE',  ( 0.6327121402699478203, 1.674153623460835627, 0.6926115325788273491 ) ) ;
#24163 = CARTESIAN_POINT ( 'NONE',  ( 0.004910489962322779275, -0.09121751714964576596, 1.913643331117439672 ) ) ;
#24162 = CARTESIAN_POINT ( 'NONE',  ( 1.499999999999990896, 8.627523663848663205, -2.579999999999991189 ) ) ;
#24164 = CARTESIAN_POINT ( 'NONE',  ( 1.346235217667652417, -0.9325981557438846048, 1.848514419461377845 ) ) ;
#24165 = CARTESIAN_POINT ( 'NONE',  ( 0.6823417656249882723, -1.094791666325249713, 1.181850606188755259 ) ) ;
#24166 = CARTESIAN_POINT ( 'NONE',  ( 6.666881909320486521, -1.711340306973156977, -0.7558587634414122292 ) ) ;
#24167 = CARTESIAN_POINT ( 'NONE',  ( 2.754317325142870754, 0.6151756178996542479, 1.719052816137212503 ) ) ;
#24169 = CARTESIAN_POINT ( 'NONE',  ( 6.438112759045284683, 6.782534085545247393, 0.3978009605737874432 ) ) ;
#24168 = CARTESIAN_POINT ( 'NONE',  ( 5.865903189996044098, 2.174886565178067777, -0.3735607071253948530 ) ) ;
#24170 = CARTESIAN_POINT ( 'NONE',  ( 0.6823417656249882723, -0.1572916663252488245, 1.181850606188755259 ) ) ;
#24171 = CARTESIAN_POINT ( 'NONE',  ( 3.016140967954855423, 2.052969616667064123, -0.1997095218184695709 ) ) ;
#24172 = CARTESIAN_POINT ( 'NONE',  ( -6.581593504430098385, 9.765943957555402122, -1.199719254218440723 ) ) ;
#24173 = CARTESIAN_POINT ( 'NONE',  ( 9.562578416340237197, 10.05076299535211781, 0.7998128361456462443 ) ) ;
#24174 = CARTESIAN_POINT ( 'NONE',  ( 5.691725559638619814, 5.534767995866836543, 1.040834085586084257E-14 ) ) ;
#24175 = CARTESIAN_POINT ( 'NONE',  ( -0.03750003396568979408, -9.978860739388867529, -10.91964959838800731 ) ) ;
#24176 = ADVANCED_FACE ( 'NONE', ( #85975 ), #121098, .F. ) ;
#24177 = CARTESIAN_POINT ( 'NONE',  ( 6.109843426155951107, 0.6047356833836557977, -1.980059631771100781 ) ) ;
#24178 = CARTESIAN_POINT ( 'NONE',  ( -0.6823417656250003738, -0.2197916663252488800, -1.181850606188749264 ) ) ;
#24179 = CARTESIAN_POINT ( 'NONE',  ( 4.042369558984196587, 2.150769235480045616, 0.2162802025119994753 ) ) ;
#24181 = CARTESIAN_POINT ( 'NONE',  ( 2.066782613880484565, 1.455849762852476248, -1.315278764014264912 ) ) ;
#24180 = CARTESIAN_POINT ( 'NONE',  ( 4.600263385724223220, -0.9500085478860437194, 1.782271578547896418 ) ) ;
#24182 = CARTESIAN_POINT ( 'NONE',  ( 4.892484645941061139, 4.880522639849741218, -0.04086785794226917984 ) ) ;
#24184 = CARTESIAN_POINT ( 'NONE',  ( 6.480434237652124452, 8.583592582059388576, 1.443375672974076540 ) ) ;
#24183 = CARTESIAN_POINT ( 'NONE',  ( 1.737499999999999378, -0.1166666666666676955, -3.009438278150925683 ) ) ;
#24185 = CARTESIAN_POINT ( 'NONE',  ( -7.767895665986912057, 8.027242796598338614, -0.7998128361456362523 ) ) ;
#24186 = CARTESIAN_POINT ( 'NONE',  ( 2.149625371984189126, 1.976669504256656218, -0.3981124878784659815 ) ) ;
#24188 = CARTESIAN_POINT ( 'NONE',  ( 1.123270288250311610, 3.172697346350006331, 0.7749999999993734123 ) ) ;
#24187 = CARTESIAN_POINT ( 'NONE',  ( -4.985647801523292344, 6.839675073242382553, -1.599625672291256295 ) ) ;
#24189 = CARTESIAN_POINT ( 'NONE',  ( -1.500000000000011324, 5.452083334016153415, 0.8660254037844403729 ) ) ;
#24190 = CARTESIAN_POINT ( 'NONE',  ( 6.117437049485344502, 1.593764408019750389, 1.056661447057717362 ) ) ;
#24191 = CARTESIAN_POINT ( 'NONE',  ( -11.97929049433705551, 12.30000000000000071, 0.7046979865771804130 ) ) ;
#24192 = CARTESIAN_POINT ( 'NONE',  ( 6.439759776366780208, 6.615400615290456088, 0.7216878364870317197 ) ) ;
#24194 = CARTESIAN_POINT ( 'NONE',  ( 3.409779952838042583, -1.203371721269937744, -1.617806234278630573 ) ) ;
#24193 = CARTESIAN_POINT ( 'NONE',  ( -8.229436053370685400, 10.62409470039771442, 1.443375672974090751 ) ) ;
#24195 = CARTESIAN_POINT ( 'NONE',  ( -1.499999999999997780, 4.400000000000021672, 1.214306433183764966E-14 ) ) ;
#24196 = CARTESIAN_POINT ( 'NONE',  ( -1.364683531250010295, 14.44270833367473550, 0.7879004041258445001 ) ) ;
#24197 = CARTESIAN_POINT ( 'NONE',  ( 5.965779495465724835, 1.698367018877691370, -0.2996015908335278310 ) ) ;
#24198 = CARTESIAN_POINT ( 'NONE',  ( 5.664274315459256748, 9.830346811336296398, -0.7998128361456481317 ) ) ;
#24199 = CARTESIAN_POINT ( 'NONE',  ( 9.585251415181632595, 10.28514086057449184, 0.000000000000000000 ) ) ;
#24200 = AXIS2_PLACEMENT_3D ( 'NONE', #16969, #131859, #46319 ) ;
#24201 = CARTESIAN_POINT ( 'NONE',  ( 10.91804383151492530, -9.900000000000074962, -0.1905751639682747856 ) ) ;
#24202 = CARTESIAN_POINT ( 'NONE',  ( 3.936663633328242096, 0.2718032920513112627, 1.850550731861917653 ) ) ;
#24203 = CYLINDRICAL_SURFACE ( 'NONE', #106174, 0.5000000000000000000 ) ;
#24204 = CARTESIAN_POINT ( 'NONE',  ( 1.657173498210939844, 1.694793865239911712, -1.188712540599102141 ) ) ;
#24205 = CARTESIAN_POINT ( 'NONE',  ( -5.912764388891193157, 9.912325863766124456, 0.000000000000000000 ) ) ;
#24206 = EDGE_LOOP ( 'NONE', ( #94248, #57078, #20752 ) ) ;
#24207 = CARTESIAN_POINT ( 'NONE',  ( 2.878073747850912412, 6.579779482459851003, -0.7998128361456362523 ) ) ;
#24208 = SURFACE_STYLE_FILL_AREA ( #58866 ) ;
#24209 = CARTESIAN_POINT ( 'NONE',  ( 6.621734039712152686, -0.3858887922842542673, 1.776151629007856281 ) ) ;
#24210 = CARTESIAN_POINT ( 'NONE',  ( 3.404505970362959655, 6.986024375483197879, 0.7216878364870257245 ) ) ;
#24211 = CARTESIAN_POINT ( 'NONE',  ( -1.760028585276028923E-15, -6.211932585243245875, -10.91339599544321537 ) ) ;
#24212 = CARTESIAN_POINT ( 'NONE',  ( 7.904040366642689719, 10.24446639921506552, 1.443375672974076540 ) ) ;
#24213 =( GEOMETRIC_REPRESENTATION_CONTEXT ( 3 ) GLOBAL_UNCERTAINTY_ASSIGNED_CONTEXT ( ( #94982 ) ) GLOBAL_UNIT_ASSIGNED_CONTEXT ( ( #159440, #42523, #74999 ) ) REPRESENTATION_CONTEXT ( 'NONE', 'WORKASPACE' ) );
#24214 = CARTESIAN_POINT ( 'NONE',  ( 8.776205506747620788, 9.133327934160710981, -0.7998128361456221525 ) ) ;
#24216 = CARTESIAN_POINT ( 'NONE',  ( 6.603150280507321668, -0.1401627607961895561, 1.883980500587930429 ) ) ;
#24215 = CARTESIAN_POINT ( 'NONE',  ( -4.530395885260773525, 8.437212299446219532, 0.7998128361456481317 ) ) ;
#24217 = DIRECTION ( 'NONE',  ( -1.000000000000000000, 0.000000000000000000, 0.000000000000000000 ) ) ;
#24218 = CARTESIAN_POINT ( 'NONE',  ( -6.489499031467138579, 6.765560312407735033, -0.1891594744549245088 ) ) ;
#24219 = CARTESIAN_POINT ( 'NONE',  ( 9.103410076571945453, 12.70806329172093818, 1.199719254218450271 ) ) ;
#24220 = CARTESIAN_POINT ( 'NONE',  ( 0.3282377607281200538, 0.5736645496846195513, 1.224999999999978995 ) ) ;
#24222 = ORIENTED_EDGE ( 'NONE', *, *, #24434, .T. ) ;
#24221 = CARTESIAN_POINT ( 'NONE',  ( 3.985733972737593778, 6.633478153960411738, -1.082531754730548412 ) ) ;
#24223 = CARTESIAN_POINT ( 'NONE',  ( -7.036318535812428721, 11.15286269184909784, 0.000000000000000000 ) ) ;
#24224 = CARTESIAN_POINT ( 'NONE',  ( 2.799875798528407511, -0.6792266858460673795, 2.052276964324008635 ) ) ;
#24225 = CARTESIAN_POINT ( 'NONE',  ( -4.496464221587651799, 5.274905009054215554, 1.199719254218452935 ) ) ;
#24226 = CARTESIAN_POINT ( 'NONE',  ( 5.063044020060520900, 4.871582543017558109, 0.7998128361456352531 ) ) ;
#24227 = CARTESIAN_POINT ( 'NONE',  ( 0.3520121086563637869, -1.504009422257305495, -1.495223887398588358 ) ) ;
#24228 = CARTESIAN_POINT ( 'NONE',  ( 5.508770632382115728, 1.381118045931900573, -1.193960910464037850 ) ) ;
#24229 = CARTESIAN_POINT ( 'NONE',  ( 11.38290105699531196, 7.490053980982428250, 5.034049216093361423 ) ) ;
#24230 = CARTESIAN_POINT ( 'NONE',  ( 1.247272744223869356, -1.551563771690873006, -1.215972028847669417 ) ) ;
#24231 = CARTESIAN_POINT ( 'NONE',  ( 3.902528505893249733, -1.892296425594198750, -0.2755589300712790735 ) ) ;
#24232 = ORIENTED_EDGE ( 'NONE', *, *, #184591, .T. ) ;
#24233 = CARTESIAN_POINT ( 'NONE',  ( -11.41126283316785361, 9.841253930915410564, -3.405403429622882783 ) ) ;
#24234 = CARTESIAN_POINT ( 'NONE',  ( 5.125436402459787821, 0.1948648891074710732, -1.959901157258244098 ) ) ;
#24235 = CARTESIAN_POINT ( 'NONE',  ( 0.4099697989727095204, 1.339763683568921504, -1.405998798013205819 ) ) ;
#24236 = ORIENTED_EDGE ( 'NONE', *, *, #61327, .F. ) ;
#24237 = CARTESIAN_POINT ( 'NONE',  ( -5.367048706163331850, 7.354919138647580290, -1.599625672291271394 ) ) ;
#24239 = CARTESIAN_POINT ( 'NONE',  ( 6.539320575229233157, 0.001224430076711413356, 2.103502572931112091 ) ) ;
#24238 = CARTESIAN_POINT ( 'NONE',  ( -6.147696309153835692, 6.137010213626392208, 0.7998128361456281477 ) ) ;
#24241 = EDGE_CURVE ( 'NONE', #52497, #71497, #180577, .T. ) ;
#24240 = CARTESIAN_POINT ( 'NONE',  ( 4.706088717274885092, 8.504537580213796133, 0.7216878364870317197 ) ) ;
#24243 = ORIENTED_EDGE ( 'NONE', *, *, #58229, .F. ) ;
#24242 = CARTESIAN_POINT ( 'NONE',  ( 3.615784255950851289, -0.5524401208748200842, 1.830756043982272097 ) ) ;
#24244 = CARTESIAN_POINT ( 'NONE',  ( 1.114635189304619356, -0.9934212416997322270, -1.970578525975318573 ) ) ;
#24245 = CARTESIAN_POINT ( 'NONE',  ( 7.834948807407927873, -5.743759731405710056, 7.720982915749591058 ) ) ;
#24246 = CARTESIAN_POINT ( 'NONE',  ( 6.393232662110455600, -0.1012007143085277561, -2.010677637860050382 ) ) ;
#24247 = CARTESIAN_POINT ( 'NONE',  ( 1.284279953904125193, 3.003360285806104368, 0.7750000000000065725 ) ) ;
#24248 = LINE ( 'NONE', #153207, #152810 ) ;
#24249 = CARTESIAN_POINT ( 'NONE',  ( 6.727182134110203826, 2.985950691969769810, 2.264927069331075238 ) ) ;
#24250 = CARTESIAN_POINT ( 'NONE',  ( 2.172408243068229439, -0.9739482337229148357, -1.826950231780352762 ) ) ;
#24251 = CARTESIAN_POINT ( 'NONE',  ( -6.388916700537716764, 8.476822122092563916, 1.599625672291283607 ) ) ;
#24252 = CARTESIAN_POINT ( 'NONE',  ( -4.683575932806860465, 8.284415941318199472, -0.5487617172068790516 ) ) ;
#24253 = CARTESIAN_POINT ( 'NONE',  ( 0.7784641540938314064, -1.199969256800371697, 1.797863220954009966 ) ) ;
#24254 = CARTESIAN_POINT ( 'NONE',  ( 5.931855901178834323, 6.879252291918818152, 1.199719254218462483 ) ) ;
#24255 = DIRECTION ( 'NONE',  ( -0.000000000000000000, 0.000000000000000000, -1.000000000000000000 ) ) ;
#24256 = CARTESIAN_POINT ( 'NONE',  ( 5.397554552016228691, 5.469770863539975991, 0.7216878364870328300 ) ) ;
#24257 = CARTESIAN_POINT ( 'NONE',  ( 7.887197531381540117, -6.766388843766935501, -7.667935170093256758 ) ) ;
#24258 = DIRECTION ( 'NONE',  ( 0.000000000000000000, -1.000000000000000000, 0.000000000000000000 ) ) ;
#24259 = CARTESIAN_POINT ( 'NONE',  ( -1.364683531250010295, 12.94270833367473550, 0.7879004041258445001 ) ) ;
#24261 = CARTESIAN_POINT ( 'NONE',  ( -7.119966945832006289, 8.335658187339330283, 1.199719254218452047 ) ) ;
#24260 = CARTESIAN_POINT ( 'NONE',  ( 6.925078400183577010, 7.053014648177382995, 2.453806744102948745 ) ) ;
#24262 = CARTESIAN_POINT ( 'NONE',  ( 5.379468213355050210, -0.4295577260071090087, -1.679954900457746980 ) ) ;
#24263 = B_SPLINE_CURVE_WITH_KNOTS ( 'NONE', 3,
 ( #198987, #65778, #101517, #52765, #97275, #50632 ),
 .UNSPECIFIED., .F., .F.,
 ( 4, 2, 4 ),
 ( 0.000000000000000000, 0.0003168911866439334617, 0.0006337823732878669234 ),
 .UNSPECIFIED. ) ;
#24264 = CARTESIAN_POINT ( 'NONE',  ( -2.591579918506545344, 6.175260338232929413, 1.040834085586084257E-14 ) ) ;
#24265 = CARTESIAN_POINT ( 'NONE',  ( 2.993098612437725681, 0.2488643248897918769, 2.055149816265568585 ) ) ;
#24266 = CARTESIAN_POINT ( 'NONE',  ( 3.128620947210249970, 0.5168888077675163339, 2.053037424179054327 ) ) ;
#24267 = CARTESIAN_POINT ( 'NONE',  ( 8.423693512792301163, 8.722063941212843119, 0.7998128361456481317 ) ) ;
#24268 = CARTESIAN_POINT ( 'NONE',  ( 0.6823417656249899377, 3.426041667008085323, -1.181850606188754593 ) ) ;
#24269 = CARTESIAN_POINT ( 'NONE',  ( 1.410928143256191092, -1.555772830594209788, 1.207522851012821308 ) ) ;
#24270 = CARTESIAN_POINT ( 'NONE',  ( 5.545980446453017798, 6.390169355917580951, 1.218016560845627483 ) ) ;
#24271 = CARTESIAN_POINT ( 'NONE',  ( -0.4642244361878701819, -7.321523296574937056, -10.36809559534895975 ) ) ;
#24272 = CARTESIAN_POINT ( 'NONE',  ( 3.451411174752341715, 0.5572527081592703047, -2.223385661236119581 ) ) ;
#24273 = CARTESIAN_POINT ( 'NONE',  ( 1.980809073483770000, -0.08854697198140694392, -1.823669195971427071 ) ) ;
#24274 = CARTESIAN_POINT ( 'NONE',  ( 4.355912491740495440, 8.303924683664389406, 0.000000000000000000 ) ) ;
#24275 = CARTESIAN_POINT ( 'NONE',  ( 6.114364089638782751, 9.116879957011832403, 1.082531754730558626 ) ) ;
#24276 = CARTESIAN_POINT ( 'NONE',  ( -6.723954117373590833, 9.932031339322813679, -1.199719254218440723 ) ) ;
#24277 = CARTESIAN_POINT ( 'NONE',  ( 3.375247105954663596, -1.777387065663883714, -0.9453995415899820731 ) ) ;
#24278 = CARTESIAN_POINT ( 'NONE',  ( 3.028120845615460688, 1.045410262836780069, 1.659804706804830277 ) ) ;
#24279 = CARTESIAN_POINT ( 'NONE',  ( -8.507905087775398556, 9.884643009614800135, 1.199719254218462483 ) ) ;
#24280 = CARTESIAN_POINT ( 'NONE',  ( -6.144869935491728441, 8.192100896205577243, -1.599625672291263179 ) ) ;
#24281 = CARTESIAN_POINT ( 'NONE',  ( 0.07536363704235481131, 0.6997989235110781969, -2.226667633679416447 ) ) ;
#24283 = CARTESIAN_POINT ( 'NONE',  ( 5.067173336470212064, 0.1711322554274422036, -1.761558580727173862 ) ) ;
#24282 = CARTESIAN_POINT ( 'NONE',  ( 6.492138175525482779, -0.5563555211482211771, -2.015168333173870785 ) ) ;
#24284 = CARTESIAN_POINT ( 'NONE',  ( 0.7124089920922619390, 15.00000000000000355, 12.66466791154580207 ) ) ;
#24285 = CARTESIAN_POINT ( 'NONE',  ( 0.5510472016944796270, -1.853416330350022179, -1.169031858332982177 ) ) ;
#24286 = CARTESIAN_POINT ( 'NONE',  ( 6.017484387666114820, -0.9725936433230500944, -1.442976214814440716 ) ) ;
#24287 = CARTESIAN_POINT ( 'NONE',  ( 7.914208982075123799, 10.25632978388623684, -1.599625672291262513 ) ) ;
#24288 = CARTESIAN_POINT ( 'NONE',  ( 0.1333692844072767447, 1.351132181276387678, -2.308013766563504987 ) ) ;
#24289 = CARTESIAN_POINT ( 'NONE',  ( 6.082725252809636274, -0.7780705872160005310, 2.163147651226764889 ) ) ;
#24290 = DIRECTION ( 'NONE',  ( 0.000000000000000000, -1.000000000000000000, 0.000000000000000000 ) ) ;
#24291 = CARTESIAN_POINT ( 'NONE',  ( 5.149590220011600827, -0.2133714078210862675, -1.720544222028724146 ) ) ;
#24292 = CARTESIAN_POINT ( 'NONE',  ( 1.840723031453334935, 2.183200880077686978, 0.3216222850719457349 ) ) ;
#24293 = CARTESIAN_POINT ( 'NONE',  ( 6.421112215724263272, -1.799107166270615732, 0.9110519380226205222 ) ) ;
#24294 =( GEOMETRIC_REPRESENTATION_CONTEXT ( 3 ) GLOBAL_UNCERTAINTY_ASSIGNED_CONTEXT ( ( #165204 ) ) GLOBAL_UNIT_ASSIGNED_CONTEXT ( ( #49154, #167164, #18751 ) ) REPRESENTATION_CONTEXT ( 'NONE', 'WORKASPACE' ) );
#24295 = CARTESIAN_POINT ( 'NONE',  ( 5.600102540861260358, 0.8850759393619503923, -1.982774263332246489 ) ) ;
#24296 = DIRECTION ( 'NONE',  ( -0.000000000000000000, -1.000000000000000000, -0.000000000000000000 ) ) ;
#24297 = CARTESIAN_POINT ( 'NONE',  ( -0.1177638760072839408, -2.117013592363240271, -0.04492315971119444085 ) ) ;
#24298 = CARTESIAN_POINT ( 'NONE',  ( 3.312500000000002220, 1.451031289061251339, 1.451031289060983998 ) ) ;
#24299 = CARTESIAN_POINT ( 'NONE',  ( 6.827182134110199918, 0.5620517916639695688, 2.240906645742099190 ) ) ;
#24300 = CARTESIAN_POINT ( 'NONE',  ( 4.102502470231626397, -0.6033306519132185519, -1.829551733875626862 ) ) ;
#24301 = CARTESIAN_POINT ( 'NONE',  ( 1.577126836321657954, -1.567749618368704967, 1.573888218047289067 ) ) ;
#24302 = ORIENTED_EDGE ( 'NONE', *, *, #176359, .F. ) ;
#24303 = CARTESIAN_POINT ( 'NONE',  ( -1.201851678989727383E-14, 3.962500000000022116, 1.732050807568877637 ) ) ;
#24304 = CARTESIAN_POINT ( 'NONE',  ( 5.847644326195776010, 5.716673223516856694, -0.7998128361456281477 ) ) ;
#24305 = CARTESIAN_POINT ( 'NONE',  ( 6.012151052656117933, 9.101594430485762999, 1.199719254218460707 ) ) ;
#24306 = CARTESIAN_POINT ( 'NONE',  ( 3.862163208519187929, 0.7476031731964963845, -2.091851990882629408 ) ) ;
#24307 = CARTESIAN_POINT ( 'NONE',  ( -7.524412065904404479, 11.72230514362308185, 0.000000000000000000 ) ) ;
#24308 = PRESENTATION_STYLE_ASSIGNMENT (( #2715 ) ) ;
#24309 = CARTESIAN_POINT ( 'NONE',  ( 5.802526556968819804, 9.713438716531550554, -0.7216878364870267237 ) ) ;
#24310 = CARTESIAN_POINT ( 'NONE',  ( -9.341204649691320583, 10.96078884847042545, 1.082531754730558626 ) ) ;
#24311 = CARTESIAN_POINT ( 'NONE',  ( 7.200788982633824276, 7.573544365927161515, 0.000000000000000000 ) ) ;
#24312 = CARTESIAN_POINT ( 'NONE',  ( 1.846327496167538884, 0.3419342931599393398, -1.987046799686801757 ) ) ;
#24314 = CARTESIAN_POINT ( 'NONE',  ( 0.3388347341246043531, -1.999784422754165458, -0.5045462532434812353 ) ) ;
#24313 = CARTESIAN_POINT ( 'NONE',  ( 6.916630921265960019, 11.22115317478565188, 0.7998128361456462443 ) ) ;
#24315 = CARTESIAN_POINT ( 'NONE',  ( -10.99740610014212550, -6.654245765634820842, 0.2680151545362552401 ) ) ;
#24316 = CARTESIAN_POINT ( 'NONE',  ( 6.007671464186812749, 10.02305078494439883, 0.7216878364870317197 ) ) ;
#24317 = CARTESIAN_POINT ( 'NONE',  ( 0.02850758872123548837, -1.683968158181762043, 0.7450552726024004535 ) ) ;
#24318 =( NAMED_UNIT ( * ) PLANE_ANGLE_UNIT ( ) SI_UNIT ( $, .RADIAN. ) );
#24319 = CARTESIAN_POINT ( 'NONE',  ( 1.364683531249990311, 2.634375000341422801, 1.214306433183764966E-14 ) ) ;
#24320 = CARTESIAN_POINT ( 'NONE',  ( 1.369957856843624366, -1.128201996292097498, 1.363478919461190708 ) ) ;
#24321 = CARTESIAN_POINT ( 'NONE',  ( 0.6158615555539399544, 0.1511424999406512648, 2.010826230049263863 ) ) ;
#24322 = CARTESIAN_POINT ( 'NONE',  ( 0.1515692981730529243, 0.7036590017722235135, 1.701685288394996665 ) ) ;
#24323 = CARTESIAN_POINT ( 'NONE',  ( 3.931398753607476593, -1.581038262191627686, -1.660111252351449185 ) ) ;
#24324 = CARTESIAN_POINT ( 'NONE',  ( 2.712652182946372559, -0.1802803596865458491, 1.832282175343015407 ) ) ;
#24325 = CARTESIAN_POINT ( 'NONE',  ( 10.23370702021670020, 10.83374636654133383, 0.7998128361456462443 ) ) ;
#24326 = CARTESIAN_POINT ( 'NONE',  ( 6.928203230275520319, 15.00000000000000000, 9.797958971132713302 ) ) ;
#24327 = CARTESIAN_POINT ( 'NONE',  ( 3.293790705515726280, -0.7410340593078695859, 1.668602820345471027 ) ) ;
#24328 = CARTESIAN_POINT ( 'NONE',  ( 3.674454069786535548, 1.462445212485608437, 1.388486266691544957 ) ) ;
#24329 = CARTESIAN_POINT ( 'NONE',  ( -9.154780037725563702, 11.70366268214508487, 1.599625672291281386 ) ) ;
#24331 = DIRECTION ( 'NONE',  ( 0.000000000000000000, 0.000000000000000000, 1.000000000000000000 ) ) ;
#24330 = CARTESIAN_POINT ( 'NONE',  ( 3.292113192954935208, -0.9186832275986864804, 2.067785417532372438 ) ) ;
#24332 = CARTESIAN_POINT ( 'NONE',  ( 5.473694172853372564, 2.030421858957079273, -0.5587401243299906506 ) ) ;
#24333 = CARTESIAN_POINT ( 'NONE',  ( 9.644012019580303630, 13.59213021077435535, 8.211487644058824031 ) ) ;
#24334 = CARTESIAN_POINT ( 'NONE',  ( 1.961466609329724164, 1.720096886549182136, 1.151944459977225055 ) ) ;
#24335 = CARTESIAN_POINT ( 'NONE',  ( 4.192495815123822744, 5.914331089109666983, -1.599625672291255185 ) ) ;
#24336 = CARTESIAN_POINT ( 'NONE',  ( -0.6801582343750177673, 0.9635416670080582113, 1.178068619123796568 ) ) ;
#24337 = CARTESIAN_POINT ( 'NONE',  ( 6.199870563505585963, 1.461971410283597894, 1.536153618249151309 ) ) ;
#24339 = CARTESIAN_POINT ( 'NONE',  ( 0.7856181369204550125, 1.292946451617222436, 1.428335531958953464 ) ) ;
#24338 = CARTESIAN_POINT ( 'NONE',  ( -7.994504133552415404, 12.47867192245318435, -0.7998128361456281477 ) ) ;
#24340 = CARTESIAN_POINT ( 'NONE',  ( -5.327428015527048366, 5.180030537728460338, -0.7998128361456362523 ) ) ;
#24341 = CARTESIAN_POINT ( 'NONE',  ( 8.609591239877852686, 10.00327685373437347, -1.199719254218445830 ) ) ;
#24342 = CARTESIAN_POINT ( 'NONE',  ( 4.041739190205284160, 7.729463131965888856, 0.000000000000000000 ) ) ;
#24343 = CARTESIAN_POINT ( 'NONE',  ( 4.839368334287259543, 6.711050605271530856, 1.249743143419468350 ) ) ;
#24344 = CARTESIAN_POINT ( 'NONE',  ( -1.737499999999997824, -0.9479166657107505056, 3.009438278150925683 ) ) ;
#24345 = CARTESIAN_POINT ( 'NONE',  ( -4.440459003675619520, 5.139289244831666714, 1.199719254218462483 ) ) ;
#24346 = CARTESIAN_POINT ( 'NONE',  ( 0.7916362837351547110, -0.06200823681477837107, -2.220726283632424192 ) ) ;
#24347 = CARTESIAN_POINT ( 'NONE',  ( 1.870285774507766119, 1.081916120455215902, 1.806640566525853808 ) ) ;
#24348 = CARTESIAN_POINT ( 'NONE',  ( -3.383641855062333281, 6.105276709951447778, -1.199719254218452047 ) ) ;
#24349 = CARTESIAN_POINT ( 'NONE',  ( 7.076466111328892694, 10.34329533227067799, -1.199719254218441611 ) ) ;
#24350 = CARTESIAN_POINT ( 'NONE',  ( 6.578945215809504532, 1.736110340762307969, 0.6705269824554618285 ) ) ;
#24351 = CARTESIAN_POINT ( 'NONE',  ( 7.507464373665139412, 9.781794407407920389, 1.599625672291281386 ) ) ;
#24352 = CARTESIAN_POINT ( 'NONE',  ( -0.02299388927988389730, 0.001624902753813084553, -1.910968047046639695 ) ) ;
#24353 = CARTESIAN_POINT ( 'NONE',  ( -6.997416678428844072, 8.296645891989347987, 1.082531754730549078 ) ) ;
#24354 = CARTESIAN_POINT ( 'NONE',  ( -7.863365906246048809, 12.11775129068834289, -0.7216878364870267237 ) ) ;
#24355 = CARTESIAN_POINT ( 'NONE',  ( 0.2816890862925770511, 0.2015970107726860194, -2.110973810222869229 ) ) ;
#24356 = CARTESIAN_POINT ( 'NONE',  ( -2.580963302752292243, 0.4788041664876945269, 0.000000000000000000 ) ) ;
#24358 = CARTESIAN_POINT ( 'NONE',  ( 3.367582429956605061, -0.3852447139683997657, 1.923494667983568718 ) ) ;
#24357 = CARTESIAN_POINT ( 'NONE',  ( -0.6125000000000314637, -0.2916666666666761776, -1.060881119635948444 ) ) ;
#24359 = CARTESIAN_POINT ( 'NONE',  ( 2.360439101503517101, 0.9236781337260314695, 1.954550705658316456 ) ) ;
#24361 = CARTESIAN_POINT ( 'NONE',  ( -5.061731940678604325, 6.567192784585701659, -1.227863150880079246 ) ) ;
#24360 = CARTESIAN_POINT ( 'NONE',  ( -3.959863383643135393, 6.777535159962392086, 1.199719254218452935 ) ) ;
#24362 = CARTESIAN_POINT ( 'NONE',  ( -1.201851678989727383E-14, 2.071875000341422801, 1.575800808251672791 ) ) ;
#24363 = CARTESIAN_POINT ( 'NONE',  ( 3.415673062852276232, 1.103011313415346306, -1.346137666936922717 ) ) ;
#24364 = CARTESIAN_POINT ( 'NONE',  ( 5.992340707560147806, 8.974519344586754599, 1.082531754730558626 ) ) ;
#24365 = CARTESIAN_POINT ( 'NONE',  ( -10.84554942614793127, 5.653270432668692891, -6.476099931950408006 ) ) ;
#24366 = EDGE_CURVE ( 'NONE', #196686, #132613, #87038, .T. ) ;
#24367 = CARTESIAN_POINT ( 'NONE',  ( 2.636092105226188309, 0.1017362925337349233, -2.013677536115268563 ) ) ;
#24368 = CARTESIAN_POINT ( 'NONE',  ( 0.07536363704235565786, 7.629137130509072051, -2.744199452819145346 ) ) ;
#24369 = CARTESIAN_POINT ( 'NONE',  ( 0.3390366800232989530, 0.3710982241871863541, 2.129449491308422537 ) ) ;
#24370 = CARTESIAN_POINT ( 'NONE',  ( 2.500799400523348037, 1.584503739761052188, -1.172863459551294341 ) ) ;
#24373 = ORIENTED_EDGE ( 'NONE', *, *, #156157, .F. ) ;
#24372 = CARTESIAN_POINT ( 'NONE',  ( -6.143253000767895600, 6.339752387083549934, 0.000000000000000000 ) ) ;
#24371 = CARTESIAN_POINT ( 'NONE',  ( 0.000000000000000000, 0.6185895741317448682, 6.264285714285709794 ) ) ;
#24374 = CARTESIAN_POINT ( 'NONE',  ( -5.194182247366913252, 7.153241603385088965, 1.443375672974058777 ) ) ;
#24375 = CARTESIAN_POINT ( 'NONE',  ( 5.875479466675786355, 7.948088359245467416, -1.599625672291283607 ) ) ;
#24376 = EDGE_CURVE ( 'NONE', #61984, #18470, #4822, .T. ) ;
#24377 = CARTESIAN_POINT ( 'NONE',  ( -4.769436176957319695, 8.786368983084006601, 0.7998128361456281477 ) ) ;
#24378 = CARTESIAN_POINT ( 'NONE',  ( 2.561199701127094830, -1.677907875943387639, 1.123823742627054312 ) ) ;
#24379 = CARTESIAN_POINT ( 'NONE',  ( 3.511198596259283544, 6.271927390929313617, -7.499999999999997335 ) ) ;
#24380 = CARTESIAN_POINT ( 'NONE',  ( 5.807753868445137080, -0.5680028841938968842, 2.236484270104825089 ) ) ;
#24381 = FACE_OUTER_BOUND ( 'NONE', #158071, .T. ) ;
#24382 = CARTESIAN_POINT ( 'NONE',  ( 2.606241817087478374, 1.961221450604538008, 0.05310280016677935283 ) ) ;
#24383 = CARTESIAN_POINT ( 'NONE',  ( 8.666686507633574621, 11.13422023037111330, 1.599625672291281386 ) ) ;
#24384 = CARTESIAN_POINT ( 'NONE',  ( 0.07093568767341934533, -0.9480374005119349690, 1.779628194860154222 ) ) ;
#24385 = ORIENTED_EDGE ( 'NONE', *, *, #96265, .F. ) ;
#24386 = CARTESIAN_POINT ( 'NONE',  ( 2.554045646286424276, 1.136978842527110123, 1.786019645988563997 ) ) ;
#24388 = CARTESIAN_POINT ( 'NONE',  ( -6.205881626753225966, 8.263281202677319470, 1.599625672291283607 ) ) ;
#24387 = CARTESIAN_POINT ( 'NONE',  ( -4.471491734408701291, 4.111161866431900513, 1.214306433183764966E-14 ) ) ;
#24389 = CARTESIAN_POINT ( 'NONE',  ( 1.816098422328410900, 1.717562825535594140, 0.6636192267199734207 ) ) ;
#24390 = VERTEX_POINT ( 'NONE', #116400 ) ;
#24391 = CARTESIAN_POINT ( 'NONE',  ( -7.947050595904583403, 12.42330946186405249, 0.7998128361456481317 ) ) ;
#24392 = CARTESIAN_POINT ( 'NONE',  ( 9.817133948775492058, 11.89457090661458238, 6.904171386027695867 ) ) ;
#24393 = CARTESIAN_POINT ( 'NONE',  ( 3.762070191281779774, 0.7111978290502696254, -1.997938288694045550 ) ) ;
#24394 = CARTESIAN_POINT ( 'NONE',  ( 6.703083108286362446, -0.4264415456523527603, 1.901745634116110084 ) ) ;
#24395 = FACE_OUTER_BOUND ( 'NONE', #27943, .T. ) ;
#24396 = CARTESIAN_POINT ( 'NONE',  ( 8.586391356156291010, 8.911878091804165791, 0.7998128361456481317 ) ) ;
#24397 = CARTESIAN_POINT ( 'NONE',  ( 6.875920180786008196, 8.050936961452347163, -1.199719254218452047 ) ) ;
#24398 = CARTESIAN_POINT ( 'NONE',  ( 4.657529158609388986, 0.4554517582456064084, -2.009643979410648651 ) ) ;
#24400 = CARTESIAN_POINT ( 'NONE',  ( 1.311775528174640604, 1.236260529797410301, -1.364685630449238740 ) ) ;
#24399 = CARTESIAN_POINT ( 'NONE',  ( -6.690058733339450114, 9.892486724616283311, 1.199719254218452047 ) ) ;
#24401 = CARTESIAN_POINT ( 'NONE',  ( -0.6823417656250212460, 5.301041667008086655, 1.181850606188767472 ) ) ;
#24402 = CARTESIAN_POINT ( 'NONE',  ( 0.000000000000000000, 8.500000000000000000, 0.000000000000000000 ) ) ;
#24403 = CARTESIAN_POINT ( 'NONE',  ( -9.499656837482767457, -9.914216672575012268, 0.08076498840997262119 ) ) ;
#24404 = CARTESIAN_POINT ( 'NONE',  ( 1.394453263437886604E-15, -1.618749999044085230, 3.474999999999999645 ) ) ;
#24405 = CARTESIAN_POINT ( 'NONE',  ( 0.5576012004645107822, -1.866542136390366036, -1.177153700605698461 ) ) ;
#24406 = CARTESIAN_POINT ( 'NONE',  ( 3.339431287149054572, -1.996970876468142864, 1.063245685667679519 ) ) ;
#24407 = CARTESIAN_POINT ( 'NONE',  ( -8.676855123066030018, 9.225345186439589895, -0.7216878364870267237 ) ) ;
#24409 = EDGE_CURVE ( 'NONE', #90194, #190431, #186518, .T. ) ;
#24408 = CARTESIAN_POINT ( 'NONE',  ( 3.146531925530637430, 1.768428357263505557, 0.3923012617871086682 ) ) ;
#24410 = CARTESIAN_POINT ( 'NONE',  ( 2.729585477426241802, 0.6851132086851609015, -1.789222977413899462 ) ) ;
#24411 = CARTESIAN_POINT ( 'NONE',  ( 3.859880467719906783, -0.6038372105774907350, 1.980330894321411517 ) ) ;
#24412 = CARTESIAN_POINT ( 'NONE',  ( -1.201851678989727383E-14, 4.509375000341417916, -1.575800808251660134 ) ) ;
#24413 = PRESENTATION_LAYER_ASSIGNMENT (  '', '', ( #180141 ) ) ;
#24414 = CARTESIAN_POINT ( 'NONE',  ( 2.957844615808038480, 1.962099266425470390, -0.1918489139557562340 ) ) ;
#24415 = CARTESIAN_POINT ( 'NONE',  ( 0.8504600536136133204, 0.5560621936452102565, 1.844401357902447414 ) ) ;
#24416 = CARTESIAN_POINT ( 'NONE',  ( 3.836663719693265584, 0.2738035037005565053, 1.850374562403465983 ) ) ;
#24417 = CARTESIAN_POINT ( 'NONE',  ( 2.104549495715298590, -2.307096348898482585, 0.05917499873058817972 ) ) ;
#24418 = CARTESIAN_POINT ( 'NONE',  ( 3.226847753617521963, -1.718569378881330989, -0.7146659259855172586 ) ) ;
#24419 = CARTESIAN_POINT ( 'NONE',  ( 0.6823417656249917140, 4.842708333674755394, 1.181850606188765695 ) ) ;
#24420 = CARTESIAN_POINT ( 'NONE',  ( -5.935772324684618795, 5.819489221753827657, 0.000000000000000000 ) ) ;
#24421 = CARTESIAN_POINT ( 'NONE',  ( 7.623762449586013901, 7.788811034138823253, 1.040834085586084257E-14 ) ) ;
#24422 = FACE_OUTER_BOUND ( 'NONE', #24909, .T. ) ;
#24423 = CARTESIAN_POINT ( 'NONE',  ( 0.5925747745999773164, -2.090437052192719136, -0.2555399532009738350 ) ) ;
#24424 = EDGE_CURVE ( 'NONE', #186457, #26370, #72606, .T. ) ;
#24425 = CARTESIAN_POINT ( 'NONE',  ( 4.487385655998885170, 5.298000022495898520, 1.082531754730560403 ) ) ;
#24427 = DIRECTION ( 'NONE',  ( -0.7347175152297782397, 3.929830605827906454E-15, 0.6783731810844091381 ) ) ;
#24426 = CARTESIAN_POINT ( 'NONE',  ( -1.364683531250010295, 5.092708333674757171, 0.7879004041258379498 ) ) ;
#24428 = CARTESIAN_POINT ( 'NONE',  ( -15.75000000000000000, 9.799999999999998934, -3.200000000000001510 ) ) ;
#24429 = CARTESIAN_POINT ( 'NONE',  ( 2.092179824929023102, 1.308410154019133076, 1.668721082780571408 ) ) ;
#24430 = PLANE ( 'NONE',  #27052 ) ;
#24431 = CARTESIAN_POINT ( 'NONE',  ( 0.8791727066333665519, -1.827835516345464484, -0.8596444897858869227 ) ) ;
#24432 = CARTESIAN_POINT ( 'NONE',  ( 1.364683531249988757, 1.134375000341421247, 0.000000000000000000 ) ) ;
#24433 = CARTESIAN_POINT ( 'NONE',  ( -3.470524135418294520, 6.992769224722559684, -0.7216878364870267237 ) ) ;
#24434 = EDGE_CURVE ( 'NONE', #80483, #85779, #53990, .T. ) ;
#24435 = CARTESIAN_POINT ( 'NONE',  ( 4.299907273828439180, 8.168308919441841454, 1.040834085586084257E-14 ) ) ;
#24436 = CARTESIAN_POINT ( 'NONE',  ( 1.317891493549529391, -2.109231647155560108, 0.4722262556789079135 ) ) ;
#24439 = CARTESIAN_POINT ( 'NONE',  ( 4.853455804012228647, 4.764712647543454693, 0.7216878364870317197 ) ) ;
#24438 = LINE ( 'NONE', #54834, #54907 ) ;
#24437 = CARTESIAN_POINT ( 'NONE',  ( 4.199993725183334803, 8.122019456014369254, -0.7998128361456362523 ) ) ;
#24440 = CARTESIAN_POINT ( 'NONE',  ( -5.340986169140711226, 5.195848383611072485, 0.000000000000000000 ) ) ;
#24441 = CARTESIAN_POINT ( 'NONE',  ( 6.175017591530616023, 1.752142144017948100, -0.9981200475188132248 ) ) ;
#24442 = CARTESIAN_POINT ( 'NONE',  ( -8.026063749610056419, 10.38682701267698150, -1.443375672974059665 ) ) ;
#24443 = CARTESIAN_POINT ( 'NONE',  ( 6.603094310190187777, -0.4545541770063685760, 2.048106021177148683 ) ) ;
#24444 = CARTESIAN_POINT ( 'NONE',  ( -9.356506676016463686, 14.56575457568656340, -7.432410969268996581 ) ) ;
#24446 = CARTESIAN_POINT ( 'NONE',  ( -0.6823417656250003738, 10.65104166700806765, 1.181850606188754593 ) ) ;
#24445 = CARTESIAN_POINT ( 'NONE',  ( 0.7786449305766733886, -1.254482527970951056, 1.882701536962180677 ) ) ;
#24448 = CARTESIAN_POINT ( 'NONE',  ( -9.755255220232635693, 11.33988483081495957, -1.199719254218441611 ) ) ;
#24447 = B_SPLINE_CURVE_WITH_KNOTS ( 'NONE', 3,
 ( #24792, #12796, #143935, #205674, #26923, #142861, #126653, #90895, #107188, #209930 ),
 .UNSPECIFIED., .F., .F.,
 ( 4, 3, 3, 4 ),
 ( 0.000000000000000000, 8.893179197954895123E-05, 0.0001334007970840213895, 0.0001778705873658962123 ),
 .UNSPECIFIED. ) ;
#24450 = CARTESIAN_POINT ( 'NONE',  ( 1.071739250477701466, -0.8599075215434035524, 1.711803488807943197 ) ) ;
#24449 = CARTESIAN_POINT ( 'NONE',  ( -6.033015167956818026, 6.140865238812146742, -0.7216878364870267237 ) ) ;
#24451 = CARTESIAN_POINT ( 'NONE',  ( -0.6823417656250003738, 1.030208333674752286, -1.181850606188749264 ) ) ;
#24452 = LINE ( 'NONE', #123153, #165063 ) ;
#24453 = CARTESIAN_POINT ( 'NONE',  ( -0.7500000000000179856, 8.791666666666669627, 1.299038105676658228 ) ) ;
#24454 = CARTESIAN_POINT ( 'NONE',  ( 2.402614999361089243, 1.385809671090399986, -1.026769200382530167 ) ) ;
#24455 = CARTESIAN_POINT ( 'NONE',  ( 2.911969131885072670, 6.619324097166378706, 0.000000000000000000 ) ) ;
#24456 = CARTESIAN_POINT ( 'NONE',  ( 4.420840606507738357, 7.315341919971147355, 1.199719254218451159 ) ) ;
#24457 = CARTESIAN_POINT ( 'NONE',  ( 0.4030913312595973408, -0.4806107285681981423, 1.703151836983556988 ) ) ;
#24459 = CARTESIAN_POINT ( 'NONE',  ( 1.770182950735105898, 2.007541250849652847, -0.1504272076729237795 ) ) ;
#24458 = COLOUR_RGB ( '', 0.09019608, 0.27058824, 0.51372549) ;
#24460 = CARTESIAN_POINT ( 'NONE',  ( 4.524592175135637717, 1.360519573838222085, -1.737388959189074100 ) ) ;
#24461 = ORIENTED_EDGE ( 'NONE', *, *, #88143, .T. ) ;
#24463 = CARTESIAN_POINT ( 'NONE',  ( 7.415946836550703303, 11.59576237604377091, 0.7216878364870438212 ) ) ;
#24462 = VECTOR ( 'NONE', #57227, 1000.000000000000000 ) ;
#24464 = CARTESIAN_POINT ( 'NONE',  ( -5.264308783856126439, 9.363720357799287797, -0.7998128361456362523 ) ) ;
#24466 = CARTESIAN_POINT ( 'NONE',  ( 3.814077502958601595, 1.076299547611740293, -1.704950967544152984 ) ) ;
#24465 = CARTESIAN_POINT ( 'NONE',  ( 3.862070080935349203, 0.7130468835700142227, -1.997148454185311506 ) ) ;
#24468 = ORIENTED_EDGE ( 'NONE', *, *, #113441, .T. ) ;
#24467 = CARTESIAN_POINT ( 'NONE',  ( 3.691515636560299463, 1.703854809669336001, -0.6157217382992925536 ) ) ;
#24469 = CARTESIAN_POINT ( 'NONE',  ( 4.929271367020211514, 7.908511140569038922, 1.199719254218452047 ) ) ;
#24470 = ORIENTED_EDGE ( 'NONE', *, *, #51899, .F. ) ;
#24471 = CARTESIAN_POINT ( 'NONE',  ( 1.129532124359374334, -1.183843481993757774, -1.448407549327054955 ) ) ;
#24472 = CARTESIAN_POINT ( 'NONE',  ( 6.287720257080702702, 1.262826302610157381, 1.318732360701305062 ) ) ;
#24473 = CARTESIAN_POINT ( 'NONE',  ( -3.195971524519394702, 4.751719416737803847, -1.599625672291262513 ) ) ;
#24474 = CARTESIAN_POINT ( 'NONE',  ( -3.179715765502671321, 5.975770656120749535, 2.419999999999999485 ) ) ;
#24475 = CARTESIAN_POINT ( 'NONE',  ( 3.834746474454188013E-15, 8.843750000682797818, 1.500000000000001554 ) ) ;
#24476 = CARTESIAN_POINT ( 'NONE',  ( -1.364683531250014514, 2.051041667008086655, -0.7879004041258289570 ) ) ;
#24477 = DIRECTION ( 'NONE',  ( 0.000000000000000000, 1.000000000000000000, 0.000000000000000000 ) ) ;
#24478 = VERTEX_POINT ( 'NONE', #101142 ) ;
#24479 = CARTESIAN_POINT ( 'NONE',  ( 4.188685576152741064, 1.555700494002542067, -1.282988152656767911 ) ) ;
#24480 = CARTESIAN_POINT ( 'NONE',  ( 5.885648082108188461, 8.920320958217979879, 1.082531754730549967 ) ) ;
#24481 = CARTESIAN_POINT ( 'NONE',  ( -4.502716413514310290, 6.346531463890372926, -1.443375672974066548 ) ) ;
#24482 = CARTESIAN_POINT ( 'NONE',  ( -6.424584688029276514, 8.588711117491191871, 1.599625672291269396 ) ) ;
#24483 = CARTESIAN_POINT ( 'NONE',  ( 3.867525618572264623, -1.764951123045129577, -1.175235903013646332 ) ) ;
#24485 = CARTESIAN_POINT ( 'NONE',  ( -9.979823206198361163, 5.589814398814587193, -5.978750339097102184 ) ) ;
#24484 = CARTESIAN_POINT ( 'NONE',  ( -0.02948999725178608200, 2.884818527723536530, -2.415019744152223868 ) ) ;
#24486 = CARTESIAN_POINT ( 'NONE',  ( 4.481683897012714191, 1.285251931988955709, 1.494896804799286993 ) ) ;
#24487 = CARTESIAN_POINT ( 'NONE',  ( 0.6823417656249899377, 1.592708333674752730, 1.181850606188755259 ) ) ;
#24488 =( BOUNDED_CURVE ( )  B_SPLINE_CURVE ( 2, ( #153060, #134707, #183421, #367, #118492 ),
 .UNSPECIFIED., .F., .T. ) 
 B_SPLINE_CURVE_WITH_KNOTS ( ( 3, 2, 3 ),
 ( 0.02206790957329452310, 0.02500000000000000139, 0.02750504326964346713 ),
 .UNSPECIFIED. ) 
 CURVE ( )  GEOMETRIC_REPRESENTATION_ITEM ( )  RATIONAL_B_SPLINE_CURVE ( ( 0.9388936963964400473, 0.9528609242817545066, 1.000000000000000000, 0.9597265407336408316, 0.9436659034065904006 ) ) 
 REPRESENTATION_ITEM ( '' )  );
#24489 = CARTESIAN_POINT ( 'NONE',  ( 0.08813964471556486047, 1.162479488604960753, 1.643474645366525877 ) ) ;
#24490 = EDGE_LOOP ( 'NONE', ( #100836, #134352, #95562, #79415 ) ) ;
#24491 = CARTESIAN_POINT ( 'NONE',  ( 0.1228732512454956405, 0.3668972607131052999, 2.085061435120295847 ) ) ;
#24492 = CARTESIAN_POINT ( 'NONE',  ( 8.208643724399392383, 14.14623621761441363, 8.753817594573789052 ) ) ;
#24493 = CARTESIAN_POINT ( 'NONE',  ( 1.434126425884488354, 1.231690216755284562, 1.664001042209894088 ) ) ;
#24494 = CARTESIAN_POINT ( 'NONE',  ( 6.180537922983273091, 8.303989891604203422, -1.599625672291281386 ) ) ;
#24495 = VERTEX_POINT ( 'NONE', #69699 ) ;
#24496 = CARTESIAN_POINT ( 'NONE',  ( 6.391743074199808916, 6.421731439513382433, -0.7998128361456481317 ) ) ;
#24497 = CARTESIAN_POINT ( 'NONE',  ( 5.688527969385528849, 8.794310509995222347, -1.199719254218452047 ) ) ;
#24499 = CARTESIAN_POINT ( 'NONE',  ( 4.306686350635271054, 8.176217842383143974, -0.7998128361456221525 ) ) ;
#24498 = CARTESIAN_POINT ( 'NONE',  ( 3.556657146437085970, -1.843967315269653628, -0.9851420625589295543 ) ) ;
#24501 = EDGE_CURVE ( 'NONE', #209728, #173454, #200462, .T. ) ;
#24500 = CARTESIAN_POINT ( 'NONE',  ( 7.364013710877980401, 8.620379413226322285, -1.199719254218452047 ) ) ;
#24504 = ORIENTED_EDGE ( 'NONE', *, *, #195285, .F. ) ;
#24503 = CARTESIAN_POINT ( 'NONE',  ( 1.611653755202663518, -0.6102688749147866520, 1.705724428093706946 ) ) ;
#24502 = CARTESIAN_POINT ( 'NONE',  ( 1.940199132888191791, 1.805219978825555627, 0.2711003711317952480 ) ) ;
#24505 = CARTESIAN_POINT ( 'NONE',  ( 5.479209177496175087, -0.05098606815037013545, -2.206463706674952618 ) ) ;
#24506 = DIRECTION ( 'NONE',  ( 0.000000000000000000, 0.000000000000000000, 1.000000000000000000 ) ) ;
#24507 = CARTESIAN_POINT ( 'NONE',  ( 3.821466819111440927, -0.1649144712266135959, 2.200675313789305143 ) ) ;
#24508 = CARTESIAN_POINT ( 'NONE',  ( 8.444030743212801227, 8.745790710036752458, 0.7998128361456462443 ) ) ;
#24510 =( BOUNDED_SURFACE ( )  B_SPLINE_SURFACE ( 3, 3, ( 
 ( #98415, #35537, #117931, #183925, #65875, #165544, #198033, #214244, #180725, #148242, #877 ),
 ( #18209, #200159, #134150, #116852, #1948, #85363, #33408, #34472, #202286, #32350, #3018 ),
 ( #151445, #149296, #17137, #82150, #133083, #100544, #84293, #168746, #4083, #20350, #150378 ),
 ( #66943, #101614, #132023, #114727, #68010, #199081, #115786, #167681, #19281, #69086, #99486 ),
 ( #164479, #135207, #52864, #184976, #50727, #36601, #70154, #136266, #16066, #49663, #83214 ),
 ( #181774, #87511, #105934, #38755, #8375, #89657, #58203, #57136, #137337, #206575, #203354 ),
 ( #5145, #122231, #103762, #121157, #40906, #157856, #74458, #156789, #155710, #91799, #107012 ) ),
 .UNSPECIFIED., .T., .F., .F. ) 
 B_SPLINE_SURFACE_WITH_KNOTS ( ( 4, 3, 4 ),
 ( 4, 1, 1, 1, 1, 1, 1, 1, 4 ),
 ( 0.000000000000000000, 0.5000000000000000000, 1.000000000000000000 ),
 ( 0.000000000000000000, 0.2255619619413396781, 0.3975297875667437308, 0.5250373104567740423, 0.6172314665434700531, 0.6832587661106447330, 0.7322037845459880012, 0.7729093456892226488, 1.000000000000000000 ),
 .UNSPECIFIED. ) 
 GEOMETRIC_REPRESENTATION_ITEM ( )  RATIONAL_B_SPLINE_SURFACE ( (
 ( 1.000000000000000000, 1.000000000000000000, 1.000000000000000444, 0.9999999999999996669, 1.000000000000000222, 0.9999999999999996669, 1.000000000000000444, 1.000000000000000000, 1.000000000000000000, 1.000000000000000000, 1.000000000000000000),
 ( 0.3333333333333333703, 0.3333333333333333703, 0.3333333333333334814, 0.3333333333333332038, 0.3333333333333333703, 0.3333333333333332593, 0.3333333333333334814, 0.3333333333333333703, 0.3333333333333334814, 0.3333333333333333703, 0.3333333333333333703),
 ( 0.3333333333333333703, 0.3333333333333333703, 0.3333333333333334814, 0.3333333333333332038, 0.3333333333333333703, 0.3333333333333332593, 0.3333333333333334814, 0.3333333333333333703, 0.3333333333333334814, 0.3333333333333333703, 0.3333333333333333703),
 ( 1.000000000000000000, 1.000000000000000000, 1.000000000000000444, 0.9999999999999996669, 1.000000000000000222, 0.9999999999999996669, 1.000000000000000444, 1.000000000000000000, 1.000000000000000000, 1.000000000000000000, 1.000000000000000000),
 ( 0.3333333333333333703, 0.3333333333333333703, 0.3333333333333334814, 0.3333333333333332038, 0.3333333333333333703, 0.3333333333333332593, 0.3333333333333334814, 0.3333333333333333703, 0.3333333333333334814, 0.3333333333333333703, 0.3333333333333333703),
 ( 0.3333333333333333703, 0.3333333333333333703, 0.3333333333333334814, 0.3333333333333332038, 0.3333333333333333703, 0.3333333333333332593, 0.3333333333333334814, 0.3333333333333333703, 0.3333333333333334814, 0.3333333333333333703, 0.3333333333333333703),
 ( 1.000000000000000000, 1.000000000000000000, 1.000000000000000444, 0.9999999999999996669, 1.000000000000000222, 0.9999999999999996669, 1.000000000000000444, 1.000000000000000000, 1.000000000000000000, 1.000000000000000000, 1.000000000000000000) ) ) 
 REPRESENTATION_ITEM ( '' )  SURFACE ( )  );
#24509 = CARTESIAN_POINT ( 'NONE',  ( 1.364683531249997417, 8.546875000341403350, 2.602085213965210642E-15 ) ) ;
#24511 = CARTESIAN_POINT ( 'NONE',  ( 3.316961667764028121, 1.505919282548912719, -1.178437403786938731 ) ) ;
#24512 = CARTESIAN_POINT ( 'NONE',  ( 7.587759525142423911, 12.00413654597487501, 0.7998128361456462443 ) ) ;
#24513 = CARTESIAN_POINT ( 'NONE',  ( 5.143061708805018561, -0.2499388813127951525, -2.055141626981969338 ) ) ;
#24515 = CARTESIAN_POINT ( 'NONE',  ( -11.43204722947019825, 11.15592754026171463, 3.649275849833181429 ) ) ;
#24514 = CARTESIAN_POINT ( 'NONE',  ( 1.573645197550626484, 8.680485584337372273, -2.499999999999989342 ) ) ;
#24516 = CARTESIAN_POINT ( 'NONE',  ( 5.530878137806295669, -1.981686641427220286, 0.9361944923952856268 ) ) ;
#24517 = VERTEX_POINT ( 'NONE', #102224 ) ;
#24518 = VERTEX_POINT ( 'NONE', #183465 ) ;
#24519 = CARTESIAN_POINT ( 'NONE',  ( -9.567202289542830584, -7.627132808484212489, 0.008219159353564688131 ) ) ;
#24520 = CARTESIAN_POINT ( 'NONE',  ( -0.2534910766302378438, 3.934660213246439220, 11.56267633880227130 ) ) ;
#24521 = CARTESIAN_POINT ( 'NONE',  ( 4.760848217054122422, 5.583353003765119560, -1.199719254218452047 ) ) ;
#24522 = CARTESIAN_POINT ( 'NONE',  ( 1.001543065824772753E-15, -1.859374999522040550, 3.793834371823810780 ) ) ;
#24523 = FACE_OUTER_BOUND ( 'NONE', #34660, .T. ) ;
#24524 = VECTOR ( 'NONE', #74998, 1000.000000000000000 ) ;
#24525 = CARTESIAN_POINT ( 'NONE',  ( -7.036318535812428721, 11.15286269184909784, 0.000000000000000000 ) ) ;
#24526 = CARTESIAN_POINT ( 'NONE',  ( 4.248501033035879004, 6.049946853332221153, -1.599625672291273171 ) ) ;
#24527 = CARTESIAN_POINT ( 'NONE',  ( 5.278213287142951238, -1.102824678039602269, -1.751873656341627505 ) ) ;
#24528 = CARTESIAN_POINT ( 'NONE',  ( 4.318917837333097864, 1.761897194459721927, 0.7795765077616281236 ) ) ;
#24529 = CARTESIAN_POINT ( 'NONE',  ( 6.538674910786447469, -1.636584463124007627, 1.342808005693174156 ) ) ;
#24530 = CARTESIAN_POINT ( 'NONE',  ( 0.000000000000000000, 0.9200000000000041478, 6.249999999999995559 ) ) ;
#24532 = CARTESIAN_POINT ( 'NONE',  ( 2.898410978271408922, 6.603506251283770112, -0.7998128361456362523 ) ) ;
#24531 = B_SPLINE_CURVE_WITH_KNOTS ( 'NONE', 3,
 ( #205671, #59432, #126650, #41077 ),
 .UNSPECIFIED., .F., .F.,
 ( 4, 4 ),
 ( 1.685346633177199101E-15, 0.0005562209383481761353 ),
 .UNSPECIFIED. ) ;
#24533 = CARTESIAN_POINT ( 'NONE',  ( -4.185765024244170185, 3.976674809167545011, -0.5846519713818258968 ) ) ;
#24534 = CARTESIAN_POINT ( 'NONE',  ( 0.07648947921621782053, -2.126777779243053779, -0.5280787695999613618 ) ) ;
#24535 = CARTESIAN_POINT ( 'NONE',  ( 5.549374350267230582, -1.441814640532925074, -1.119852386600270311 ) ) ;
#24536 = CARTESIAN_POINT ( 'NONE',  ( 5.777182853198898904, 6.873039762554409293, -1.082531754730548412 ) ) ;
#24537 = CARTESIAN_POINT ( 'NONE',  ( 3.917943204224906939, 5.594019709727598766, -1.443375672974051449 ) ) ;
#24538 = CARTESIAN_POINT ( 'NONE',  ( -5.468734858265826837, 7.473552982767158070, 1.599625672291263179 ) ) ;
#24539 = CARTESIAN_POINT ( 'NONE',  ( 4.436542580169809291, 6.199052314996659874, 1.599625672291267398 ) ) ;
#24540 = CARTESIAN_POINT ( 'NONE',  ( 3.932747076415766596, 6.745899468197171345, 1.199719254218451159 ) ) ;
#24541 = VERTEX_POINT ( 'NONE', #213809 ) ;
#24543 = CARTESIAN_POINT ( 'NONE',  ( 5.888937080504050847, -1.913070152547487579, -0.6273127349021755395 ) ) ;
#24542 = CARTESIAN_POINT ( 'NONE',  ( 2.471991059931688106, -1.762569054296094340, -0.5325411743367302053 ) ) ;
#24544 = CARTESIAN_POINT ( 'NONE',  ( 1.001802975355575054, 2.264736134964080438, 0.3911735967057332064 ) ) ;
#24545 = CARTESIAN_POINT ( 'NONE',  ( 6.596542563702321615, 1.939940506139478327, 0.2910815776849539627 ) ) ;
#24546 = CARTESIAN_POINT ( 'NONE',  ( -6.403528624356093601, 6.365204904703887223, 1.040834085586084257E-14 ) ) ;
#24547 = DIRECTION ( 'NONE',  ( 2.949029909160572061E-17, 1.000000000000000000, -8.673600428462429131E-15 ) ) ;
#24548 = CARTESIAN_POINT ( 'NONE',  ( -3.755772246185468788, 4.340488027759846545, -1.199719254218452047 ) ) ;
#24549 = CARTESIAN_POINT ( 'NONE',  ( 0.8364851226981102617, -1.151554295457988930, 1.720357586142134076 ) ) ;
#24550 = CARTESIAN_POINT ( 'NONE',  ( -2.972980823146582186, 6.690504403638126263, 0.000000000000000000 ) ) ;
#24552 = CARTESIAN_POINT ( 'NONE',  ( 1.445950363956361340, 1.868363765441739099, 0.09516058986362013750 ) ) ;
#24551 = CARTESIAN_POINT ( 'NONE',  ( 2.525039811729863359, -1.949768895325499463, 0.7551890176837258162 ) ) ;
#24553 = CARTESIAN_POINT ( 'NONE',  ( 1.511092056569414366, 2.013677475703846476, 0.1017375232199163593 ) ) ;
#24554 = CARTESIAN_POINT ( 'NONE',  ( 9.585251415181632595, 10.28514086057449184, 0.000000000000000000 ) ) ;
#24555 = ORIENTED_EDGE ( 'NONE', *, *, #41976, .F. ) ;
#24556 = CARTESIAN_POINT ( 'NONE',  ( -1.364683531249997417, 4.821875000341417916, 1.214306433183764966E-14 ) ) ;
#24557 = CARTESIAN_POINT ( 'NONE',  ( 1.663200723894017852, 0.8946008992836312901, 1.492777717291964512 ) ) ;
#24558 = AXIS2_PLACEMENT_3D ( 'NONE', #13575, #28774, #211765 ) ;
#24559 = CARTESIAN_POINT ( 'NONE',  ( 5.717788096661236885, 7.693838750903348789, 1.599625672291267398 ) ) ;
#24561 = CARTESIAN_POINT ( 'NONE',  ( 0.1009995753616280273, 2.612933547399907130, -1.997555607063249861 ) ) ;
#24560 = PRESENTATION_STYLE_ASSIGNMENT (( #39766 ) ) ;
#24562 = CARTESIAN_POINT ( 'NONE',  ( 3.211258912624019857, -0.3355696072399985685, 1.691725950409156631 ) ) ;
#24563 = CARTESIAN_POINT ( 'NONE',  ( 2.788834510562918645, 1.878274557074947948, -1.128960604485473862 ) ) ;
#24564 = CARTESIAN_POINT ( 'NONE',  ( 5.496761087669068679, -0.5331231007881258588, -2.141394884921154151 ) ) ;
#24565 = CARTESIAN_POINT ( 'NONE',  ( -9.813523197712067159, 5.212597839642568509, -6.298667959258508198 ) ) ;
#24566 =( BOUNDED_CURVE ( )  B_SPLINE_CURVE ( 2, ( #25226, #91329, #157389, #75056, #105446, #37212, #55599, #103286, #153101, #136862, #139006, #21994, #38283, #4676, #70750, #154175, #71820, #187722, #202887, #39350, #120679, #104360, #170405, #205028, #6822, #72901, #56674, #126020, #160569, #46847, #194130, #59868, #42583, #43647, #208236, #128168, #191980, #124957, #96670, #193057, #45779, #95606, #92405, #111896, #178973, #177900, #161655, #212503, #108687, #60937, #174716, #78249, #29513, #12177, #159503, #195210, #80388 ),
 .UNSPECIFIED., .F., .T. ) 
 B_SPLINE_CURVE_WITH_KNOTS ( ( 3, 2, 2, 2, 2, 2, 2, 2, 2, 2, 2, 2, 2, 2, 2, 2, 2, 2, 2, 2, 2, 2, 2, 2, 2, 2, 2, 2, 3 ),
 ( 0.2844739210328581791, 0.2916666666666666852, 0.2999999999999999889, 0.3083333333333333481, 0.3166666666666666519, 0.3250000000000000111, 0.3333333333333333148, 0.3416666666666666741, 0.3499999999999999778, 0.3583333333333333370, 0.3666666666666666408, 0.3750000000000000000, 0.3833333333333333592, 0.3916666666666666630, 0.4000000000000000222, 0.4083333333333333259, 0.4166666666666666852, 0.4249999999999999889, 0.4333333333333333481, 0.4416666666666666519, 0.4500000000000000111, 0.4583333333333333148, 0.4666666666666666741, 0.4749999999999999778, 0.4833333333333333370, 0.4916666666666666408, 0.5000000000000000000, 0.5083333333333333037, 0.5122792266304363462 ),
 .UNSPECIFIED. ) 
 CURVE ( )  GEOMETRIC_REPRESENTATION_ITEM ( )  RATIONAL_B_SPLINE_CURVE ( ( 0.9683452906431593288, 0.8843625769635120593, 1.000000000000000000, 0.8660254037844387076, 1.000000000000000000, 0.8660254037844387076, 1.000000000000000000, 0.8660254037844387076, 1.000000000000000000, 0.8660254037844387076, 1.000000000000000000, 0.8660254037844387076, 1.000000000000000000, 0.8660254037844387076, 1.000000000000000000, 0.8660254037844387076, 1.000000000000000000, 0.8660254037844387076, 1.000000000000000000, 0.8660254037844387076, 1.000000000000000000, 0.8660254037844387076, 1.000000000000000000, 0.8660254037844387076, 1.000000000000000000, 0.8660254037844387076, 1.000000000000000000, 0.8660254037844387076, 1.000000000000000000, 0.8660254037844387076, 1.000000000000000000, 0.8660254037844387076, 1.000000000000000000, 0.8660254037844387076, 1.000000000000000000, 0.8660254037844387076, 1.000000000000000000, 0.8660254037844387076, 1.000000000000000000, 0.8660254037844387076, 1.000000000000000000, 0.8660254037844387076, 1.000000000000000000, 0.8660254037844387076, 1.000000000000000000, 0.8660254037844387076, 1.000000000000000000, 0.8660254037844387076, 1.000000000000000000, 0.8660254037844387076, 1.000000000000000000, 0.8660254037844387076, 1.000000000000000000, 0.8660254037844387076, 1.000000000000000000, 0.9365620646573122876, 0.9332007670388082765 ) ) 
 REPRESENTATION_ITEM ( '' )  );
#24567 = CARTESIAN_POINT ( 'NONE',  ( 2.096751143937364947, 2.146985459555655673, 0.3218790139906148040 ) ) ;
#24568 = CARTESIAN_POINT ( 'NONE',  ( 0.5217476098421744979, -0.9739702522407606144, -1.544006022310390192 ) ) ;
#24569 = CARTESIAN_POINT ( 'NONE',  ( 0.08058608058607655278, -9.900000000000005684, 10.99970480893082225 ) ) ;
#24570 = CARTESIAN_POINT ( 'NONE',  ( 4.259064461820570635, -0.003692207519963904699, -2.117513409117043999 ) ) ;
#24571 = CARTESIAN_POINT ( 'NONE',  ( 6.539320575229256249, 4.699150603835311912, 2.459441311396874941 ) ) ;
#24572 = ORIENTED_EDGE ( 'NONE', *, *, #163868, .T. ) ;
#24574 = CARTESIAN_POINT ( 'NONE',  ( -0.6823417656250003738, 0.7802083336747520637, -1.181850606188749264 ) ) ;
#24573 = CARTESIAN_POINT ( 'NONE',  ( 4.353268756680241047, 0.5026898720560546430, -2.236438357558430123 ) ) ;
#24575 = CARTESIAN_POINT ( 'NONE',  ( 2.364109784339328312E-15, 11.09999999999999609, -5.500000000000003553 ) ) ;
#24576 = CARTESIAN_POINT ( 'NONE',  ( 2.530568227245037605, 6.104080031761181857, 0.000000000000000000 ) ) ;
#24577 = CARTESIAN_POINT ( 'NONE',  ( 0.4871770963560326240, -1.998059126451703138, -0.7104936405118513765 ) ) ;
#24578 = CARTESIAN_POINT ( 'NONE',  ( -4.595850885352567694, 8.305650432979225783, 1.040834085586084257E-14 ) ) ;
#24579 = EDGE_CURVE ( 'NONE', #154420, #6976, #19890, .T. ) ;
#24580 = CARTESIAN_POINT ( 'NONE',  ( 4.202664430556257713, 4.965825259479493603, 1.082531754730560403 ) ) ;
#24581 = CARTESIAN_POINT ( 'NONE',  ( -6.846504384776765484, 8.050305206070113684, -1.082531754730543083 ) ) ;
#24582 = CARTESIAN_POINT ( 'NONE',  ( 4.177320726786311056, 5.966903162707725805, -1.443375672974068769 ) ) ;
#24583 = ORIENTED_EDGE ( 'NONE', *, *, #115695, .T. ) ;
#24584 = CARTESIAN_POINT ( 'NONE',  ( 4.729138786257041538, 2.011204126674607462, 0.1455352507326590494 ) ) ;
#24586 = CARTESIAN_POINT ( 'NONE',  ( 3.450102088163331082, -0.8403066601648312428, 1.883826651212586745 ) ) ;
#24585 = CARTESIAN_POINT ( 'NONE',  ( 6.308621549060418054, 6.254479983525607523, 0.7998128361456341429 ) ) ;
#24588 = CARTESIAN_POINT ( 'NONE',  ( -0.1409997244346088141, 7.629137130509076492, -2.600278764091648487 ) ) ;
#24587 = DIRECTION ( 'NONE',  ( 0.000000000000000000, -1.000000000000000000, 0.000000000000000000 ) ) ;
#24589 = CARTESIAN_POINT ( 'NONE',  ( 3.973948422136968084, 5.729635473950147606, -1.443375672974068769 ) ) ;
#24590 = CARTESIAN_POINT ( 'NONE',  ( 1.642778471875001811, -3.842708332855375275, 2.845375778867859751 ) ) ;
#24591 =( NAMED_UNIT ( * ) SI_UNIT ( $, .STERADIAN. ) SOLID_ANGLE_UNIT ( ) );
#24592 = CARTESIAN_POINT ( 'NONE',  ( 6.474583112218436298, -0.1034247314782872212, -2.189140632845664403 ) ) ;
#24593 = CARTESIAN_POINT ( 'NONE',  ( 3.076796235938107138, -0.8146265060355701859, 1.844709937164576097 ) ) ;
#24594 = CARTESIAN_POINT ( 'NONE',  ( 3.333393596924072444, 0.8250370302015205271, -1.646115572170883112 ) ) ;
#24595 = CARTESIAN_POINT ( 'NONE',  ( 6.226218857173709154, 8.287007971501239467, 1.599625672291281386 ) ) ;
#24596 = CARTESIAN_POINT ( 'NONE',  ( 6.334959139596201716, 0.1821375521317940283, 1.816452708017932238 ) ) ;
#24597 = CARTESIAN_POINT ( 'NONE',  ( 0.1417928296247125686, 0.8878553654741733192, 2.120496703859587662 ) ) ;
#24598 = CARTESIAN_POINT ( 'NONE',  ( -7.009729113465285266, 8.136771039586342624, -1.199719254218446718 ) ) ;
#24599 = CARTESIAN_POINT ( 'NONE',  ( 0.5271418889439123401, 2.165442452462429834, 0.6551351998097357798 ) ) ;
#24600 = CARTESIAN_POINT ( 'NONE',  ( 1.559346616682453668, -1.807134503733454078, -1.081319387842846425 ) ) ;
#24601 = CARTESIAN_POINT ( 'NONE',  ( -5.098748287191073203, 8.106234214101666780, 1.199719254218452935 ) ) ;
#24602 = CARTESIAN_POINT ( 'NONE',  ( 9.088043039861931405, 9.497138389460751284, 1.040834085586084257E-14 ) ) ;
#24603 = CARTESIAN_POINT ( 'NONE',  ( 7.309254211098760834, 8.660456346770972758, 1.082531754730549967 ) ) ;
#24604 = CARTESIAN_POINT ( 'NONE',  ( -7.549192604710863286, 7.701812881784464437, -0.7998128361456291469 ) ) ;
#24605 = EDGE_CURVE ( 'NONE', #188712, #142732, #149508, .T. ) ;
#24606 = CARTESIAN_POINT ( 'NONE',  ( 6.087247782411444597, 10.04561347954795281, -0.7216878364870267237 ) ) ;
#24607 = CARTESIAN_POINT ( 'NONE',  ( 4.009205846845453003, 7.815100513429686480, -0.2297154615349787654 ) ) ;
#24608 = CARTESIAN_POINT ( 'NONE',  ( -5.087333953625788219, 6.958308917361963886, 1.599625672291267398 ) ) ;
#24610 = CARTESIAN_POINT ( 'NONE',  ( 4.078556047614148028, 1.049247773278503049, 1.958029639119197585 ) ) ;
#24609 = CARTESIAN_POINT ( 'NONE',  ( 2.232824136269210502, 1.381628265877183903, -1.608862310199298928 ) ) ;
#24611 = CARTESIAN_POINT ( 'NONE',  ( 1.992365796559266267, -0.5863786240636534863, -2.111471653062434672 ) ) ;
#24612 = CARTESIAN_POINT ( 'NONE',  ( 0.5752038918783763943, -2.079344756725898691, -0.7397341299467049547 ) ) ;
#24613 = CARTESIAN_POINT ( 'NONE',  ( -5.808742468812186033, 5.741564066561132940, 0.000000000000000000 ) ) ;
#24614 = CARTESIAN_POINT ( 'NONE',  ( 4.264078424595136418, -1.956757550135434620, 0.1421211968542570592 ) ) ;
#24615 = CARTESIAN_POINT ( 'NONE',  ( 8.191097360950562845, 12.70803068775103739, -0.7998128361456352531 ) ) ;
#24616 = CARTESIAN_POINT ( 'NONE',  ( 4.227444969362701421, 3.826440640544909400, 1.214306433183764966E-14 ) ) ;
#24617 = CARTESIAN_POINT ( 'NONE',  ( 0.6823417656249899377, 0.5927083336747518416, 1.181850606188755259 ) ) ;
#24618 = CARTESIAN_POINT ( 'NONE',  ( -4.841670253855968831, 4.821239182352949904, 0.000000000000000000 ) ) ;
#24620 = ORIENTED_EDGE ( 'NONE', *, *, #1218, .T. ) ;
#24619 = CARTESIAN_POINT ( 'NONE',  ( -5.504247177468192476, 7.444707678511436555, 1.443375672974064550 ) ) ;
#24621 = AXIS2_PLACEMENT_3D ( 'NONE', #104067, #121462, #187432 ) ;
#24622 = CARTESIAN_POINT ( 'NONE',  ( 3.076547362214879566, 0.9570632234598417387, 1.892448740577145738 ) ) ;
#24623 = CARTESIAN_POINT ( 'NONE',  ( -5.171509248969888617, 4.998125310078441075, 0.7998128361456281477 ) ) ;
#24624 = CARTESIAN_POINT ( 'NONE',  ( 5.032170685167933755, 1.114402916724830161, -1.852182961850391774 ) ) ;
#24625 = CARTESIAN_POINT ( 'NONE',  ( 4.229911503591711863, 1.806553461410321582, 0.3548724298726435022 ) ) ;
#24626 = CARTESIAN_POINT ( 'NONE',  ( -5.693503466768185639, 6.133329901302775333, 0.7540896269448340572 ) ) ;
#24627 = CARTESIAN_POINT ( 'NONE',  ( -1.201851678989727383E-14, 1.134375000341418582, 1.575800808251672791 ) ) ;
#24628 = CARTESIAN_POINT ( 'NONE',  ( -0.07713737713477014646, -1.067615817814296042, -1.374817276609247907 ) ) ;
#24629 = CARTESIAN_POINT ( 'NONE',  ( 6.827182134110177714, 4.703275060517408512, 2.273677308227497917 ) ) ;
#24630 = CARTESIAN_POINT ( 'NONE',  ( 4.202664430556261266, 4.005456045178151570, 0.7216878364870317197 ) ) ;
#24631 = CARTESIAN_POINT ( 'NONE',  ( -5.593777659986292505, 7.397990072842402398, -1.241664499109219166 ) ) ;
#24632 = CARTESIAN_POINT ( 'NONE',  ( 3.889662759143839299, 1.564074849111227516, 1.492423382767386730 ) ) ;
#24633 = CARTESIAN_POINT ( 'NONE',  ( -3.737243898861318137, 7.511868315313511069, 0.7998128361456341429 ) ) ;
#24634 = CARTESIAN_POINT ( 'NONE',  ( 5.132185397524263060, 0.2004025303571632666, -2.006139158026089220 ) ) ;
#24635 = CARTESIAN_POINT ( 'NONE',  ( -6.846504384776750385, 10.93141284897413890, -0.7216878364870267237 ) ) ;
#24636 = CARTESIAN_POINT ( 'NONE',  ( 4.030267251519312310, 1.158562084521784108, -1.824840551714689507 ) ) ;
#24637 = CARTESIAN_POINT ( 'NONE',  ( 4.059811131046401123, 1.956822991617146457, -0.2382644796226577599 ) ) ;
#24638 = CARTESIAN_POINT ( 'NONE',  ( 0.000000000000000000, 4.446955548196618757, 0.000000000000000000 ) ) ;
#24639 = CARTESIAN_POINT ( 'NONE',  ( 1.536587678696316184, 1.135727589777148605, -2.008695742776007709 ) ) ;
#24640 = CARTESIAN_POINT ( 'NONE',  ( 3.514965343742028736, 1.861552560010207191, 0.8843320499443955152 ) ) ;
#24641 = CARTESIAN_POINT ( 'NONE',  ( 5.249535210367334948, 1.939651965044559390, -0.09935550175556999430 ) ) ;
#24643 = ORIENTED_EDGE ( 'NONE', *, *, #61688, .T. ) ;
#24642 = CARTESIAN_POINT ( 'NONE',  ( -7.985389288324697965, 10.33937347451072775, -1.443375672974058777 ) ) ;
#24644 = CARTESIAN_POINT ( 'NONE',  ( -7.456058132872594335, 7.663432341298296535, 0.000000000000000000 ) ) ;
#24645 = DIRECTION ( 'NONE',  ( -0.7592566023652990159, -0.6507913734559659380, 0.000000000000000000 ) ) ;
#24646 = EDGE_CURVE ( 'NONE', #77611, #155158, #170223, .T. ) ;
#24648 = ORIENTED_EDGE ( 'NONE', *, *, #30406, .T. ) ;
#24647 = CARTESIAN_POINT ( 'NONE',  ( 0.3870774458628380987, 0.9691415390508764105, -11.89165654491649526 ) ) ;
#24649 = CARTESIAN_POINT ( 'NONE',  ( -6.819388077549415783, 10.89977715720891815, 0.7216878364870458196 ) ) ;
#24650 = CARTESIAN_POINT ( 'NONE',  ( 2.573496151666111231, 0.1090403232480302298, -2.204208057042057245 ) ) ;
#24651 = CARTESIAN_POINT ( 'NONE',  ( -1.642778471875000035, -0.1677083328553742592, -2.845375778867859751 ) ) ;
#24652 = EDGE_LOOP ( 'NONE', ( #78227, #100239, #211382, #68722 ) ) ;
#24653 = CARTESIAN_POINT ( 'NONE',  ( 1.041598845562411890, 1.244476351500271472, 1.383831004058704961 ) ) ;
#24654 = CARTESIAN_POINT ( 'NONE',  ( 6.539320575229274901, 4.692178491785949923, 2.665866134390063813 ) ) ;
#24655 = CARTESIAN_POINT ( 'NONE',  ( -1.499999999999997780, 5.181250000682820378, 1.214306433183764966E-14 ) ) ;
#24656 = FILL_AREA_STYLE_COLOUR ( '', #47616 ) ;
#24658 = DIRECTION ( 'NONE',  ( -0.9989777552170296948, -3.541417115716614946E-16, -0.04520447523801517098 ) ) ;
#24657 = CARTESIAN_POINT ( 'NONE',  ( -6.041797769283476782, 7.151762567314746022, -1.181783516275588752 ) ) ;
#24659 = CARTESIAN_POINT ( 'NONE',  ( 5.384640740818634086, 1.621930891500168226, -0.8712783443201176370 ) ) ;
#24660 = ORIENTED_EDGE ( 'NONE', *, *, #21981, .F. ) ;
#24661 = CARTESIAN_POINT ( 'NONE',  ( 2.202092877552201067, -2.060466153685360791, 0.04932271190436626068 ) ) ;
#24662 = CARTESIAN_POINT ( 'NONE',  ( -1.360316468750040642, 1.161458333674751486, 0.7853790794158861388 ) ) ;
#24663 = CARTESIAN_POINT ( 'NONE',  ( -6.775324078527193983, 8.927630729746953264, -1.599625672291263179 ) ) ;
#24664 = CARTESIAN_POINT ( 'NONE',  ( 10.91893890296302416, -9.990657656777852225, -0.1342453211083859954 ) ) ;
#24665 = FACE_OUTER_BOUND ( 'NONE', #156276, .T. ) ;
#24666 = CARTESIAN_POINT ( 'NONE',  ( 4.822949958159288286, 6.649860922651058992, -1.599625672291256295 ) ) ;
#24667 = CARTESIAN_POINT ( 'NONE',  ( 0.6552379465495603572, -1.740689658905628878, -1.102993579323052753 ) ) ;
#24668 = ADVANCED_FACE ( 'NONE', ( #171490 ), #155249, .T. ) ;
#24670 = CARTESIAN_POINT ( 'NONE',  ( 4.739718475747470627, 1.836682745182907972, 0.1304020654292817605 ) ) ;
#24669 = DIRECTION ( 'NONE',  ( -0.000000000000000000, 1.000000000000000000, -0.000000000000000000 ) ) ;
#24671 = CARTESIAN_POINT ( 'NONE',  ( 7.039708073993665494, 9.236078724457858158, 1.599625672291281386 ) ) ;
#24672 = CARTESIAN_POINT ( 'NONE',  ( -5.818384198920079520, 6.817144982608731141, 1.199719254218452935 ) ) ;
#24674 = ORIENTED_EDGE ( 'NONE', *, *, #41280, .F. ) ;
#24673 = CARTESIAN_POINT ( 'NONE',  ( 7.005397802120290507, 5.950282834973755541, 2.500000000000000444 ) ) ;
#24675 = CARTESIAN_POINT ( 'NONE',  ( 3.932405576212230525, 1.181341412803040614, -1.863887651898883613 ) ) ;
#24676 = CARTESIAN_POINT ( 'NONE',  ( 0.5620833348847533717, 2.138143771118843350, -0.3165822943479515983 ) ) ;
#24677 = CARTESIAN_POINT ( 'NONE',  ( -6.575341312947811545, 6.773579074634973551, 1.040834085586084257E-14 ) ) ;
#24678 = CARTESIAN_POINT ( 'NONE',  ( 0.7207899753199145110, 1.446443371814851941, -1.251069288267861346 ) ) ;
#24679 = CARTESIAN_POINT ( 'NONE',  ( 1.200408080392855181, 1.350732740426639822, -1.497504596960941958 ) ) ;
#24680 = CARTESIAN_POINT ( 'NONE',  ( 0.006768871532346317291, 8.210909518262139883, 2.038649385027042626 ) ) ;
#24681 = CARTESIAN_POINT ( 'NONE',  ( 1.581885565347431966, 1.542867095709683056, -1.703685752350136751 ) ) ;
#24682 = CARTESIAN_POINT ( 'NONE',  ( 8.397938042107668366, 15.16470181921706306, -8.573252516252733102 ) ) ;
#24683 = CARTESIAN_POINT ( 'NONE',  ( 6.393217174440144035, -0.09883813596619006603, -1.909861267343159863 ) ) ;
#24684 = DIRECTION ( 'NONE',  ( 0.000000000000000000, -1.000000000000000000, 0.000000000000000000 ) ) ;
#24685 = CARTESIAN_POINT ( 'NONE',  ( 0.2505829665140328899, -1.505242420826727656, 1.110479572284161831 ) ) ;
#24686 = CARTESIAN_POINT ( 'NONE',  ( 2.009000277268524481, 0.004839059525654776373, 2.016708403978189956 ) ) ;
#24688 = CARTESIAN_POINT ( 'NONE',  ( -4.271379415251800538, 7.751480557515569636, 0.6337447475577907552 ) ) ;
#24687 = CARTESIAN_POINT ( 'NONE',  ( -1.364683531250012516, 0.7802083336747528408, 0.7879004041258379498 ) ) ;
#24690 = CARTESIAN_POINT ( 'NONE',  ( 3.703829026103040434, -0.6115302605771840705, 2.015330080423376913 ) ) ;
#24689 = CARTESIAN_POINT ( 'NONE',  ( -8.853638004923878313, 10.28799807962136548, 1.199719254218462483 ) ) ;
#24691 = EDGE_CURVE ( 'NONE', #179842, #145502, #201276, .T. ) ;
#24692 = CARTESIAN_POINT ( 'NONE',  ( 7.796102023057898123, 9.054206100777749455, -1.199719254218441611 ) ) ;
#24694 = CARTESIAN_POINT ( 'NONE',  ( -7.720478407978036195, 11.09464301169468037, -1.199719254218446718 ) ) ;
#24693 = CARTESIAN_POINT ( 'NONE',  ( 5.032011289327418702, 5.899709921417326974, 1.199719254218452935 ) ) ;
#24695 = CARTESIAN_POINT ( 'NONE',  ( 11.41381675112459959, 10.19999999999997087, 3.704697986577257129 ) ) ;
#24696 = CARTESIAN_POINT ( 'NONE',  ( 3.691669705439902138, 1.900360886217996370, -0.6845428438169256502 ) ) ;
#24697 = CARTESIAN_POINT ( 'NONE',  ( 1.364683531249988535, 5.405208333674750953, -0.7879004041258300672 ) ) ;
#24698 = EDGE_CURVE ( 'NONE', #93151, #94599, #210836, .T. ) ;
#24699 = CARTESIAN_POINT ( 'NONE',  ( 7.605760987586388744, 11.81721221891873697, 1.040834085586084257E-14 ) ) ;
#24700 = CARTESIAN_POINT ( 'NONE',  ( 4.516967039858135635, 1.974289957696921949, 0.8805908171375662619 ) ) ;
#24701 = CARTESIAN_POINT ( 'NONE',  ( 7.388267364804250725, 7.584343111885245570, -0.7998128361456341429 ) ) ;
#24702 = CARTESIAN_POINT ( 'NONE',  ( -1.364683531250014514, -0.1989583329919157317, -0.7879004041258359514 ) ) ;
#24704 = CARTESIAN_POINT ( 'NONE',  ( -9.481348452320373710, -9.006862915010128035, 0.5950054837411746789 ) ) ;
#24703 = CARTESIAN_POINT ( 'NONE',  ( 7.015418140428412386, 7.149352350113456822, 0.7998128361456331437 ) ) ;
#24705 = CARTESIAN_POINT ( 'NONE',  ( 9.558135107509954764, 10.25350516829085379, -0.7216878364870257245 ) ) ;
#24707 = CARTESIAN_POINT ( 'NONE',  ( 6.727182134110201162, 7.629137130509070275, 2.410944104600750038 ) ) ;
#24706 = CARTESIAN_POINT ( 'NONE',  ( 1.522189222387077656, 2.139176736804601298, -0.3705008953195278454 ) ) ;
#24709 = CARTESIAN_POINT ( 'NONE',  ( 1.030510548812729965, -1.664561007783531332, 0.7873658874757857307 ) ) ;
#24708 = CARTESIAN_POINT ( 'NONE',  ( -6.426201623197489887, 6.599582769926260362, 0.7216878364870317197 ) ) ;
#24710 = CARTESIAN_POINT ( 'NONE',  ( -1.364683531250012516, 2.530208333674753174, 0.7879004041258379498 ) ) ;
#24711 = CARTESIAN_POINT ( 'NONE',  ( 3.404031855413204966, -0.8899279105200922357, -2.002928011436304612 ) ) ;
#24712 = DIRECTION ( 'NONE',  ( 0.000000000000000000, 0.000000000000000000, 1.000000000000000000 ) ) ;
#24713 = CARTESIAN_POINT ( 'NONE',  ( 4.135799973978175892, -1.557659423114423847, -1.641163307807387950 ) ) ;
#24714 = CARTESIAN_POINT ( 'NONE',  ( -6.693975156845199059, 8.832723654451292816, 1.599625672291283607 ) ) ;
#24715 = CARTESIAN_POINT ( 'NONE',  ( -0.6823417656250212460, 4.613541667008086655, 1.181850606188767472 ) ) ;
#24716 = CARTESIAN_POINT ( 'NONE',  ( 5.910429572389825026, 7.145202977605201511, -1.123150837922413547 ) ) ;
#24717 = VECTOR ( 'NONE', #77353, 1000.000000000000000 ) ;
#24718 = CARTESIAN_POINT ( 'NONE',  ( -1.500000000000008216, 12.74999999999999822, 3.469446951953614189E-15 ) ) ;
#24719 = CARTESIAN_POINT ( 'NONE',  ( 5.234856708652227297, 7.200695141551334721, 1.443375672974065660 ) ) ;
#24720 = CARTESIAN_POINT ( 'NONE',  ( 3.813518172763687986, -1.743905005666521291, 0.3001630661942331080 ) ) ;
#24721 = CARTESIAN_POINT ( 'NONE',  ( 7.771848369131631351, 10.09024240211882351, -1.599625672291262513 ) ) ;
#24722 = CARTESIAN_POINT ( 'NONE',  ( 0.4816451290811329389, 1.964891932219949844, -0.7582931990086133611 ) ) ;
#24724 = CARTESIAN_POINT ( 'NONE',  ( 0.7499999999999902300, 1.233333333333357151, 1.299038105676657340 ) ) ;
#24723 = CARTESIAN_POINT ( 'NONE',  ( -8.012344526598182026E-15, 11.04687500034139980, -1.575800808251669460 ) ) ;
#24725 = CARTESIAN_POINT ( 'NONE',  ( 1.240603756995876772, -1.920774042053990494, -0.4348295819559512831 ) ) ;
#24726 = DIRECTION ( 'NONE',  ( 0.000000000000000000, 1.000000000000000000, 0.000000000000000000 ) ) ;
#24727 = CARTESIAN_POINT ( 'NONE',  ( -9.333041836226904309, 15.44694763438996077, -7.472413793095822321 ) ) ;
#24729 = VERTEX_POINT ( 'NONE', #105454 ) ;
#24728 = CARTESIAN_POINT ( 'NONE',  ( 6.345981700719151242, -1.190820116993321243, -1.365292378351635083 ) ) ;
#24730 = CARTESIAN_POINT ( 'NONE',  ( 6.263503779833467178, 9.290876262238963790, -1.082531754730537088 ) ) ;
#24731 = TOROIDAL_SURFACE ( 'NONE', #204683, 11.92000000000000171, 0.08000000000000000167 ) ;
#24732 = CARTESIAN_POINT ( 'NONE',  ( 8.886479618753304166, 12.45497775759917758, -1.199719254218446718 ) ) ;
#24733 = CARTESIAN_POINT ( 'NONE',  ( 4.416781281874038179, 1.710313510141375115, 0.7581657270378170388 ) ) ;
#24734 = CARTESIAN_POINT ( 'NONE',  ( 4.162516854595432747, 4.815023404238158555, 1.199719254218464037 ) ) ;
#24735 = ORIENTED_EDGE ( 'NONE', *, *, #211914, .F. ) ;
#24736 = CARTESIAN_POINT ( 'NONE',  ( 4.276279003695676373, -1.059865903354087813, -1.778221194881628220 ) ) ;
#24737 = CARTESIAN_POINT ( 'NONE',  ( -1.225000000000010747, 1.500000000000008216, -8.673617379884035472E-15 ) ) ;
#24738 = CARTESIAN_POINT ( 'NONE',  ( -5.926322542504877333, 7.047036066744706950, -1.082531754730549967 ) ) ;
#24739 = FILL_AREA_STYLE_COLOUR ( '', #177964 ) ;
#24740 = CARTESIAN_POINT ( 'NONE',  ( 7.703003830858588863, 12.13858823597705872, -0.7998128361456291469 ) ) ;
#24741 = CARTESIAN_POINT ( 'NONE',  ( -1.510814038188236452, 8.678413394653590629, 2.539834060596353638 ) ) ;
#24742 = CARTESIAN_POINT ( 'NONE',  ( 6.831329296439236032, 9.063246493969506545, -1.599625672291267398 ) ) ;
#24743 = CARTESIAN_POINT ( 'NONE',  ( 4.835665178762361904, 4.878023855840926792, -0.5635330974447970709 ) ) ;
#24744 = CARTESIAN_POINT ( 'NONE',  ( -1.364683531250014514, -0.2614583329919080157, -0.7879004041258359514 ) ) ;
#24745 = CARTESIAN_POINT ( 'NONE',  ( 1.499999999999987121, 0.5041666666666856367, 0.8660254037844524744 ) ) ;
#24746 = CARTESIAN_POINT ( 'NONE',  ( 3.912515228517557286, 0.7039278570535618673, 1.831416474553926310 ) ) ;
#24747 = CARTESIAN_POINT ( 'NONE',  ( 2.407577179044288584, 0.4389615990625857500, 1.967586618684707522 ) ) ;
#24748 = DIRECTION ( 'NONE',  ( 0.000000000000000000, 0.000000000000000000, -1.000000000000000000 ) ) ;
#24749 = DIRECTION ( 'NONE',  ( 1.276756478318932585E-15, -1.000000000000000000, 1.665334536937738262E-16 ) ) ;
#24750 = CARTESIAN_POINT ( 'NONE',  ( -11.92619526248521034, 10.07255386085831894, 1.328859120100916558 ) ) ;
#24751 = CARTESIAN_POINT ( 'NONE',  ( 2.020564968092851021, 1.743606242109306148, 0.6777753874912318954 ) ) ;
#24752 = CARTESIAN_POINT ( 'NONE',  ( -1.364683531250010295, 4.780208333674755394, 0.7879004041258379498 ) ) ;
#24753 = CARTESIAN_POINT ( 'NONE',  ( 3.603774441610514412, 1.461153639754816824, 1.385179026781646394 ) ) ;
#24755 = CARTESIAN_POINT ( 'NONE',  ( 2.794651083563943761, 1.531546425470770245, -1.462076589042210495 ) ) ;
#24754 = CARTESIAN_POINT ( 'NONE',  ( -5.260200412422200600, 8.120355666925794580, -1.082531754730544860 ) ) ;
#24756 = DIRECTION ( 'NONE',  ( 0.000000000000000000, -1.000000000000000000, 0.000000000000000000 ) ) ;
#24757 = CARTESIAN_POINT ( 'NONE',  ( 4.457524453155742528, 1.660904245173303373, 1.235824716467534889 ) ) ;
#24758 = CARTESIAN_POINT ( 'NONE',  ( 7.191674137406095291, 7.354984346587396082, 0.000000000000000000 ) ) ;
#24760 = CARTESIAN_POINT ( 'NONE',  ( 6.620655732516651071, 2.021119449029490589, 2.477762541108457839 ) ) ;
#24759 = CARTESIAN_POINT ( 'NONE',  ( 6.685487044060022477, -0.8959250478542144513, 1.887356362924677233 ) ) ;
#24762 = ORIENTED_EDGE ( 'NONE', *, *, #162536, .T. ) ;
#24761 = CARTESIAN_POINT ( 'NONE',  ( 5.139593076133685656, -1.292025762983131099, -1.289991942498528665 ) ) ;
#24763 = CARTESIAN_POINT ( 'NONE',  ( 8.535021395002688749, 9.916278701380017324, 1.199719254218462483 ) ) ;
#24764 = CARTESIAN_POINT ( 'NONE',  ( -7.664830294503444996, -6.134628647623485698, 7.777967379493320621 ) ) ;
#24765 = CARTESIAN_POINT ( 'NONE',  ( -11.97929049433705551, 13.88000000000000078, 0.7046979865771804130 ) ) ;
#24766 = CARTESIAN_POINT ( 'NONE',  ( -10.32184838934336213, 3.007359993651753438, 7.367400555339857604 ) ) ;
#24767 = CARTESIAN_POINT ( 'NONE',  ( 6.412643469139427843, 10.42524178073059993, -0.7216878364870267237 ) ) ;
#24768 = CARTESIAN_POINT ( 'NONE',  ( 0.6823417656249969321, 11.83854166700806765, -1.181850606188757036 ) ) ;
#24769 = CARTESIAN_POINT ( 'NONE',  ( 5.777967262743825216, 1.883199444611630691, -0.3313529498064629597 ) ) ;
#24770 = CARTESIAN_POINT ( 'NONE',  ( -8.890396042259075315, 11.39521468743417998, -1.599625672291263179 ) ) ;
#24771 = CARTESIAN_POINT ( 'NONE',  ( 5.133733721068893807, 9.141106441222381918, 1.040834085586084257E-14 ) ) ;
#24772 = AXIS2_PLACEMENT_3D ( 'NONE', #154002, #122660, #74882 ) ;
#24773 = CARTESIAN_POINT ( 'NONE',  ( 1.360316468749951602, 2.526041667008118274, 0.7853790794158560518 ) ) ;
#24774 = CARTESIAN_POINT ( 'NONE',  ( 3.348500752450942031, 4.929670182657964084, 1.443375672974066548 ) ) ;
#24775 = DIRECTION ( 'NONE',  ( 1.000000000000000000, 3.451266460341926211E-31, 0.000000000000000000 ) ) ;
#24776 = CARTESIAN_POINT ( 'NONE',  ( 4.955668840994886359, 5.740367388370866131, 1.199719254218462483 ) ) ;
#24777 = ORIENTED_EDGE ( 'NONE', *, *, #9768, .F. ) ;
#24778 = CARTESIAN_POINT ( 'NONE',  ( -5.773793314573309132, 7.829454515125894964, 1.599625672291263179 ) ) ;
#24779 = CARTESIAN_POINT ( 'NONE',  ( 5.501577430365036214, -1.966641501487207622, 0.4445218866586594930 ) ) ;
#24780 = CARTESIAN_POINT ( 'NONE',  ( 0.000000000000000000, -0.02876672507444791305, 0.000000000000000000 ) ) ;
#24781 = CARTESIAN_POINT ( 'NONE',  ( 6.620655732516627090, 7.629137130509076492, 2.426260288887295502 ) ) ;
#24782 = CARTESIAN_POINT ( 'NONE',  ( -0.1405533004718312329, 0.7798934913714054007, -1.807795836271476331 ) ) ;
#24783 = CARTESIAN_POINT ( 'NONE',  ( -3.795919822146277767, 7.372397525905215687, -0.7216878364870267237 ) ) ;
#24784 = CARTESIAN_POINT ( 'NONE',  ( 3.277320446201373638, 4.846626492033466072, 1.599625672291267398 ) ) ;
#24785 = CARTESIAN_POINT ( 'NONE',  ( 2.166797266485945617, 1.462705959888461971, -1.319016900598804831 ) ) ;
#24786 = CARTESIAN_POINT ( 'NONE',  ( 4.921500000981174239, -1.427949280599305482, -1.423951169029838315 ) ) ;
#24787 = CARTESIAN_POINT ( 'NONE',  ( -5.045605722580076780, 9.038290442985410067, -0.7998128361456231517 ) ) ;
#24788 = CARTESIAN_POINT ( 'NONE',  ( 6.727182134110201162, 1.237345558575110083, 2.302850971298702198 ) ) ;
#24789 = CARTESIAN_POINT ( 'NONE',  ( 4.628971764384363752, -2.004251508290517680, 0.8866568735110615940 ) ) ;
#24790 = CARTESIAN_POINT ( 'NONE',  ( 2.836843495735667187, 0.2342426253194809793, 1.912026175940540140 ) ) ;
#24791 = CARTESIAN_POINT ( 'NONE',  ( -9.806625181386236179, 10.33548422123910449, -0.7998128361456291469 ) ) ;
#24792 = CARTESIAN_POINT ( 'NONE',  ( 1.123270288250311610, 3.110197346350006331, 0.7749999999993734123 ) ) ;
#24793 = CARTESIAN_POINT ( 'NONE',  ( 0.2587985324217951244, 0.8487602207661277820, 2.037339956011213093 ) ) ;
#24794 = DIRECTION ( 'NONE',  ( -0.000000000000000000, -0.000000000000000000, -1.000000000000000000 ) ) ;
#24795 = CARTESIAN_POINT ( 'NONE',  ( 5.316205630334249754, 7.295602216847000498, -1.443375672974078316 ) ) ;
#24796 = CARTESIAN_POINT ( 'NONE',  ( 4.150767584078112193, 7.994312614733129152, 0.7998128361456321445 ) ) ;
#24797 = CARTESIAN_POINT ( 'NONE',  ( -6.849430810391480939, -7.996947095390788185, 6.637758778446722907 ) ) ;
#24798 = CARTESIAN_POINT ( 'NONE',  ( 5.451787166470912993, 6.493411461371761284, -1.082531754730548412 ) ) ;
#24799 = ORIENTED_EDGE ( 'NONE', *, *, #81110, .F. ) ;
#24801 = CARTESIAN_POINT ( 'NONE',  ( 2.983067126429808091, -1.860865636787402577, -0.7683904602088088565 ) ) ;
#24800 = CARTESIAN_POINT ( 'NONE',  ( 6.409700764581637067, -0.8744420883355051854, -1.620376909479949390 ) ) ;
#24802 = CARTESIAN_POINT ( 'NONE',  ( 5.272985406448559509, -2.287992931341980896, 0.2183071761258491283 ) ) ;
#24804 = CARTESIAN_POINT ( 'NONE',  ( 2.817075279929776688, -1.616631405580427838, -0.9216590669160623639 ) ) ;
#24803 = CARTESIAN_POINT ( 'NONE',  ( 11.86239285000045740, 11.37999999999998302, 1.812080536912751061 ) ) ;
#24805 = CARTESIAN_POINT ( 'NONE',  ( -3.285556943750000070, -0.4593749995220435256, 0.000000000000000000 ) ) ;
#24806 = CARTESIAN_POINT ( 'NONE',  ( -4.604090349816896577, 8.398638366325423377, -0.2811922690319359486 ) ) ;
#24807 = CARTESIAN_POINT ( 'NONE',  ( 8.917737905728806425, 4.000000000000003553, 8.029567276306217138 ) ) ;
#24808 = CARTESIAN_POINT ( 'NONE',  ( -6.170932472514347289, 10.35117165124207972, 0.000000000000000000 ) ) ;
#24809 = CARTESIAN_POINT ( 'NONE',  ( -5.370438244788932280, 6.398504386076097283, 1.082531754730549078 ) ) ;
#24810 = CARTESIAN_POINT ( 'NONE',  ( 5.864805775728457071, 0.1527762835577218814, -2.085202849681159876 ) ) ;
#24811 = CARTESIAN_POINT ( 'NONE',  ( 5.422898255786183341, 7.349800603215774331, -1.443375672974051449 ) ) ;
#24812 = ORIENTED_EDGE ( 'NONE', *, *, #117742, .F. ) ;
#24813 = EDGE_CURVE ( 'NONE', #57689, #142717, #48371, .T. ) ;
#24814 = CARTESIAN_POINT ( 'NONE',  ( -1.474248253921377483, 7.378028154548616158, 4.279201940598175824 ) ) ;
#24815 = DIRECTION ( 'NONE',  ( 0.000000000000000000, -1.000000000000000000, 0.000000000000000000 ) ) ;
#24816 = CARTESIAN_POINT ( 'NONE',  ( 5.883370885758751001, 1.591107372635025330, -0.6665480857693687478 ) ) ;
#24817 = CARTESIAN_POINT ( 'NONE',  ( -4.252453736180621391, 8.112946458852704268, -0.7998128361456281477 ) ) ;
#24818 = CARTESIAN_POINT ( 'NONE',  ( 1.002125825150332883, -1.692058386710117990, 0.3787823561424672469 ) ) ;
#24819 = CARTESIAN_POINT ( 'NONE',  ( -5.580332384298489323, 14.55306937873557338, 10.58301128396242419 ) ) ;
#24820 = CARTESIAN_POINT ( 'NONE',  ( 7.446209719563365859, -5.223431457505076203, 8.064677165291195493 ) ) ;
#24821 = FILL_AREA_STYLE ('',( #8576 ) ) ;
#24822 = CARTESIAN_POINT ( 'NONE',  ( 5.436453865645980876, -1.212139536413152197, 1.801006579369943239 ) ) ;
#24823 = CARTESIAN_POINT ( 'NONE',  ( 4.547361323050268744, -1.413013347330991598, -1.156083184146582177 ) ) ;
#24824 = CARTESIAN_POINT ( 'NONE',  ( 2.114041031776827673, 1.956853317873577414, -0.1391692324632237410 ) ) ;
#24825 = B_SPLINE_CURVE_WITH_KNOTS ( 'NONE', 3,
 ( #48065, #115232, #133588, #167123, #212646, #118428, #36033 ),
 .UNSPECIFIED., .F., .F.,
 ( 4, 3, 4 ),
 ( 0.000000000000000000, 0.0008000000000005100470, 0.002977368225425562533 ),
 .UNSPECIFIED. ) ;
#24826 = EDGE_CURVE ( 'NONE', #113572, #177076, #179569, .T. ) ;
#24827 = DIRECTION ( 'NONE',  ( 6.314299915563594049E-62, 8.546850786086437571E-32, 1.000000000000000000 ) ) ;
#24828 = CARTESIAN_POINT ( 'NONE',  ( -8.859363311525973117, 12.42334206583395328, -1.199719254218446718 ) ) ;
#24829 = CARTESIAN_POINT ( 'NONE',  ( 6.642605195691581699, 9.837124264027149678, 1.199719254218462483 ) ) ;
#24830 = CARTESIAN_POINT ( 'NONE',  ( 4.090573159264241809, -1.219870178150096462, 1.734285844867427651 ) ) ;
#24831 = CARTESIAN_POINT ( 'NONE',  ( 6.827182134110194589, 2.412578537245218868, 2.569476350730160785 ) ) ;
#24832 = ADVANCED_FACE ( 'NONE', ( #207185 ), #89764, .F. ) ;
#24833 = CARTESIAN_POINT ( 'NONE',  ( -1.500000000000022204, 10.00000000000000178, 4.154462424328226433 ) ) ;
#24834 = CARTESIAN_POINT ( 'NONE',  ( -4.362038794589177648, 7.192753374110822051, -1.033456106840037192 ) ) ;
#24835 = CARTESIAN_POINT ( 'NONE',  ( 1.516557075436252733, 0.8353943144701718726, 1.894387172633307692 ) ) ;
#24837 = CARTESIAN_POINT ( 'NONE',  ( 0.6823417656249864960, -0.7614583329919113464, -1.181850606188749264 ) ) ;
#24836 = CARTESIAN_POINT ( 'NONE',  ( -10.85075961359308216, 3.974415841077576061, 3.932216895623811936 ) ) ;
#24839 = EDGE_LOOP ( 'NONE', ( #3905, #44652, #18092, #198938, #118887, #60968, #157164, #92105, #40960, #162535, #120254, #160899, #4036, #209285, #121765, #135364, #53042, #15205, #212201, #196370 ) ) ;
#24838 = CARTESIAN_POINT ( 'NONE',  ( 3.352378926113183777, 0.9974692666060747115, -1.984802063203878086 ) ) ;
#24840 = CARTESIAN_POINT ( 'NONE',  ( 2.022535828336795127, -2.051039051814534719, 1.038070753253451439 ) ) ;
#24842 = CARTESIAN_POINT ( 'NONE',  ( 0.2858946156298440844, -1.202361161835348025, -1.550730028719159215 ) ) ;
#24841 = CARTESIAN_POINT ( 'NONE',  ( 10.41229878561526512, 11.25002945941372623, -0.7216878364870257245 ) ) ;
#24844 = CARTESIAN_POINT ( 'NONE',  ( 3.475000000000000533, -0.8458333333333335480, -2.006292185433951047 ) ) ;
#24843 = CARTESIAN_POINT ( 'NONE',  ( 4.848976215542928792, 5.686169002002086970, 1.199719254218452047 ) ) ;
#24845 = CARTESIAN_POINT ( 'NONE',  ( 0.000000000000000000, 5.499999999999998224, 0.000000000000000000 ) ) ;
#24846 = CARTESIAN_POINT ( 'NONE',  ( 6.409700764581637067, -0.8744420883355051854, -1.620376909479949390 ) ) ;
#24847 = CARTESIAN_POINT ( 'NONE',  ( -5.689683820183289775, 6.135727912364857595, -0.7597814889456652176 ) ) ;
#24848 = CARTESIAN_POINT ( 'NONE',  ( 2.696000938853719830, -1.719994558248700844, -0.1292177092697097962 ) ) ;
#24849 = CARTESIAN_POINT ( 'NONE',  ( 1.973842561262352469, -0.8578407463649927456, 1.825077436249371354 ) ) ;
#24850 = CARTESIAN_POINT ( 'NONE',  ( 2.743178873131403961, 2.287300171779807378, -0.2288005476599272447 ) ) ;
#24851 = CARTESIAN_POINT ( 'NONE',  ( 3.339431287149054572, -1.996970876468142864, 1.063245685667679519 ) ) ;
#24852 = CARTESIAN_POINT ( 'NONE',  ( 5.268238656634978589, 1.036954370284940419, 1.833022835974008613 ) ) ;
#24853 = CARTESIAN_POINT ( 'NONE',  ( -7.431277594066160397, 7.842447745931541370, -0.7216878364870338292 ) ) ;
#24854 = CARTESIAN_POINT ( 'NONE',  ( 3.092752268530512438, 1.519777622694931773, -0.9064811718217934411 ) ) ;
#24856 = CARTESIAN_POINT ( 'NONE',  ( 6.392113680008942644, -0.6066422732131382389, -2.210563551359717938 ) ) ;
#24855 = CARTESIAN_POINT ( 'NONE',  ( 3.512971199272317602, 6.152197928242737923, -1.082531754730549967 ) ) ;
#24857 = CARTESIAN_POINT ( 'NONE',  ( 5.613187951484799321, -1.795345830453990654, 0.4073638586896133340 ) ) ;
#24858 = CARTESIAN_POINT ( 'NONE',  ( -2.839543107058306592, 5.400218493954923815, -1.199719254218446718 ) ) ;
#24859 = CARTESIAN_POINT ( 'NONE',  ( 0.7499999999999885647, 3.066666666666689522, -1.299038105676658228 ) ) ;
#24860 = AXIS2_PLACEMENT_3D ( 'NONE', #182044, #32614, #152764 ) ;
#24861 = CARTESIAN_POINT ( 'NONE',  ( 5.437503290160631941, 0.8905978969957989433, -2.002497223260243153 ) ) ;
#24862 = CARTESIAN_POINT ( 'NONE',  ( -3.327636637150278798, 5.969660945728899826, -1.199719254218452935 ) ) ;
#24863 = LINE ( 'NONE', #72546, #184406 ) ;
#24864 = CARTESIAN_POINT ( 'NONE',  ( 5.529760519541640384, 1.996289034380031913, -0.5486624943154896350 ) ) ;
#24865 = CARTESIAN_POINT ( 'NONE',  ( 0.5851731681005939434, 1.651346252830317551, 1.157095189655330314 ) ) ;
#24866 = CARTESIAN_POINT ( 'NONE',  ( -1.500000000000001332, -1.068749999317178290, 0.000000000000000000 ) ) ;
#24867 = CARTESIAN_POINT ( 'NONE',  ( 4.582597182753257670, -1.869065293654921023, -0.4664472792492486697 ) ) ;
#24868 = CARTESIAN_POINT ( 'NONE',  ( -1.364683531250000748, 10.85937500034139802, 0.000000000000000000 ) ) ;
#24869 = CARTESIAN_POINT ( 'NONE',  ( -4.121315508874280553, 3.910548969882488901, -0.7216878364870207285 ) ) ;
#24870 = CARTESIAN_POINT ( 'NONE',  ( 6.293239850429793947, -0.1054838202379469042, -2.118119863012501991 ) ) ;
#24872 = ORIENTED_EDGE ( 'NONE', *, *, #12835, .F. ) ;
#24871 = DIRECTION ( 'NONE',  ( 0.000000000000000000, 0.000000000000000000, -1.000000000000000000 ) ) ;
#24873 = CARTESIAN_POINT ( 'NONE',  ( -4.882344714696960075, 5.829061934302122161, 1.082531754730549078 ) ) ;
#24874 = CARTESIAN_POINT ( 'NONE',  ( 2.354312230267378236, 5.898448035287240820, -0.7998128361456281477 ) ) ;
#24875 = FILL_AREA_STYLE ('',( #9698 ) ) ;
#24876 = LINE ( 'NONE', #58461, #149401 ) ;
#24877 = CARTESIAN_POINT ( 'NONE',  ( -1.499999999999993339, 10.64264068711930733, 1.232676135170975238E-14 ) ) ;
#24878 = CARTESIAN_POINT ( 'NONE',  ( 10.07334494482924292, 11.81495252613139257, -1.082531754730537088 ) ) ;
#24879 = CARTESIAN_POINT ( 'NONE',  ( 0.8890225878602634468, 0.1407106197201784259, 1.956863499422318631 ) ) ;
#24880 = CARTESIAN_POINT ( 'NONE',  ( 1.364683531249986537, 0.6760416670080884316, 0.7879004041258500513 ) ) ;
#24881 = PLANE ( 'NONE',  #54202 ) ;
#24882 = CARTESIAN_POINT ( 'NONE',  ( 5.230891786122516152, -1.846674803186045821, -0.6626716404555529349 ) ) ;
#24883 = CARTESIAN_POINT ( 'NONE',  ( -6.984421689334302741, 11.30024240419870374, 0.000000000000000000 ) ) ;
#24884 = CARTESIAN_POINT ( 'NONE',  ( -5.707619481228832115, 6.721606151930833661, -1.082531754730543971 ) ) ;
#24885 = CARTESIAN_POINT ( 'NONE',  ( 6.526263005029544928, 1.249015235541932167, -1.764162671312206498 ) ) ;
#24887 = ORIENTED_EDGE ( 'NONE', *, *, #107493, .T. ) ;
#24886 = CARTESIAN_POINT ( 'NONE',  ( -7.217017841176048165, 7.314275657660511243, 1.040834085586084257E-14 ) ) ;
#24888 = CARTESIAN_POINT ( 'NONE',  ( 1.364683531249988535, 5.155208333674749177, -0.7879004041258300672 ) ) ;
#24889 = CARTESIAN_POINT ( 'NONE',  ( 1.721729502718066795, -1.034818790731323990, -1.558030248997283040 ) ) ;
#24890 = CARTESIAN_POINT ( 'NONE',  ( 0.4219819185556292207, -1.224561070735529444, -1.228170329033271724 ) ) ;
#24892 = CARTESIAN_POINT ( 'NONE',  ( 3.790727848299980440, 1.850687065220711469, -1.173560875862532660 ) ) ;
#24891 = CARTESIAN_POINT ( 'NONE',  ( -4.957638175832625493E-14, 2.078125000341435769, -1.570758158831802254 ) ) ;
#24893 = CARTESIAN_POINT ( 'NONE',  ( 4.471882758057180496, 2.239461445850467580, -0.5561450820626266944 ) ) ;
#24894 = CARTESIAN_POINT ( 'NONE',  ( 0.4443025167278572551, 2.055347410954794451, 0.1520637142833832778 ) ) ;
#24895 = CARTESIAN_POINT ( 'NONE',  ( 2.290873232013816541, 1.501373485850267198, 1.231690586011934041 ) ) ;
#24896 = CARTESIAN_POINT ( 'NONE',  ( -5.544921637864833386, 7.492161215640853023, -1.443375672974051449 ) ) ;
#24897 =( NAMED_UNIT ( * ) SI_UNIT ( $, .STERADIAN. ) SOLID_ANGLE_UNIT ( ) );
#24898 = EDGE_CURVE ( 'NONE', #210539, #197889, #154889, .T. ) ;
#24899 = CARTESIAN_POINT ( 'NONE',  ( 5.449516625918088053, -1.916229881892789866, 0.9086369058012438993 ) ) ;
#24900 = DIRECTION ( 'NONE',  ( 0.000000000000000000, 0.000000000000000000, -1.000000000000000000 ) ) ;
#24901 = CARTESIAN_POINT ( 'NONE',  ( 3.797500137148449362, 1.423962148579031917, -1.427936706820939872 ) ) ;
#24902 = CARTESIAN_POINT ( 'NONE',  ( -3.904385050611244079, 7.498940292447679568, 1.040834085586084257E-14 ) ) ;
#24903 = CARTESIAN_POINT ( 'NONE',  ( -7.065734331377342414, 8.272386803808890576, -1.199719254218452047 ) ) ;
#24904 = CARTESIAN_POINT ( 'NONE',  ( 8.211434591371064684, 12.73175745657494851, -0.7998128361456352531 ) ) ;
#24905 = CARTESIAN_POINT ( 'NONE',  ( 1.435882461153328515, 0.9014729512111450127, -1.587519582607027635 ) ) ;
#24906 = CARTESIAN_POINT ( 'NONE',  ( -5.098748287191073203, 8.106234214101666780, 1.199719254218452935 ) ) ;
#24907 = CARTESIAN_POINT ( 'NONE',  ( -5.064290697676250730, 7.960144884870772763, -1.236948567437242907 ) ) ;
#24908 = CARTESIAN_POINT ( 'NONE',  ( -11.19490907666120272, 4.805655862119510680, 5.952061394947645745 ) ) ;
#24909 = EDGE_LOOP ( 'NONE', ( #19159, #136035, #181034, #152695 ) ) ;
#24910 = CARTESIAN_POINT ( 'NONE',  ( 5.489158015974754612, 1.818697853212094095, -0.9693054586683967910 ) ) ;
#24912 = MANIFOLD_SOLID_BREP ( 'Sweep1[9]', #108812 ) ;
#24911 = CARTESIAN_POINT ( 'NONE',  ( -7.065207446052813367, 8.375735120883982532, -1.082531754730549967 ) ) ;
#24913 = UNCERTAINTY_MEASURE_WITH_UNIT (LENGTH_MEASURE( 1.000000000000000082E-05 ), #170060, 'distance_accuracy_value', 'NONE');
#24914 = CARTESIAN_POINT ( 'NONE',  ( -0.4019237886466966447, 11.83258545099816317, 1.500000000000003997 ) ) ;
#24915 = CARTESIAN_POINT ( 'NONE',  ( -3.253066792275140173, 5.882662793374543675, 1.199719254218462483 ) ) ;
#24916 = CARTESIAN_POINT ( 'NONE',  ( -4.285806009943333272, 7.464806705703632694, 1.099619435331932404 ) ) ;
#24917 = CARTESIAN_POINT ( 'NONE',  ( 4.547524150180999314, -1.845711718722802486, 0.8204608018674663938 ) ) ;
#24918 = CARTESIAN_POINT ( 'NONE',  ( 5.162811894357514753, 0.6434298260243781487, 2.126049117748362249 ) ) ;
#24920 = CARTESIAN_POINT ( 'NONE',  ( 7.605760987586388744, 11.81721221891873697, 1.040834085586084257E-14 ) ) ;
#24919 = CARTESIAN_POINT ( 'NONE',  ( -5.002032328799064231, 4.800402236545811441, -0.7998128361456362523 ) ) ;
#24921 = CARTESIAN_POINT ( 'NONE',  ( 6.144869935491714230, 8.192100896205568361, -1.599625672291262513 ) ) ;
#24922 = CARTESIAN_POINT ( 'NONE',  ( 3.995036845513312951, 1.742007986889832161, -1.100897373992800299 ) ) ;
#24923 = CARTESIAN_POINT ( 'NONE',  ( 4.360000113718985659, -0.002809843368253156070, -2.016597020062675050 ) ) ;
#24924 = ORIENTED_EDGE ( 'NONE', *, *, #17272, .T. ) ;
#24925 = EDGE_CURVE ( 'NONE', #71638, #155393, #33257, .T. ) ;
#24926 =( NAMED_UNIT ( * ) SI_UNIT ( $, .STERADIAN. ) SOLID_ANGLE_UNIT ( ) );
#24927 = CARTESIAN_POINT ( 'NONE',  ( 5.040934186182656873, 4.775511393501539636, 1.040834085586084257E-14 ) ) ;
#24928 = COLOUR_RGB ( '', 0.40784314, 0.44705882, 0.49803922) ;
#24930 = VERTEX_POINT ( 'NONE', #200243 ) ;
#24929 = CARTESIAN_POINT ( 'NONE',  ( -5.420227550413282636, 9.545625585449309725, 0.7998128361456291469 ) ) ;
#24931 = CARTESIAN_POINT ( 'NONE',  ( 5.559975706299111309, 7.414571502401146930, -1.245397951563255834 ) ) ;
#24932 = CARTESIAN_POINT ( 'NONE',  ( 3.532577226125938274, 1.967586357134976094, -0.4389627639644277934 ) ) ;
#24933 = CARTESIAN_POINT ( 'NONE',  ( 2.853255899669316697, 1.832232481769331844, -0.1808706098178694266 ) ) ;
#24934 = AXIS2_PLACEMENT_3D ( 'NONE', #135653, #43504, #58661 ) ;
#24935 = CARTESIAN_POINT ( 'NONE',  ( 0.8566255916394946990, 2.304767657353411270, -0.1186049529825431298 ) ) ;
#24936 = CARTESIAN_POINT ( 'NONE',  ( 3.074666975249065626, 6.809138247757705820, 0.000000000000000000 ) ) ;
#24937 = CARTESIAN_POINT ( 'NONE',  ( 3.479894426560462328, 1.368377867093536482, 1.673357603396708360 ) ) ;
#24938 = CARTESIAN_POINT ( 'NONE',  ( -7.386494761346872551, 7.511998731193139989, -0.7998128361456291469 ) ) ;
#24939 = CARTESIAN_POINT ( 'NONE',  ( 3.480086682454126557, 2.076208366568982555, 0.9861560518420305899 ) ) ;
#24940 = EDGE_LOOP ( 'NONE', ( #104737, #27394, #55937, #69684 ) ) ;
#24941 = CARTESIAN_POINT ( 'NONE',  ( 0.000000000000000000, -6.527411821100059797, 0.000000000000000000 ) ) ;
#24942 = CARTESIAN_POINT ( 'NONE',  ( 2.447944060942487621, 1.870205405844455049, 0.04815357881200743595 ) ) ;
#24943 = CARTESIAN_POINT ( 'NONE',  ( 5.946159419501746868, 1.969187058922382993, 0.09738397392708775246 ) ) ;
#24945 = CARTESIAN_POINT ( 'NONE',  ( 9.259855728009286580, 10.86588177317476855, -1.082531754730543083 ) ) ;
#24944 = CARTESIAN_POINT ( 'NONE',  ( -0.6823417656250212460, 4.051041667008085767, 1.181850606188767472 ) ) ;
#24947 = CARTESIAN_POINT ( 'NONE',  ( 0.4345545588612038657, 1.130843733186673639, -1.894998796914903139 ) ) ;
#24946 = CARTESIAN_POINT ( 'NONE',  ( -6.735703387890906946, 6.752742128827836865, -0.7998128361456291469 ) ) ;
#24948 = B_SPLINE_CURVE_WITH_KNOTS ( 'NONE', 3,
 ( #181619, #66776, #80939, #165381, #178455, #50568, #46326, #30064 ),
 .UNSPECIFIED., .F., .F.,
 ( 4, 2, 2, 4 ),
 ( 0.000000000000000000, 0.0006693095108161682119, 0.001003964266224251396, 0.001338619021632334689 ),
 .UNSPECIFIED. ) ;
#24949 = ADVANCED_FACE ( 'NONE', ( #187209 ), #71304, .F. ) ;
#24950 = CARTESIAN_POINT ( 'NONE',  ( -1.500000000000057288, 7.438721522839117029, -4.195160983902607832 ) ) ;
#24951 = CARTESIAN_POINT ( 'NONE',  ( 5.867981556616276073, 5.740399992340775803, -0.7998128361456281477 ) ) ;
#24952 = CARTESIAN_POINT ( 'NONE',  ( -4.791917227426195858, 7.677988301050826969, -1.199719254218452047 ) ) ;
#24953 = CARTESIAN_POINT ( 'NONE',  ( 11.86145016429273191, 13.40000000000000036, 1.099999999999996980 ) ) ;
#24954 = CARTESIAN_POINT ( 'NONE',  ( 6.631714602856194851, -1.287423518921044341, -1.493153376739835947 ) ) ;
#24955 = CARTESIAN_POINT ( 'NONE',  ( 5.602268381685036935, -2.307868969066428022, -0.005371834822459965395 ) ) ;
#24956 = CARTESIAN_POINT ( 'NONE',  ( 0.1331565106231328843, 0.003911343561965873426, -1.946049565259087455 ) ) ;
#24957 = EDGE_CURVE ( 'NONE', #205506, #104139, #169891, .T. ) ;
#24958 = CARTESIAN_POINT ( 'NONE',  ( 2.940340207046471921, -1.064325496585982078, 1.766646112275678693 ) ) ;
#24959 = CARTESIAN_POINT ( 'NONE',  ( 5.666945020832160118, 9.555260257705446847, 0.7216878364870438212 ) ) ;
#24960 = CARTESIAN_POINT ( 'NONE',  ( 3.410758162289653672, 6.136912401716668519, -1.199719254218453823 ) ) ;
#24961 = CARTESIAN_POINT ( 'NONE',  ( 7.768458830506048685, 8.165549511786275971, -0.7216878364870267237 ) ) ;
#24962 = CARTESIAN_POINT ( 'NONE',  ( 1.364683531249988535, 3.467708333674749621, -0.7879004041258239610 ) ) ;
#24963 = CARTESIAN_POINT ( 'NONE',  ( -5.940857138655644576, 14.48120657956202351, 10.43616353783158957 ) ) ;
#24964 = CARTESIAN_POINT ( 'NONE',  ( 6.439759776366775768, 7.575769829591800786, 1.082531754730558626 ) ) ;
#24965 = CARTESIAN_POINT ( 'NONE',  ( 5.635278836315742446, -0.04772081403418790974, -2.170810874590335171 ) ) ;
#24967 = CARTESIAN_POINT ( 'NONE',  ( 5.724118993814841794, 1.776208094789998304, 0.4848738846057951135 ) ) ;
#24966 = CARTESIAN_POINT ( 'NONE',  ( -4.121315508874280553, 3.910548969882488901, -0.7216878364870207285 ) ) ;
#24969 = CARTESIAN_POINT ( 'NONE',  ( 6.720655732516646275, 4.698042323276835575, 2.488944259588221186 ) ) ;
#24968 = CARTESIAN_POINT ( 'NONE',  ( 0.6823417656249899377, 5.426041667008087543, -1.181850606188754593 ) ) ;
#24970 = DIRECTION ( 'NONE',  ( 0.9982742078614211811, 0.000000000000000000, -0.05872483221476467591 ) ) ;
#24971 = CARTESIAN_POINT ( 'NONE',  ( -0.3000000000000157541, 3.214163249644056197, -0.5238375172406551927 ) ) ;
#24972 = CARTESIAN_POINT ( 'NONE',  ( 6.702048742255109381, -2.262191126150433274, 0.04724482429044154358 ) ) ;
#24973 = CARTESIAN_POINT ( 'NONE',  ( -4.002466101043451019, 7.812316210466456745, 0.3644823170804913914 ) ) ;
#24974 = DIRECTION ( 'NONE',  ( 0.000000000000000000, 8.546850786086437571E-32, 1.000000000000000000 ) ) ;
#24975 = CARTESIAN_POINT ( 'NONE',  ( 6.582202237817778467, 6.781708767774706104, 0.2773405359152263383 ) ) ;
#24976 = CARTESIAN_POINT ( 'NONE',  ( -5.790741006368224753, 5.928488393617260321, 0.7216878364870257245 ) ) ;
#24977 = CARTESIAN_POINT ( 'NONE',  ( 0.1176276963383571517, -0.5100272734060510293, 1.842954807014775653 ) ) ;
#24978 = CARTESIAN_POINT ( 'NONE',  ( 2.201683042903946230, -1.769559083619182349, 0.04015057502057895605 ) ) ;
#24979 = CARTESIAN_POINT ( 'NONE',  ( 5.936195100277483760, -1.120233448768311435, -1.672418650214458014 ) ) ;
#24980 = CARTESIAN_POINT ( 'NONE',  ( 4.547870462380197765, 7.393267075163835855, 1.199719254218462483 ) ) ;
#24981 = CARTESIAN_POINT ( 'NONE',  ( 4.946364073002400552, 2.100128792357182750, 0.1576013620808654481 ) ) ;
#24983 = CARTESIAN_POINT ( 'NONE',  ( 3.163600654563469838, 1.217692022474494262, 1.478743580268084390 ) ) ;
#24982 = CARTESIAN_POINT ( 'NONE',  ( -2.589244150085650009, 5.964609241834465614, 0.7216878364870317197 ) ) ;
#24984 = CARTESIAN_POINT ( 'NONE',  ( 0.1236583036082015280, 1.000000000000000888, -11.99936284241577233 ) ) ;
#24985 = CARTESIAN_POINT ( 'NONE',  ( 3.807052887859848855, -1.611515334864065840, 1.132039114057415308 ) ) ;
#24986 = CARTESIAN_POINT ( 'NONE',  ( 6.416272379866970965, -2.019260422740985828, 0.05364450914858465147 ) ) ;
#24987 = CARTESIAN_POINT ( 'NONE',  ( -4.620631424159025613, 4.285158171140619032, -0.7998128361456221525 ) ) ;
#24988 = CARTESIAN_POINT ( 'NONE',  ( 3.168673215318769110, -1.727878594304608217, -0.7172629358194044791 ) ) ;
#24990 = VERTEX_POINT ( 'NONE', #20432 ) ;
#24989 = CARTESIAN_POINT ( 'NONE',  ( 5.268053373232242542, 0.8548693298336268453, 1.498049451945895116 ) ) ;
#24992 = CARTESIAN_POINT ( 'NONE',  ( 5.666945020832181434, 5.713783400500082266, 0.7216878364870317197 ) ) ;
#24991 = CARTESIAN_POINT ( 'NONE',  ( 2.702037527177497012, -0.6914408288211832954, 2.095836555436859872 ) ) ;
#24993 = CARTESIAN_POINT ( 'NONE',  ( -1.364683531250012516, 3.551041667008086211, -0.7879004041258300672 ) ) ;
#24994 = CARTESIAN_POINT ( 'NONE',  ( 0.1860857499333635756, -1.268064657576525978, -1.627672589050175089 ) ) ;
#24995 = CARTESIAN_POINT ( 'NONE',  ( 6.564118927310645724, 10.80988918183778225, -0.7998128361456291469 ) ) ;
#24996 = CARTESIAN_POINT ( 'NONE',  ( -9.480175724453545172, 12.08329098332774265, 1.599625672291281386 ) ) ;
#24997 = CARTESIAN_POINT ( 'NONE',  ( 1.519470924986870308, 8.761764328395914347, 2.483655442635868571 ) ) ;
#24998 = CARTESIAN_POINT ( 'NONE',  ( -4.874319919312905647, 5.645460313075203018, -1.199719254218446718 ) ) ;
#24999 = STYLED_ITEM ( 'NONE', ( #113199 ), #76119 ) ;
#25000 = AXIS2_PLACEMENT_3D ( 'NONE', #1305, #30653, #194198 ) ;
#25001 = ORIENTED_EDGE ( 'NONE', *, *, #155697, .T. ) ;
#25002 = CARTESIAN_POINT ( 'NONE',  ( 2.207561477879273593, -1.661462528888792090, -1.235070534849058266 ) ) ;
#25003 = CARTESIAN_POINT ( 'NONE',  ( -1.499999999999997780, 2.900000000000020783, 1.214306433183764966E-14 ) ) ;
#25004 = CARTESIAN_POINT ( 'NONE',  ( 7.149227073107712549, 7.235186428247455837, -0.7998128361456281477 ) ) ;
#25005 = CARTESIAN_POINT ( 'NONE',  ( 4.686278372178935392, 5.496354851410763409, 1.199719254218452047 ) ) ;
#25006 = CARTESIAN_POINT ( 'NONE',  ( 6.358074577831472673, 0.8120454629646983724, -1.959034198684066697 ) ) ;
#25007 = CARTESIAN_POINT ( 'NONE',  ( 0.4330238300980764898, -6.527411821100045586, 9.549638505170038982 ) ) ;
#25008 = CARTESIAN_POINT ( 'NONE',  ( 1.364683531249990311, 3.634375000341416584, 1.214306433183764966E-14 ) ) ;
#25009 = ORIENTED_EDGE ( 'NONE', *, *, #171577, .F. ) ;
#25010 = CARTESIAN_POINT ( 'NONE',  ( 9.734391104931951588, 11.41950637958454706, 1.082531754730548412 ) ) ;
#25011 = CARTESIAN_POINT ( 'NONE',  ( 5.835314490094169138, -1.281163661392352493, 1.556671411349755285 ) ) ;
#25012 = CARTESIAN_POINT ( 'NONE',  ( 5.296063324668989658, -0.8673027158061608066, -1.708257925969633551 ) ) ;
#25013 = CARTESIAN_POINT ( 'NONE',  ( 0.000000000000000000, -4.000000000000003553, 6.200000000000000178 ) ) ;
#25014 = CARTESIAN_POINT ( 'NONE',  ( 2.630644284709309666, 0.2711686948545319886, 2.174668582101045633 ) ) ;
#25015 = CARTESIAN_POINT ( 'NONE',  ( -0.7500000000000006661, 2.389583334016155636, -1.299038105676652011 ) ) ;
#25016 = CARTESIAN_POINT ( 'NONE',  ( 1.916128293556786044, -1.911906470838855343, 0.05044092668918254141 ) ) ;
#25017 = CARTESIAN_POINT ( 'NONE',  ( -5.096975683733680818, 8.033889833409558534, -1.199719254218452047 ) ) ;
#25018 = EDGE_CURVE ( 'NONE', #128202, #134989, #96774, .T. ) ;
#25020 = CARTESIAN_POINT ( 'NONE',  ( 6.380470236391142080, -0.5646626916907444560, -2.040458243955853401 ) ) ;
#25019 = CARTESIAN_POINT ( 'NONE',  ( 3.588273936444265289, 7.344317902764286643, -0.3372145678562175064 ) ) ;
#25021 = CARTESIAN_POINT ( 'NONE',  ( -1.364683531250000748, 9.921875000341398021, 0.000000000000000000 ) ) ;
#25023 = CARTESIAN_POINT ( 'NONE',  ( -6.740338644649361832, 7.892758502626242567, -1.199719254218452047 ) ) ;
#25022 = CARTESIAN_POINT ( 'NONE',  ( 3.597287555019304861, -0.6049611382589085151, 2.001324503170316849 ) ) ;
#25025 = ORIENTED_EDGE ( 'NONE', *, *, #68075, .F. ) ;
#25024 = CARTESIAN_POINT ( 'NONE',  ( 2.942113945249478668, 1.711507881387188013, 0.2129122850730424121 ) ) ;
#25026 = CARTESIAN_POINT ( 'NONE',  ( 4.408728476930470165E-16, -0.5000000000000004441, -3.599999999999999201 ) ) ;
#25027 = CARTESIAN_POINT ( 'NONE',  ( 7.135668919494039031, 7.219368582364847242, 1.040834085586084257E-14 ) ) ;
#25028 = STYLED_ITEM ( 'NONE', ( #212408 ), #175193 ) ;
#25029 = DIRECTION ( 'NONE',  ( -0.000000000000000000, 1.000000000000000000, -0.000000000000000000 ) ) ;
#25030 = CARTESIAN_POINT ( 'NONE',  ( -1.040834085586084257E-14, 13.49999999999999822, 1.240450515248290753 ) ) ;
#25031 = CARTESIAN_POINT ( 'NONE',  ( 11.45846087878779329, 10.00688399218553570, -3.566076377698155664 ) ) ;
#25032 = CARTESIAN_POINT ( 'NONE',  ( 6.179819089730593795, 6.104210447640811665, 1.040834085586084257E-14 ) ) ;
#25033 = LINE ( 'NONE', #5553, #206451 ) ;
#25034 = VERTEX_POINT ( 'NONE', #34558 ) ;
#25035 = CARTESIAN_POINT ( 'NONE',  ( -3.380278471875000523, -0.05468749976102194044, 0.000000000000000000 ) ) ;
#25036 = VERTEX_POINT ( 'NONE', #184005 ) ;
#25037 = CARTESIAN_POINT ( 'NONE',  ( 2.859786144356114779, 0.6500800702718724233, -1.690994707955698617 ) ) ;
#25038 = ORIENTED_EDGE ( 'NONE', *, *, #101745, .T. ) ;
#25039 = CARTESIAN_POINT ( 'NONE',  ( 8.703444544968814256, 12.24143683818393313, -1.199719254218446718 ) ) ;
#25040 = CARTESIAN_POINT ( 'NONE',  ( 3.739016502318667445, 7.584212696005614873, 0.7998128361456271485 ) ) ;
#25041 = CARTESIAN_POINT ( 'NONE',  ( 4.090334381980924583, -1.039670344891037601, 1.483205724144847748 ) ) ;
#25042 = CARTESIAN_POINT ( 'NONE',  ( -6.760415694342130179E-18, -5.633679745285109895E-18, -0.4330127018938150774 ) ) ;
#25043 =( NAMED_UNIT ( * ) PLANE_ANGLE_UNIT ( ) SI_UNIT ( $, .RADIAN. ) );
#25044 = CARTESIAN_POINT ( 'NONE',  ( 5.744750223003346257, 6.067414509003485001, 0.6312745094601609486 ) ) ;
#25045 = ORIENTED_EDGE ( 'NONE', *, *, #97858, .F. ) ;
#25047 = CARTESIAN_POINT ( 'NONE',  ( -1.364683531250014514, 14.33854166700806232, -0.7879004041258335089 ) ) ;
#25046 = CARTESIAN_POINT ( 'NONE',  ( 4.668306603206507255, -0.7948602423475581435, -1.682893250223691517 ) ) ;
#25048 = CARTESIAN_POINT ( 'NONE',  ( 1.599098272587581748, -0.2325377738172547115, 1.901345697680896007 ) ) ;
#25049 = CARTESIAN_POINT ( 'NONE',  ( 1.447985623159939284, 1.823312892812560593, 0.09356915273009414058 ) ) ;
#25050 = CARTESIAN_POINT ( 'NONE',  ( 4.733245298435761583, 8.205245971696047746, 0.7015191473903161778 ) ) ;
#25051 = CARTESIAN_POINT ( 'NONE',  ( -0.1036471877147697312, 3.479999999999997318, 1.999999999999997780 ) ) ;
#25052 = CARTESIAN_POINT ( 'NONE',  ( 5.264264421420239870, 7.666326994050936428, 1.218248458220503094 ) ) ;
#25053 = CARTESIAN_POINT ( 'NONE',  ( -1.115562610750309283E-14, 8.562500000000000000, 1.500000000000001554 ) ) ;
#25054 = CARTESIAN_POINT ( 'NONE',  ( -1.445377862185231344, 8.715816065047343741, -2.588769565374613002 ) ) ;
#25055 = CARTESIAN_POINT ( 'NONE',  ( 6.925078400183550364, -0.007619068086212391067, 2.144148427808051594 ) ) ;
#25056 = CARTESIAN_POINT ( 'NONE',  ( 7.131225611108088280, 9.342849184424693476, 1.443375672974076540 ) ) ;
#25057 = CARTESIAN_POINT ( 'NONE',  ( 6.086760365903021608, 1.896989206666617633, 0.5289026096024685986 ) ) ;
#25058 = CARTESIAN_POINT ( 'NONE',  ( -3.741160322367112379, 6.452105245148518797, 1.199719254218464037 ) ) ;
#25059 = DIRECTION ( 'NONE',  ( 0.8164965809277251463, 0.000000000000000000, 0.5773502691896270633 ) ) ;
#25060 = CARTESIAN_POINT ( 'NONE',  ( 1.570382428225084226, -1.985578813138744403, -0.6546124938694962703 ) ) ;
#25061 = CARTESIAN_POINT ( 'NONE',  ( 0.2350025537052654601, -1.671451849548213797, 0.7345932495873632728 ) ) ;
#25062 = CARTESIAN_POINT ( 'NONE',  ( -7.054319997812058318, 7.124461507069184130, 1.040834085586084257E-14 ) ) ;
#25063 = CARTESIAN_POINT ( 'NONE',  ( 1.412830140145465263, 1.608106816955911178, 0.8641515426408912237 ) ) ;
#25064 = CARTESIAN_POINT ( 'NONE',  ( 2.860232119962682784, 2.196193069775736362, -0.2169517147150926140 ) ) ;
#25065 = CARTESIAN_POINT ( 'NONE',  ( 1.441514601552947417, -1.799640695080907182, 0.6472408003148700795 ) ) ;
#25066 = ORIENTED_EDGE ( 'NONE', *, *, #77767, .T. ) ;
#25067 = CARTESIAN_POINT ( 'NONE',  ( 1.504289420374326447, 1.967163215448018088, 0.09980459116839916767 ) ) ;
#25068 = CARTESIAN_POINT ( 'NONE',  ( 2.770961567126817737, 1.843342918492569149, -0.6114499264749191365 ) ) ;
#25069 = EDGE_LOOP ( 'NONE', ( #86281, #156172, #1583, #58580 ) ) ;
#25070 = CARTESIAN_POINT ( 'NONE',  ( -9.579603127937250662, -9.900000000000005684, 0.08720040834116031536 ) ) ;
#25072 = CARTESIAN_POINT ( 'NONE',  ( 6.877813048773076865, -1.805165420234026818, 0.4518952398848713470 ) ) ;
#25071 = CARTESIAN_POINT ( 'NONE',  ( -5.438755897737433287, 6.374245297895642537, -1.199719254218453823 ) ) ;
#25073 = CARTESIAN_POINT ( 'NONE',  ( 5.598591087800349086, 5.496387455380669529, -0.7998128361456481317 ) ) ;
#25074 = CARTESIAN_POINT ( 'NONE',  ( 10.58621901417202515, 11.24501035948919991, -0.7998128361456281477 ) ) ;
#25075 = CARTESIAN_POINT ( 'NONE',  ( -6.947627372360122955, 7.070263120700404968, 0.000000000000000000 ) ) ;
#25076 = CARTESIAN_POINT ( 'NONE',  ( 2.261505105119133052, 2.148611799745976381, -0.4309092228176118478 ) ) ;
#25077 = FACE_OUTER_BOUND ( 'NONE', #40861, .T. ) ;
#25078 = CARTESIAN_POINT ( 'NONE',  ( -10.56511880488638333, 12.34113476418481170, -3.405056808716381944 ) ) ;
#25079 = CARTESIAN_POINT ( 'NONE',  ( 2.894927146036041510, 1.565677646668685696, -0.9388022922067614795 ) ) ;
#25080 = CARTESIAN_POINT ( 'NONE',  ( -3.277320446201389181, 4.846626492033466072, 1.599625672291267398 ) ) ;
#25081 = AXIS2_PLACEMENT_3D ( 'NONE', #98723, #108, #128114 ) ;
#25082 = CARTESIAN_POINT ( 'NONE',  ( -5.297016005617503076, 7.750740434075895635, -1.313619143682826396 ) ) ;
#25083 = CARTESIAN_POINT ( 'NONE',  ( -1.854049621773913525, 5.499999999999998224, 0.7500000000000006661 ) ) ;
#25084 = CARTESIAN_POINT ( 'NONE',  ( 8.914649696185335870, 10.35917838609310593, -1.199719254218446718 ) ) ;
#25085 = CIRCLE ( 'NONE', #114987, 1.500000000000000222 ) ;
#25086 = CARTESIAN_POINT ( 'NONE',  ( 2.262220261732431403, 0.8237980678013016034, 1.741618625116077235 ) ) ;
#25087 = CARTESIAN_POINT ( 'NONE',  ( 5.559412779221331924, 1.601624451964112739, 1.132529127964493121 ) ) ;
#25088 = EDGE_CURVE ( 'NONE', #93416, #139784, #123908, .T. ) ;
#25089 = CARTESIAN_POINT ( 'NONE',  ( -6.009258394948636914E-15, 15.18750000000000000, -1.732050807568875195 ) ) ;
#25090 = CARTESIAN_POINT ( 'NONE',  ( -6.581593504430098385, 9.765943957555402122, -1.199719254218440723 ) ) ;
#25091 = CARTESIAN_POINT ( 'NONE',  ( 4.172158584703322681, 5.890604320285754980, -1.599625672291256295 ) ) ;
#25092 = CARTESIAN_POINT ( 'NONE',  ( -5.655159470231558849, 6.730679149092498648, 1.082531754730549078 ) ) ;
#25093 =( BOUNDED_CURVE ( )  B_SPLINE_CURVE ( 2, ( #97409, #15044, #94213 ),
 .UNSPECIFIED., .F., .T. ) 
 B_SPLINE_CURVE_WITH_KNOTS ( ( 3, 3 ),
 ( 0.000000000000000000, 0.002220828379238357509 ),
 .UNSPECIFIED. ) 
 CURVE ( )  GEOMETRIC_REPRESENTATION_ITEM ( )  RATIONAL_B_SPLINE_CURVE ( ( 1.000000000000000000, 0.9285916995105956140, 0.9333044775364149892 ) ) 
 REPRESENTATION_ITEM ( '' )  );
#25094 = CARTESIAN_POINT ( 'NONE',  ( 3.147464216666835402, 6.823792019419957278, -0.7998128361456291469 ) ) ;
#25095 = CARTESIAN_POINT ( 'NONE',  ( -3.226477370372317743, 4.787309570232886280, 1.443375672974064550 ) ) ;
#25096 = CARTESIAN_POINT ( 'NONE',  ( 5.577033793921920335, 1.910671465402475677, 0.7975372692515869666 ) ) ;
#25098 = CARTESIAN_POINT ( 'NONE',  ( 1.364683531249988757, 2.446875000341415696, 1.214306433183764966E-14 ) ) ;
#25097 = CARTESIAN_POINT ( 'NONE',  ( 6.902720145097993587, 14.55347103577521217, 9.761920446463554057 ) ) ;
#25099 = CARTESIAN_POINT ( 'NONE',  ( 5.362068906036296490, -0.05402111011005260310, -2.298215290733228500 ) ) ;
#25100 = CARTESIAN_POINT ( 'NONE',  ( 6.968527767744104651, 8.192665819532020777, 1.082531754730558626 ) ) ;
#25102 = CARTESIAN_POINT ( 'NONE',  ( -15.75000000000000000, 12.69999999999999929, -3.200000000000001510 ) ) ;
#25101 = CARTESIAN_POINT ( 'NONE',  ( 3.906157654512984134, 7.571284673658201569, -0.7216878364870338292 ) ) ;
#25103 = CARTESIAN_POINT ( 'NONE',  ( 0.1820931442207155415, -1.074843934555272273, 2.024655709774853207 ) ) ;
#25104 = CARTESIAN_POINT ( 'NONE',  ( 7.949604103952363054, -6.836271202499947464, -7.404765023120915224 ) ) ;
#25105 = CARTESIAN_POINT ( 'NONE',  ( -7.761116589180078407, 8.019333873657032541, 0.000000000000000000 ) ) ;
#25106 = CARTESIAN_POINT ( 'NONE',  ( 4.523342001410900259, -1.195735706813789045, -1.530077746507539027 ) ) ;
#25107 = VERTEX_POINT ( 'NONE', #51893 ) ;
#25108 = CARTESIAN_POINT ( 'NONE',  ( 8.961576348508637935, 11.47825837805867799, -1.443375672974052559 ) ) ;
#25109 = EDGE_CURVE ( 'NONE', #96541, #14256, #110828, .T. ) ;
#25110 = ORIENTED_EDGE ( 'NONE', *, *, #191848, .T. ) ;
#25111 = CARTESIAN_POINT ( 'NONE',  ( 5.959226163113887864, -1.611951592244726950, 1.028742869173946861 ) ) ;
#25112 = CARTESIAN_POINT ( 'NONE',  ( 6.159189016523521687, -1.482050057771692186, -0.8820200739605223994 ) ) ;
#25113 = CARTESIAN_POINT ( 'NONE',  ( 5.594935472981866553, 1.780666063871166882, 0.9463038388278844915 ) ) ;
#25115 = CARTESIAN_POINT ( 'NONE',  ( -3.174017359375036929, 6.717120995997236221, 0.7216878364870338292 ) ) ;
#25114 = CARTESIAN_POINT ( 'NONE',  ( -7.980945979938748103, 12.46285407657057220, 0.000000000000000000 ) ) ;
#25116 = CARTESIAN_POINT ( 'NONE',  ( 1.642778471875000035, -1.013541666188708223, -2.845375778867859751 ) ) ;
#25118 = CARTESIAN_POINT ( 'NONE',  ( 0.3909914118310651165, 1.306912223127455919, 1.193654972778479539 ) ) ;
#25117 = CARTESIAN_POINT ( 'NONE',  ( 1.587951679898065294, -2.080713178594826296, -0.2033740637906420179 ) ) ;
#25119 = DIRECTION ( 'NONE',  ( -0.2684563758389304500, -0.000000000000000000, -0.9632918427306581544 ) ) ;
#25121 = CARTESIAN_POINT ( 'NONE',  ( 3.451411174752341715, 0.5572527081592703047, -2.223385661236119581 ) ) ;
#25120 = CARTESIAN_POINT ( 'NONE',  ( 4.167152111353856547, 5.955039778036558040, 1.599625672291262513 ) ) ;
#25122 = CARTESIAN_POINT ( 'NONE',  ( 2.079653994411820417, -1.706432041406182654, -0.3408243062450431182 ) ) ;
#25123 = CARTESIAN_POINT ( 'NONE',  ( 2.760144723603759065, 0.7592700852765141839, -1.980205354017528840 ) ) ;
#25124 = CARTESIAN_POINT ( 'NONE',  ( 1.224999999999934808, 0.7083333340161593883, -0.7072540797573136917 ) ) ;
#25125 = CARTESIAN_POINT ( 'NONE',  ( 2.477566078851959563, 1.547001316009195548, 0.7831083592614047628 ) ) ;
#25126 = CARTESIAN_POINT ( 'NONE',  ( -4.156403723172807449E-14, 1.859375000341410678, -1.570758158831802254 ) ) ;
#25127 = CARTESIAN_POINT ( 'NONE',  ( 1.908444903620472477, 0.5799682436128813512, 1.768463464005122443 ) ) ;
#25128 = CARTESIAN_POINT ( 'NONE',  ( 2.647136220323087485, -0.3691774202370365354, -2.139407045683580755 ) ) ;
#25129 = CARTESIAN_POINT ( 'NONE',  ( 6.810273232766058449, 6.839740281182199233, 1.040834085586084257E-14 ) ) ;
#25130 = CARTESIAN_POINT ( 'NONE',  ( 3.714077560468319827, 1.074663192196689376, -1.706111893292367343 ) ) ;
#25131 = CARTESIAN_POINT ( 'NONE',  ( 4.718750000000002665, -0.7852924748297362978, 1.895863743164184045 ) ) ;
#25132 = CARTESIAN_POINT ( 'NONE',  ( 1.499999999999989120, 2.806250000682818158, 1.214306433183764966E-14 ) ) ;
#25133 = CARTESIAN_POINT ( 'NONE',  ( 0.8680396935916842027, 0.9469273490957976769, 1.677514697326354387 ) ) ;
#25134 = CARTESIAN_POINT ( 'NONE',  ( -1.364683531250010295, 14.88020833367472839, 0.7879004041258445001 ) ) ;
#25135 = CARTESIAN_POINT ( 'NONE',  ( 4.183969649472300212, 2.154223736155444602, -0.5416631952432825470 ) ) ;
#25136 = ORIENTED_EDGE ( 'NONE', *, *, #161571, .F. ) ;
#25137 = CARTESIAN_POINT ( 'NONE',  ( 1.224999999999991651, 2.437500000682837786, -4.336808689942017736E-14 ) ) ;
#25138 = CARTESIAN_POINT ( 'NONE',  ( 1.499999999999987121, 0.7541666666666868579, 0.8660254037844524744 ) ) ;
#25139 = CARTESIAN_POINT ( 'NONE',  ( 7.884230021546724920, 9.157022099014721306, 1.199719254218462483 ) ) ;
#25140 = CARTESIAN_POINT ( 'NONE',  ( -1.364683531250014514, 0.03020833367475737191, 0.7879004041258379498 ) ) ;
#25141 = CARTESIAN_POINT ( 'NONE',  ( 6.539320575229294441, -0.001643797937642132567, 2.203502507913539521 ) ) ;
#25142 = CARTESIAN_POINT ( 'NONE',  ( 5.178158156489047315, -1.047961880893449882, -1.658324637040713867 ) ) ;
#25144 = CARTESIAN_POINT ( 'NONE',  ( -5.205967797967562483, 8.057084283395347768, 1.082531754730548412 ) ) ;
#25143 = CARTESIAN_POINT ( 'NONE',  ( 8.703971430293332645, 12.13808852110884118, -1.082531754730543083 ) ) ;
#25145 = CARTESIAN_POINT ( 'NONE',  ( -1.297623789354738655, 4.098502054883955914, -0.4387493294077370320 ) ) ;
#25146 = CARTESIAN_POINT ( 'NONE',  ( 5.764971491839249396, -2.041691765312734663, -0.9750072289948004123 ) ) ;
#25147 = AXIS2_PLACEMENT_3D ( 'NONE', #65891, #98431, #213222 ) ;
#25148 = CARTESIAN_POINT ( 'NONE',  ( -5.804299160426242388, 6.904675454319632699, -1.082531754730549967 ) ) ;
#25149 = CARTESIAN_POINT ( 'NONE',  ( 2.928243574330684496, 1.101304876339922467, 1.743887257993762763 ) ) ;
#25150 = CARTESIAN_POINT ( 'NONE',  ( -5.045605722580076780, 9.038290442985410067, -0.7998128361456231517 ) ) ;
#25151 = VERTEX_POINT ( 'NONE', #168828 ) ;
#25152 = CARTESIAN_POINT ( 'NONE',  ( -1.500000000000013101, 2.660416667349483788, -0.8660254037844313801 ) ) ;
#25153 = CARTESIAN_POINT ( 'NONE',  ( -0.6823417656250212460, 4.113541667008085767, 1.181850606188767472 ) ) ;
#25154 = CARTESIAN_POINT ( 'NONE',  ( 4.622238261848357510, 1.152259890254858421, -1.473394524551620011 ) ) ;
#25155 = CARTESIAN_POINT ( 'NONE',  ( 4.025767975679870325, -1.506360102045413596, 0.8590090823815172971 ) ) ;
#25156 = CARTESIAN_POINT ( 'NONE',  ( 2.419155098189431641, -1.003372571555812831, -1.421874531148322740 ) ) ;
#25157 = CARTESIAN_POINT ( 'NONE',  ( 0.5918695612782381987, -0.8180161699140885423, 2.141640516796620375 ) ) ;
#25158 = CARTESIAN_POINT ( 'NONE',  ( 1.184930176456780115, -2.153272645635353033, -0.4822455307981614592 ) ) ;
#25159 = CARTESIAN_POINT ( 'NONE',  ( 4.845306142872277455, 0.6545843485197681000, -1.985720288498250774 ) ) ;
#25160 = CARTESIAN_POINT ( 'NONE',  ( 5.894467665742915585, 1.586334124781592969, -1.119885764912365467 ) ) ;
#25162 = ORIENTED_EDGE ( 'NONE', *, *, #134538, .T. ) ;
#25161 = CARTESIAN_POINT ( 'NONE',  ( 0.000000000000000000, 4.099999999999999645, 0.000000000000000000 ) ) ;
#25163 = SHAPE_REPRESENTATION_RELATIONSHIP ( 'NONE' , 'NONE' ,  #62426, #181761 ) ;
#25164 = CARTESIAN_POINT ( 'NONE',  ( 0.9674229098759130618, -1.967888300253183953, -0.4390273639364171698 ) ) ;
#25165 = EDGE_CURVE ( 'NONE', #89693, #175232, #16323, .T. ) ;
#25166 =( LENGTH_UNIT ( ) NAMED_UNIT ( * ) SI_UNIT ( .MILLI., .METRE. ) );
#25167 = DIRECTION ( 'NONE',  ( 0.7613463080411785322, -0.000000000000000000, 0.6483454320283801309 ) ) ;
#25168 = AXIS2_PLACEMENT_3D ( 'NONE', #102918, #135429, #186283 ) ;
#25169 = CARTESIAN_POINT ( 'NONE',  ( -7.804689982961090955, 12.25722208009664094, 0.7998128361456481317 ) ) ;
#25170 = CARTESIAN_POINT ( 'NONE',  ( 7.481401836642521452, 7.622723652371411696, 1.040834085586084257E-14 ) ) ;
#25171 = LINE ( 'NONE', #91272, #80701 ) ;
#25172 = CARTESIAN_POINT ( 'NONE',  ( 4.828627627824715773, 1.747987318788373656, 0.5269492854979712648 ) ) ;
#25173 = CARTESIAN_POINT ( 'NONE',  ( 1.694636308673210801, -2.196210861363355082, -0.2157497520150277459 ) ) ;
#25174 = ORIENTED_EDGE ( 'NONE', *, *, #198514, .T. ) ;
#25175 = CARTESIAN_POINT ( 'NONE',  ( -6.420668264523499147, 9.648474187656182366, 1.199719254218452935 ) ) ;
#25176 = CARTESIAN_POINT ( 'NONE',  ( -0.3846410972798977590, -8.199730735666003412, -9.492545994385777064 ) ) ;
#25177 = CARTESIAN_POINT ( 'NONE',  ( -3.285556943750000514, -2.326041666188709112, -1.896917185911906500 ) ) ;
#25178 = CARTESIAN_POINT ( 'NONE',  ( -7.528855374290365887, 7.678086112960552434, -0.7998128361456291469 ) ) ;
#25179 = CARTESIAN_POINT ( 'NONE',  ( 1.213155585027906325, 1.648708085711389160, -1.166442415167892932 ) ) ;
#25181 = CARTESIAN_POINT ( 'NONE',  ( 5.777182853198898904, 6.873039762554409293, -1.082531754730548412 ) ) ;
#25180 = CIRCLE ( 'NONE', #153201, 4.500000000000000000 ) ;
#25182 = CARTESIAN_POINT ( 'NONE',  ( -3.959863383643135393, 6.777535159962392086, 1.199719254218452935 ) ) ;
#25183 = CARTESIAN_POINT ( 'NONE',  ( 2.658860470891976302, 1.497794124733292431, -1.104231377384189861 ) ) ;
#25184 = CARTESIAN_POINT ( 'NONE',  ( 10.05353459973327368, 11.68787744023238417, -1.199719254218440723 ) ) ;
#25185 = CARTESIAN_POINT ( 'NONE',  ( -3.906720819032141190, 7.709591388846142479, -0.7998128361456281477 ) ) ;
#25186 =( BOUNDED_CURVE ( )  B_SPLINE_CURVE ( 2, ( #90111, #171335, #55458, #191841, #158310, #141023, #9902, #121613, #73845 ),
 .UNSPECIFIED., .F., .T. ) 
 B_SPLINE_CURVE_WITH_KNOTS ( ( 3, 2, 2, 2, 3 ),
 ( 0.3124999999999999445, 0.3154761904761904656, 0.3214285714285714524, 0.3273809523809523836, 0.3303571428571428492 ),
 .UNSPECIFIED. ) 
 CURVE ( )  GEOMETRIC_REPRESENTATION_ITEM ( )  RATIONAL_B_SPLINE_CURVE ( ( 0.9330127018922194093, 0.9330127018922180770, 1.000000000000000000, 0.8660254037844387076, 1.000000000000000000, 0.8660254037844387076, 1.000000000000000000, 0.9330127018922194093, 0.9330127018922194093 ) ) 
 REPRESENTATION_ITEM ( '' )  );
#25187 = CARTESIAN_POINT ( 'NONE',  ( -8.646349277213090545, 11.11049346154719508, 1.599625672291269396 ) ) ;
#25188 = CARTESIAN_POINT ( 'NONE',  ( 4.248545464119923842, 0.4890907236730773766, 1.758887239191930796 ) ) ;
#25190 = CARTESIAN_POINT ( 'NONE',  ( 3.475000000000000533, -2.974999999999998312, 0.000000000000000000 ) ) ;
#25189 = CARTESIAN_POINT ( 'NONE',  ( -6.454563648557663846, 9.688018802362710957, -1.199719254218452047 ) ) ;
#25191 = CARTESIAN_POINT ( 'NONE',  ( 6.038137670975392446, 7.156622065392123311, -1.170913047369964710 ) ) ;
#25192 = CARTESIAN_POINT ( 'NONE',  ( 1.106332979110283610, 0.7092076354480534306, -1.582373438193741322 ) ) ;
#25193 = CARTESIAN_POINT ( 'NONE',  ( 6.122987604524110949, -1.732013368603693593, 0.6248225064409973495 ) ) ;
#25194 = CARTESIAN_POINT ( 'NONE',  ( 4.547712581667567200, -1.782031661950409962, -1.466240793230636275 ) ) ;
#25195 = CARTESIAN_POINT ( 'NONE',  ( 5.174371902270911150, 6.065797303184739420, 1.199719254218452047 ) ) ;
#25196 = CARTESIAN_POINT ( 'NONE',  ( 0.3685255395303523307, -1.348100972195030334, 1.558720748697209224 ) ) ;
#25197 = CARTESIAN_POINT ( 'NONE',  ( 5.396019846235262207, 0.1618137187183350256, 2.292739235009821908 ) ) ;
#25198 = CARTESIAN_POINT ( 'NONE',  ( 0.4019237886466884846, 11.45758545099816494, -1.499999999999994449 ) ) ;
#25199 = CARTESIAN_POINT ( 'NONE',  ( -5.002032328799064231, 4.800402236545811441, -0.7998128361456362523 ) ) ;
#25200 = CARTESIAN_POINT ( 'NONE',  ( 6.157094445334826638, -1.605393284960114242, -0.9600186418455139981 ) ) ;
#25201 = ORIENTED_EDGE ( 'NONE', *, *, #172906, .F. ) ;
#25203 = CARTESIAN_POINT ( 'NONE',  ( -4.309512724297390740, 6.121127159803966933, 1.599625672291270506 ) ) ;
#25202 = CARTESIAN_POINT ( 'NONE',  ( 2.654443970922310214, 1.898414275235399407, 0.2300336082040748686 ) ) ;
#25204 = CARTESIAN_POINT ( 'NONE',  ( 3.703933201646680828, -0.6411959742554216302, 2.111683309420588905 ) ) ;
#25205 = CARTESIAN_POINT ( 'NONE',  ( 5.137957784024314911, 2.114781318005181099, -0.1070058694263714694 ) ) ;
#25206 = CARTESIAN_POINT ( 'NONE',  ( -4.957638175832625493E-14, 0.3750000006828378418, 1.414508159514567431 ) ) ;
#25207 = ADVANCED_FACE ( 'NONE', ( #202371 ), #153661, .F. ) ;
#25208 = CARTESIAN_POINT ( 'NONE',  ( 6.883263157960335832, 7.629137130509037412, 2.646189081643287810 ) ) ;
#25209 = CARTESIAN_POINT ( 'NONE',  ( -0.2110808730067273986, 0.0005491059566040295322, -1.796958327270286704 ) ) ;
#25210 = CARTESIAN_POINT ( 'NONE',  ( 4.950135482320912494, 6.868520377498098739, -1.443375672974068769 ) ) ;
#25211 = CARTESIAN_POINT ( 'NONE',  ( -4.950135482320918712, 7.828889591799445213, -1.082531754730549967 ) ) ;
#25212 = CARTESIAN_POINT ( 'NONE',  ( 2.450585703787050651, 2.307050653106942573, 0.05676454813420374335 ) ) ;
#25213 = CARTESIAN_POINT ( 'NONE',  ( 3.191801227909254912, -1.315628469008291557, -1.455533501494077342 ) ) ;
#25214 = DIRECTION ( 'NONE',  ( 0.9366510587354612838, 0.000000000000000000, -0.3502638921866474409 ) ) ;
#25215 = CARTESIAN_POINT ( 'NONE',  ( 6.895384927792009400, -1.844987169530726723, 0.9222207602926129066 ) ) ;
#25216 = CARTESIAN_POINT ( 'NONE',  ( 2.385871846325007706, 5.727341554113725586, -0.7216878364870267237 ) ) ;
#25217 = CARTESIAN_POINT ( 'NONE',  ( 3.230585741806197841, 6.991043475407723307, 0.7998128361456271485 ) ) ;
#25218 = ORIENTED_EDGE ( 'NONE', *, *, #23600, .F. ) ;
#25219 = CARTESIAN_POINT ( 'NONE',  ( 5.366422816783521732, -1.968444216653497003, -0.4370823996120917765 ) ) ;
#25220 = EDGE_CURVE ( 'NONE', #83638, #192862, #176369, .T. ) ;
#25221 = CARTESIAN_POINT ( 'NONE',  ( -9.267161690140662600, 10.77044237904097734, -1.199719254218441611 ) ) ;
#25222 = CARTESIAN_POINT ( 'NONE',  ( -1.500000000000043299, 4.170833333333358262, 0.8660254037844216102 ) ) ;
#25223 = CARTESIAN_POINT ( 'NONE',  ( -10.60630082101195804, 5.715768461961713953, -4.896526734066639186 ) ) ;
#25224 = CARTESIAN_POINT ( 'NONE',  ( 9.745613490124728884, 10.26430391476735338, 0.7998128361456462443 ) ) ;
#25225 = CARTESIAN_POINT ( 'NONE',  ( 1.534277631021633059, 1.291084678180357104, 1.745351423456573015 ) ) ;
#25226 = CARTESIAN_POINT ( 'NONE',  ( 4.393008644795362905, 7.016788222801661590, 1.284222742053114041 ) ) ;
#25227 = ADVANCED_FACE ( 'NONE', ( #141717 ), #204006, .T. ) ;
#25228 = PRESENTATION_STYLE_ASSIGNMENT (( #158444 ) ) ;
#25229 = CARTESIAN_POINT ( 'NONE',  ( 4.725438941449205288, 8.332574750205820280, 0.7120043264817934592 ) ) ;
#25230 = CARTESIAN_POINT ( 'NONE',  ( 1.177107960601676551, -0.04769765464058715876, -2.060389331245067179 ) ) ;
#25232 = CARTESIAN_POINT ( 'NONE',  ( 6.727182134110196721, 3.701357331967893405, 2.425430364167603603 ) ) ;
#25231 = CARTESIAN_POINT ( 'NONE',  ( 6.938893903907228378E-15, 10.64264068711930733, 1.214306433183764966E-14 ) ) ;
#25233 = CARTESIAN_POINT ( 'NONE',  ( -0.6823417656250003738, 0.9677083336747521747, -1.181850606188749264 ) ) ;
#25234 = DIRECTION ( 'NONE',  ( 0.000000000000000000, -1.000000000000000000, 0.000000000000000000 ) ) ;
#25235 = ORIENTED_EDGE ( 'NONE', *, *, #131603, .T. ) ;
#25236 = CARTESIAN_POINT ( 'NONE',  ( 3.246637215680724164, 1.866209232881730573, 0.4165188312477489663 ) ) ;
#25237 = CIRCLE ( 'NONE', #135944, 0.5000000000000013323 ) ;
#25238 = CARTESIAN_POINT ( 'NONE',  ( 4.873781607783202574, 1.020544065373253817, 1.445763320596996193 ) ) ;
#25239 = CARTESIAN_POINT ( 'NONE',  ( 5.712781623311797397, 7.758274208654143855, -1.599625672291283607 ) ) ;
#25240 = AXIS2_PLACEMENT_3D ( 'NONE', #83612, #199480, #180066 ) ;
#25241 = CARTESIAN_POINT ( 'NONE',  ( -5.264643720808155791, 5.036505850564608089, 0.000000000000000000 ) ) ;
#25243 = CARTESIAN_POINT ( 'NONE',  ( 0.1982580178685423022, 1.319089833320963079, -1.389493073782912091 ) ) ;
#25242 = CYLINDRICAL_SURFACE ( 'NONE', #59573, 3.475000000000000089 ) ;
#25244 = CARTESIAN_POINT ( 'NONE',  ( -1.500000000000001332, -0.09999999999997510880, 0.000000000000000000 ) ) ;
#25245 = CARTESIAN_POINT ( 'NONE',  ( 0.4321921490204432281, 1.190796696626210682, 1.693455153822187587 ) ) ;
#25246 = CARTESIAN_POINT ( 'NONE',  ( -1.201851678989727383E-14, 5.837500000000023448, -1.732050807568863648 ) ) ;
#25247 = CARTESIAN_POINT ( 'NONE',  ( 6.614126560844452385, -0.8839695271746010885, -1.648598838400926692 ) ) ;
#25248 = CARTESIAN_POINT ( 'NONE',  ( 3.351995281737112364, 1.825872481133209879, -0.0009662468829912954560 ) ) ;
#25250 = CARTESIAN_POINT ( 'NONE',  ( 4.637309883081485395, 8.320457421531981979, 0.4059539251603030974 ) ) ;
#25249 = CARTESIAN_POINT ( 'NONE',  ( 5.795608111622330583, 1.668732747960173235, 1.444295198399044855 ) ) ;
#25251 = CARTESIAN_POINT ( 'NONE',  ( -1.364683531250014514, 0.4885416670080875434, -0.7879004041258289570 ) ) ;
#25252 = CARTESIAN_POINT ( 'NONE',  ( 2.629405133799759486, 0.1038056934173016560, -2.060197576267445818 ) ) ;
#25253 = CARTESIAN_POINT ( 'NONE',  ( -5.879432169820529630, 10.01108796476595764, -0.7998128361456221525 ) ) ;
#25254 = CARTESIAN_POINT ( 'NONE',  ( 7.703003830858588863, 12.13858823597705872, -0.7998128361456291469 ) ) ;
#25255 = CARTESIAN_POINT ( 'NONE',  ( -1.249999999999964695, 8.500000000000000000, 11.02939254900287303 ) ) ;
#25256 = ADVANCED_FACE ( 'NONE', ( #91885 ), #81516, .T. ) ;
#25257 = CARTESIAN_POINT ( 'NONE',  ( 0.5444778865218367070, 2.155786741090206959, 0.1595364878888144988 ) ) ;
#25258 = CARTESIAN_POINT ( 'NONE',  ( 6.475954649182838807, 7.584310507915338562, 1.199719254218452047 ) ) ;
#25259 = CARTESIAN_POINT ( 'NONE',  ( 5.213363469605923228, -1.747142239327776903, -1.110534646669825376 ) ) ;
#25260 = CARTESIAN_POINT ( 'NONE',  ( -1.402160292154681736E-14, -0.1156249996585793222, 1.575800808251672791 ) ) ;
#25261 = CARTESIAN_POINT ( 'NONE',  ( 3.356853517036356038, -1.639235867460669294, 1.409173823127254144 ) ) ;
#25262 = CARTESIAN_POINT ( 'NONE',  ( -4.665006653791238911, 8.307176129776033591, 0.4851093158183654719 ) ) ;
#25264 = CARTESIAN_POINT ( 'NONE',  ( 1.908577322519442454, 0.6123880975643315461, 1.863924812142327525 ) ) ;
#25263 = CARTESIAN_POINT ( 'NONE',  ( 2.895180478094826704, -0.1506588039767979559, -2.014126839200135688 ) ) ;
#25265 = CARTESIAN_POINT ( 'NONE',  ( 7.629869294364564958, -5.350481869465718354, 7.876942567271134621 ) ) ;
#25268 = CARTESIAN_POINT ( 'NONE',  ( 5.314433026876846711, 9.143996264757578984, -0.7216878364870267237 ) ) ;
#25267 = CARTESIAN_POINT ( 'NONE',  ( 3.475000000000000533, -2.245833333333331350, -2.006292185433951047 ) ) ;
#25266 = CARTESIAN_POINT ( 'NONE',  ( -1.499999999999946709, 7.750000000000000000, 15.75000000000000711 ) ) ;
#25269 = CARTESIAN_POINT ( 'NONE',  ( -5.824109505522200081, 8.952488968821326054, -1.199719254218452047 ) ) ;
#25270 = CARTESIAN_POINT ( 'NONE',  ( 1.165250339122084533, 1.861343190080061882, -0.7762330495894869120 ) ) ;
#25272 = CARTESIAN_POINT ( 'NONE',  ( 6.040607902356621040, -1.852314659301614874, 1.170993205287726768 ) ) ;
#25271 = CARTESIAN_POINT ( 'NONE',  ( -4.232116505760120440, 8.089219690028791376, -0.7998128361456281477 ) ) ;
#25273 = CARTESIAN_POINT ( 'NONE',  ( -3.707465945607718805, 7.355851012256872323, 0.5743249234583160945 ) ) ;
#25274 = CARTESIAN_POINT ( 'NONE',  ( 6.170165192347925043, 1.906784905861274249, -0.1475879885542986658 ) ) ;
#25275 = CARTESIAN_POINT ( 'NONE',  ( -11.89197816957260123, 12.30000000000000071, 0.8055420615339489165 ) ) ;
#25276 = CARTESIAN_POINT ( 'NONE',  ( 5.680503174001485078, 6.689970460165617361, -1.082531754730543083 ) ) ;
#25278 = CARTESIAN_POINT ( 'NONE',  ( 3.392203995056555232, -0.8197896108859267228, -1.842441248588816860 ) ) ;
#25277 = CARTESIAN_POINT ( 'NONE',  ( -8.988692655735990300, 9.589155641221221771, 0.7216878364870438212 ) ) ;
#25279 = CARTESIAN_POINT ( 'NONE',  ( 1.499999999999990896, 3.775000000000021227, 1.214306433183764966E-14 ) ) ;
#25280 = CARTESIAN_POINT ( 'NONE',  ( -8.012344526598182026E-15, 14.10937500034139802, -1.575800808251669460 ) ) ;
#25281 = CARTESIAN_POINT ( 'NONE',  ( 6.581054485068423610, -0.09077197429533871709, -1.722499283940544634 ) ) ;
#25282 = CARTESIAN_POINT ( 'NONE',  ( 5.515134625708930649, 9.656350506627580543, 0.000000000000000000 ) ) ;
#25283 = CONICAL_SURFACE ( 'NONE', #187777, 1.540450515248283025, 0.7853981633974428389 ) ;
#25284 = CARTESIAN_POINT ( 'NONE',  ( 9.571693261567965294, 10.26932301469188857, 0.7216878364870438212 ) ) ;
#25285 = CARTESIAN_POINT ( 'NONE',  ( -0.4205683736966763231, 3.129384673317354704, 0.4296503687815398376 ) ) ;
#25286 = CARTESIAN_POINT ( 'NONE',  ( 4.674985431947434655, 0.001863223488791227334, -1.870726058175266715 ) ) ;
#25287 = SURFACE_SIDE_STYLE ('',( #120743 ) ) ;
#25288 = ORIENTED_EDGE ( 'NONE', *, *, #139797, .T. ) ;
#25289 = CARTESIAN_POINT ( 'NONE',  ( 2.518496159030516601, 0.8812310945605882351, 1.873447404777649261 ) ) ;
#25290 = CARTESIAN_POINT ( 'NONE',  ( 0.4373347461412347426, -7.712532583864853741, -10.97876033714413069 ) ) ;
#25291 = VERTEX_POINT ( 'NONE', #160054 ) ;
#25292 = CARTESIAN_POINT ( 'NONE',  ( 3.542423274920540432, 7.354853930707762721, -1.734723475976807094E-15 ) ) ;
#25293 = CARTESIAN_POINT ( 'NONE',  ( 0.2108110590392465178, 1.506053368259860248, -1.006445417241896845 ) ) ;
#25294 = CARTESIAN_POINT ( 'NONE',  ( 3.838366886000300404, 6.531826229425389485, -1.082531754730548412 ) ) ;
#25295 = CARTESIAN_POINT ( 'NONE',  ( -1.364683531249997417, 5.790625000341422357, 1.214306433183764966E-14 ) ) ;
#25296 = EDGE_LOOP ( 'NONE', ( #55223, #94245, #153883, #175868 ) ) ;
#25297 = CARTESIAN_POINT ( 'NONE',  ( 9.259855728009286580, 10.86588177317476855, -1.082531754730543083 ) ) ;
#25299 = CARTESIAN_POINT ( 'NONE',  ( 8.589254009457354400, 9.979550084910457031, -1.199719254218446718 ) ) ;
#25298 = CARTESIAN_POINT ( 'NONE',  ( 1.504273306027693602, 1.959471947749168663, 0.09963418240711149898 ) ) ;
#25300 = TOROIDAL_SURFACE ( 'NONE', #49566, 7.374593666277937665, 0.08000000000000000167 ) ;
#25301 = CARTESIAN_POINT ( 'NONE',  ( 5.554270809058080793, -1.211575977211576172, 1.483806794280813302 ) ) ;
#25302 = CARTESIAN_POINT ( 'NONE',  ( -4.133872419145380839, 3.976560215030992662, -0.5735765104555013982 ) ) ;
#25303 = DIRECTION ( 'NONE',  ( 0.6507913734559652719, 0.7592566023652995710, 1.725633230170963762E-31 ) ) ;
#25305 = EDGE_LOOP ( 'NONE', ( #169051, #142565, #213254 ) ) ;
#25304 = CARTESIAN_POINT ( 'NONE',  ( 5.016153647376212277, 5.914896012436124728, 1.082531754730558626 ) ) ;
#25306 = CARTESIAN_POINT ( 'NONE',  ( -8.378575743565381373, 8.877352577022161739, 0.7216878364870438212 ) ) ;
#25307 = CARTESIAN_POINT ( 'NONE',  ( 2.711983997553392811, -2.138339778157403615, 0.3160903847422362745 ) ) ;
#25308 = CARTESIAN_POINT ( 'NONE',  ( -5.966997003790217136, 9.975597247814986801, -0.7216878364870338292 ) ) ;
#25309 = CARTESIAN_POINT ( 'NONE',  ( 5.709392085130549077, 9.675058176045386205, 0.000000000000000000 ) ) ;
#25310 = CARTESIAN_POINT ( 'NONE',  ( -2.927671105547157371, 5.503034492191895666, 1.199719254218462483 ) ) ;
#25311 = CARTESIAN_POINT ( 'NONE',  ( 6.317409609008932669, -0.2203418483949574069, 1.812181760327068680 ) ) ;
#25312 = VECTOR ( 'NONE', #25466, 1000.000000000000000 ) ;
#25313 = CARTESIAN_POINT ( 'NONE',  ( 10.24318454578369852, 9.275991984790607603, -5.779941430892880483 ) ) ;
#25314 = CARTESIAN_POINT ( 'NONE',  ( 1.264844077314925652, -1.780367465076490019, -0.8468111885079774304 ) ) ;
#25315 = CARTESIAN_POINT ( 'NONE',  ( 3.392734571251673881, -1.844325299564765652, -0.5055192353106837677 ) ) ;
#25316 = ORIENTED_EDGE ( 'NONE', *, *, #53487, .T. ) ;
#25317 = CARTESIAN_POINT ( 'NONE',  ( -11.52483635780544624, 9.720000086424647634, -3.345866325258088914 ) ) ;
#25318 = CARTESIAN_POINT ( 'NONE',  ( 5.142998410927586583, -0.2390059684120172390, -1.954905448695958059 ) ) ;
#25319 = ORIENTED_EDGE ( 'NONE', *, *, #47376, .F. ) ;
#25320 = CARTESIAN_POINT ( 'NONE',  ( 6.251511512115349056, 1.936530502255621622, -0.1475284815631947022 ) ) ;
#25321 = EDGE_LOOP ( 'NONE', ( #138966, #62331, #140605, #88168, #93539, #84687, #155470, #175835 ) ) ;
#25322 = CARTESIAN_POINT ( 'NONE',  ( -4.288121723672178476, 8.224835454251337552, -0.7998128361456362523 ) ) ;
#25324 = CARTESIAN_POINT ( 'NONE',  ( 6.345950370838200350, -1.386202306585911925, -1.604841549997563455 ) ) ;
#25323 = CARTESIAN_POINT ( 'NONE',  ( -4.553559489343377287, 6.405848385690952718, -1.599625672291271394 ) ) ;
#25325 = CARTESIAN_POINT ( 'NONE',  ( 7.987161891782087686, 8.490979426600148372, -0.7216878364870317197 ) ) ;
#25327 = EDGE_LOOP ( 'NONE', ( #122261, #35315, #87118, #208741 ) ) ;
#25326 = CARTESIAN_POINT ( 'NONE',  ( 4.389254143344611947, -0.003399479254035177832, -1.912461472815998320 ) ) ;
#25328 = AXIS2_PLACEMENT_3D ( 'NONE', #121110, #73320, #158859 ) ;
#25329 = CARTESIAN_POINT ( 'NONE',  ( 0.7455094363101981703, -1.891729906373079029, 1.136061337225414913 ) ) ;
#25330 = CARTESIAN_POINT ( 'NONE',  ( 9.444297818689598500, 3.530917896769790065, -7.404075800243193228 ) ) ;
#25331 = CARTESIAN_POINT ( 'NONE',  ( 6.147140879040452255, 0.1997598139246952731, 2.003170966399501651 ) ) ;
#25332 = DIRECTION ( 'NONE',  ( 0.000000000000000000, 0.000000000000000000, -1.000000000000000000 ) ) ;
#25333 = CARTESIAN_POINT ( 'NONE',  ( 5.953692858212231265, 0.5253669772854427933, -1.748464709795935157 ) ) ;
#25334 = CARTESIAN_POINT ( 'NONE',  ( 2.313015868914463091, -1.601887806243259771, 1.311650804931147274 ) ) ;
#25335 = CARTESIAN_POINT ( 'NONE',  ( -6.470265622219711688, 8.571729197388226140, -1.599625672291263179 ) ) ;
#25336 = CARTESIAN_POINT ( 'NONE',  ( -5.221311770390402174, 7.721201550036163042, -1.200461426208466076 ) ) ;
#25337 = CARTESIAN_POINT ( 'NONE',  ( 1.270904146967301473, 2.834693569853255823, -0.7749999999999910294 ) ) ;
#25338 = CARTESIAN_POINT ( 'NONE',  ( 6.719622092096638966, -1.813896567892055112, 0.4569536213836836169 ) ) ;
#25339 = CARTESIAN_POINT ( 'NONE',  ( 6.796715079152391148, 6.823922435299587974, 0.7998128361456341429 ) ) ;
#25340 = DIRECTION ( 'NONE',  ( -5.578564026256490882E-16, -1.000000000000000000, -9.066213480720158442E-32 ) ) ;
#25341 = CARTESIAN_POINT ( 'NONE',  ( 3.933273961740296087, 6.642551151122080277, 1.082531754730549078 ) ) ;
#25342 = ADVANCED_FACE ( 'NONE', ( #143853 ), #205587, .F. ) ;
#25343 = DIRECTION ( 'NONE',  ( -1.000000000000000000, 1.014813233446432150E-15, 1.972152263052529514E-31 ) ) ;
#25344 = CARTESIAN_POINT ( 'NONE',  ( -0.6823417656250003738, 11.71354166700806765, 1.181850606188754593 ) ) ;
#25346 = CARTESIAN_POINT ( 'NONE',  ( -5.121948170912633991, 9.197632976031879792, -0.7998128361456362523 ) ) ;
#25345 = CARTESIAN_POINT ( 'NONE',  ( 6.925078400183515726, -0.002206826874838820583, 1.955452213090567160 ) ) ;
#25347 = CARTESIAN_POINT ( 'NONE',  ( 5.098194074801078557, -0.2466363661708069477, 1.716370243172520516 ) ) ;
#25348 = CARTESIAN_POINT ( 'NONE',  ( -5.264643720808155791, 5.036505850564608089, 0.000000000000000000 ) ) ;
#25349 = CARTESIAN_POINT ( 'NONE',  ( 2.395452669547156077, -1.851176756146424074, 0.9269567275110508486 ) ) ;
#25350 = CARTESIAN_POINT ( 'NONE',  ( 3.462624114536147157, -2.041159069107215007, -0.5622701121768166610 ) ) ;
#25351 = CARTESIAN_POINT ( 'NONE',  ( 5.777746017718023097, 9.892454120646377191, 0.7998128361456462443 ) ) ;
#25352 = CARTESIAN_POINT ( 'NONE',  ( -1.364683531249997417, 3.759375000341423689, 1.214306433183764966E-14 ) ) ;
#25353 = CARTESIAN_POINT ( 'NONE',  ( 2.201947278869041291, 0.7584239558163529127, -1.817761916770490149 ) ) ;
#25354 = CARTESIAN_POINT ( 'NONE',  ( 5.379472278790374595, 6.509029678566758292, 1.321781506194243727 ) ) ;
#25356 = CARTESIAN_POINT ( 'NONE',  ( 1.387358672534390935, 7.315968950353690659, -4.254625267138188782 ) ) ;
#25355 = CARTESIAN_POINT ( 'NONE',  ( -1.737499999999997824, -1.691666666666667762, 3.009438278150925683 ) ) ;
#25357 = CARTESIAN_POINT ( 'NONE',  ( 4.101757505036166762, -2.286240945789700607, 0.1669829803510776423 ) ) ;
#25358 = CARTESIAN_POINT ( 'NONE',  ( 2.033574986395149775, -1.191784744093337123, -1.383114941912518159 ) ) ;
#25359 = CARTESIAN_POINT ( 'NONE',  ( 6.554440917563797875, 6.611545590104705994, -0.7998128361456481317 ) ) ;
#25360 = CARTESIAN_POINT ( 'NONE',  ( 5.138177029454829459, 8.938364267765221527, 0.7216878364870438212 ) ) ;
#25361 = CARTESIAN_POINT ( 'NONE',  ( -6.333630315878337136, 10.54098580183340772, 0.000000000000000000 ) ) ;
#25362 =( BOUNDED_SURFACE ( )  B_SPLINE_SURFACE ( 3, 2, ( 
 ( #156128, #73793, #139888 ),
 ( #140974, #74868, #126900 ),
 ( #27168, #159307, #91134 ),
 ( #161461, #125832, #124767 ),
 ( #129032, #174523, #45581 ),
 ( #206983, #58612, #190727 ) ),
 .UNSPECIFIED., .F., .F., .T. ) 
 B_SPLINE_SURFACE_WITH_KNOTS ( ( 4, 2, 4 ),
 ( 3, 3 ),
 ( 0.000000000000000000, 0.0003766405729503173702, 0.0007532811459006347405 ),
 ( 0.000000000000000000, 1.000000000000000000 ),
 .UNSPECIFIED. ) 
 GEOMETRIC_REPRESENTATION_ITEM ( )  RATIONAL_B_SPLINE_SURFACE ( (
 ( 1.000000000000000000, 0.7071067811865474617, 1.000000000000000000),
 ( 1.000000000000000000, 0.7211294902955810437, 1.000000000000000000),
 ( 1.000000000000000000, 0.7311181975227820651, 1.000000000000000000),
 ( 1.000000000000000000, 0.7429553055063957689, 1.000000000000000000),
 ( 1.000000000000000000, 0.7451698531056420993, 1.000000000000000000),
 ( 1.000000000000000000, 0.7452309222762957264, 1.000000000000000000) ) ) 
 REPRESENTATION_ITEM ( '' )  SURFACE ( )  );
#25363 = CARTESIAN_POINT ( 'NONE',  ( 3.410405542056849981, -2.011076457950426555, -0.09466423678533388009 ) ) ;
#25364 = CARTESIAN_POINT ( 'NONE',  ( 2.483191118468269565, -0.005009705968514814069, 1.961936380092830223 ) ) ;
#25365 = CARTESIAN_POINT ( 'NONE',  ( -6.835281999583978418, 11.12624609948998966, -0.7998128361456291469 ) ) ;
#25366 = CARTESIAN_POINT ( 'NONE',  ( -5.713871673155502151, 8.753601821068331290, 1.199719254218452047 ) ) ;
#25367 = DIRECTION ( 'NONE',  ( -0.000000000000000000, -1.000000000000000000, -0.000000000000000000 ) ) ;
#25369 = CARTESIAN_POINT ( 'NONE',  ( 4.803428869931958722, -0.4704684023625771983, 1.706073424435787134 ) ) ;
#25368 = CARTESIAN_POINT ( 'NONE',  ( 5.841762345275034463, 2.088193589346263312, 0.1035180442379990684 ) ) ;
#25370 = CARTESIAN_POINT ( 'NONE',  ( -1.878313713276878127, 14.99999999999692157, 12.68000002627078082 ) ) ;
#25371 = CARTESIAN_POINT ( 'NONE',  ( 0.5686479265839607944, -2.064760635122906418, -0.7346842419702694915 ) ) ;
#25372 = CARTESIAN_POINT ( 'NONE',  ( 5.859256971114414014, 1.713395515214741538, -0.3040290152411839752 ) ) ;
#25373 = CARTESIAN_POINT ( 'NONE',  ( 7.781490099239519509, 11.16582331816642260, 1.199719254218460707 ) ) ;
#25374 = DIRECTION ( 'NONE',  ( 0.000000000000000000, 1.000000000000000000, 0.000000000000000000 ) ) ;
#25375 = CARTESIAN_POINT ( 'NONE',  ( 6.557281991921043662, -1.419039031320767474, 1.809608378690949149 ) ) ;
#25376 = CARTESIAN_POINT ( 'NONE',  ( -3.474999999999997868, -1.327083332377416713, 2.006292185433951047 ) ) ;
#25377 = CARTESIAN_POINT ( 'NONE',  ( 5.044171318280882055, 1.617313383883935529, -0.6254187727454744161 ) ) ;
#25378 = VECTOR ( 'NONE', #61416, 1000.000000000000000 ) ;
#25379 = CARTESIAN_POINT ( 'NONE',  ( 5.617690636765501289, 0.4290425436993560715, -2.128212118068722347 ) ) ;
#25380 = CARTESIAN_POINT ( 'NONE',  ( -1.500000000000008216, 11.24999999999999645, 3.469446951953614189E-15 ) ) ;
#25381 = CARTESIAN_POINT ( 'NONE',  ( 0.2689693067343159605, -0.2660441693766130711, -2.100534484541769498 ) ) ;
#25382 = CARTESIAN_POINT ( 'NONE',  ( 3.718750000000002220, -0.7852924748297895885, 1.895863743164163617 ) ) ;
#25383 = VECTOR ( 'NONE', #59680, 1000.000000000000000 ) ;
#25384 = CARTESIAN_POINT ( 'NONE',  ( 0.000000000000000000, -9.331509131462439655, 0.000000000000000000 ) ) ;
#25385 = CARTESIAN_POINT ( 'NONE',  ( 4.032187520235196665, 1.031363847994439142, -1.626874456138996949 ) ) ;
#25386 = CARTESIAN_POINT ( 'NONE',  ( 1.500000000000001332, 10.65625000068279249, 0.000000000000000000 ) ) ;
#25387 = CARTESIAN_POINT ( 'NONE',  ( 0.6982527715983916083, 1.495984496936525021, 1.642170479989105480 ) ) ;
#25388 = ORIENTED_EDGE ( 'NONE', *, *, #104171, .F. ) ;
#25389 = CARTESIAN_POINT ( 'NONE',  ( 1.499999999999990896, 4.275000000000021672, 1.214306433183764966E-14 ) ) ;
#25390 = CARTESIAN_POINT ( 'NONE',  ( 5.443762371086860341, 6.309809840144842141, 1.199719254218462483 ) ) ;
#25391 = CARTESIAN_POINT ( 'NONE',  ( 7.657657833620182153, 7.828355648845348291, -0.7998128361456281477 ) ) ;
#25392 = CARTESIAN_POINT ( 'NONE',  ( 2.209928731909744481, 1.719286606775907611, 1.406518386542881638 ) ) ;
#25393 = CARTESIAN_POINT ( 'NONE',  ( -8.514157279702033065, 9.995900250149611921, -1.082531754730543971 ) ) ;
#25394 = DIRECTION ( 'NONE',  ( 0.000000000000000000, 0.000000000000000000, 1.000000000000000000 ) ) ;
#25395 = CARTESIAN_POINT ( 'NONE',  ( 7.321039761699430493, 7.643560598178549270, -0.7216878364870257245 ) ) ;
#25396 = CARTESIAN_POINT ( 'NONE',  ( -8.148087131688679818, 12.44992605370473804, -0.7216878364870267237 ) ) ;
#25397 = CARTESIAN_POINT ( 'NONE',  ( 5.885648082108188461, 8.920320958217979879, 1.082531754730549967 ) ) ;
#25398 = CARTESIAN_POINT ( 'NONE',  ( 0.6861729220449981348, 1.650083401500940239, 1.158686392676591570 ) ) ;
#25400 = CARTESIAN_POINT ( 'NONE',  ( 6.391093295415360309, 0.1985076180841711668, 2.053089703019762791 ) ) ;
#25399 = CARTESIAN_POINT ( 'NONE',  ( 7.730120138085914583, 12.17022392774227768, 0.7998128361456462443 ) ) ;
#25401 = CARTESIAN_POINT ( 'NONE',  ( 5.844973620822830895, 8.872867420051733234, 1.082531754730549967 ) ) ;
#25402 = CARTESIAN_POINT ( 'NONE',  ( 1.364683531249988757, 1.134375000341421247, 0.000000000000000000 ) ) ;
#25403 = CARTESIAN_POINT ( 'NONE',  ( 0.8953273879380260203, -0.6444125412686675380, 1.648433012593934155 ) ) ;
#25404 = CARTESIAN_POINT ( 'NONE',  ( 0.2818752512256904597, 1.674885806461807958, -1.122501178855893400 ) ) ;
#25405 = CARTESIAN_POINT ( 'NONE',  ( 5.970193594734433340, -1.655480682217812083, -0.5374289683400793605 ) ) ;
#25406 = CARTESIAN_POINT ( 'NONE',  ( 4.652058317211603011, 0.8762739730861779375, 2.118468771859642441 ) ) ;
#25407 = CARTESIAN_POINT ( 'NONE',  ( 0.6823417656249864960, -1.073958332991911568, -1.181850606188749264 ) ) ;
#25408 = CARTESIAN_POINT ( 'NONE',  ( 2.027068592762204080, -1.202062398780713748, -1.394650109237540070 ) ) ;
#25409 = CARTESIAN_POINT ( 'NONE',  ( 8.778014389843965759, 12.32843499053828928, 1.199719254218450271 ) ) ;
#25410 = CARTESIAN_POINT ( 'NONE',  ( 3.223480179809079971, -1.759765543241718966, 0.4855387900214308550 ) ) ;
#25411 = CARTESIAN_POINT ( 'NONE',  ( 3.604138833494671346, -0.1455340571130462057, 2.011204217620660817 ) ) ;
#25412 = CARTESIAN_POINT ( 'NONE',  ( -10.65400978224035811, 11.32409958890225710, 1.040834085586084257E-14 ) ) ;
#25414 = LINE ( 'NONE', #127285, #65646 ) ;
#25413 = CARTESIAN_POINT ( 'NONE',  ( 1.833286743572108968, 0.2227676567047157941, 2.251508545315301646 ) ) ;
#25415 = CARTESIAN_POINT ( 'NONE',  ( 5.297925755477892906, -0.7609016685872365127, 1.963875245004148562 ) ) ;
#25416 = CARTESIAN_POINT ( 'NONE',  ( 8.542663007067599068, 15.39167316688947018, 7.880542118333895729 ) ) ;
#25417 = CARTESIAN_POINT ( 'NONE',  ( 2.998552181135270001, 2.054425100943928051, 0.2560010573490826835 ) ) ;
#25418 = CARTESIAN_POINT ( 'NONE',  ( 5.030238685870051185, 5.827365540725222282, -1.199719254218452047 ) ) ;
#25419 = CARTESIAN_POINT ( 'NONE',  ( -1.360316468749996677, 0.4010416670080598767, -0.7853790794158941324 ) ) ;
#25420 = CARTESIAN_POINT ( 'NONE',  ( 4.987034407221377030, -1.996844880220369545, -0.7138980100366009163 ) ) ;
#25422 = CARTESIAN_POINT ( 'NONE',  ( 0.7504602152685091454, 0.5580118324238073635, 1.843911685078497120 ) ) ;
#25421 = CARTESIAN_POINT ( 'NONE',  ( -9.561524646135538319, 12.17819805862340310, -1.599625672291263179 ) ) ;
#25423 = CARTESIAN_POINT ( 'NONE',  ( -5.167592825464113915, 6.057888380243431570, 1.199719254218452935 ) ) ;
#25424 = CARTESIAN_POINT ( 'NONE',  ( 8.097244055859613709, 10.46987070330147063, -1.599625672291262513 ) ) ;
#25425 = CARTESIAN_POINT ( 'NONE',  ( 4.678972410047582464, 8.472901888448573615, -0.7216878364870357165 ) ) ;
#25426 = CARTESIAN_POINT ( 'NONE',  ( 4.847318722290685500, 6.704483692258053296, 1.249926399124022147 ) ) ;
#25427 = CARTESIAN_POINT ( 'NONE',  ( -3.475000000000000533, -0.3062499990440850639, 0.000000000000000000 ) ) ;
#25428 = CARTESIAN_POINT ( 'NONE',  ( -3.554208825076827782, 7.298327395898266623, 0.7998128361456341429 ) ) ;
#25429 = CARTESIAN_POINT ( 'NONE',  ( 5.941668366282724101, -1.996146358238064522, 0.7160658055916299114 ) ) ;
#25430 = CARTESIAN_POINT ( 'NONE',  ( 1.694499644457616583, -2.095784359944006248, -0.2068371402374687973 ) ) ;
#25431 = CARTESIAN_POINT ( 'NONE',  ( -3.305155586681401303, 7.078041627762083898, 0.7998128361456352531 ) ) ;
#25432 = CARTESIAN_POINT ( 'NONE',  ( 6.903072767652295383, 11.20533532890304684, 1.040834085586084257E-14 ) ) ;
#25433 = CARTESIAN_POINT ( 'NONE',  ( 6.455886261557550299, -0.6278800607443285609, 1.751925260802848827 ) ) ;
#25434 = CARTESIAN_POINT ( 'NONE',  ( 7.935599982700328958, 8.152621489438862667, 0.7998128361456481317 ) ) ;
#25435 =( NAMED_UNIT ( * ) PLANE_ANGLE_UNIT ( ) SI_UNIT ( $, .RADIAN. ) );
#25436 = CARTESIAN_POINT ( 'NONE',  ( -3.526002468005825286, 6.271364091718859335, -1.199719254218450271 ) ) ;
#25437 = CARTESIAN_POINT ( 'NONE',  ( -9.327646496521989405, 10.94497100310623594, -1.082531754730539753 ) ) ;
#25438 = CARTESIAN_POINT ( 'NONE',  ( -1.854512760316423536, 2.488359591189891251, 2.484105960264900936 ) ) ;
#25439 = DIRECTION ( 'NONE',  ( 1.000000000000000000, 0.000000000000000000, 0.000000000000000000 ) ) ;
#25441 = CARTESIAN_POINT ( 'NONE',  ( 2.840232074097197579, -1.010955899468408248, 1.681206195012739046 ) ) ;
#25440 = CARTESIAN_POINT ( 'NONE',  ( 0.6124999999999707345, -0.5833333333332968440, -1.060881119635976200 ) ) ;
#25442 = CARTESIAN_POINT ( 'NONE',  ( 2.518638242371186386, 1.412657066830936392, -1.636333507658905173 ) ) ;
#25444 = CARTESIAN_POINT ( 'NONE',  ( -5.526577223899823643, 6.240148858909590146, -0.9599604131041916677 ) ) ;
#25443 = CARTESIAN_POINT ( 'NONE',  ( -5.123001941117347080, 7.070197912760590064, 1.599625672291263179 ) ) ;
#25445 = CARTESIAN_POINT ( 'NONE',  ( -0.6823417656250003738, 1.717708333674752730, -1.181850606188749264 ) ) ;
#25446 = CARTESIAN_POINT ( 'NONE',  ( 3.644249385861945800, -1.421566135898670646, 1.003629588703761621 ) ) ;
#25447 = CARTESIAN_POINT ( 'NONE',  ( 7.022760382198770301, 8.255937203062467589, -1.082531754730543083 ) ) ;
#25448 = CARTESIAN_POINT ( 'NONE',  ( -12.00288634729131232, 5.507422065878898820, 4.496070577805427959 ) ) ;
#25449 = ORIENTED_EDGE ( 'NONE', *, *, #175830, .F. ) ;
#25450 = VECTOR ( 'NONE', #147537, 1000.000000000000000 ) ;
#25451 = CARTESIAN_POINT ( 'NONE',  ( 2.723982329760873178, -1.752761823190003287, -0.9961495992579154635 ) ) ;
#25452 = CARTESIAN_POINT ( 'NONE',  ( 6.825078400183575589, -0.005632053428735600553, 2.144262460745151255 ) ) ;
#25454 = CIRCLE ( 'NONE', #73857, 0.08000000000000020983 ) ;
#25453 = CARTESIAN_POINT ( 'NONE',  ( 0.2335756976950612018, -1.975703151049061024, 0.8776370805363906680 ) ) ;
#25455 = CARTESIAN_POINT ( 'NONE',  ( 1.867985033921132798, 1.011920226373051346, 1.691812110196472041 ) ) ;
#25456 = EDGE_CURVE ( 'NONE', #137116, #117552, #127649, .T. ) ;
#25457 = AXIS2_PLACEMENT_3D ( 'NONE', #154990, #55353, #138751 ) ;
#25459 = CARTESIAN_POINT ( 'NONE',  ( -4.665414256878301025, 6.536345614481700927, -1.443375672974066548 ) ) ;
#25458 = CARTESIAN_POINT ( 'NONE',  ( 6.170165192347925931, 1.906784905861274693, -0.1475879885542986936 ) ) ;
#25460 = CARTESIAN_POINT ( 'NONE',  ( -5.655159470231558849, 6.730679149092498648, 1.082531754730549078 ) ) ;
#25461 = CARTESIAN_POINT ( 'NONE',  ( 6.900173834712277632, 7.014900660111269559, -0.7998128361456341429 ) ) ;
#25462 = CARTESIAN_POINT ( 'NONE',  ( -6.414942957921379474, 7.513130201443591005, -1.199719254218452047 ) ) ;
#25463 = CARTESIAN_POINT ( 'NONE',  ( 1.858075313305072473, 0.7708903827231723405, -1.866970155298973921 ) ) ;
#25464 = CARTESIAN_POINT ( 'NONE',  ( 0.000000000000000000, 1.000000000000000888, 0.000000000000000000 ) ) ;
#25465 = CARTESIAN_POINT ( 'NONE',  ( 5.262836394871557744, -1.675821390925121168, 1.586616667910417888 ) ) ;
#25466 = DIRECTION ( 'NONE',  ( 0.6507913734559640506, -0.7592566023653004592, 0.000000000000000000 ) ) ;
#25467 = CARTESIAN_POINT ( 'NONE',  ( 2.518345088137901477, 0.8342845254802437882, 1.775630740545742992 ) ) ;
#25468 = CARTESIAN_POINT ( 'NONE',  ( 8.178592977541601527, 10.56477777859713463, 1.599625672291281386 ) ) ;
#25469 = CARTESIAN_POINT ( 'NONE',  ( 0.4049229342097167006, -1.081068455937021611, -1.701946057285643965 ) ) ;
#25471 = EDGE_LOOP ( 'NONE', ( #210146, #172802, #118346, #135873 ) ) ;
#25470 = B_SPLINE_CURVE_WITH_KNOTS ( 'NONE', 3,
 ( #6293, #54004, #120142, #106008, #172029, #3084, #23622, #37753, #103827, #169875, #87574 ),
 .UNSPECIFIED., .F., .F.,
 ( 4, 1, 1, 1, 1, 1, 1, 1, 4 ),
 ( 0.000000000000000000, 0.2256777920876190668, 0.3978457394851813711, 0.5256768607792676740, 0.6183602023682204241, 0.6850295134299612121, 0.7345374503969632762, 0.7752450576501028756, 1.000000000000000000 ),
 .UNSPECIFIED. ) ;
#25472 = CARTESIAN_POINT ( 'NONE',  ( 1.798220840057991543, -1.003180963283013982, -1.864648404631663148 ) ) ;
#25474 = CARTESIAN_POINT ( 'NONE',  ( -5.585069213825653023, 8.603332285183535433, -1.199719254218440723 ) ) ;
#25473 = CARTESIAN_POINT ( 'NONE',  ( -3.704402285031864306, 5.344888637335695414, -1.599625672291256295 ) ) ;
#25475 = CARTESIAN_POINT ( 'NONE',  ( 1.956743257466783570, 0.3155556147324266036, -1.813728304320901596 ) ) ;
#25476 = VERTEX_POINT ( 'NONE', #114570 ) ;
#25477 = CARTESIAN_POINT ( 'NONE',  ( -9.622536337397040285, 12.24937836509514710, 1.599625672291281386 ) ) ;
#25478 = CARTESIAN_POINT ( 'NONE',  ( 10.26598409777793464, 10.85580239508950307, 6.219453420784894604 ) ) ;
#25480 = EDGE_CURVE ( 'NONE', #132967, #180190, #165376, .T. ) ;
#25479 = CARTESIAN_POINT ( 'NONE',  ( 3.094099843433151253, 1.348383549611749332, 1.636666742212993686 ) ) ;
#25481 = CARTESIAN_POINT ( 'NONE',  ( 0.5328340850149284602, -1.300071877079148841, -1.303948673260245439 ) ) ;
#25482 = CARTESIAN_POINT ( 'NONE',  ( -1.500000000000013101, 4.160416667349482900, -0.8660254037844313801 ) ) ;
#25483 = CARTESIAN_POINT ( 'NONE',  ( 6.968000882419564945, 10.21675256520979858, 1.199719254218460707 ) ) ;
#25484 = CARTESIAN_POINT ( 'NONE',  ( 6.526270840131753737, 8.707344961610770540, -1.599625672291283607 ) ) ;
#25485 = CARTESIAN_POINT ( 'NONE',  ( 4.165347332011271497, 0.2559277237221342371, -2.044777286818760142 ) ) ;
#25487 = CARTESIAN_POINT ( 'NONE',  ( 0.8723036553972834950, -0.04505207493780280514, -1.840872848514919502 ) ) ;
#25486 = CARTESIAN_POINT ( 'NONE',  ( -8.525379664894808585, 8.840697785332414682, -0.7998128361456291469 ) ) ;
#25488 = CARTESIAN_POINT ( 'NONE',  ( -1.364683531249997417, 4.509375000341424133, 1.214306433183764966E-14 ) ) ;
#25489 = CARTESIAN_POINT ( 'NONE',  ( -0.02224634325198419221, -0.007204097619508199532, -2.289079630542793620 ) ) ;
#25490 = CARTESIAN_POINT ( 'NONE',  ( -1.536181705502190908, 8.701161256998856786, 2.509509933406568472 ) ) ;
#25491 = CARTESIAN_POINT ( 'NONE',  ( -0.1007326007324986367, -10.00000000000001243, -10.99953876047305812 ) ) ;
#25492 = CARTESIAN_POINT ( 'NONE',  ( 1.084930333755677045, -2.153824616689365978, -0.4803136671489223741 ) ) ;
#25493 = CARTESIAN_POINT ( 'NONE',  ( 3.813984095001612395, -2.229740912845196377, 0.3821933647679372492 ) ) ;
#25494 = CARTESIAN_POINT ( 'NONE',  ( -8.270110514656041190, 10.67154823856396817, 1.443375672974090751 ) ) ;
#25495 = CARTESIAN_POINT ( 'NONE',  ( 3.322321318109163979, -0.7387318680696324247, -1.654322230785286063 ) ) ;
#25496 = CARTESIAN_POINT ( 'NONE',  ( 2.676846564686267804, 1.640678131122888406, -0.9888057999517668728 ) ) ;
#25497 = CARTESIAN_POINT ( 'NONE',  ( 4.457524453155742528, 1.660904245173303373, 1.235824716467534889 ) ) ;
#25498 = CARTESIAN_POINT ( 'NONE',  ( 1.364683531249988535, 3.176041667008084435, 0.7879004041258500513 ) ) ;
#25499 = CARTESIAN_POINT ( 'NONE',  ( 2.922686454756417085, 1.855838157306726632, 0.6655703372969791198 ) ) ;
#25500 = CARTESIAN_POINT ( 'NONE',  ( 0.7801460289126905812, -1.072782840069667509, 1.599849161009530674 ) ) ;
#25501 = CARTESIAN_POINT ( 'NONE',  ( 4.416781281874038179, 1.710313510141375115, 0.7581657270378170388 ) ) ;
#25502 = CARTESIAN_POINT ( 'NONE',  ( 2.262750896497740527, 0.9887190084108381516, 2.085292768615305992 ) ) ;
#25503 = CARTESIAN_POINT ( 'NONE',  ( 3.631172916894987779, 0.04772338994715261129, -1.860622308654858559 ) ) ;
#25504 = CARTESIAN_POINT ( 'NONE',  ( -1.201851678989727383E-14, 4.696875000341419693, -1.575800808251660134 ) ) ;
#25505 = CARTESIAN_POINT ( 'NONE',  ( -5.111587607552082524, 5.922272616020886282, 1.199719254218450271 ) ) ;
#25506 = CARTESIAN_POINT ( 'NONE',  ( 6.124532705071213279, 8.168374127381657246, -1.599625672291262513 ) ) ;
#25507 = CARTESIAN_POINT ( 'NONE',  ( 0.7500000000000006661, 8.864583334016129967, 1.299038105676657340 ) ) ;
#25508 = EDGE_CURVE ( 'NONE', #95167, #213971, #63618, .T. ) ;
#25509 = CARTESIAN_POINT ( 'NONE',  ( 1.172648168047723649, -1.334858166028422222, 1.629009436104215558 ) ) ;
#25511 = CARTESIAN_POINT ( 'NONE',  ( -1.284279953904132077, 3.159610286488902187, -0.7749999999999935829 ) ) ;
#25510 = CARTESIAN_POINT ( 'NONE',  ( -1.201851678989727383E-14, 4.509375000341417916, -1.575800808251660134 ) ) ;
#25512 = CARTESIAN_POINT ( 'NONE',  ( 1.264911064067348656, 3.849999999999994316, 0.5000000000000064393 ) ) ;
#25513 = CARTESIAN_POINT ( 'NONE',  ( 2.637105894733019262, 1.998242115483703341, 0.7103459930332192140 ) ) ;
#25514 = CARTESIAN_POINT ( 'NONE',  ( 6.569012466128139494, -1.559778377529440929, 1.282785893457456750 ) ) ;
#25515 = CARTESIAN_POINT ( 'NONE',  ( 1.364683531249986537, 0.1552083336747499542, -0.7879004041258309554 ) ) ;
#25516 = CARTESIAN_POINT ( 'NONE',  ( -4.365362273920257330, 6.116008624372160973, 1.443375672974064550 ) ) ;
#25517 = CARTESIAN_POINT ( 'NONE',  ( 5.996784015946103885, 5.890669528225568996, 1.040834085586084257E-14 ) ) ;
#25518 = CARTESIAN_POINT ( 'NONE',  ( 1.089409339093825979, 1.906878951332368954, -1.017924135055588541 ) ) ;
#25521 = CARTESIAN_POINT ( 'NONE',  ( 5.178851490740207453, 5.144340948726102702, 0.7216878364870317197 ) ) ;
#25520 = CARTESIAN_POINT ( 'NONE',  ( 6.825078400183582694, 7.052760558784821221, 2.553807217019073761 ) ) ;
#25519 = CARTESIAN_POINT ( 'NONE',  ( 4.549643065837591038, 7.465611455855944101, -1.199719254218452047 ) ) ;
#25522 = CARTESIAN_POINT ( 'NONE',  ( -3.709037541790315640, 6.484905011134099340, -1.199719254218450271 ) ) ;
#25523 = CARTESIAN_POINT ( 'NONE',  ( 6.192592252150040721, 1.490973663936447258, -1.357864438797616868 ) ) ;
#25525 = CARTESIAN_POINT ( 'NONE',  ( -5.600926855776888758, 7.627776979863398310, -1.443375672974066548 ) ) ;
#25524 = CARTESIAN_POINT ( 'NONE',  ( -9.666600336863641729, 10.38004793587015584, 1.040834085586084257E-14 ) ) ;
#25526 = DIRECTION ( 'NONE',  ( -0.000000000000000000, -1.000000000000000000, 0.000000000000000000 ) ) ;
#25528 = CARTESIAN_POINT ( 'NONE',  ( -8.012344526598182026E-15, 10.54687500034139624, -1.575800808251669460 ) ) ;
#25527 = CARTESIAN_POINT ( 'NONE',  ( 0.1107634673921135821, -0.9696846621911526798, -2.041722876818732324 ) ) ;
#25529 = CARTESIAN_POINT ( 'NONE',  ( -8.448702279610222021, 13.00856975952063088, 1.040834085586084257E-14 ) ) ;
#25531 = CARTESIAN_POINT ( 'NONE',  ( -0.01814341541641998484, -1.915199053885572988, -0.04638162876333290496 ) ) ;
#25530 = CARTESIAN_POINT ( 'NONE',  ( -5.544921637864833386, 7.492161215640853023, -1.443375672974051449 ) ) ;
#25532 = CARTESIAN_POINT ( 'NONE',  ( -0.6823417656250003738, 0.5302083336747518416, -1.181850606188749264 ) ) ;
#25533 = CARTESIAN_POINT ( 'NONE',  ( 0.4382560683119193223, -5.166862915010159263, 10.99126615174921007 ) ) ;
#25534 = CARTESIAN_POINT ( 'NONE',  ( 11.94105721237522921, 11.02740390989733044, 1.187919463087248273 ) ) ;
#25535 = CARTESIAN_POINT ( 'NONE',  ( 2.982692045960423588, -0.1271664282922572997, -1.720251185527998272 ) ) ;
#25536 = CARTESIAN_POINT ( 'NONE',  ( 5.982890925380405456, 10.20206618957764100, 0.000000000000000000 ) ) ;
#25537 = CARTESIAN_POINT ( 'NONE',  ( 5.234329823327693809, 8.264412672927770487, 1.199719254218451159 ) ) ;
#25538 = CARTESIAN_POINT ( 'NONE',  ( 1.106321208856683613, 1.344927736385517658, -1.150416400790694960 ) ) ;
#25539 = AXIS2_PLACEMENT_3D ( 'NONE', #92231, #106371, #172394 ) ;
#25540 = CARTESIAN_POINT ( 'NONE',  ( 1.436190773529995468, -1.120142249841639348, -1.672479584328613988 ) ) ;
#25541 = CARTESIAN_POINT ( 'NONE',  ( 6.883263157960391787, -0.001104538646235289417, 1.946037152736757925 ) ) ;
#25542 = CARTESIAN_POINT ( 'NONE',  ( 4.383934217864794647, 1.438874268414831015, 1.673263306058408340 ) ) ;
#25543 = ORIENTED_EDGE ( 'NONE', *, *, #130359, .T. ) ;
#25544 = CARTESIAN_POINT ( 'NONE',  ( 8.446366511189332016, 9.916811020218137429, -1.082531754730543083 ) ) ;
#25546 = CARTESIAN_POINT ( 'NONE',  ( 3.163685574146878565, 1.281377625384312324, 1.556896677758594416 ) ) ;
#25545 = CARTESIAN_POINT ( 'NONE',  ( 3.774183692772983267, 2.104302197123971485, -0.2610650231627819062 ) ) ;
#25548 = ORIENTED_EDGE ( 'NONE', *, *, #147413, .T. ) ;
#25547 = CARTESIAN_POINT ( 'NONE',  ( 3.656362025717549535, 1.803379273073001388, 0.1719060212231597329 ) ) ;
#25549 = CARTESIAN_POINT ( 'NONE',  ( 4.441177836928239309, 7.339068688795062911, 1.199719254218452047 ) ) ;
#25550 = CARTESIAN_POINT ( 'NONE',  ( 1.885419139999934934, 1.287927767047766903, 1.356919574424742203 ) ) ;
#25551 = CARTESIAN_POINT ( 'NONE',  ( 3.192055101013606233, 5.811482486902795230, -1.199719254218446718 ) ) ;
#25552 = CARTESIAN_POINT ( 'NONE',  ( 5.953692858212231265, 0.5253669772854427933, -1.748464709795935157 ) ) ;
#25554 = CARTESIAN_POINT ( 'NONE',  ( 2.571384127028350175, 1.358050290760448364, 1.351446277617992076 ) ) ;
#25553 = CARTESIAN_POINT ( 'NONE',  ( -3.602716132929368875, 5.226254793216122074, 1.599625672291267398 ) ) ;
#25555 = CARTESIAN_POINT ( 'NONE',  ( -9.645406396194509568, 4.042443384815813445, -6.587269312116742270 ) ) ;
#25556 = FILL_AREA_STYLE_COLOUR ( '', #152593 ) ;
#25557 = CARTESIAN_POINT ( 'NONE',  ( -1.364683531250012516, 2.092708333674750953, 0.7879004041258379498 ) ) ;
#25558 = CARTESIAN_POINT ( 'NONE',  ( 0.6170404364503341288, -1.000000000000000888, -1.902435570468864690 ) ) ;
#25559 = VERTEX_POINT ( 'NONE', #49498 ) ;
#25560 = CARTESIAN_POINT ( 'NONE',  ( 5.872089928494542477, 9.864872326636710653, 0.000000000000000000 ) ) ;
#25561 = CARTESIAN_POINT ( 'NONE',  ( -3.363831509966360489, 6.938570838353784076, -0.7216878364870458196 ) ) ;
#25562 = CARTESIAN_POINT ( 'NONE',  ( -7.045397100956844127, 8.248660034984974132, -1.199719254218452047 ) ) ;
#25563 = CARTESIAN_POINT ( 'NONE',  ( 3.217144136595586179, 1.669276650691432495, -1.307696563879121143 ) ) ;
#25565 = CARTESIAN_POINT ( 'NONE',  ( -10.84558554699185784, 5.653278704827924273, 6.476092148523931336 ) ) ;
#25564 = CARTESIAN_POINT ( 'NONE',  ( -0.02988540731095785247, 0.7668091516429014209, -1.812018377701756888 ) ) ;
#25566 = CARTESIAN_POINT ( 'NONE',  ( 4.938727034960622930, 0.3341968672867478007, 1.942665651468850951 ) ) ;
#25567 = CARTESIAN_POINT ( 'NONE',  ( 0.2814942100668381131, 0.1933317163467423994, -2.003872996790170724 ) ) ;
#25568 = ORIENTED_EDGE ( 'NONE', *, *, #137968, .T. ) ;
#25569 = CARTESIAN_POINT ( 'NONE',  ( 0.4041146219485808877, -1.136702437883057470, -1.786057295064005013 ) ) ;
#25570 = DIRECTION ( 'NONE',  ( 1.000000000000000000, 0.000000000000000000, 0.000000000000000000 ) ) ;
#25571 = CARTESIAN_POINT ( 'NONE',  ( 1.504437137538238600, 2.067909592606699487, 0.1035681241481553605 ) ) ;
#25572 = CARTESIAN_POINT ( 'NONE',  ( 2.326030237553232016, 1.883725225384206281, 0.4715086074991140519 ) ) ;
#25573 = CARTESIAN_POINT ( 'NONE',  ( 6.150558962454855561, 7.204682206732687000, 1.199719254218452047 ) ) ;
#25574 = CARTESIAN_POINT ( 'NONE',  ( 5.417364897112183719, 8.477953592343014932, 1.199719254218451159 ) ) ;
#25576 = CARTESIAN_POINT ( 'NONE',  ( 4.171104814498611368, 8.018039383557042044, 0.7998128361456321445 ) ) ;
#25575 = CARTESIAN_POINT ( 'NONE',  ( 4.031257853796605062, -1.441737515256842572, -1.514218249133948868 ) ) ;
#25577 = CARTESIAN_POINT ( 'NONE',  ( 4.217995187182922656, 6.014356699837137832, 1.443375672974058777 ) ) ;
#25579 = EDGE_LOOP ( 'NONE', ( #160454, #171920, #134662, #83234 ) ) ;
#25578 = CARTESIAN_POINT ( 'NONE',  ( 0.3811517019768875802, 0.1791931900220759266, -1.802556192996515705 ) ) ;
#25580 = CARTESIAN_POINT ( 'NONE',  ( 5.567066847960510323, -1.993696164035433371, -0.9465883713010987410 ) ) ;
#25581 = DIRECTION ( 'NONE',  ( -0.000000000000000000, -1.000000000000000000, -0.000000000000000000 ) ) ;
#25582 = CARTESIAN_POINT ( 'NONE',  ( 4.419099417909471583, 2.016199240759775524, 0.8975180220924662278 ) ) ;
#25583 = CARTESIAN_POINT ( 'NONE',  ( 6.584456157731144899, 10.83361595066169514, -0.7998128361456291469 ) ) ;
#25584 = LINE ( 'NONE', #10399, #82369 ) ;
#25585 = CARTESIAN_POINT ( 'NONE',  ( 2.631394046745598736, -0.1854624247320437458, 1.903247139735386284 ) ) ;
#25586 = CARTESIAN_POINT ( 'NONE',  ( 7.411503528164766763, 11.79850454950093841, 1.040834085586084257E-14 ) ) ;
#25587 = CARTESIAN_POINT ( 'NONE',  ( 4.949704645232673172, 1.531818663031824013, 1.392983054852282132 ) ) ;
#25589 = CARTESIAN_POINT ( 'NONE',  ( 2.764712544972968811, -1.491509591961351910, 1.564943835847030229 ) ) ;
#25588 = CARTESIAN_POINT ( 'NONE',  ( -3.049795748596713985, 6.452024942755530290, 0.6608969203207606391 ) ) ;
#25590 = CARTESIAN_POINT ( 'NONE',  ( 4.388337494309430653, -0.4807229498768311182, -2.138019847805587403 ) ) ;
#25591 = CARTESIAN_POINT ( 'NONE',  ( 1.737500000000001155, -2.289583332377418401, 3.009438278150922130 ) ) ;
#25592 = CARTESIAN_POINT ( 'NONE',  ( 9.499766273075879397, -10.00000000000009592, -0.06663900456897582647 ) ) ;
#25593 = EDGE_CURVE ( 'NONE', #44776, #189774, #207435, .T. ) ;
#25594 = CARTESIAN_POINT ( 'NONE',  ( 4.061549535745618833, 6.896169004081968090, -1.199719254218452047 ) ) ;
#25595 = CARTESIAN_POINT ( 'NONE',  ( 3.285556943750000514, -2.501041666188708046, 1.896917185911906722 ) ) ;
#25596 = DIRECTION ( 'NONE',  ( -1.000000000000000000, 0.000000000000000000, 0.000000000000000000 ) ) ;
#25597 = PRESENTATION_LAYER_ASSIGNMENT (  '', '', ( #119060 ) ) ;
#25598 = CARTESIAN_POINT ( 'NONE',  ( -8.188761592974046266, 10.57664116326830595, -1.443375672974059665 ) ) ;
#25599 = CARTESIAN_POINT ( 'NONE',  ( 4.766573523656222555, 7.718696989977711809, 1.199719254218452047 ) ) ;
#25600 = CARTESIAN_POINT ( 'NONE',  ( 5.506714918851105089, 0.5956099481174789156, 1.982760374633622424 ) ) ;
#25601 = CARTESIAN_POINT ( 'NONE',  ( 4.406810040222974401, 1.488408744443140863, -1.223127719473691588 ) ) ;
#25602 = CARTESIAN_POINT ( 'NONE',  ( 0.1226730236999207246, 0.3474926252081366185, 1.986097365194151809 ) ) ;
#25603 = AXIS2_PLACEMENT_3D ( 'NONE', #93759, #7126, #173952 ) ;
#25604 = CARTESIAN_POINT ( 'NONE',  ( -9.001723924469462901, 12.58942944760136484, -1.199719254218446718 ) ) ;
#25605 = CARTESIAN_POINT ( 'NONE',  ( 7.693325821111733021, 7.940244644243982464, -0.7998128361456341429 ) ) ;
#25606 = FACE_OUTER_BOUND ( 'NONE', #54529, .T. ) ;
#25607 = CARTESIAN_POINT ( 'NONE',  ( 0.7092355107721182161, -0.3178641103029449799, 2.168156088950490723 ) ) ;
#25608 = CARTESIAN_POINT ( 'NONE',  ( 5.619710272201024814, -1.780234218580947436, 0.4041525643716862848 ) ) ;
#25609 = EDGE_CURVE ( 'NONE', #102463, #142570, #114138, .T. ) ;
#25610 = CARTESIAN_POINT ( 'NONE',  ( 5.641601317062233001, 7.675230518029648508, -1.443375672974078761 ) ) ;
#25611 = CARTESIAN_POINT ( 'NONE',  ( 2.345197385039651472, 5.679888015947478941, -0.7216878364870267237 ) ) ;
#25612 = CARTESIAN_POINT ( 'NONE',  ( -5.818384198920079520, 6.817144982608731141, 1.199719254218452935 ) ) ;
#25613 = CARTESIAN_POINT ( 'NONE',  ( 4.030516805012513082, 7.924296382481737844, 0.000000000000000000 ) ) ;
#25614 = ORIENTED_EDGE ( 'NONE', *, *, #85807, .T. ) ;
#25616 = CARTESIAN_POINT ( 'NONE',  ( 6.170187344554162401, 2.007508049254663529, -0.1525455265532823512 ) ) ;
#25615 = CARTESIAN_POINT ( 'NONE',  ( 2.348939331405873077, 0.4892633877765646400, -1.774999737812533063 ) ) ;
#25617 = CARTESIAN_POINT ( 'NONE',  ( 0.6503308509665306492, -0.2843267121918050533, -2.280655268134044622 ) ) ;
#25618 = CARTESIAN_POINT ( 'NONE',  ( 6.666857073735664052, 1.455856877570886887, -1.315125143065517532 ) ) ;
#25619 = CARTESIAN_POINT ( 'NONE',  ( -5.880485940025243607, 7.883652901494672349, 1.599625672291269396 ) ) ;
#25620 = CARTESIAN_POINT ( 'NONE',  ( -5.674335135020206700, 6.369890614947046892, -0.8991698295912193828 ) ) ;
#25621 = CARTESIAN_POINT ( 'NONE',  ( -2.774614992291035698, 6.388801257648172971, 1.040834085586084257E-14 ) ) ;
#25622 = CARTESIAN_POINT ( 'NONE',  ( 0.7310241076574041097, -1.948878508384953356, -0.6990896207654460071 ) ) ;
#25623 = CARTESIAN_POINT ( 'NONE',  ( -4.285259070371116863, 7.157163461145040095, 1.199719254218452935 ) ) ;
#25625 = CARTESIAN_POINT ( 'NONE',  ( 0.7955152940811484052, -0.6771210053572243037, 1.743984199989514927 ) ) ;
#25624 = CARTESIAN_POINT ( 'NONE',  ( 2.489882245090881963, -2.085347646507927699, -0.1508444384941027561 ) ) ;
#25626 = CARTESIAN_POINT ( 'NONE',  ( 1.809922493048341297, -1.704678386728165185, 1.076150803433255865 ) ) ;
#25627 = VERTEX_POINT ( 'NONE', #162197 ) ;
#25628 = CARTESIAN_POINT ( 'NONE',  ( 0.6823417656249899377, 3.738541667008085767, -1.181850606188754593 ) ) ;
#25629 = CARTESIAN_POINT ( 'NONE',  ( 2.173056921186319546, 1.071630648972416333, 1.371277206274525096 ) ) ;
#25630 = CARTESIAN_POINT ( 'NONE',  ( 4.137209430464448445, 7.978494768850520558, 1.040834085586084257E-14 ) ) ;
#25632 = CARTESIAN_POINT ( 'NONE',  ( 1.501328131443582459, 8.653248444470666101, 2.562127481693529774 ) ) ;
#25631 = CARTESIAN_POINT ( 'NONE',  ( -6.661184041422474778, -7.645986912801312485, 6.773376349081643433 ) ) ;
#25633 = CARTESIAN_POINT ( 'NONE',  ( 2.578358533787118212, -1.650418691300073570, -0.5013113332296408320 ) ) ;
#25634 = CARTESIAN_POINT ( 'NONE',  ( 3.034921719543516971, -1.931671641359738567, 1.035203715903771915 ) ) ;
#25635 = CARTESIAN_POINT ( 'NONE',  ( 5.444034239667132624, 0.8972360612293399651, -2.016436982482258333 ) ) ;
#25636 = CARTESIAN_POINT ( 'NONE',  ( -11.73097396203126763, 4.534521666694462105, -5.066462175338618756 ) ) ;
#25637 = CARTESIAN_POINT ( 'NONE',  ( 2.659224658930594121, 1.746150167319389990, -1.290005652201154263 ) ) ;
#25638 = CARTESIAN_POINT ( 'NONE',  ( 1.312830284664792790, 1.609138963534262778, 0.8624270714618911260 ) ) ;
#25639 = CARTESIAN_POINT ( 'NONE',  ( 3.960252432329254724, -1.215859836287141116, 1.733281388416860525 ) ) ;
#25640 = DIRECTION ( 'NONE',  ( -1.000000000000000000, 0.000000000000000000, 0.000000000000000000 ) ) ;
#25641 = EDGE_CURVE ( 'NONE', #16921, #112218, #141773, .T. ) ;
#25642 = ORIENTED_EDGE ( 'NONE', *, *, #19150, .T. ) ;
#25644 = CARTESIAN_POINT ( 'NONE',  ( -1.402160292154681736E-14, 0.7593750003414168059, -1.575800808251659024 ) ) ;
#25643 = CARTESIAN_POINT ( 'NONE',  ( 3.738036193864560541, 2.281383974799616521, 0.2239769770701737495 ) ) ;
#25645 = CARTESIAN_POINT ( 'NONE',  ( 11.09999999999960707, -2.070930125360890341E-15, 0.2598076211376220135 ) ) ;
#25646 = CARTESIAN_POINT ( 'NONE',  ( 5.217190183160311356, 4.981143389975473568, -0.7998128361456211532 ) ) ;
#25647 = CARTESIAN_POINT ( 'NONE',  ( 5.637407045567618624, -0.05664847855723317838, 2.220727194027871665 ) ) ;
#25648 = CARTESIAN_POINT ( 'NONE',  ( -6.914295153289458540, 7.169025221700239925, 0.7216878364870317197 ) ) ;
#25649 = CARTESIAN_POINT ( 'NONE',  ( 3.877268743828270470, 5.546566172598190292, 1.443375672974062551 ) ) ;
#25650 = CARTESIAN_POINT ( 'NONE',  ( -5.382223794500835545, 8.262716279350872384, -1.082531754730543971 ) ) ;
#25651 = CARTESIAN_POINT ( 'NONE',  ( 4.909461021924256485, 4.900328411765999981, 0.7216878364870338292 ) ) ;
#25652 = CIRCLE ( 'NONE', #15286, 3.099999999999999201 ) ;
#25653 = VERTEX_POINT ( 'NONE', #211978 ) ;
#25654 = CARTESIAN_POINT ( 'NONE',  ( 4.606092368833686557, -0.09613688574180989654, 2.014232646917232916 ) ) ;
#25656 = CARTESIAN_POINT ( 'NONE',  ( 3.748931555198372845, -0.3975983499134613242, -2.023727603370987449 ) ) ;
#25655 = CARTESIAN_POINT ( 'NONE',  ( 6.908042961362778733, 8.018137195466769285, 1.199719254218462483 ) ) ;
#25657 = CARTESIAN_POINT ( 'NONE',  ( 5.806634928402749196, 9.996434193103704402, -0.7998128361456481317 ) ) ;
#25658 = ADVANCED_FACE ( 'NONE', ( #13784 ), #129773, .T. ) ;
#25659 = CARTESIAN_POINT ( 'NONE',  ( 3.838366886000300404, 6.531826229425389485, -1.082531754730548412 ) ) ;
#25660 = CARTESIAN_POINT ( 'NONE',  ( 1.642778471875000035, -2.676041666188708756, -2.845375778867859751 ) ) ;
#25661 = CARTESIAN_POINT ( 'NONE',  ( 5.947271710577298087, 0.6394180277670692414, -2.096098967930816848 ) ) ;
#25662 = CARTESIAN_POINT ( 'NONE',  ( 3.445935549842124690, -1.779626424299302956, -0.9480406757386842242 ) ) ;
#25663 = CARTESIAN_POINT ( 'NONE',  ( 3.684953445348177148, 1.336164438771630714, 1.267087564277062484 ) ) ;
#25664 = EDGE_CURVE ( 'NONE', #137788, #204338, #113506, .T. ) ;
#25665 = CARTESIAN_POINT ( 'NONE',  ( 6.470265622219697477, 8.571729197388226140, -1.599625672291262513 ) ) ;
#25666 = FILL_AREA_STYLE ('',( #7270 ) ) ;
#25667 = CARTESIAN_POINT ( 'NONE',  ( 6.422862827026682098, 1.704596635199370880, 0.6539724957527744964 ) ) ;
#25668 = CARTESIAN_POINT ( 'NONE',  ( 0.1769827672329090662, 1.709356359883105636, 1.537109589704383827 ) ) ;
#25669 = CARTESIAN_POINT ( 'NONE',  ( -6.958359152311683893, 9.141171649162195934, -1.599625672291263179 ) ) ;
#25670 = CARTESIAN_POINT ( 'NONE',  ( 0.5095019425028306514, 1.969206903598280212, 1.113800330609107103 ) ) ;
#25671 = CARTESIAN_POINT ( 'NONE',  ( 1.541775746491366395, -1.526411702840410722, -1.451317155924846336 ) ) ;
#25672 = CARTESIAN_POINT ( 'NONE',  ( -5.315678745009726924, 8.359319748223434487, -1.199719254218453823 ) ) ;
#25673 = CARTESIAN_POINT ( 'NONE',  ( 9.264299036839600987, 9.702770385934682551, -0.7998128361456281477 ) ) ;
#25674 = CARTESIAN_POINT ( 'NONE',  ( 5.668717623845194176, 9.627604637879139560, 0.000000000000000000 ) ) ;
#25675 = SHAPE_REPRESENTATION_RELATIONSHIP ( 'NONE' , 'NONE' ,  #149737, #47143 ) ;
#25676 = CARTESIAN_POINT ( 'NONE',  ( -8.037286134802835491, 8.271255333558444889, -0.7998128361456291469 ) ) ;
#25677 = CARTESIAN_POINT ( 'NONE',  ( 7.362820735712755749, -5.796536394784340018, 7.362820735709910025 ) ) ;
#25678 = CARTESIAN_POINT ( 'NONE',  ( 8.242994206984347372, 8.719174117677642499, 1.040834085586084257E-14 ) ) ;
#25679 = CARTESIAN_POINT ( 'NONE',  ( 3.999262108721039155, 7.828827674157968985, 0.07552679838754294828 ) ) ;
#25680 = CARTESIAN_POINT ( 'NONE',  ( -4.599240423533815125, 6.388866465587984322, 1.599625672291267398 ) ) ;
#25681 = CARTESIAN_POINT ( 'NONE',  ( 3.586370468055916305, 1.236567345028506182, 1.845233891176313756 ) ) ;
#25682 = CARTESIAN_POINT ( 'NONE',  ( 1.377182423176852133, 2.023737929115625445, -0.8412682346608522099 ) ) ;
#25683 = CARTESIAN_POINT ( 'NONE',  ( 0.2412292383832773390, 0.3817025157030576321, 2.173470055567463088 ) ) ;
#25684 = CARTESIAN_POINT ( 'NONE',  ( -5.472651281771599763, 6.413789912602166687, 1.199719254218452935 ) ) ;
#25685 = PRODUCT_RELATED_PRODUCT_CATEGORY ( 'part', '', ( #207916 ) ) ;
#25686 = CARTESIAN_POINT ( 'NONE',  ( 4.896903505236655185, 0.3334610245491422265, 1.933150054703360432 ) ) ;
#25687 = CARTESIAN_POINT ( 'NONE',  ( 7.716561984472250835, 12.15440608185967086, 1.040834085586084257E-14 ) ) ;
#25688 = CARTESIAN_POINT ( 'NONE',  ( -5.076477019373391464, 6.555905325687263030, 1.224675693024103174 ) ) ;
#25689 = DIRECTION ( 'NONE',  ( 5.329070518200750605E-15, 0.000000000000000000, 1.000000000000000000 ) ) ;
#25690 = CARTESIAN_POINT ( 'NONE',  ( 1.364683531249986537, 1.113541667008082658, 0.7879004041258500513 ) ) ;
#25691 = CARTESIAN_POINT ( 'NONE',  ( -3.201133666602369310, 6.748756687762456963, -0.7216878364870458196 ) ) ;
#25693 = EDGE_LOOP ( 'NONE', ( #208329, #166933, #49311, #196295 ) ) ;
#25692 = CARTESIAN_POINT ( 'NONE',  ( -6.724481002698138532, 6.947575379343695623, -0.7216878364870278340 ) ) ;
#25694 = CARTESIAN_POINT ( 'NONE',  ( 3.656581996618038843, 2.110704406498860486, 0.2042969539849878724 ) ) ;
#25695 = CARTESIAN_POINT ( 'NONE',  ( -4.309512724297390740, 6.121127159803966933, 1.599625672291270506 ) ) ;
#25696 = CARTESIAN_POINT ( 'NONE',  ( 5.506754051192107369, 1.639644015412666800, -1.408845030788405506 ) ) ;
#25697 = CARTESIAN_POINT ( 'NONE',  ( 4.036529152626888717, -1.599951230533543045, 0.9111318136766359821 ) ) ;
#25698 = CARTESIAN_POINT ( 'NONE',  ( 5.419157771004846857, -1.820987890746316173, 0.8666037247077316152 ) ) ;
#25699 = CARTESIAN_POINT ( 'NONE',  ( -5.906331710381417466, 6.003565991635761989, -0.1321356564752910190 ) ) ;
#25700 = CARTESIAN_POINT ( 'NONE',  ( 0.6823417656249899377, 1.405208333674752508, 1.181850606188755259 ) ) ;
#25701 = CARTESIAN_POINT ( 'NONE',  ( -0.1298852118744100725, 0.003815113116375101580, -1.726395881205537330 ) ) ;
#25702 = CARTESIAN_POINT ( 'NONE',  ( 6.827182134110205247, 0.5943742033862747798, 1.864010940340610212 ) ) ;
#25703 = CARTESIAN_POINT ( 'NONE',  ( 4.039966587192267866, 4.776011108888172707, 1.082531754730560403 ) ) ;
#25704 = CARTESIAN_POINT ( 'NONE',  ( 11.08642519832315543, 7.950771188443131798, 4.613362863501950351 ) ) ;
#25705 = CARTESIAN_POINT ( 'NONE',  ( 3.959979445722985325, 2.145676688911036578, -0.2621329562078680842 ) ) ;
#25706 = CLOSED_SHELL ( 'NONE', ( #152368, #37246, #160190, #54459, #73787, #9068, #152261, #169109, #51527, #213750 ) ) ;
#25707 = CARTESIAN_POINT ( 'NONE',  ( 5.958361200765043719, 1.524811557412728114, 1.319025083221535333 ) ) ;
#25708 = CARTESIAN_POINT ( 'NONE',  ( -7.659993601596710278, 10.92011438762942355, -1.082531754730543083 ) ) ;
#25709 = CARTESIAN_POINT ( 'NONE',  ( 3.995124980148881288, 1.827535992889782523, -1.154293374375232828 ) ) ;
#25710 = CARTESIAN_POINT ( 'NONE',  ( 3.479716606839049930, 1.247861786229450543, 1.526166498753677825 ) ) ;
#25711 = CARTESIAN_POINT ( 'NONE',  ( -2.173285075505815599E-15, -8.011313137147263674, 11.00000000000000178 ) ) ;
#25712 = CARTESIAN_POINT ( 'NONE',  ( 0.9917865004017255570, 2.033541294120873033, -1.090684920485317733 ) ) ;
#25713 = CARTESIAN_POINT ( 'NONE',  ( 2.671226777604285729, 0.1043416919609811144, -2.058284026376159925 ) ) ;
#25714 = CARTESIAN_POINT ( 'NONE',  ( 5.425317942119275649, -1.235012148030777412, -1.498765763798795891 ) ) ;
#25716 = ORIENTED_EDGE ( 'NONE', *, *, #8288, .F. ) ;
#25715 = CARTESIAN_POINT ( 'NONE',  ( -6.656690234185426824, 10.70996300661758660, 0.7216878364870458196 ) ) ;
#25717 = CARTESIAN_POINT ( 'NONE',  ( -6.794571259104023930, 7.956029886156682274, 1.199719254218452047 ) ) ;
#25718 = CARTESIAN_POINT ( 'NONE',  ( 6.938893903907228378E-15, 10.64264068711930733, 1.214306433183764966E-14 ) ) ;
#25720 = ORIENTED_EDGE ( 'NONE', *, *, #151802, .F. ) ;
#25719 = CARTESIAN_POINT ( 'NONE',  ( -5.815521545619021460, 5.749472989502435460, -0.7998128361456362523 ) ) ;
#25721 = CARTESIAN_POINT ( 'NONE',  ( -6.521108698048772467, 9.591415333490143524, -1.082531754730537976 ) ) ;
#25722 = CARTESIAN_POINT ( 'NONE',  ( 2.784424029790978139, -1.135345490304447091, 1.892179603154810597 ) ) ;
#25723 = CARTESIAN_POINT ( 'NONE',  ( -1.642778471874998480, -0.4010416661887096224, 2.845375778867863303 ) ) ;
#25724 = CARTESIAN_POINT ( 'NONE',  ( 6.631700630569578259, 1.878258136613653040, -0.5663492180864730940 ) ) ;
#25725 = CARTESIAN_POINT ( 'NONE',  ( -0.1291982275798625457, 6.946856551170387029, -2.669038260222480918 ) ) ;
#25726 = CARTESIAN_POINT ( 'NONE',  ( -1.499999999999997780, 3.681250000682819046, 1.214306433183764966E-14 ) ) ;
#25728 = CARTESIAN_POINT ( 'NONE',  ( 11.89942855770813956, 9.719999999999998863, -0.7000000000000009548 ) ) ;
#25727 = CARTESIAN_POINT ( 'NONE',  ( -6.238615401616060652, 7.011456692927672485, -1.010807710288418981 ) ) ;
#25729 = CARTESIAN_POINT ( 'NONE',  ( 4.839718430358881385, 1.836437689789902405, 0.1323948491315785347 ) ) ;
#25730 = ORIENTED_EDGE ( 'NONE', *, *, #25801, .F. ) ;
#25731 = CARTESIAN_POINT ( 'NONE',  ( 2.131779597171743923, -1.345384690298248698, -1.561254108789570827 ) ) ;
#25732 = CARTESIAN_POINT ( 'NONE',  ( -3.956095110007852622E-14, 0.3281250003414356020, -1.570758158831788265 ) ) ;
#25733 = CARTESIAN_POINT ( 'NONE',  ( -7.379715684540041565, 7.504089808251839244, 1.040834085586084257E-14 ) ) ;
#25734 = CARTESIAN_POINT ( 'NONE',  ( 10.91812205866965613, -9.932868363016993385, -0.1856806763506236857 ) ) ;
#25737 = EDGE_CURVE ( 'NONE', #142577, #195087, #89960, .T. ) ;
#25736 =( GEOMETRIC_REPRESENTATION_CONTEXT ( 3 ) GLOBAL_UNCERTAINTY_ASSIGNED_CONTEXT ( ( #79765 ) ) GLOBAL_UNIT_ASSIGNED_CONTEXT ( ( #187316, #184111, #2139 ) ) REPRESENTATION_CONTEXT ( 'NONE', 'WORKASPACE' ) );
#25735 = CARTESIAN_POINT ( 'NONE',  ( -1.499999999999993339, 10.64264068711930733, 1.232676135170975238E-14 ) ) ;
#25738 = CARTESIAN_POINT ( 'NONE',  ( 3.811813743736467419, 7.598866467667865443, 1.040834085586084257E-14 ) ) ;
#25739 = CARTESIAN_POINT ( 'NONE',  ( 1.164996006578455923, -1.862832630767555120, -0.8818606138344189382 ) ) ;
#25740 = CARTESIAN_POINT ( 'NONE',  ( 4.458453498679889826, -1.646799808365447149, -0.8236825204945982248 ) ) ;
#25741 = CARTESIAN_POINT ( 'NONE',  ( 6.123478934866503742, 10.29580919065294431, 0.7998128361456462443 ) ) ;
#25742 = CARTESIAN_POINT ( 'NONE',  ( 1.523611765266693396, 0.5999999999999998668, -1.789163823896769978 ) ) ;
#25743 = CARTESIAN_POINT ( 'NONE',  ( -4.471156797456668386, 8.438376373666578445, -0.7998128361456362523 ) ) ;
#25745 = ORIENTED_EDGE ( 'NONE', *, *, #151879, .F. ) ;
#25744 = CARTESIAN_POINT ( 'NONE',  ( 6.610000000000022524, 3.695490760540712127, 2.514297579034238783 ) ) ;
#25746 = CARTESIAN_POINT ( 'NONE',  ( 4.951907052881864502, 0.6945806438464275923, -2.094803410698709900 ) ) ;
#25747 = CARTESIAN_POINT ( 'NONE',  ( 6.802048716365778347, -2.262122309816359422, 0.04523717395405778968 ) ) ;
#25748 = CARTESIAN_POINT ( 'NONE',  ( -4.744990575102892905, 8.479646737687938085, 0.7216878364870458196 ) ) ;
#25749 = CARTESIAN_POINT ( 'NONE',  ( 0.1582721923853447621, 1.907395734848855051, 0.1385995803297388196 ) ) ;
#25750 = CARTESIAN_POINT ( 'NONE',  ( 6.350803879971770982, -1.754615558991738267, -0.7693843322766678039 ) ) ;
#25751 = CARTESIAN_POINT ( 'NONE',  ( -4.543684818008837389, 5.386939200858302357, 1.243851604716961212 ) ) ;
#25752 = CARTESIAN_POINT ( 'NONE',  ( 0.07536363704235565786, 7.629137130509072051, -2.744199452819145346 ) ) ;
#25753 = ADVANCED_FACE ( 'NONE', ( #83050 ), #115618, .T. ) ;
#25754 = CARTESIAN_POINT ( 'NONE',  ( 5.865855438783554199, 0.5507134639845880919, -1.831277125143706774 ) ) ;
#25755 = AXIS2_PLACEMENT_3D ( 'NONE', #134614, #68487, #171339 ) ;
#25756 = CARTESIAN_POINT ( 'NONE',  ( 0.4263524580605422276, 1.788790299270696993, 0.5473224044415525569 ) ) ;
#25757 = CARTESIAN_POINT ( 'NONE',  ( 2.747280062631300535, 0.2910806042949847239, -1.995268371848608835 ) ) ;
#25759 = CARTESIAN_POINT ( 'NONE',  ( 3.914754834457169874, 1.489469167258972382, -1.489228550157334574 ) ) ;
#25758 = CARTESIAN_POINT ( 'NONE',  ( -8.690940161559884913, 10.09818392903003748, 1.199719254218462483 ) ) ;
#25760 = AXIS2_PLACEMENT_3D ( 'NONE', #7193, #5047, #154542 ) ;
#25761 = CARTESIAN_POINT ( 'NONE',  ( 6.923409998072794558, 11.22906209772695618, 1.040834085586084257E-14 ) ) ;
#25763 = CARTESIAN_POINT ( 'NONE',  ( -6.828502922777144768, 11.11833717654868892, 0.7998128361456481317 ) ) ;
#25762 = CARTESIAN_POINT ( 'NONE',  ( -1.500000000000015099, 0.1291666666666918539, -0.8660254037844383745 ) ) ;
#25764 = LINE ( 'NONE', #124437, #120535 ) ;
#25765 = CARTESIAN_POINT ( 'NONE',  ( 3.621357264417348620, 1.734514936435461507, 1.034602781942542515 ) ) ;
#25766 = CARTESIAN_POINT ( 'NONE',  ( -1.201851678989727383E-14, 4.196875000341417028, -1.575800808251660134 ) ) ;
#25767 = ADVANCED_FACE ( 'NONE', ( #28991 ), #155649, .T. ) ;
#25768 = CARTESIAN_POINT ( 'NONE',  ( 10.05978679165993839, 10.83876546646586014, 0.7216878364870438212 ) ) ;
#25769 = CARTESIAN_POINT ( 'NONE',  ( 4.235729478701364847, -1.487246874726022128, -1.568870776130903089 ) ) ;
#25770 = CARTESIAN_POINT ( 'NONE',  ( 5.905458427204159477, 9.047396044116986502, 1.199719254218452047 ) ) ;
#25771 = CARTESIAN_POINT ( 'NONE',  ( -1.500000000000011324, 5.670833333333358262, 0.8660254037844403729 ) ) ;
#25772 = CARTESIAN_POINT ( 'NONE',  ( 5.342795052237045539, 8.390955439988655229, -1.199719254218450271 ) ) ;
#25773 = CARTESIAN_POINT ( 'NONE',  ( 9.056483423804305488, 9.668244870634271848, 1.040834085586084257E-14 ) ) ;
#25775 = DIRECTION ( 'NONE',  ( -0.000000000000000000, -1.000000000000000000, -0.000000000000000000 ) ) ;
#25774 = CARTESIAN_POINT ( 'NONE',  ( 2.190095119440739424, -1.416971674389384761, -1.645159614449900776 ) ) ;
#25776 = AXIS2_PLACEMENT_3D ( 'NONE', #124553, #25879, #75712 ) ;
#25778 = CARTESIAN_POINT ( 'NONE',  ( 0.8195642880178370948, 1.096917009463085790, -1.478703137254427924 ) ) ;
#25777 = CARTESIAN_POINT ( 'NONE',  ( -7.076992996653451939, 7.358839372291564374, 0.7216878364870317197 ) ) ;
#25779 = CARTESIAN_POINT ( 'NONE',  ( -1.364683531250000748, 1.759375000341421913, 0.000000000000000000 ) ) ;
#25780 = CARTESIAN_POINT ( 'NONE',  ( 3.544632465004614374, -1.790652189326558563, 1.263247045326252094 ) ) ;
#25781 = CARTESIAN_POINT ( 'NONE',  ( 6.463880482550782958, 6.803305507656864037, -0.5117977836574041373 ) ) ;
#25782 = CARTESIAN_POINT ( 'NONE',  ( 3.485499699327331502, 2.046305154993263375, -0.9654624412855338234 ) ) ;
#25783 = CARTESIAN_POINT ( 'NONE',  ( -7.542413527904030524, 7.693903958843159252, 1.040834085586084257E-14 ) ) ;
#25784 = CARTESIAN_POINT ( 'NONE',  ( 4.592982591267942283, 1.756852934926198317, 0.9896879400849432074 ) ) ;
#25785 = CARTESIAN_POINT ( 'NONE',  ( 1.364683531249990311, 4.946875000341417916, 1.214306433183764966E-14 ) ) ;
#25786 = CARTESIAN_POINT ( 'NONE',  ( 6.326190869690321961, 6.855918622363850190, 0.6739092513716876676 ) ) ;
#25787 = CARTESIAN_POINT ( 'NONE',  ( -1.500000000000015099, 12.72916666666666963, -0.8660254037844309360 ) ) ;
#25788 = CARTESIAN_POINT ( 'NONE',  ( 6.753369913382843315, 8.011924666102361314, -1.082531754730548412 ) ) ;
#25789 =( BOUNDED_SURFACE ( )  B_SPLINE_SURFACE ( 3, 2, ( 
 ( #188804, #90252, #32701 ),
 ( #15366, #176827, #79323 ),
 ( #48970, #195213, #13252 ),
 ( #114037, #46849, #115087 ) ),
 .UNSPECIFIED., .F., .F., .F. ) 
 B_SPLINE_SURFACE_WITH_KNOTS ( ( 4, 4 ),
 ( 3, 3 ),
 ( 0.01090518310586315390, 0.01337341879808987347 ),
 ( 0.000000000000000000, 1.000000000000000000 ),
 .UNSPECIFIED. ) 
 GEOMETRIC_REPRESENTATION_ITEM ( )  RATIONAL_B_SPLINE_SURFACE ( (
 ( 1.000000000000000000, 0.6967468848055786701, 1.000000000000000000),
 ( 1.000000000000000000, 0.6961913616436842256, 1.000000000000000000),
 ( 1.000000000000000000, 0.6955505937921928616, 1.000000000000000000),
 ( 1.000000000000000000, 0.6947640035364115452, 1.000000000000000000) ) ) 
 REPRESENTATION_ITEM ( '' )  SURFACE ( )  );
#25790 = CARTESIAN_POINT ( 'NONE',  ( 4.446413189832159496, 0.4709973186826624802, 1.705850592114676489 ) ) ;
#25791 = CARTESIAN_POINT ( 'NONE',  ( 8.829384350997564468, 11.32403438096243775, 1.599625672291281386 ) ) ;
#25793 = AXIS2_PLACEMENT_3D ( 'NONE', #106055, #7412, #23671 ) ;
#25792 = CARTESIAN_POINT ( 'NONE',  ( 0.8683613728089655259, 1.037855563948440363, 1.832367646046024534 ) ) ;
#25795 = CARTESIAN_POINT ( 'NONE',  ( -0.7500000000000215383, 1.191666666666688190, 1.299038105676659116 ) ) ;
#25794 = CARTESIAN_POINT ( 'NONE',  ( -1.364683531250014514, 11.08854166700806410, -0.7879004041258335089 ) ) ;
#25796 = CARTESIAN_POINT ( 'NONE',  ( 0.8538788329778913555, -0.7122206123622039087, 1.836445260119154543 ) ) ;
#25797 = CARTESIAN_POINT ( 'NONE',  ( -5.659602779061863487, 5.567567761852417085, 0.7998128361456281477 ) ) ;
#25798 = CARTESIAN_POINT ( 'NONE',  ( 6.151970292378349470, 1.039009440890667824, 1.727993850779283580 ) ) ;
#25799 = ORIENTED_EDGE ( 'NONE', *, *, #75497, .T. ) ;
#25800 = CARTESIAN_POINT ( 'NONE',  ( 6.100805936469477331, 9.101062111647635788, -1.082531754730537088 ) ) ;
#25801 = EDGE_CURVE ( 'NONE', #201551, #8301, #179514, .T. ) ;
#25802 = CARTESIAN_POINT ( 'NONE',  ( 4.328871119428026049, 0.09166491666120352155, 1.868520897946590598 ) ) ;
#25803 = CARTESIAN_POINT ( 'NONE',  ( 4.399325512199628641, -1.803763729973751451, 1.015883459259236954 ) ) ;
#25804 = CARTESIAN_POINT ( 'NONE',  ( -0.6125000000000140332, 2.041666666666650087, 1.060881119635936232 ) ) ;
#25805 = CARTESIAN_POINT ( 'NONE',  ( -6.916067756302494374, 7.241369601873926420, 0.000000000000000000 ) ) ;
#25806 = CARTESIAN_POINT ( 'NONE',  ( -0.4019237886467001974, 10.83258545099816672, 1.500000000000001998 ) ) ;
#25807 = CARTESIAN_POINT ( 'NONE',  ( 9.101601193475611140, 9.512956235343358102, -0.7998128361456221525 ) ) ;
#25808 = CARTESIAN_POINT ( 'NONE',  ( -10.49131193887636826, 11.13428543831092909, 1.040834085586084257E-14 ) ) ;
#25809 = CARTESIAN_POINT ( 'NONE',  ( -4.226151626080061341, 7.204621842858783154, -0.9994034082375232719 ) ) ;
#25810 = CARTESIAN_POINT ( 'NONE',  ( 0.6823417656249917140, 5.655208333674749177, 1.181850606188765695 ) ) ;
#25811 = AXIS2_PLACEMENT_3D ( 'NONE', #6429, #103967, #72503 ) ;
#25812 = CARTESIAN_POINT ( 'NONE',  ( 4.088298575758734898, 1.051444423028622399, -1.656135347060924135 ) ) ;
#25813 = CARTESIAN_POINT ( 'NONE',  ( 1.827499746633702182, -1.427720486614523221, 1.423741782973136694 ) ) ;
#25814 = CARTESIAN_POINT ( 'NONE',  ( -3.851398154733808088, 6.650992392901508232, -1.199719254218450271 ) ) ;
#25815 = CARTESIAN_POINT ( 'NONE',  ( 0.4999999999999761302, 3.172938907704328404, 0.3999999999999750422 ) ) ;
#25816 = CARTESIAN_POINT ( 'NONE',  ( 1.264687732342294701, -1.688641954842164283, -0.8049673154429252131 ) ) ;
#25817 = CARTESIAN_POINT ( 'NONE',  ( 1.364683531249990311, 4.134375000341417028, 1.214306433183764966E-14 ) ) ;
#25818 = CARTESIAN_POINT ( 'NONE',  ( 2.707291822170342144, 1.724471752635655664, -1.038662168513148965 ) ) ;
#25820 = CARTESIAN_POINT ( 'NONE',  ( 3.673546786387419605, 1.535089753090538078, 1.458380203637131833 ) ) ;
#25819 = CARTESIAN_POINT ( 'NONE',  ( -5.531363484695544841, 8.436712584578003771, 1.082531754730548412 ) ) ;
#25821 = CARTESIAN_POINT ( 'NONE',  ( 0.000000000000000000, 0.000000000000000000, 0.000000000000000000 ) ) ;
#25822 = CARTESIAN_POINT ( 'NONE',  ( 5.195788487752976081, -1.461605715988937515, -1.466586839339318882 ) ) ;
#25823 = CARTESIAN_POINT ( 'NONE',  ( 6.047819040147648373, 9.213483425884394507, 1.199719254218452047 ) ) ;
#25825 = CARTESIAN_POINT ( 'NONE',  ( 6.720655732516665815, 7.629137130509056064, 2.773739711112707340 ) ) ;
#25824 = CARTESIAN_POINT ( 'NONE',  ( -0.1116087887279961222, -0.4605761454780517572, -2.046466910313152532 ) ) ;
#25827 = ORIENTED_EDGE ( 'NONE', *, *, #115899, .T. ) ;
#25826 = CARTESIAN_POINT ( 'NONE',  ( 5.420859398437725574, 1.687492901312273474, 0.6969783729503381542 ) ) ;
#25828 = CARTESIAN_POINT ( 'NONE',  ( 7.456094412511537151, 10.78619501698377370, 1.199719254218460707 ) ) ;
#25829 = DIRECTION ( 'NONE',  ( 0.000000000000000000, 0.000000000000000000, 1.000000000000000000 ) ) ;
#25830 = FACE_OUTER_BOUND ( 'NONE', #14130, .T. ) ;
#25831 = CARTESIAN_POINT ( 'NONE',  ( -11.55001508359621987, 4.031797291955615314, 5.408777164504234847 ) ) ;
#25832 = CARTESIAN_POINT ( 'NONE',  ( -0.6823417656250039265, 11.88020833367473017, -1.181850606188755259 ) ) ;
#25833 = CARTESIAN_POINT ( 'NONE',  ( 6.428373272941257710, -0.9058926715965059939, -1.684108486221975953 ) ) ;
#25834 = CARTESIAN_POINT ( 'NONE',  ( -8.483651433849100698, 10.92067931095586886, 1.599625672291269396 ) ) ;
#25835 =( BOUNDED_CURVE ( )  B_SPLINE_CURVE ( 3, ( #160689, #142342, #188911, #176941 ),
 .UNSPECIFIED., .F., .T. ) 
 B_SPLINE_CURVE_WITH_KNOTS ( ( 4, 4 ),
 ( 0.5000000000000001110, 1.000000000000000000 ),
 .UNSPECIFIED. ) 
 CURVE ( )  GEOMETRIC_REPRESENTATION_ITEM ( )  RATIONAL_B_SPLINE_CURVE ( ( 0.9999999999999998890, 0.3333333333333333703, 0.3333333333333335369, 1.000000000000000000 ) ) 
 REPRESENTATION_ITEM ( '' )  );
#25836 = CARTESIAN_POINT ( 'NONE',  ( 6.331821432781979730, 7.345878745455822312, -1.199719254218445830 ) ) ;
#25838 = B_SPLINE_CURVE_WITH_KNOTS ( 'NONE', 3,
 ( #116827, #182829, #168720, #114705, #34444, #100519, #115759, #131999, #135180, #86409 ),
 .UNSPECIFIED., .F., .F.,
 ( 4, 3, 3, 4 ),
 ( 0.000000000000000000, 4.502046072368877275E-05, 9.004093402560205887E-05, 0.0001800865003231008306 ),
 .UNSPECIFIED. ) ;
#25837 = CARTESIAN_POINT ( 'NONE',  ( -4.858757509019083543, 5.629766575900002401, -2.420000000000000373 ) ) ;
#25839 = DIRECTION ( 'NONE',  ( 8.638326563840814399E-31, 0.000000000000000000, 1.000000000000000000 ) ) ;
#25840 = EDGE_CURVE ( 'NONE', #212849, #9659, #156179, .T. ) ;
#25841 = CARTESIAN_POINT ( 'NONE',  ( 4.497554271431305040, 6.270232621468402989, -1.599625672291256295 ) ) ;
#25842 = ORIENTED_EDGE ( 'NONE', *, *, #173321, .F. ) ;
#25843 = CARTESIAN_POINT ( 'NONE',  ( -5.399890319992785237, 9.521898816625391504, 0.7998128361456291469 ) ) ;
#25844 = CARTESIAN_POINT ( 'NONE',  ( 5.167592292328679449, 1.356312711205298172, 1.492245250866150785 ) ) ;
#25845 = CARTESIAN_POINT ( 'NONE',  ( -4.199533704925234368, 7.510932310329544670, -0.9222493318717175370 ) ) ;
#25846 = CIRCLE ( 'NONE', #146962, 0.07999999999999994615 ) ;
#25847 = CARTESIAN_POINT ( 'NONE',  ( -6.452141306522730879, 6.789529044577018446, 0.3774816029595753353 ) ) ;
#25848 = CARTESIAN_POINT ( 'NONE',  ( -5.599154252763867134, 5.634694171087028636, 0.000000000000000000 ) ) ;
#25849 = CARTESIAN_POINT ( 'NONE',  ( 3.171717870593107058, 5.787755718078879674, -1.199719254218446718 ) ) ;
#25850 = CARTESIAN_POINT ( 'NONE',  ( 2.729305274051788022, 0.1014009245450513547, -1.966985261555218800 ) ) ;
#25851 = CARTESIAN_POINT ( 'NONE',  ( 3.937125189161301719, -1.678018027730580286, -1.117815418662113425 ) ) ;
#25852 = CARTESIAN_POINT ( 'NONE',  ( -8.518600588087975822, 8.832788862391110385, 1.040834085586084257E-14 ) ) ;
#25853 = CARTESIAN_POINT ( 'NONE',  ( 6.727182134110242906, 2.956326135258012577, 2.541581140702349195 ) ) ;
#25854 = CARTESIAN_POINT ( 'NONE',  ( 3.293114190187882429, 1.727671002657789057, 1.348082825637614279 ) ) ;
#25855 = CARTESIAN_POINT ( 'NONE',  ( 0.000000000000000000, 13.49999999999999822, 0.000000000000000000 ) ) ;
#25856 = CARTESIAN_POINT ( 'NONE',  ( 2.239170187357332420, -1.721643101494104044, 0.8643732543716446948 ) ) ;
#25857 = CARTESIAN_POINT ( 'NONE',  ( -6.970863535720637216, 11.28442455831609337, 0.7998128361456481317 ) ) ;
#25858 = CARTESIAN_POINT ( 'NONE',  ( 0.1333542156527660338, 2.021264325465597977, -2.461897275464264290 ) ) ;
#25859 = EDGE_CURVE ( 'NONE', #90338, #89251, #175631, .T. ) ;
#25860 = FILL_AREA_STYLE_COLOUR ( '', #6648 ) ;
#25861 = CARTESIAN_POINT ( 'NONE',  ( 7.365103760721646076, 9.615707025640515937, 1.599625672291281386 ) ) ;
#25862 = CARTESIAN_POINT ( 'NONE',  ( 3.960953433486789521, 7.772862772376584850, -0.7998128361456221525 ) ) ;
#25863 = CARTESIAN_POINT ( 'NONE',  ( -6.844216539294140311, -8.074889850123483370, 6.588752024304639576 ) ) ;
#25864 = CARTESIAN_POINT ( 'NONE',  ( 6.061904079085887354, 6.244845311787889486, 0.000000000000000000 ) ) ;
#25865 = ORIENTED_EDGE ( 'NONE', *, *, #200558, .F. ) ;
#25867 = CARTESIAN_POINT ( 'NONE',  ( 2.402991782874515092, -0.3463731968284866625, -1.982927098142922784 ) ) ;
#25866 = CARTESIAN_POINT ( 'NONE',  ( 5.917501325027624048, -1.028386522942719816, -1.527094029191010893 ) ) ;
#25868 = CARTESIAN_POINT ( 'NONE',  ( 4.675370021169432455, -0.9774931845568238797, -2.080278028362152032 ) ) ;
#25870 = CARTESIAN_POINT ( 'NONE',  ( 2.711566728334329213, 0.5015729494155155566, -1.791976956261555953 ) ) ;
#25869 = CARTESIAN_POINT ( 'NONE',  ( -0.02919842301648319441, 0.2290444945237135044, -2.107092690553781456 ) ) ;
#25871 = CARTESIAN_POINT ( 'NONE',  ( 8.025500584646550806, 8.327781868367935658, 0.000000000000000000 ) ) ;
#25872 = PLANE ( 'NONE',  #212739 ) ;
#25873 = CARTESIAN_POINT ( 'NONE',  ( -8.369460898337653276, 8.658792557682392754, 0.7998128361456462443 ) ) ;
#25874 = VECTOR ( 'NONE', #170169, 1000.000000000000000 ) ;
#25875 = CARTESIAN_POINT ( 'NONE',  ( -5.153507786970285665, 5.185049637652990207, -0.7216878364870338292 ) ) ;
#25876 = CARTESIAN_POINT ( 'NONE',  ( 5.636299653793654940, 0.4088526781071535887, 2.050197504659311942 ) ) ;
#25877 = CARTESIAN_POINT ( 'NONE',  ( 7.022760382198770301, 8.255937203062467589, -1.082531754730543083 ) ) ;
#25878 = ORIENTED_EDGE ( 'NONE', *, *, #201882, .F. ) ;
#25879 = DIRECTION ( 'NONE',  ( 0.000000000000000000, -1.000000000000000000, -1.804652791718263484E-16 ) ) ;
#25880 = CARTESIAN_POINT ( 'NONE',  ( -11.07131503167114772, 12.30000000000000071, 0.8043049353970799231 ) ) ;
#25881 = CARTESIAN_POINT ( 'NONE',  ( 6.305283062370508063, 1.438394668203015092, 0.9516435707833100777 ) ) ;
#25882 = CARTESIAN_POINT ( 'NONE',  ( -5.494078562035765501, 7.432844293840273231, -1.599625672291256295 ) ) ;
#25883 = CARTESIAN_POINT ( 'NONE',  ( 1.248208839261849112, 1.708581046602712039, -0.2955488178391346143 ) ) ;
#25884 = FILL_AREA_STYLE_COLOUR ( '', #26525 ) ;
#25885 = CYLINDRICAL_SURFACE ( 'NONE', #50193, 0.07999999999999954370 ) ;
#25886 = CARTESIAN_POINT ( 'NONE',  ( 10.62873463776380056, 11.29999999999999893, -3.200000000000001510 ) ) ;
#25887 = CARTESIAN_POINT ( 'NONE',  ( 5.963789030284865511, -0.5350816163755196531, 2.103975319158644552 ) ) ;
#25888 = CARTESIAN_POINT ( 'NONE',  ( 4.793472150574508817, 1.354911484294840429, 1.223852735664505698 ) ) ;
#25889 = CARTESIAN_POINT ( 'NONE',  ( 2.307404798597446849, -1.572557994556064154, -1.172606125687980061 ) ) ;
#25890 = SURFACE_STYLE_FILL_AREA ( #11773 ) ;
#25891 = CARTESIAN_POINT ( 'NONE',  ( -8.469039510030723861, 13.03229652834454733, 1.040834085586084257E-14 ) ) ;
#25892 = CARTESIAN_POINT ( 'NONE',  ( 7.618792255875527886, 10.97600916757510170, 1.199719254218460707 ) ) ;
#25893 = CARTESIAN_POINT ( 'NONE',  ( 3.158948766716848766, 0.5171890032967979556, 2.056314737185329644 ) ) ;
#25894 = CARTESIAN_POINT ( 'NONE',  ( -3.633221978782304351, 4.301475732409860697, -1.082531754730549967 ) ) ;
#25895 = CIRCLE ( 'NONE', #174689, 0.08000000000000040412 ) ;
#25896 = FACE_OUTER_BOUND ( 'NONE', #182085, .T. ) ;
#25897 = CARTESIAN_POINT ( 'NONE',  ( -4.553630449417391368, 6.998240405024593436, -1.173447104293420473 ) ) ;
#25898 = CARTESIAN_POINT ( 'NONE',  ( 1.041946221393402539, 1.387617377995558288, 1.536584593769604323 ) ) ;
#25900 = CARTESIAN_POINT ( 'NONE',  ( 1.364683531249986537, -1.073958332991911790, 0.7879004041258500513 ) ) ;
#25899 = FACE_OUTER_BOUND ( 'NONE', #53283, .T. ) ;
#25903 = EDGE_LOOP ( 'NONE', ( #170392, #57169, #22058, #203320 ) ) ;
#25902 = CARTESIAN_POINT ( 'NONE',  ( 3.528187740469524769, -2.188240134182100949, 0.3810097408954765119 ) ) ;
#25901 = AXIS2_PLACEMENT_3D ( 'NONE', #3190, #186225, #5313 ) ;
#25904 = CARTESIAN_POINT ( 'NONE',  ( 1.583111924021431305, -0.7688449931826674133, 2.166437542035759556 ) ) ;
#25906 = CARTESIAN_POINT ( 'NONE',  ( 6.280145880020024052, -1.141028152120068917, -1.718028578259041872 ) ) ;
#25905 = CARTESIAN_POINT ( 'NONE',  ( 8.432808358020004391, 12.78210081775797669, 0.7216878364870438212 ) ) ;
#25908 = CARTESIAN_POINT ( 'NONE',  ( -3.475000000000000533, -0.3791666666666649865, -2.006292185433948827 ) ) ;
#25907 = CARTESIAN_POINT ( 'NONE',  ( 3.715816618597135523, 6.492813934075403637, -1.199719254218453823 ) ) ;
#25909 = EDGE_CURVE ( 'NONE', #119587, #190223, #38499, .T. ) ;
#25910 = B_SPLINE_CURVE_WITH_KNOTS ( 'NONE', 3,
 ( #76817, #157031, #141873, #140804, #58449, #62696 ),
 .UNSPECIFIED., .F., .F.,
 ( 4, 2, 4 ),
 ( 0.000000000000000000, 0.0003778774010236166992, 0.0007557548020472333985 ),
 .UNSPECIFIED. ) ;
#25911 = CARTESIAN_POINT ( 'NONE',  ( -4.161989969715295778, 4.726297878971393196, 2.420000000000010587 ) ) ;
#25912 = CARTESIAN_POINT ( 'NONE',  ( -10.97058181929407716, -5.254568858751056837, 0.2903707658989288509 ) ) ;
#25913 = CARTESIAN_POINT ( 'NONE',  ( -10.68054077891638265, -8.644755361503008828, 0.1864295327644238942 ) ) ;
#25914 = ADVANCED_FACE ( 'NONE', ( #50563 ), #101442, .F. ) ;
#25915 = CARTESIAN_POINT ( 'NONE',  ( -0.2106725631050176961, 2.017899180269961956, -2.418275446281520136 ) ) ;
#25916 = CARTESIAN_POINT ( 'NONE',  ( 2.555303990735880770, 0.4627875540959677236, -1.661435987504814360 ) ) ;
#25917 = CARTESIAN_POINT ( 'NONE',  ( 2.536342520008515233, 0.6839386381054488595, 1.897109991223707937 ) ) ;
#25918 = CARTESIAN_POINT ( 'NONE',  ( 2.936492027000091376, -1.880918663215241926, -1.321213444053377373 ) ) ;
#25919 = CARTESIAN_POINT ( 'NONE',  ( 4.060077147624012284, 2.245929291707829289, -0.2719227649434445282 ) ) ;
#25920 = CARTESIAN_POINT ( 'NONE',  ( 5.584633104594088238, -2.054432100182907561, -0.4627632117069883089 ) ) ;
#25921 = CARTESIAN_POINT ( 'NONE',  ( -5.804299160426229953, 8.825413882922319431, -1.082531754730549967 ) ) ;
#25922 = CARTESIAN_POINT ( 'NONE',  ( 3.743183411477500222, -1.338374212114415762, -1.157953421578450381 ) ) ;
#25924 = CARTESIAN_POINT ( 'NONE',  ( 5.847306917912500346, 0.6688746937079934618, -2.192647164702413498 ) ) ;
#25923 = CARTESIAN_POINT ( 'NONE',  ( 4.882344714252594642, 4.868692719482363707, 0.000000000000000000 ) ) ;
#25925 = CARTESIAN_POINT ( 'NONE',  ( 5.173706384855800700, -1.019854773079221344, 1.532662130498331887 ) ) ;
#25926 = CARTESIAN_POINT ( 'NONE',  ( -4.783329267523015460, 4.474972321731942593, -0.7998128361456221525 ) ) ;
#25927 = UNCERTAINTY_MEASURE_WITH_UNIT (LENGTH_MEASURE( 1.000000000000000082E-05 ), #94783, 'distance_accuracy_value', 'NONE');
#25928 = CARTESIAN_POINT ( 'NONE',  ( 4.134873662043553111, 7.767843672452050541, -0.7216878364870197293 ) ) ;
#25929 = CARTESIAN_POINT ( 'NONE',  ( -1.201851678989727383E-14, 3.462500000000019895, 1.732050807568877637 ) ) ;
#25930 = CARTESIAN_POINT ( 'NONE',  ( 4.435597005726048536, 0.9382243502508281763, -1.980580373504265301 ) ) ;
#25931 = CARTESIAN_POINT ( 'NONE',  ( -4.634189577772691138, 4.300976017023221409, 1.214306433183764966E-14 ) ) ;
#25932 = CARTESIAN_POINT ( 'NONE',  ( 11.01135777277262306, 13.40000000000000036, -1.400000000000001910 ) ) ;
#25933 = CARTESIAN_POINT ( 'NONE',  ( 6.021949436824264978, 2.040384406434097464, -0.3501103912618847014 ) ) ;
#25934 = DIRECTION ( 'NONE',  ( 0.6507913734559658270, 0.7592566023652989049, 0.000000000000000000 ) ) ;
#25935 = CARTESIAN_POINT ( 'NONE',  ( 1.364683531249990311, 4.863541667008084879, 0.7879004041258500513 ) ) ;
#25936 = CARTESIAN_POINT ( 'NONE',  ( 3.439987180796261423, 0.8656686944604700118, -1.721121497068250017 ) ) ;
#25937 = CARTESIAN_POINT ( 'NONE',  ( -1.402160292154681736E-14, 10.67187500034139624, 1.575800808251682339 ) ) ;
#25939 = CARTESIAN_POINT ( 'NONE',  ( -2.467220768007014176, 5.822248629409386922, 0.7216878364870317197 ) ) ;
#25938 = AXIS2_PLACEMENT_3D ( 'NONE', #11430, #127421, #193392 ) ;
#25940 = CARTESIAN_POINT ( 'NONE',  ( 0.3521972369381949908, -1.576644756679127513, -1.565149006781616725 ) ) ;
#25941 = ORIENTED_EDGE ( 'NONE', *, *, #211412, .F. ) ;
#25943 = FACE_OUTER_BOUND ( 'NONE', #203281, .T. ) ;
#25942 = CARTESIAN_POINT ( 'NONE',  ( -3.336715202739028552, 6.906935146588564223, 0.7216878364870338292 ) ) ;
#25944 = CARTESIAN_POINT ( 'NONE',  ( 5.542585869888291938, 5.360771691158120689, -0.7998128361456211532 ) ) ;
#25945 = PRESENTATION_STYLE_ASSIGNMENT (( #206827 ) ) ;
#25946 = CARTESIAN_POINT ( 'NONE',  ( -11.00592705432737972, 9.989806926531038300, 1.444010445236424856 ) ) ;
#25947 = CARTESIAN_POINT ( 'NONE',  ( 11.57874831553684380, 8.190333010158946436, -2.985585545478492975 ) ) ;
#25948 = CARTESIAN_POINT ( 'NONE',  ( 9.042925270190622200, 12.53353466765568669, 1.082531754730546636 ) ) ;
#25949 = CARTESIAN_POINT ( 'NONE',  ( 0.8187140321147531319, -1.423520202335259999, 1.350257566363553208 ) ) ;
#25950 = CARTESIAN_POINT ( 'NONE',  ( 1.364683531249988535, 1.426041667008083991, 0.7879004041258500513 ) ) ;
#25951 = CARTESIAN_POINT ( 'NONE',  ( -2.580963302752292243, 0.4788041664876945269, 0.000000000000000000 ) ) ;
#25952 = CARTESIAN_POINT ( 'NONE',  ( 6.074655751228532630, 1.318658252384183438, -1.452748870126779890 ) ) ;
#25953 = CARTESIAN_POINT ( 'NONE',  ( -9.155833807930273238, 9.576227618873799585, -0.7998128361456291469 ) ) ;
#25954 = CARTESIAN_POINT ( 'NONE',  ( -4.568734577680880093, 7.313645526394248364, -1.082531754730548412 ) ) ;
#25955 = COLOUR_RGB ( '', 0.72549020, 0.75294118, 0.79215686) ;
#25956 = CARTESIAN_POINT ( 'NONE',  ( 0.4974159974337259427, 1.879172763871908902, -1.259763710243780865 ) ) ;
#25958 = ORIENTED_EDGE ( 'NONE', *, *, #1238, .T. ) ;
#25957 = CARTESIAN_POINT ( 'NONE',  ( -0.4373225248172954438, -5.223431457505083308, -10.96785329849813273 ) ) ;
#25959 = CARTESIAN_POINT ( 'NONE',  ( 0.6823417656249899377, 5.676041667008087543, -1.181850606188754593 ) ) ;
#25960 = CARTESIAN_POINT ( 'NONE',  ( 0.3505827959322353471, -1.506356567903786470, 1.108807183729618062 ) ) ;
#25961 = CARTESIAN_POINT ( 'NONE',  ( 6.468101748929986350, 1.443884034049055298, 0.9595089302780019924 ) ) ;
#25963 = CARTESIAN_POINT ( 'NONE',  ( 3.386445149735781257, -0.4294187885149694517, -2.148908265708626697 ) ) ;
#25962 = CARTESIAN_POINT ( 'NONE',  ( 0.6801582343749831283, 1.223958333674737720, 1.178068619123822547 ) ) ;
#25964 = CARTESIAN_POINT ( 'NONE',  ( 4.665214083390394784, -2.058938813511351551, -1.042142520334616185 ) ) ;
#25965 = CARTESIAN_POINT ( 'NONE',  ( 0.6903932018771785639, -2.045263458338997253, -0.2527981509174073715 ) ) ;
#25966 = CARTESIAN_POINT ( 'NONE',  ( 2.642442020880403586, -1.614326438788242557, 1.079121087018119152 ) ) ;
#25967 = CARTESIAN_POINT ( 'NONE',  ( -3.917943204224913156, 7.514758138330285497, -0.7216878364870257245 ) ) ;
#25968 = CARTESIAN_POINT ( 'NONE',  ( 5.579538156164684182, 5.837173214716261604, -0.7738445141641551173 ) ) ;
#25969 = CARTESIAN_POINT ( 'NONE',  ( 5.326475955075804514, -0.9554483686352827077, -1.893264085526874974 ) ) ;
#25970 = CARTESIAN_POINT ( 'NONE',  ( -5.758872628492442907E-14, 0.4531250003414521998, 1.570758158831760287 ) ) ;
#25971 = CARTESIAN_POINT ( 'NONE',  ( 3.920546200773936896, -1.392545040883992336, -1.458557299768625581 ) ) ;
#25972 = CARTESIAN_POINT ( 'NONE',  ( -4.894130264408866893, 6.732904613275549899, -1.443375672974051449 ) ) ;
#25973 = CARTESIAN_POINT ( 'NONE',  ( -5.921879234118920365, 10.13088588310589699, 0.000000000000000000 ) ) ;
#25974 = CARTESIAN_POINT ( 'NONE',  ( 9.317477881089539338, 11.89347683273640932, 1.599625672291279388 ) ) ;
#25975 = CARTESIAN_POINT ( 'NONE',  ( 1.506192966688112422, -0.6554880476431452774, -1.704135612709246184 ) ) ;
#25976 = CARTESIAN_POINT ( 'NONE',  ( -5.074494633264801990, 9.142270515442742607, 0.7998128361456291469 ) ) ;
#25977 = CARTESIAN_POINT ( 'NONE',  ( -5.604063331876898424, 5.713547423438217976, 0.3306394700328639802 ) ) ;
#25978 = DIRECTION ( 'NONE',  ( 1.000000000000000000, 0.000000000000000000, 0.000000000000000000 ) ) ;
#25979 = ORIENTED_EDGE ( 'NONE', *, *, #71412, .T. ) ;
#25980 = CARTESIAN_POINT ( 'NONE',  ( 5.541890059496114240, 0.8373154222949423797, -1.883320703650725125 ) ) ;
#25981 = CARTESIAN_POINT ( 'NONE',  ( -7.227905289416804102, 8.565549271475310533, -1.082531754730549967 ) ) ;
#25982 = CARTESIAN_POINT ( 'NONE',  ( 7.526184668917440312, 8.913541880892736913, -1.082531754730548412 ) ) ;
#25983 = CARTESIAN_POINT ( 'NONE',  ( -2.754277761870538299, 6.365074488824250309, 1.040834085586084257E-14 ) ) ;
#25984 = CARTESIAN_POINT ( 'NONE',  ( -5.163658976018723479, 6.664880576339902163, 1.429021111749773532 ) ) ;
#25985 = CARTESIAN_POINT ( 'NONE',  ( 4.600263385724223220, -0.9500085478860437194, 1.782271578547896418 ) ) ;
#25987 = ORIENTED_EDGE ( 'NONE', *, *, #81885, .T. ) ;
#25986 = CARTESIAN_POINT ( 'NONE',  ( 6.235052692738393354, 2.071546745583602522, 0.8022605484305275203 ) ) ;
#25989 = CARTESIAN_POINT ( 'NONE',  ( 9.300530189294644146, 10.91333531134101165, -1.082531754730543083 ) ) ;
#25988 = CARTESIAN_POINT ( 'NONE',  ( -7.923814432544069142, 8.209148024248356990, 0.000000000000000000 ) ) ;
#25990 = CARTESIAN_POINT ( 'NONE',  ( 7.318703993278529829, 7.432909501780090800, 1.040834085586084257E-14 ) ) ;
#25991 = CARTESIAN_POINT ( 'NONE',  ( 3.907146709503729110, 1.766719954806586612, 1.060879741047163316 ) ) ;
#25992 = CARTESIAN_POINT ( 'NONE',  ( 3.041638857185970046, -1.525043868314728934, 1.319228477497782936 ) ) ;
#25993 = EDGE_LOOP ( 'NONE', ( #26618, #205681, #503, #58083, #168067 ) ) ;
#25994 = CARTESIAN_POINT ( 'NONE',  ( 3.167801447087334576, 6.847518788243868393, -0.7998128361456291469 ) ) ;
#25996 = ORIENTED_EDGE ( 'NONE', *, *, #23468, .T. ) ;
#25995 = CARTESIAN_POINT ( 'NONE',  ( -0.4210486379899329723, 7.995128625469242856, -1.998698746375223045 ) ) ;
#25997 = CARTESIAN_POINT ( 'NONE',  ( 5.364009635805341958, 7.578432035813580825, -1.241402483855597039 ) ) ;
#25998 = CARTESIAN_POINT ( 'NONE',  ( 3.040388574052850235, 1.915307028720541371, -0.6297779509270851062 ) ) ;
#25999 = CARTESIAN_POINT ( 'NONE',  ( 2.044624030687072214, -1.478315374303545315, -1.097237131862264903 ) ) ;
#26000 = CARTESIAN_POINT ( 'NONE',  ( 0.8741376776274005778, 2.222666731570396959, -0.6204599517294244748 ) ) ;
#26001 = CARTESIAN_POINT ( 'NONE',  ( 6.994027139803230320, 9.253060644560830994, -1.599625672291267398 ) ) ;
#26002 = CARTESIAN_POINT ( 'NONE',  ( 4.147864318636265146, 0.7325676050485960822, -2.033789780341701547 ) ) ;
#26003 = CARTESIAN_POINT ( 'NONE',  ( -7.061099074618889304, 7.132370430010492868, -0.7998128361456291469 ) ) ;
#26004 = CARTESIAN_POINT ( 'NONE',  ( 3.444923099841538772, 1.455166840473320233, 1.779090439993118888 ) ) ;
#26005 = ORIENTED_EDGE ( 'NONE', *, *, #53239, .T. ) ;
#26006 = CARTESIAN_POINT ( 'NONE',  ( -8.996750068618080576, 1.000000000000000888, -7.838941051145383199 ) ) ;
#26007 = PRESENTATION_LAYER_ASSIGNMENT (  '', '', ( #1856 ) ) ;
#26008 = CARTESIAN_POINT ( 'NONE',  ( 1.147088892781012781, -1.472398045354219365, -1.153743250124287689 ) ) ;
#26009 = VERTEX_POINT ( 'NONE', #66771 ) ;
#26010 = CARTESIAN_POINT ( 'NONE',  ( 5.787953125587765868, -0.8870788200928159117, 1.760698262704742723 ) ) ;
#26012 = CARTESIAN_POINT ( 'NONE',  ( 7.253248993186713456, 11.40594822545244824, 0.7216878364870438212 ) ) ;
#26011 = CARTESIAN_POINT ( 'NONE',  ( -1.201851678989727383E-14, 4.696875000341419693, -1.575800808251660134 ) ) ;
#26014 = CARTESIAN_POINT ( 'NONE',  ( 0.8739773845415178544, 2.125910683164092152, -0.5920798734769525673 ) ) ;
#26013 = CARTESIAN_POINT ( 'NONE',  ( -5.442708600882160574, 8.437244903416123876, -1.199719254218446718 ) ) ;
#26015 = CARTESIAN_POINT ( 'NONE',  ( -2.680963302752291000, 0.4848410213535060964, -0.1005551520456262199 ) ) ;
#26016 = CARTESIAN_POINT ( 'NONE',  ( 4.680589345215795838, 6.483773540883647435, -1.599625672291256295 ) ) ;
#26017 = CARTESIAN_POINT ( 'NONE',  ( -4.564291269294938225, 8.476756914152748124, 1.040834085586084257E-14 ) ) ;
#26018 = CARTESIAN_POINT ( 'NONE',  ( 6.639320575229256782, 2.033582276073117701, 2.408309898857839304 ) ) ;
#26019 = CARTESIAN_POINT ( 'NONE',  ( 5.366080375918201639, 0.9711980517450971018, 1.715566965677978173 ) ) ;
#26020 = CARTESIAN_POINT ( 'NONE',  ( 5.250698995481407394, 0.6654115676409579905, 2.209675006967478428 ) ) ;
#26021 = CARTESIAN_POINT ( 'NONE',  ( 5.758217292028081857, -1.861241882002647285, 0.0004304118630827496474 ) ) ;
#26022 = CARTESIAN_POINT ( 'NONE',  ( 2.957939313049274599, -0.6512127342562739063, 1.957104789517728483 ) ) ;
#26023 = CARTESIAN_POINT ( 'NONE',  ( 5.653386867218496370, 9.539442411822841805, 1.040834085586084257E-14 ) ) ;
#26024 = CARTESIAN_POINT ( 'NONE',  ( 2.911969131885072670, 6.619324097166378706, 0.000000000000000000 ) ) ;
#26025 = CARTESIAN_POINT ( 'NONE',  ( 8.080296363620359301, 8.529359967086321603, 1.040834085586084257E-14 ) ) ;
#26026 = CARTESIAN_POINT ( 'NONE',  ( -1.364683531250014514, 1.551041667008084435, -0.7879004041258289570 ) ) ;
#26027 = CARTESIAN_POINT ( 'NONE',  ( -4.723283533108845411, 14.53085706694251478, 11.04060857866791956 ) ) ;
#26028 = CARTESIAN_POINT ( 'NONE',  ( 6.629573926958101993, 6.836850457647000390, -0.7216878364870257245 ) ) ;
#26029 = CARTESIAN_POINT ( 'NONE',  ( 4.897030219210679824, 0.3665305452156160659, 2.139867649710110786 ) ) ;
#26031 = CARTESIAN_POINT ( 'NONE',  ( 4.247483403459266782, 1.840758003770435414, -0.04960325993209198370 ) ) ;
#26030 = CARTESIAN_POINT ( 'NONE',  ( -11.41176686791169104, 9.840491965131459295, -3.404018756831829418 ) ) ;
#26033 = CARTESIAN_POINT ( 'NONE',  ( 0.000000000000000000, 13.49999999999999822, 0.000000000000000000 ) ) ;
#26032 = CARTESIAN_POINT ( 'NONE',  ( -1.364683531250010295, 5.488541667008087543, -0.7879004041258300672 ) ) ;
#26034 = CARTESIAN_POINT ( 'NONE',  ( 6.304242050522723240, 1.625252681175231029, -1.470355468214133543 ) ) ;
#26035 = CARTESIAN_POINT ( 'NONE',  ( 1.772826578343088544, 3.950000000000001954, -0.4500000000000284883 ) ) ;
#26036 = CARTESIAN_POINT ( 'NONE',  ( 0.5798237426192736077, 2.110460337659907371, -0.8156065903286384700 ) ) ;
#26037 = CARTESIAN_POINT ( 'NONE',  ( -4.021356766390437265, 7.786759281977493785, -0.4705729632344165525 ) ) ;
#26038 = DIRECTION ( 'NONE',  ( 0.000000000000000000, 0.000000000000000000, 1.000000000000000000 ) ) ;
#26039 = CARTESIAN_POINT ( 'NONE',  ( 6.597622414017595638, 6.771646741010207471, 0.1687998040609314243 ) ) ;
#26040 = CARTESIAN_POINT ( 'NONE',  ( -5.275531169048911728, 6.287779464379406491, -1.082531754730549967 ) ) ;
#26041 = CARTESIAN_POINT ( 'NONE',  ( 0.1000639402851908749, -0.9014739813196898099, 1.686438745833309660 ) ) ;
#26042 = CARTESIAN_POINT ( 'NONE',  ( 1.269958040854075154, -1.126728106645444205, 1.364847948389063870 ) ) ;
#26043 = CARTESIAN_POINT ( 'NONE',  ( 5.250644345176154637, 1.983683461502975254, 0.3419521592970317103 ) ) ;
#26044 = CARTESIAN_POINT ( 'NONE',  ( 4.333802657862601215, 8.207853534148366492, 0.7998128361456462443 ) ) ;
#26045 = CARTESIAN_POINT ( 'NONE',  ( 3.733512407637301855, -1.946585179706640467, 0.8041552576890409476 ) ) ;
#26046 = CARTESIAN_POINT ( 'NONE',  ( 2.882342042720618558, -0.5589011775578194285, -1.832234547041192929 ) ) ;
#26047 = CARTESIAN_POINT ( 'NONE',  ( -5.204170427930421283E-15, 3.447199233515649386, -11.99999999999998224 ) ) ;
#26048 = CARTESIAN_POINT ( 'NONE',  ( 4.211352281912852824, -1.636193967830642748, -1.096030559421146133 ) ) ;
#26050 = EDGE_CURVE ( 'NONE', #108697, #163734, #79575, .T. ) ;
#26049 = CARTESIAN_POINT ( 'NONE',  ( 5.062762828692743966, 0.5904309321736100902, 1.931528952932992427 ) ) ;
#26051 = CARTESIAN_POINT ( 'NONE',  ( 3.221420234344949840, -1.803205065257794004, 0.4975683872451354683 ) ) ;
#26054 = EDGE_LOOP ( 'NONE', ( #71518, #119290, #189482, #171422 ) ) ;
#26053 = CARTESIAN_POINT ( 'NONE',  ( 0.7559434568639655794, 0.7726834774516875282, -1.749509110286852742 ) ) ;
#26052 = CARTESIAN_POINT ( 'NONE',  ( 5.303229652072571021, 1.413297086782526302, 0.9885393367406664078 ) ) ;
#26056 = CARTESIAN_POINT ( 'NONE',  ( 5.043269954603547767, 4.986162489899998995, -0.7216878364870197293 ) ) ;
#26055 = CARTESIAN_POINT ( 'NONE',  ( 2.737190076726934151, 0.2709513247245790013, 2.190122135706531914 ) ) ;
#26057 = CARTESIAN_POINT ( 'NONE',  ( 0.6823417656249882723, 2.488541667008084435, -1.181850606188749264 ) ) ;
#26058 = CARTESIAN_POINT ( 'NONE',  ( 6.865691018405424728, -0.4312029709039078007, 1.920920986087648163 ) ) ;
#26060 = ADVANCED_FACE ( 'NONE', ( #84126 ), #119901, .F. ) ;
#26059 = CARTESIAN_POINT ( 'NONE',  ( 8.599949509769960088, 8.927695937686774386, 1.040834085586084257E-14 ) ) ;
#26061 = CARTESIAN_POINT ( 'NONE',  ( -10.47775378526269918, 11.11846759242831872, -0.7998128361456221525 ) ) ;
#26062 = CARTESIAN_POINT ( 'NONE',  ( 0.4294425147611385940, -9.006862915010128035, -9.490288674561771387 ) ) ;
#26063 = CARTESIAN_POINT ( 'NONE',  ( 0.000000000000000000, 13.49999999999999822, 0.000000000000000000 ) ) ;
#26064 = CARTESIAN_POINT ( 'NONE',  ( 6.905598574191389005, -7.287292132484016527, 6.905598574191363248 ) ) ;
#26065 = ORIENTED_EDGE ( 'NONE', *, *, #89674, .F. ) ;
#26066 = CARTESIAN_POINT ( 'NONE',  ( 1.838419004579601834, -1.109345826794335688, 1.747895861591180156 ) ) ;
#26068 = CARTESIAN_POINT ( 'NONE',  ( -1.500000000000011324, 2.920833333333352932, 0.8660254037844403729 ) ) ;
#26067 = AXIS2_PLACEMENT_3D ( 'NONE', #122402, #89831, #9612 ) ;
#26069 = CARTESIAN_POINT ( 'NONE',  ( 6.823831386379729302, 6.855558127064808716, -0.7998128361456281477 ) ) ;
#26070 = CARTESIAN_POINT ( 'NONE',  ( -6.795661308947694934, 8.951357498570873261, -1.599625672291263179 ) ) ;
#26071 = CARTESIAN_POINT ( 'NONE',  ( 4.390861645979372341, 6.216034235099629157, -1.599625672291269396 ) ) ;
#26072 = CARTESIAN_POINT ( 'NONE',  ( 0.3112020186443940628, 1.677875239561373855, -1.123872588032665210 ) ) ;
#26073 = CARTESIAN_POINT ( 'NONE',  ( -9.495347311156809411, -6.857257212219918685, 3.422217897015904270E-15 ) ) ;
#26074 = CARTESIAN_POINT ( 'NONE',  ( -1.364683531250012516, 3.238541667008084879, -0.7879004041258289570 ) ) ;
#26075 = VERTEX_POINT ( 'NONE', #186953 ) ;
#26077 = CARTESIAN_POINT ( 'NONE',  ( 10.38518247838791986, 11.21839376764850726, 0.7216878364870438212 ) ) ;
#26076 = CARTESIAN_POINT ( 'NONE',  ( 0.07479286986303290696, 5.725009232006174287, -2.449550298930736059 ) ) ;
#26078 = CARTESIAN_POINT ( 'NONE',  ( 5.413435409655408925, 0.5825687168248098180, 1.930121546480124461 ) ) ;
#26079 = CARTESIAN_POINT ( 'NONE',  ( 5.032410968829077014, 0.5625187028349203366, 1.831241071522809127 ) ) ;
#26080 = CARTESIAN_POINT ( 'NONE',  ( 2.243918346939121733, 2.191141468336772036, 0.05030144379260944459 ) ) ;
#26081 = CARTESIAN_POINT ( 'NONE',  ( -4.663641653420935285, 5.503632019488245319, 1.082531754730560403 ) ) ;
#26082 = CARTESIAN_POINT ( 'NONE',  ( -0.7500000000000006661, 1.639583334016154970, -1.299038105676652011 ) ) ;
#26083 = CARTESIAN_POINT ( 'NONE',  ( 5.695569903961543723, 1.858472494656268958, -0.7744561248179144819 ) ) ;
#26084 = CARTESIAN_POINT ( 'NONE',  ( 1.476665317443916381, -1.350161712199383413, 1.354623164920423672 ) ) ;
#26085 = CARTESIAN_POINT ( 'NONE',  ( -5.961834861707238531, 7.978559976790334574, -1.599625672291263179 ) ) ;
#26086 = CARTESIAN_POINT ( 'NONE',  ( 0.4566579290818244541, -1.899626807963299635, -0.6766942018802262204 ) ) ;
#26087 = CARTESIAN_POINT ( 'NONE',  ( -1.402160292154681736E-14, 9.234375000341398021, 1.575800808251682339 ) ) ;
#26088 = B_SPLINE_CURVE_WITH_KNOTS ( 'NONE', 3,
 ( #200970, #198845, #629, #101364, #164246, #1708 ),
 .UNSPECIFIED., .F., .F.,
 ( 4, 2, 4 ),
 ( 0.0004037790303856098246, 0.0007126936173801977749, 0.001021608204374785563 ),
 .UNSPECIFIED. ) ;
#26090 = CARTESIAN_POINT ( 'NONE',  ( -4.633854640820660009, 8.628190524257904670, -0.7998128361456362523 ) ) ;
#26089 = CARTESIAN_POINT ( 'NONE',  ( 2.946908815893133138, -1.710673590971498292, -1.201729372296795662 ) ) ;
#26092 = EDGE_LOOP ( 'NONE', ( #165046, #143177, #119411, #11303, #21838, #46099, #58383 ) ) ;
#26091 = CARTESIAN_POINT ( 'NONE',  ( 1.922448523189672853, 1.607815062812420370, 0.6247884732281087095 ) ) ;
#26093 = CARTESIAN_POINT ( 'NONE',  ( 6.275647701495586261, 0.3610785225884837191, -2.089460823871174266 ) ) ;
#26094 = CARTESIAN_POINT ( 'NONE',  ( 4.313465427442102929, 8.184126765324453601, 0.7998128361456462443 ) ) ;
#26095 = CARTESIAN_POINT ( 'NONE',  ( -15.75000000000000000, 13.40000000000000036, -1.100000000000002087 ) ) ;
#26096 = CARTESIAN_POINT ( 'NONE',  ( 0.3440982351944205653, -0.9282241650855774795, 1.728402704573737125 ) ) ;
#26097 = CARTESIAN_POINT ( 'NONE',  ( -11.84668730067608777, 10.09365272245204714, -1.400000000000002132 ) ) ;
#26098 = CARTESIAN_POINT ( 'NONE',  ( 6.830610463186557624, 6.863467050006115677, 1.040834085586084257E-14 ) ) ;
#26099 = ORIENTED_EDGE ( 'NONE', *, *, #129911, .T. ) ;
#26100 = DIRECTION ( 'NONE',  ( -1.276756478318932585E-15, 1.000000000000000000, -1.665334536937738262E-16 ) ) ;
#26101 = ORIENTED_EDGE ( 'NONE', *, *, #139194, .F. ) ;
#26102 = CARTESIAN_POINT ( 'NONE',  ( 2.947712979364258690, -1.218347856841961452, -1.340696891046004868 ) ) ;
#26103 = AXIS2_PLACEMENT_3D ( 'NONE', #216, #98839, #95661 ) ;
#26104 = EDGE_LOOP ( 'NONE', ( #106132, #155824 ) ) ;
#26105 = CARTESIAN_POINT ( 'NONE',  ( 2.367870383881045981, 5.914265881169853856, 0.000000000000000000 ) ) ;
#26106 = CARTESIAN_POINT ( 'NONE',  ( 3.874598038455354665, 7.742391154831717692, -0.7998128361456362523 ) ) ;
#26107 = CARTESIAN_POINT ( 'NONE',  ( 4.213381321868588714, 1.457370398675205569, 1.075660112967236737 ) ) ;
#26108 = CARTESIAN_POINT ( 'NONE',  ( 0.5727075793229207124, 3.454207612412955708, -0.3118784721225411061 ) ) ;
#26109 = FACE_OUTER_BOUND ( 'NONE', #128209, .T. ) ;
#26110 = CARTESIAN_POINT ( 'NONE',  ( 5.449628763635895545, 6.258197423388296876, 1.014392677442396806 ) ) ;
#26111 = CARTESIAN_POINT ( 'NONE',  ( 3.648742529127374734, -0.3609857515115758586, -1.825517407628447053 ) ) ;
#26112 = CARTESIAN_POINT ( 'NONE',  ( 1.757307594529472272, 1.832486779838927937, -0.5580655975847663708 ) ) ;
#26113 = CARTESIAN_POINT ( 'NONE',  ( 0.8854529848611718545, 1.222500307375608886, 1.355994775097228766 ) ) ;
#26114 = CARTESIAN_POINT ( 'NONE',  ( 4.716156256285582771, 8.225219390492719995, 0.6619851453327877389 ) ) ;
#26115 = CARTESIAN_POINT ( 'NONE',  ( -10.84253909858433218, 4.919570308430900596, -5.035411995924089723 ) ) ;
#26116 = AXIS2_PLACEMENT_3D ( 'NONE', #48784, #98595, #150551 ) ;
#26117 = CARTESIAN_POINT ( 'NONE',  ( 6.210774601750883583, 6.933448576277219111, 0.8519936491524527922 ) ) ;
#26118 = CARTESIAN_POINT ( 'NONE',  ( -11.55950211276791251, 9.799999999999982947, 3.221476510067111665 ) ) ;
#26119 = DIRECTION ( 'NONE',  ( 0.000000000000000000, 1.000000000000000000, 0.000000000000000000 ) ) ;
#26120 = CARTESIAN_POINT ( 'NONE',  ( 6.925078400183550364, 3.684205305355064297, 2.658256427561227486 ) ) ;
#26121 = CARTESIAN_POINT ( 'NONE',  ( 6.643132081016111634, 9.733775946952057723, 1.082531754730558626 ) ) ;
#26122 = CARTESIAN_POINT ( 'NONE',  ( 5.260591308972474067, -0.6599101888420509932, -1.855755260766891235 ) ) ;
#26123 = CARTESIAN_POINT ( 'NONE',  ( -4.391951695823077984, 7.211361847513815704, 1.199719254218464037 ) ) ;
#26124 = CARTESIAN_POINT ( 'NONE',  ( 4.360407863076827793E-16, 4.000000000000003553, -2.400000000000000355 ) ) ;
#26125 = AXIS2_PLACEMENT_3D ( 'NONE', #32040, #36276, #182524 ) ;
#26126 = CARTESIAN_POINT ( 'NONE',  ( 6.492125937493531396, -0.5805207454109837517, -2.113085764653479082 ) ) ;
#26127 = CARTESIAN_POINT ( 'NONE',  ( 4.999011269523485623, 1.601735033023284904, -1.069960431631542752 ) ) ;
#26128 = CARTESIAN_POINT ( 'NONE',  ( -6.555530967407501741, 7.606873202518897870, 1.199719254218450271 ) ) ;
#26129 = CARTESIAN_POINT ( 'NONE',  ( 0.8854529848611718545, 1.222500307375608886, 1.355994775097228766 ) ) ;
#26130 = CARTESIAN_POINT ( 'NONE',  ( 1.735297346119796691, 0.2185962045802778420, 2.196029071591873993 ) ) ;
#26131 = ADVANCED_FACE ( 'NONE', ( #117767 ), #183758, .F. ) ;
#26132 = CARTESIAN_POINT ( 'NONE',  ( 0.7500000000000006661, 10.41666666666667140, -1.299038105676657340 ) ) ;
#26133 = CARTESIAN_POINT ( 'NONE',  ( 0.8789968191965717992, -1.730013457311157188, -0.8152767527440167861 ) ) ;
#26134 = ORIENTED_EDGE ( 'NONE', *, *, #181495, .F. ) ;
#26135 = CARTESIAN_POINT ( 'NONE',  ( 0.8890313061419883311, 0.1412731933134198092, 1.964529561086136189 ) ) ;
#26136 = CARTESIAN_POINT ( 'NONE',  ( 2.190873381757904692, 1.502741926987064325, 1.230217333823523163 ) ) ;
#26137 = ORIENTED_EDGE ( 'NONE', *, *, #210187, .F. ) ;
#26138 = CARTESIAN_POINT ( 'NONE',  ( 1.247422469434919412, -1.966343046301596509, -0.4444367004674750210 ) ) ;
#26140 = CARTESIAN_POINT ( 'NONE',  ( 6.649252725998297642, 1.619456339520190413, -0.9165514639192672286 ) ) ;
#26139 = CARTESIAN_POINT ( 'NONE',  ( -6.805266759416629618, 6.904175738932996964, 0.000000000000000000 ) ) ;
#26141 = CARTESIAN_POINT ( 'NONE',  ( 5.585032934186686226, 5.480569609498057382, 0.000000000000000000 ) ) ;
#26142 = CARTESIAN_POINT ( 'NONE',  ( -11.35573736746281348, 13.61270414413282204, -3.554362808847921773 ) ) ;
#26143 = CARTESIAN_POINT ( 'NONE',  ( 4.041704886938696006, 3.985977791876626597, -0.7864694415971177355 ) ) ;
#26144 = CARTESIAN_POINT ( 'NONE',  ( -6.069210040772897052, 7.109775131437022999, -1.199719254218453823 ) ) ;
#26145 = CARTESIAN_POINT ( 'NONE',  ( 2.876726420669137863, -0.1638259704515396820, -2.185508879517850112 ) ) ;
#26146 = CARTESIAN_POINT ( 'NONE',  ( 3.389175213736292047, 5.937492935125556315, 1.082531754730558626 ) ) ;
#26147 = CARTESIAN_POINT ( 'NONE',  ( 6.770317605177710085, 8.992066187497757213, 1.599625672291268286 ) ) ;
#26148 = DIRECTION ( 'NONE',  ( 0.6507913734559641616, -0.7592566023653004592, 0.000000000000000000 ) ) ;
#26150 = EDGE_CURVE ( 'NONE', #179040, #195055, #200853, .T. ) ;
#26149 = CARTESIAN_POINT ( 'NONE',  ( 2.666400811807769777, -1.259032629953384719, 1.322343945743660543 ) ) ;
#26151 = DIRECTION ( 'NONE',  ( 0.000000000000000000, 1.000000000000000000, 0.000000000000000000 ) ) ;
#26152 = CARTESIAN_POINT ( 'NONE',  ( -3.090368948911150770, 5.692848642783215674, 1.199719254218462483 ) ) ;
#26153 = CARTESIAN_POINT ( 'NONE',  ( -5.018240346111991990, 8.014652766117364990, -1.155606277404798821 ) ) ;
#26154 = CARTESIAN_POINT ( 'NONE',  ( -9.499668754385632852, -7.473374494045003757, -0.07933194154487524519 ) ) ;
#26155 = CARTESIAN_POINT ( 'NONE',  ( 8.697719238366680372, 10.10609285197134533, 1.199719254218462483 ) ) ;
#26156 = CARTESIAN_POINT ( 'NONE',  ( 1.225083325515680555, -0.04812572341393595021, 1.926057772195179485 ) ) ;
#26157 = CARTESIAN_POINT ( 'NONE',  ( 5.893401036868160858, -1.775023410133094615, 0.8355650083611900758 ) ) ;
#26158 = CARTESIAN_POINT ( 'NONE',  ( 0.7500000000000006661, 14.66666666666666785, -1.299038105676657340 ) ) ;
#26159 = CARTESIAN_POINT ( 'NONE',  ( -8.525379664894808585, 8.840697785332414682, -0.7998128361456291469 ) ) ;
#26160 = CARTESIAN_POINT ( 'NONE',  ( 4.690231075323689325, 7.559354456931247412, 1.199719254218462483 ) ) ;
#26161 = CARTESIAN_POINT ( 'NONE',  ( 4.546525781634036534, -1.759932548463913671, 1.305750774140898685 ) ) ;
#26162 = CARTESIAN_POINT ( 'NONE',  ( 5.332434488876471868, 5.115595079977664383, 0.7998128361456341429 ) ) ;
#26163 = CARTESIAN_POINT ( 'NONE',  ( 4.873920291170623642, -2.031351322358550870, 0.3986081187722507746 ) ) ;
#26164 = CARTESIAN_POINT ( 'NONE',  ( -0.6823417656250212460, 2.113541667008083991, 1.181850606188767472 ) ) ;
#26165 = CARTESIAN_POINT ( 'NONE',  ( 5.467524615204178318, -2.242144116172717361, -0.5062228086629757540 ) ) ;
#26166 = CARTESIAN_POINT ( 'NONE',  ( 7.022760382198770301, 8.255937203062467589, -1.082531754730543083 ) ) ;
#26168 = DIRECTION ( 'NONE',  ( 0.000000000000000000, 0.3953086839949192521, -0.9185483353412627894 ) ) ;
#26167 = CARTESIAN_POINT ( 'NONE',  ( 6.238160076063542725, 6.450477308261824305, -0.7216878364870458196 ) ) ;
#26169 = CARTESIAN_POINT ( 'NONE',  ( 0.7445458516137266614, 0.6704725750066173884, 2.192023251310899923 ) ) ;
#26171 = ADVANCED_FACE ( 'NONE', ( #168574 ), #113223, .T. ) ;
#26170 = DIRECTION ( 'NONE',  ( 0.000000000000000000, 0.000000000000000000, -1.000000000000000000 ) ) ;
#26172 = B_SPLINE_CURVE_WITH_KNOTS ( 'NONE', 3,
 ( #49136, #44884, #211601, #47011, #110990, #30757, #96836, #176994, #162885, #80556, #146655, #212668, #130455, #69610 ),
 .UNSPECIFIED., .F., .F.,
 ( 4, 2, 2, 2, 2, 2, 4 ),
 ( 0.001720018798322700722, 0.002147110083253294267, 0.002360655725718589087, 0.002574201368183881306, 0.003001292653114468779, 0.003214838295579761432, 0.003428383938045054084 ),
 .UNSPECIFIED. ) ;
#26173 = CARTESIAN_POINT ( 'NONE',  ( -7.099629715411508890, 8.311931418515415615, 1.199719254218452047 ) ) ;
#26174 = CARTESIAN_POINT ( 'NONE',  ( 4.699130951095971120, -0.5162677480817599029, 1.872006234571305772 ) ) ;
#26175 = EDGE_LOOP ( 'NONE', ( #142943, #94038 ) ) ;
#26176 = CARTESIAN_POINT ( 'NONE',  ( 9.205623113554615600, 11.76297960394566466, 1.443375672974076540 ) ) ;
#26177 = ADVANCED_FACE ( 'NONE', ( #54367 ), #147941, .T. ) ;
#26178 = ORIENTED_EDGE ( 'NONE', *, *, #94349, .T. ) ;
#26179 = CARTESIAN_POINT ( 'NONE',  ( 5.308822938259078583, -0.4706598425541131947, -1.853433239416848455 ) ) ;
#26180 = CARTESIAN_POINT ( 'NONE',  ( 6.264645798839446833, -1.215808215430391304, 1.223651055087880080 ) ) ;
#26181 = CARTESIAN_POINT ( 'NONE',  ( 5.630092293170263495, 2.014432788975322630, 0.09412139267171715229 ) ) ;
#26183 = CARTESIAN_POINT ( 'NONE',  ( -11.97181073603049661, 12.22000000000000064, 0.8318477717169575625 ) ) ;
#26182 = CARTESIAN_POINT ( 'NONE',  ( -10.00321840878439339, 10.56484298653695397, 1.040834085586084257E-14 ) ) ;
#26184 = CARTESIAN_POINT ( 'NONE',  ( 3.285556943750000070, -1.071874999522042016, 0.000000000000000000 ) ) ;
#26186 = CARTESIAN_POINT ( 'NONE',  ( 0.5140565032336151807, 1.225199188247323878, -1.277449566202024656 ) ) ;
#26185 = CARTESIAN_POINT ( 'NONE',  ( 1.095779546523030668, -2.090823718873015657, 0.001679924440483454573 ) ) ;
#26187 = CARTESIAN_POINT ( 'NONE',  ( 5.397111353752316987, -0.9091427841607623295, -1.799923777076550824 ) ) ;
#26189 = CARTESIAN_POINT ( 'NONE',  ( 3.398623556838876514, 1.807253594820698250, -1.409964679536945598 ) ) ;
#26188 = CARTESIAN_POINT ( 'NONE',  ( 5.248941747146098180, 6.152795455539095570, -1.199719254218452047 ) ) ;
#26190 = CARTESIAN_POINT ( 'NONE',  ( 1.815945235625218590, 1.623157326234461628, 0.6282625412417954802 ) ) ;
#26191 = CARTESIAN_POINT ( 'NONE',  ( 2.865608904542978674, -1.736054085904148669, -1.217558864107195715 ) ) ;
#26192 = CARTESIAN_POINT ( 'NONE',  ( 5.468734858265785093, 7.473552982767156294, 1.599625672291269396 ) ) ;
#26193 = CARTESIAN_POINT ( 'NONE',  ( 1.633743589071215974, 0.1333172958793479579, -1.728787957231948447 ) ) ;
#26194 = CARTESIAN_POINT ( 'NONE',  ( 1.360316468749961816, 2.026041667008099179, 0.7853790794158520550 ) ) ;
#26195 = CARTESIAN_POINT ( 'NONE',  ( 1.925991809680915878, 0.9530580284189617002, 1.598336604343030931 ) ) ;
#26196 = CARTESIAN_POINT ( 'NONE',  ( 2.049520782779357120, 1.889653518395111753, -1.069053457954100006 ) ) ;
#26197 = CARTESIAN_POINT ( 'NONE',  ( 3.169157936054858293, 1.820986098869777470, -0.8666075021629695563 ) ) ;
#26198 = CARTESIAN_POINT ( 'NONE',  ( 4.625000000000002665, -2.052068128417944504, 2.503915141160646116E-13 ) ) ;
#26199 = CARTESIAN_POINT ( 'NONE',  ( -1.499999999999997780, 1.681250000682817047, 0.000000000000000000 ) ) ;
#26200 = CARTESIAN_POINT ( 'NONE',  ( 0.7274102002729305738, -1.830281784476958773, 0.6011100631785198933 ) ) ;
#26201 = CARTESIAN_POINT ( 'NONE',  ( 0.6823417656249934904, 13.94270833367473195, 1.181850606188764807 ) ) ;
#26202 = CARTESIAN_POINT ( 'NONE',  ( 3.603960747418310184, 1.611073206568460758, 1.529666071269941474 ) ) ;
#26203 = ORIENTED_EDGE ( 'NONE', *, *, #24579, .T. ) ;
#26204 = CARTESIAN_POINT ( 'NONE',  ( -0.2108831679771168421, 7.629137130509075604, -2.497154329497493386 ) ) ;
#26205 = CARTESIAN_POINT ( 'NONE',  ( -1.402160292154681736E-14, 0.2125000000000202283, 1.732050807568877637 ) ) ;
#26206 = CARTESIAN_POINT ( 'NONE',  ( 7.263417608619159083, 9.497073181520933716, -1.599625672291262513 ) ) ;
#26207 = CARTESIAN_POINT ( 'NONE',  ( 1.364683531249988757, -0.6156249996585803075, 0.000000000000000000 ) ) ;
#26208 = CARTESIAN_POINT ( 'NONE',  ( 6.521772982575972044, -0.4919494239215887466, 2.174507958589830370 ) ) ;
#26209 = CARTESIAN_POINT ( 'NONE',  ( 4.439869198996494681, 1.279870211898268550, 1.486999339763886097 ) ) ;
#26211 = CARTESIAN_POINT ( 'NONE',  ( -5.422898255786193111, 8.310169817517122581, -1.082531754730544860 ) ) ;
#26210 = CARTESIAN_POINT ( 'NONE',  ( 8.866669273657322492, 12.32790267170016207, -1.082531754730543083 ) ) ;
#26212 = FILL_AREA_STYLE_COLOUR ( '', #35211 ) ;
#26213 = CARTESIAN_POINT ( 'NONE',  ( 5.641944544108610238, 0.9243782401199867049, -2.065144452299176425 ) ) ;
#26214 = VECTOR ( 'NONE', #13782, 1000.000000000000000 ) ;
#26215 = CARTESIAN_POINT ( 'NONE',  ( 2.242701489527811454, -2.022432087814116652, -0.4046766347945063846 ) ) ;
#26216 = CARTESIAN_POINT ( 'NONE',  ( -5.042743069279040036, 7.970618449879118828, 1.199719254218464037 ) ) ;
#26217 = AXIS2_PLACEMENT_3D ( 'NONE', #195633, #31009, #163136 ) ;
#26218 = EDGE_LOOP ( 'NONE', ( #51288, #181700, #30938, #61134 ) ) ;
#26219 = CARTESIAN_POINT ( 'NONE',  ( -1.201851678989727383E-14, 1.993750000682816381, 1.732050807568877637 ) ) ;
#26220 = CARTESIAN_POINT ( 'NONE',  ( 4.182764291190976813, -0.1809548918480126112, -1.861743760598027597 ) ) ;
#26221 = CARTESIAN_POINT ( 'NONE',  ( 2.320625381698769640, 0.8157257908444032202, -1.530271591396751729 ) ) ;
#26222 = CARTESIAN_POINT ( 'NONE',  ( 0.2051334325893399424, 1.998568519175287328, 1.122693669494337909 ) ) ;
#26223 = CARTESIAN_POINT ( 'NONE',  ( 0.5170026063063514199, 1.520138765826519300, -1.599913083071627273 ) ) ;
#26224 = DIRECTION ( 'NONE',  ( 0.000000000000000000, 0.000000000000000000, -1.000000000000000000 ) ) ;
#26225 = CARTESIAN_POINT ( 'NONE',  ( 5.701106494887172360, -0.4696333794993942101, 1.884192904834626869 ) ) ;
#26226 = CARTESIAN_POINT ( 'NONE',  ( 7.505683250481794744, 15.49109367268993154, 9.369457576475557659 ) ) ;
#26227 = CARTESIAN_POINT ( 'NONE',  ( 0.3346115673153668424, 0.6298721381652396811, -1.915601020889952322 ) ) ;
#26228 = PRESENTATION_STYLE_ASSIGNMENT (( #209227 ) ) ;
#26229 = PLANE ( 'NONE',  #46553 ) ;
#26230 = CARTESIAN_POINT ( 'NONE',  ( 6.574846728087075931, -0.8593996854794653251, 1.822268861383633531 ) ) ;
#26231 = CARTESIAN_POINT ( 'NONE',  ( -9.287498920561160887, 10.79416914786490089, -1.199719254218441611 ) ) ;
#26232 = CARTESIAN_POINT ( 'NONE',  ( 5.947222937888848371, 10.09017719417900416, 1.040834085586084257E-14 ) ) ;
#26233 = FACE_OUTER_BOUND ( 'NONE', #131216, .T. ) ;
#26234 = CARTESIAN_POINT ( 'NONE',  ( 3.826616632296374831, 1.734130841282412128, 0.5711148077138239465 ) ) ;
#26235 = CARTESIAN_POINT ( 'NONE',  ( 2.186817281270125424, -2.164169025584137263, -0.4306803264119417607 ) ) ;
#26236 = ORIENTED_EDGE ( 'NONE', *, *, #72841, .F. ) ;
#26237 = CARTESIAN_POINT ( 'NONE',  ( -3.594320120954326292, 6.247105003538398371, 1.082531754730549967 ) ) ;
#26238 = CARTESIAN_POINT ( 'NONE',  ( 3.285556943749998737, -2.792708332855373676, -1.896917185911906500 ) ) ;
#26239 = CARTESIAN_POINT ( 'NONE',  ( -8.670602931139386627, 10.07445716020612103, 1.199719254218462483 ) ) ;
#26240 = CARTESIAN_POINT ( 'NONE',  ( 1.090109951703751801, 1.206612241219229942, 1.619577932830415623 ) ) ;
#26241 = CARTESIAN_POINT ( 'NONE',  ( -3.796053574490222626, 14.00000000000128964, -12.24940615670150557 ) ) ;
#26242 = CARTESIAN_POINT ( 'NONE',  ( -4.878955176071358757, 6.785476686873604280, -1.599625672291271394 ) ) ;
#26243 = CARTESIAN_POINT ( 'NONE',  ( 3.098338563049109151, 1.846317948315750357, 0.2325098740301386746 ) ) ;
#26244 = CARTESIAN_POINT ( 'NONE',  ( 8.530051201292206287, 13.10347683481629488, 0.000000000000000000 ) ) ;
#26245 = FACE_OUTER_BOUND ( 'NONE', #107397, .T. ) ;
#26246 = ORIENTED_EDGE ( 'NONE', *, *, #130785, .F. ) ;
#26247 = ORIENTED_EDGE ( 'NONE', *, *, #99329, .F. ) ;
#26248 = CARTESIAN_POINT ( 'NONE',  ( -7.147119532698295252, 11.49005655479003174, 0.000000000000000000 ) ) ;
#26249 = CARTESIAN_POINT ( 'NONE',  ( 4.037589748876240670, -1.260430739550026269, -1.321009972365666307 ) ) ;
#26250 = AXIS2_PLACEMENT_3D ( 'NONE', #94587, #175828, #160629 ) ;
#26252 = CARTESIAN_POINT ( 'NONE',  ( -5.703190497605960196, 6.276721696052339539, -1.111643793752248754 ) ) ;
#26251 = CARTESIAN_POINT ( 'NONE',  ( -3.156015896931072540, 6.904045323053366268, 0.000000000000000000 ) ) ;
#26253 = CARTESIAN_POINT ( 'NONE',  ( 6.546060204425600659, 6.805396270974036987, -0.4351356575816138772 ) ) ;
#26254 = CARTESIAN_POINT ( 'NONE',  ( 1.036033436886945047, 1.672847207165208072, -0.4555716438836182602 ) ) ;
#26255 = CARTESIAN_POINT ( 'NONE',  ( 5.560457619783242933, -1.666209093894938764, -0.7835883864039174806 ) ) ;
#26256 = B_SPLINE_CURVE_WITH_KNOTS ( 'NONE', 3,
 ( #175143, #60297, #22441, #98158, #61375, #97095 ),
 .UNSPECIFIED., .F., .F.,
 ( 4, 2, 4 ),
 ( 0.000000000000000000, 0.0006533415270788660040, 0.001306683054157732008 ),
 .UNSPECIFIED. ) ;
#26257 = CARTESIAN_POINT ( 'NONE',  ( 4.055530604549876017, -1.917597210323931378, -1.283581016687604270 ) ) ;
#26258 = CARTESIAN_POINT ( 'NONE',  ( 4.030516805012513082, 7.924296382481737844, 0.000000000000000000 ) ) ;
#26259 = CARTESIAN_POINT ( 'NONE',  ( 0.8255485222598609729, -1.957653584835903349, 0.6440290526678188465 ) ) ;
#26260 = CARTESIAN_POINT ( 'NONE',  ( 7.145310649601935182, 8.294949498412453437, -1.199719254218446718 ) ) ;
#26261 = CARTESIAN_POINT ( 'NONE',  ( 6.134147193249257946, 0.1786779444946043904, -2.291516319396588397 ) ) ;
#26262 = CARTESIAN_POINT ( 'NONE',  ( -1.115562610750309283E-14, 11.34375000068279604, 1.500000000000001554 ) ) ;
#26263 = CARTESIAN_POINT ( 'NONE',  ( -6.050681693448748177, 10.28115541899069463, 0.7998128361456291469 ) ) ;
#26264 = COLOUR_RGB ( '', 0.40784314, 0.44705882, 0.49803922) ;
#26265 = CARTESIAN_POINT ( 'NONE',  ( 5.471519871388384360, 1.802534880541529994, -0.5000026934619330454 ) ) ;
#26267 = ORIENTED_EDGE ( 'NONE', *, *, #7685, .F. ) ;
#26266 = AXIS2_PLACEMENT_3D ( 'NONE', #85266, #53846, #170788 ) ;
#26269 = CARTESIAN_POINT ( 'NONE',  ( -6.296835998904160014, 6.311006518335105397, 0.000000000000000000 ) ) ;
#26268 = CARTESIAN_POINT ( 'NONE',  ( 2.074333847954575205, 0.8209984392052707136, 1.727357542596375861 ) ) ;
#26270 = CARTESIAN_POINT ( 'NONE',  ( 3.440233207309027375, 0.9924059104887033023, -1.971224004288201881 ) ) ;
#26271 = CARTESIAN_POINT ( 'NONE',  ( 0.6124999999999741762, 0.1458333340161460656, 1.060881119635889380 ) ) ;
#26272 = DIRECTION ( 'NONE',  ( 3.706092522800016599E-15, 0.000000000000000000, 1.000000000000000000 ) ) ;
#26273 = CARTESIAN_POINT ( 'NONE',  ( 5.519577934094861860, 6.572500690266394940, 1.082531754730549078 ) ) ;
#26274 = AXIS2_PLACEMENT_3D ( 'NONE', #155088, #138848, #122680 ) ;
#26275 = CARTESIAN_POINT ( 'NONE',  ( -6.414416072596849538, 7.616478518518682073, -1.082531754730549967 ) ) ;
#26276 = CARTESIAN_POINT ( 'NONE',  ( 1.800300592175264613, -0.7760554750895022336, 2.173288546431056734 ) ) ;
#26277 = CARTESIAN_POINT ( 'NONE',  ( 2.576550507925364109, 1.283677811227203147, -1.483670167215108693 ) ) ;
#26278 = CARTESIAN_POINT ( 'NONE',  ( -4.450819567036170099, 8.414649604842665553, -0.7998128361456361413 ) ) ;
#26279 = EDGE_CURVE ( 'NONE', #72363, #110148, #195919, .T. ) ;
#26280 = CARTESIAN_POINT ( 'NONE',  ( 6.209847231236663490, 0.6040719066883664112, -1.972102366942799945 ) ) ;
#26281 = CARTESIAN_POINT ( 'NONE',  ( 4.528060117284244512, 4.385084346360807572, 0.7216878364870317197 ) ) ;
#26282 = CARTESIAN_POINT ( 'NONE',  ( 3.819546216251490822, -1.394084564108012403, -1.457236891723237449 ) ) ;
#26283 = CARTESIAN_POINT ( 'NONE',  ( 4.472210567661338843, 6.310941310395290493, 1.599625672291261402 ) ) ;
#26284 = EDGE_LOOP ( 'NONE', ( #50992, #90066, #169161, #183469 ) ) ;
#26285 = CARTESIAN_POINT ( 'NONE',  ( 4.417204035549080920, -1.841734835922325120, 0.8216704330437707426 ) ) ;
#26286 = CARTESIAN_POINT ( 'NONE',  ( -8.459397779922852578, 11.95671561229694824, 1.199719254218453823 ) ) ;
#26287 = CYLINDRICAL_SURFACE ( 'NONE', #14326, 0.05000000000000002359 ) ;
#26288 = CARTESIAN_POINT ( 'NONE',  ( 10.57266086055835075, 11.22919251360659310, 0.000000000000000000 ) ) ;
#26289 = CARTESIAN_POINT ( 'NONE',  ( 2.184662588793543136, 1.252765144364040850, -1.772974741507940211 ) ) ;
#26290 = DIRECTION ( 'NONE',  ( -0.000000000000000000, -1.000000000000000000, -0.000000000000000000 ) ) ;
#26291 = CARTESIAN_POINT ( 'NONE',  ( 4.892426280589802445, 6.808304349406905764, 1.389186069060392104 ) ) ;
#26292 = CARTESIAN_POINT ( 'NONE',  ( 2.477632765499269141, 1.147360842229189437, 1.477270975257204633 ) ) ;
#26293 = CARTESIAN_POINT ( 'NONE',  ( 6.169229141836320096, 0.1658205177522271700, -2.155315574850395155 ) ) ;
#26295 = CARTESIAN_POINT ( 'NONE',  ( 6.727182134110203826, 0.5859025467632031914, 1.963451964196837984 ) ) ;
#26294 = CARTESIAN_POINT ( 'NONE',  ( -0.02224634325198419221, -0.007204097619508199532, -2.289079630542793620 ) ) ;
#26296 = CARTESIAN_POINT ( 'NONE',  ( -0.6823417656250003738, 1.217708333674752286, -1.181850606188749264 ) ) ;
#26297 =( NAMED_UNIT ( * ) SI_UNIT ( $, .STERADIAN. ) SOLID_ANGLE_UNIT ( ) );
#26298 = EDGE_LOOP ( 'NONE', ( #159425, #60743 ) ) ;
#26299 = CARTESIAN_POINT ( 'NONE',  ( 2.930216680654484485, -0.9444820207657660394, -1.662695861641521278 ) ) ;
#26300 = CARTESIAN_POINT ( 'NONE',  ( 3.977242411272710942, 1.666424048269627534, -0.5965368118019414023 ) ) ;
#26301 = CARTESIAN_POINT ( 'NONE',  ( 1.436035868020806738, -1.063167577064242142, -1.589284522738307448 ) ) ;
#26302 = CARTESIAN_POINT ( 'NONE',  ( -3.228813138348844536, 6.918699094715619502, 0.7998128361456341429 ) ) ;
#26304 = CARTESIAN_POINT ( 'NONE',  ( -0.01269188720853537365, -0.5084903737302053361, 1.846954624685708923 ) ) ;
#26303 = CARTESIAN_POINT ( 'NONE',  ( 3.609978820808554811, 4.211641957610042120, 2.420000000000023022 ) ) ;
#26305 = CARTESIAN_POINT ( 'NONE',  ( -0.7500000000000249800, -0.05833333333331303105, 1.299038105676659116 ) ) ;
#26306 = CARTESIAN_POINT ( 'NONE',  ( 0.6958625912084138720, -1.462932864358768459, -1.465259690088885014 ) ) ;
#26307 = CARTESIAN_POINT ( 'NONE',  ( -1.364683531250000748, -0.9281249996585805295, 0.000000000000000000 ) ) ;
#26308 = ADVANCED_FACE ( 'NONE', ( #95397 ), #184068, .T. ) ;
#26309 = CARTESIAN_POINT ( 'NONE',  ( 5.717618200960680852, -1.824738551054584379, 0.4112096411929695439 ) ) ;
#26310 = CARTESIAN_POINT ( 'NONE',  ( 1.488595654847742145, -0.2661386877833261111, -1.806066791206423439 ) ) ;
#26312 = CARTESIAN_POINT ( 'NONE',  ( 4.595929827128614420, 8.372548788374160722, -0.07784623617661419470 ) ) ;
#26311 = CARTESIAN_POINT ( 'NONE',  ( 6.041676539500916654, -1.595688354349385607, -1.524751901930617715 ) ) ;
#26313 = CARTESIAN_POINT ( 'NONE',  ( 0.6823417656249882723, -0.3239583329919110133, -1.181850606188749264 ) ) ;
#26314 = CARTESIAN_POINT ( 'NONE',  ( 2.611848684353266226, 0.5523815846302374544, -1.987258587729407999 ) ) ;
#26315 = EDGE_CURVE ( 'NONE', #85478, #104308, #32492, .T. ) ;
#26316 = CARTESIAN_POINT ( 'NONE',  ( -7.039708073993679704, 9.236078724457858158, 1.599625672291283607 ) ) ;
#26317 = CARTESIAN_POINT ( 'NONE',  ( 9.725276259704228821, 10.24057714594344048, 0.7998128361456462443 ) ) ;
#26318 = CARTESIAN_POINT ( 'NONE',  ( 1.464648953335777604, 3.471602976812853125, -0.3340396966001203394 ) ) ;
#26319 = CARTESIAN_POINT ( 'NONE',  ( 0.2632415847364302786, -1.930764589519979424, -0.9721467891136772455 ) ) ;
#26320 = CARTESIAN_POINT ( 'NONE',  ( 6.210516883511641772, 9.403297576475722508, 1.199719254218452047 ) ) ;
#26321 = CARTESIAN_POINT ( 'NONE',  ( 4.896967953096117654, 0.3505727482827174502, 2.040303948762006492 ) ) ;
#26322 = CARTESIAN_POINT ( 'NONE',  ( -0.6823417656250003738, 0.5302083336747518416, -1.181850606188749264 ) ) ;
#26323 = CARTESIAN_POINT ( 'NONE',  ( 3.040462492942562545, 2.144887288335277198, 0.2678724578094940356 ) ) ;
#26324 = CARTESIAN_POINT ( 'NONE',  ( -4.839221724899702259, 8.104102677821947154, -0.8803655321611182361 ) ) ;
#26326 = CARTESIAN_POINT ( 'NONE',  ( 2.277722772326017608, -1.903703133612335119, 0.4737097981617058862 ) ) ;
#26325 = CARTESIAN_POINT ( 'NONE',  ( 3.352217588874096599, 0.9059935441126705236, -1.805122612331450105 ) ) ;
#26327 = CARTESIAN_POINT ( 'NONE',  ( 7.710915694720367419, -5.615420858948574789, 7.765925996254662067 ) ) ;
#26328 = PRODUCT ( 'positive coil', 'positive coil', '', ( #166342 ) ) ;
#26329 = ADVANCED_FACE ( 'NONE', ( #131130 ), #98566, .F. ) ;
#26332 = CARTESIAN_POINT ( 'NONE',  ( 6.399085315970131305, 8.488685506763726352, -1.443375672974057666 ) ) ;
#26331 = CARTESIAN_POINT ( 'NONE',  ( 0.000000000000000000, -1.137499999999999067, -4.012584370867899430 ) ) ;
#26330 = DIRECTION ( 'NONE',  ( -1.000000000000000000, 0.000000000000000000, 0.000000000000000000 ) ) ;
#26333 = CARTESIAN_POINT ( 'NONE',  ( -7.445362632559989535, 8.715286488521982733, 1.199719254218452047 ) ) ;
#26334 = CARTESIAN_POINT ( 'NONE',  ( 1.464077725791514517, -1.074659653367866952, 1.706114136832518779 ) ) ;
#26336 = CARTESIAN_POINT ( 'NONE',  ( 5.935146830689759234, -1.586316731616247200, -1.512381816529739353 ) ) ;
#26335 = CARTESIAN_POINT ( 'NONE',  ( -5.850506979496850057, 6.784345216623154151, -1.199719254218446718 ) ) ;
#26337 = CARTESIAN_POINT ( 'NONE',  ( -3.752568318859959007, 7.355240624044412812, 0.6449737300090957470 ) ) ;
#26338 = CARTESIAN_POINT ( 'NONE',  ( 5.677967274442059953, 1.882970570262190613, -0.3333453579756897600 ) ) ;
#26339 = CARTESIAN_POINT ( 'NONE',  ( -11.94105721237523099, 12.69999999999999929, 1.187919463087245386 ) ) ;
#26340 = MANIFOLD_SOLID_BREP ( 'Revolve1', #105368 ) ;
#26341 = CARTESIAN_POINT ( 'NONE',  ( 4.622967192135525316, 8.337286124226029216, -0.7216878364870207285 ) ) ;
#26343 = CARTESIAN_POINT ( 'NONE',  ( 3.093375225471244772, -0.3905761854139707667, 1.978056131710544063 ) ) ;
#26342 = CARTESIAN_POINT ( 'NONE',  ( -8.636180661780660017, 11.09863007687603087, -1.443375672974058777 ) ) ;
#26344 = CARTESIAN_POINT ( 'NONE',  ( -1.364683531250000748, 13.42187500034139980, 0.000000000000000000 ) ) ;
#26345 = CARTESIAN_POINT ( 'NONE',  ( 5.332891432879703686, 0.1301960547291525494, 1.719897333435776776 ) ) ;
#26346 = CARTESIAN_POINT ( 'NONE',  ( 5.013482942003290255, 9.071090208970993274, -0.7998128361456481317 ) ) ;
#26347 = CARTESIAN_POINT ( 'NONE',  ( 4.207107738942202246, 3.802713871720993399, 1.214306433183764966E-14 ) ) ;
#26348 = CARTESIAN_POINT ( 'NONE',  ( 10.91877484692250277, -9.999999999999973355, -0.1449562030364739129 ) ) ;
#26349 = CARTESIAN_POINT ( 'NONE',  ( 4.499188554602613799, 1.501106652244098116, 1.115835331622745841 ) ) ;
#26350 = CARTESIAN_POINT ( 'NONE',  ( 1.041946221393402539, 1.387617377995558066, 1.536584593769604101 ) ) ;
#26351 = DIRECTION ( 'NONE',  ( 0.000000000000000000, -1.000000000000000000, 0.000000000000000000 ) ) ;
#26352 = ORIENTED_EDGE ( 'NONE', *, *, #129464, .F. ) ;
#26353 = CARTESIAN_POINT ( 'NONE',  ( 3.393283585170187688, 7.180857625999046867, 0.7998128361456271485 ) ) ;
#26354 = CARTESIAN_POINT ( 'NONE',  ( 0.06993570063764525946, -0.9480199632962028611, 1.779638758220257522 ) ) ;
#26355 = CARTESIAN_POINT ( 'NONE',  ( 0.7557781591117664899, 0.7332364915693561080, -1.656728582389139781 ) ) ;
#26356 = CARTESIAN_POINT ( 'NONE',  ( 6.007671464186834065, 7.141943142040370063, 1.082531754730549967 ) ) ;
#26357 = CARTESIAN_POINT ( 'NONE',  ( 10.42254519813228697, 10.51899034650841358, 5.955849994509172518 ) ) ;
#26358 = ORIENTED_EDGE ( 'NONE', *, *, #37732, .T. ) ;
#26359 = CARTESIAN_POINT ( 'NONE',  ( 8.961576348508637935, 11.47825837805867799, -1.443375672974052559 ) ) ;
#26360 = CIRCLE ( 'NONE', #40300, 2.400000000000000799 ) ;
#26362 = CARTESIAN_POINT ( 'NONE',  ( 8.925345196497941558, 9.307324238869423283, 1.040834085586084257E-14 ) ) ;
#26361 = CARTESIAN_POINT ( 'NONE',  ( 0.7308173252688826560, -1.846041318942293286, -0.6644482084196751126 ) ) ;
#26363 = CARTESIAN_POINT ( 'NONE',  ( 4.974201611368001430, -1.901669438865726924, -0.2299391999119395624 ) ) ;
#26364 = CARTESIAN_POINT ( 'NONE',  ( 0.07479286986305370977, 0.004866263145587856019, -1.855573292446038414 ) ) ;
#26365 = CARTESIAN_POINT ( 'NONE',  ( -4.026408433134269771, 6.680931691089825541, 1.082531754730560403 ) ) ;
#26366 =( BOUNDED_CURVE ( )  B_SPLINE_CURVE ( 2, ( #213515, #113992, #182087, #100850, #48923, #65137, #197283, #134464, #115044 ),
 .UNSPECIFIED., .F., .T. ) 
 B_SPLINE_CURVE_WITH_KNOTS ( ( 3, 2, 2, 2, 3 ),
 ( 0.6093749999999996669, 0.6145833333333333703, 0.6250000000000000000, 0.6354166666666666297, 0.6406250000000002220 ),
 .UNSPECIFIED. ) 
 CURVE ( )  GEOMETRIC_REPRESENTATION_ITEM ( )  RATIONAL_B_SPLINE_CURVE ( ( 0.9330127018922194093, 0.9330127018922150794, 1.000000000000000000, 0.8660254037844387076, 1.000000000000000000, 0.8660254037844387076, 1.000000000000000000, 0.9330127018922165227, 0.9330127018922194093 ) ) 
 REPRESENTATION_ITEM ( '' )  );
#26367 = AXIS2_PLACEMENT_3D ( 'NONE', #37386, #151156, #154347 ) ;
#26368 = DIRECTION ( 'NONE',  ( -1.000000000000000000, 7.109522442527899011E-16, 0.000000000000000000 ) ) ;
#26370 = VERTEX_POINT ( 'NONE', #72434 ) ;
#26369 = CARTESIAN_POINT ( 'NONE',  ( 5.666945020832181434, 5.713783400500082266, 0.7216878364870317197 ) ) ;
#26371 = CARTESIAN_POINT ( 'NONE',  ( -8.527715433315703919, 9.051348881730875817, 1.040834085586084257E-14 ) ) ;
#26372 = CARTESIAN_POINT ( 'NONE',  ( 2.325270847726228496, -0.0006328605136555341855, 2.161883445422786654 ) ) ;
#26373 = CARTESIAN_POINT ( 'NONE',  ( -4.659162064951642535, 5.464719159645540003, 1.199719254218452935 ) ) ;
#26374 = CARTESIAN_POINT ( 'NONE',  ( 7.187230829020129441, 8.518095734345896730, 1.082531754730549967 ) ) ;
#26375 = CARTESIAN_POINT ( 'NONE',  ( -2.764973262183167968, 5.313220341600567664, 1.199719254218462483 ) ) ;
#26376 = CARTESIAN_POINT ( 'NONE',  ( 4.647361241834577328, -1.411646026218037253, -1.157555111390089264 ) ) ;
#26377 = EDGE_CURVE ( 'NONE', #74902, #7171, #67089, .T. ) ;
#26378 = CARTESIAN_POINT ( 'NONE',  ( 9.868838213939689297, 9.992711175144377123, 6.338997305163716511 ) ) ;
#26379 = CARTESIAN_POINT ( 'NONE',  ( 1.229685887263828770, -1.247259403286736124, -1.526659406866498481 ) ) ;
#26380 = CARTESIAN_POINT ( 'NONE',  ( 3.744317949583543470, 1.018843395500759197, -1.618198357137661469 ) ) ;
#26381 = ORIENTED_EDGE ( 'NONE', *, *, #24691, .T. ) ;
#26382 = CARTESIAN_POINT ( 'NONE',  ( -5.000000000000009770, 3.850000000000006306, -0.4999999999999942824 ) ) ;
#26383 = CARTESIAN_POINT ( 'NONE',  ( 4.967230218399325103, 1.712698785223613740, 0.9724057732015491951 ) ) ;
#26384 = ORIENTED_EDGE ( 'NONE', *, *, #184656, .F. ) ;
#26385 = CARTESIAN_POINT ( 'NONE',  ( 5.671417317124205937, 1.160065345341480647, 1.557364503162941061 ) ) ;
#26386 = ORIENTED_EDGE ( 'NONE', *, *, #159892, .F. ) ;
#26387 = CARTESIAN_POINT ( 'NONE',  ( -6.310394152517827315, 6.326824364217716656, 0.7998128361456281477 ) ) ;
#26389 = CARTESIAN_POINT ( 'NONE',  ( 6.222909436229170588, 1.570324008046734221, -1.425282903188800798 ) ) ;
#26388 = CARTESIAN_POINT ( 'NONE',  ( -5.581116510680924847, 6.540332679663050541, -1.199719254218453823 ) ) ;
#26390 = CARTESIAN_POINT ( 'NONE',  ( 7.322812364712459221, 7.715904978352238430, 0.000000000000000000 ) ) ;
#26392 = ORIENTED_EDGE ( 'NONE', *, *, #1866, .T. ) ;
#26391 = CARTESIAN_POINT ( 'NONE',  ( 4.231050068913538631, 1.749697241329374098, 0.7720063087622434095 ) ) ;
#26393 = CARTESIAN_POINT ( 'NONE',  ( 0.000000000000000000, 0.08000000000000020983, 0.000000000000000000 ) ) ;
#26394 = CARTESIAN_POINT ( 'NONE',  ( 2.878073747850912412, 6.579779482459851003, -0.7998128361456362523 ) ) ;
#26395 = CARTESIAN_POINT ( 'NONE',  ( 9.534369015033231420, 4.462424917548963421, -7.287319680779428488 ) ) ;
#26396 = CARTESIAN_POINT ( 'NONE',  ( 5.145186220991746495, 0.1505098195577254938, 2.007535063509538809 ) ) ;
#26397 = CARTESIAN_POINT ( 'NONE',  ( 0.1639926229446086736, 8.277376109547596172, 1.999401122995874358 ) ) ;
#26398 = CARTESIAN_POINT ( 'NONE',  ( 6.059193749186201572, -1.568369423792463024, -0.9343120793870243190 ) ) ;
#26399 = CARTESIAN_POINT ( 'NONE',  ( 6.727182134110199385, 2.469373133786161301, 2.195552656936059055 ) ) ;
#26400 = CARTESIAN_POINT ( 'NONE',  ( 1.504437137538238600, 2.067909592606699487, 0.1035681241481553605 ) ) ;
#26401 = CARTESIAN_POINT ( 'NONE',  ( -5.819474248763749635, 7.812472595022922128, -1.599625672291256295 ) ) ;
#26402 = CIRCLE ( 'NONE', #126845, 3.475000000000000089 ) ;
#26403 = CARTESIAN_POINT ( 'NONE',  ( -6.074251926901598431, 7.043194046877760961, -1.007762736454496988 ) ) ;
#26404 = CARTESIAN_POINT ( 'NONE',  ( 6.368025811218641863, 0.9635043244729593059, 1.603280169136585220 ) ) ;
#26405 = CARTESIAN_POINT ( 'NONE',  ( 4.449046963578762615, 8.342305224150557308, -0.7998128361456231517 ) ) ;
#26406 = FACE_OUTER_BOUND ( 'NONE', #15395, .T. ) ;
#26407 = CARTESIAN_POINT ( 'NONE',  ( 3.607878275012302627, 7.223292064240769861, 0.7216878364870257245 ) ) ;
#26408 = AXIS2_PLACEMENT_3D ( 'NONE', #72582, #21675, #155988 ) ;
#26409 = CARTESIAN_POINT ( 'NONE',  ( 3.728655938958122196, 4.308852335994623139, -1.199719254218446718 ) ) ;
#26410 = CARTESIAN_POINT ( 'NONE',  ( 1.364683531249997417, 12.04687500034139980, 2.602085213965210642E-15 ) ) ;
#26412 = CARTESIAN_POINT ( 'NONE',  ( -6.577640801285370209, 7.702944352034914566, -1.199719254218452047 ) ) ;
#26411 = FACE_OUTER_BOUND ( 'NONE', #37940, .T. ) ;
#26413 = CARTESIAN_POINT ( 'NONE',  ( 5.186046676097956443, 1.422060760911178390, 0.9921614550853893322 ) ) ;
#26414 = CARTESIAN_POINT ( 'NONE',  ( -4.416205349749324327, 6.175325546172740765, 1.599625672291267398 ) ) ;
#26415 = CARTESIAN_POINT ( 'NONE',  ( 2.413015750098276513, -1.603085927076562500, 1.310038033242977518 ) ) ;
#26416 = CARTESIAN_POINT ( 'NONE',  ( 3.040728130433269616, -1.601530262690466389, 1.384902248896832333 ) ) ;
#26417 = CARTESIAN_POINT ( 'NONE',  ( 7.751511138711133064, 10.06651563329490529, -1.599625672291262513 ) ) ;
#26418 = CARTESIAN_POINT ( 'NONE',  ( -1.201851678989727383E-14, 3.321875000341421025, 1.575800808251672791 ) ) ;
#26419 = CARTESIAN_POINT ( 'NONE',  ( 1.709744157921966101, 0.5768405975999196800, -1.883039948965541610 ) ) ;
#26420 = CARTESIAN_POINT ( 'NONE',  ( 5.966167892564917530, 6.109520806784549229, 0.6870465322655286977 ) ) ;
#26421 = CARTESIAN_POINT ( 'NONE',  ( 4.094199201646931741, 4.839282492418613302, -1.082531754730543083 ) ) ;
#26423 = CYLINDRICAL_SURFACE ( 'NONE', #56395, 1.224999999999996980 ) ;
#26422 = CARTESIAN_POINT ( 'NONE',  ( -1.737500000000000266, -2.158333333333331439, -3.009438278150923907 ) ) ;
#26424 = CARTESIAN_POINT ( 'NONE',  ( 4.136908408643169111, -1.995281682711878668, 1.128303315244700178 ) ) ;
#26426 = EDGE_CURVE ( 'NONE', #45318, #123196, #55143, .T. ) ;
#26425 = CARTESIAN_POINT ( 'NONE',  ( 0.5569169099325712580, -1.540613122784354916, -0.9793164655157863274 ) ) ;
#26427 = CIRCLE ( 'NONE', #43782, 10.99999999999999112 ) ;
#26428 = CARTESIAN_POINT ( 'NONE',  ( 6.204791576909545192, 7.267953590263130259, -1.199719254218452047 ) ) ;
#26429 = CARTESIAN_POINT ( 'NONE',  ( 6.765155463094759014, 7.955398130774449683, 1.082531754730558626 ) ) ;
#26430 = CARTESIAN_POINT ( 'NONE',  ( -8.646349277213090545, 11.11049346154719508, 1.599625672291269396 ) ) ;
#26431 = CARTESIAN_POINT ( 'NONE',  ( 2.461191956773252087, -1.671442449460639468, 1.121892926246186306 ) ) ;
#26432 = CARTESIAN_POINT ( 'NONE',  ( 2.219515905360454067, 0.3404028402014187549, -1.931851785523025944 ) ) ;
#26433 = CARTESIAN_POINT ( 'NONE',  ( -8.025536864285518490, 11.45054454405341282, -1.199719254218446718 ) ) ;
#26434 = CARTESIAN_POINT ( 'NONE',  ( -5.228640796364566690, 9.251831362400652736, -0.7998128361456231517 ) ) ;
#26436 = EDGE_CURVE ( 'NONE', #86666, #205543, #85501, .T. ) ;
#26435 = CARTESIAN_POINT ( 'NONE',  ( 0.07536363704237906969, 4.084105538841027894, -2.698926661290324880 ) ) ;
#26438 = CARTESIAN_POINT ( 'NONE',  ( 2.992752380588555638, 1.518849080061919654, -0.9082622674112093009 ) ) ;
#26437 = CARTESIAN_POINT ( 'NONE',  ( 5.138659532522440010, -1.793477146331866612, 1.074093663348500760 ) ) ;
#26439 = CARTESIAN_POINT ( 'NONE',  ( 0.3554123170488062700, 16.00000000000058265, 12.67999999502907649 ) ) ;
#26440 = CARTESIAN_POINT ( 'NONE',  ( 6.474598600699414064, -0.1057723710937721190, -2.289958182497778161 ) ) ;
#26441 = CARTESIAN_POINT ( 'NONE',  ( 5.490116972639333071, -0.4286210177542044697, -1.686591927243533240 ) ) ;
#26442 = CARTESIAN_POINT ( 'NONE',  ( 8.076906825439115423, 10.44614393447756129, -1.599625672291262513 ) ) ;
#26443 = CARTESIAN_POINT ( 'NONE',  ( 5.783868576693856234, 1.881360230585613413, -1.320557073901595047 ) ) ;
#26444 = CARTESIAN_POINT ( 'NONE',  ( -11.84668730067608422, 12.69999999999999929, -1.320000000000001616 ) ) ;
#26445 = CARTESIAN_POINT ( 'NONE',  ( 5.237493459246572947, -1.633055164623600897, -0.5828427842848020735 ) ) ;
#26446 =( BOUNDED_CURVE ( )  B_SPLINE_CURVE ( 2, ( #31471, #130108, #127995, #129051, #43468, #193950, #175592, #45597, #111713 ),
 .UNSPECIFIED., .F., .T. ) 
 B_SPLINE_CURVE_WITH_KNOTS ( ( 3, 2, 2, 2, 3 ),
 ( 0.5446428571428572063, 0.5476190476190476719, 0.5535714285714286031, 0.5595238095238095344, 0.5625000000000000000 ),
 .UNSPECIFIED. ) 
 CURVE ( )  GEOMETRIC_REPRESENTATION_ITEM ( )  RATIONAL_B_SPLINE_CURVE ( ( 0.9330127018922194093, 0.9330127018922206306, 1.000000000000000000, 0.8660254037844387076, 1.000000000000000000, 0.8660254037844387076, 1.000000000000000000, 0.9330127018922194093, 0.9330127018922194093 ) ) 
 REPRESENTATION_ITEM ( '' )  );
#26447 = CARTESIAN_POINT ( 'NONE',  ( 6.109878594781020134, 0.6360665949224998394, -2.075910194261113784 ) ) ;
#26448 = CARTESIAN_POINT ( 'NONE',  ( 2.198393463710220264, 5.716542807637226886, 0.7998128361456462443 ) ) ;
#26449 = CARTESIAN_POINT ( 'NONE',  ( 6.503150282362620160, -0.1410805869419759218, 1.984311032119711715 ) ) ;
#26450 = CARTESIAN_POINT ( 'NONE',  ( 6.031250000000003553, -0.7852924748303007352, -1.895863743163946680 ) ) ;
#26451 = CARTESIAN_POINT ( 'NONE',  ( 6.727182134110196721, 6.033756510516266935, 2.783943001041962795 ) ) ;
#26452 = CARTESIAN_POINT ( 'NONE',  ( 4.717753586115435382, -1.889304338648789106, 0.3753660715558500005 ) ) ;
#26453 = CARTESIAN_POINT ( 'NONE',  ( -6.009258394948636914E-15, 11.21875000068279249, -1.732050807568875195 ) ) ;
#26454 = CARTESIAN_POINT ( 'NONE',  ( 6.486594595706023370, -1.368296875179885852, 1.750867008312809059 ) ) ;
#26455 = EDGE_LOOP ( 'NONE', ( #122832, #113672, #148969, #80222 ) ) ;
#26456 = CARTESIAN_POINT ( 'NONE',  ( 1.499999999999989120, 4.754166666666689522, 0.8660254037844524744 ) ) ;
#26457 = CARTESIAN_POINT ( 'NONE',  ( 3.662674053986138656, 7.424870162959149589, 0.7998128361456321445 ) ) ;
#26458 = CARTESIAN_POINT ( 'NONE',  ( 7.156006149914539982, 7.243095351188763686, 1.040834085586084257E-14 ) ) ;
#26459 = CARTESIAN_POINT ( 'NONE',  ( 3.106314965395097438, -0.8985160938580877277, 2.031629072759451926 ) ) ;
#26460 = DIRECTION ( 'NONE',  ( -3.330669073875481947E-16, 4.742150360713068815E-16, 1.000000000000000000 ) ) ;
#26461 = CARTESIAN_POINT ( 'NONE',  ( 7.470179451449751262, 7.817556902887268677, 1.040834085586084257E-14 ) ) ;
#26462 = CARTESIAN_POINT ( 'NONE',  ( -7.632877294369372123, 11.84884791016554573, 0.7216878364870458196 ) ) ;
#26463 = EDGE_CURVE ( 'NONE', #186231, #49308, #53569, .T. ) ;
#26464 = CARTESIAN_POINT ( 'NONE',  ( 6.156811154381533591, 9.236677875870187293, -1.082531754730548412 ) ) ;
#26465 = CARTESIAN_POINT ( 'NONE',  ( 0.4049229342097167006, -1.081068455937021611, -1.701946057285643743 ) ) ;
#26467 = CARTESIAN_POINT ( 'NONE',  ( 4.984863162817260829, 1.972918577937707196, 0.6018043753471848945 ) ) ;
#26466 = CARTESIAN_POINT ( 'NONE',  ( 7.944187942603509356, 11.35563746875774882, 1.199719254218460707 ) ) ;
#26468 = CARTESIAN_POINT ( 'NONE',  ( -10.85699613886989390, -6.836286050428373784, 0.3891817118475745518 ) ) ;
#26469 = CARTESIAN_POINT ( 'NONE',  ( 6.495764994278795612, 9.632124022417032805, 1.082531754730549078 ) ) ;
#26470 = DIRECTION ( 'NONE',  ( 0.000000000000000000, 8.546850786086437571E-32, 1.000000000000000000 ) ) ;
#26471 = CARTESIAN_POINT ( 'NONE',  ( -0.6823417656250003738, 0.7177083336747519526, -1.181850606188749264 ) ) ;
#26472 = CARTESIAN_POINT ( 'NONE',  ( 0.3855647087021807362, -0.8419519913594010196, 1.556653678627561543 ) ) ;
#26473 = CARTESIAN_POINT ( 'NONE',  ( -0.08726289061519039436, -1.242903867559573161, -1.588418431006669351 ) ) ;
#26474 = CARTESIAN_POINT ( 'NONE',  ( 5.987833318177087527, -1.732952516383274855, -0.1613439405771869561 ) ) ;
#26475 = CARTESIAN_POINT ( 'NONE',  ( 4.370831947049586219, 0.0005328150827835219676, -2.292545470631628390 ) ) ;
#26476 = CARTESIAN_POINT ( 'NONE',  ( 0.6823417656249882723, -0.3239583329919110133, -1.181850606188749264 ) ) ;
#26477 = CARTESIAN_POINT ( 'NONE',  ( 2.695044507329581673, -0.5773736025265225891, 1.748335772842606106 ) ) ;
#26478 = CARTESIAN_POINT ( 'NONE',  ( 9.103410076571945453, 12.70806329172093818, 1.199719254218450271 ) ) ;
#26479 =( NAMED_UNIT ( * ) SI_UNIT ( $, .STERADIAN. ) SOLID_ANGLE_UNIT ( ) );
#26480 = CARTESIAN_POINT ( 'NONE',  ( 3.557459645987316232, 0.4443818804308434789, -1.770531947851671006 ) ) ;
#26481 = CARTESIAN_POINT ( 'NONE',  ( 3.498672800139957406, -1.986100699840901651, 0.3474671148789992836 ) ) ;
#26482 = CARTESIAN_POINT ( 'NONE',  ( -9.561524646135538319, 12.17819805862340310, -1.599625672291263179 ) ) ;
#26483 = CARTESIAN_POINT ( 'NONE',  ( 7.449797558097145611, 15.00000000000000000, -10.26196259744787653 ) ) ;
#26484 = CARTESIAN_POINT ( 'NONE',  ( 4.963951390035996170, 2.083465175373377498, -0.3060735771123861970 ) ) ;
#26485 = CARTESIAN_POINT ( 'NONE',  ( 8.302289836269501677, 14.87052365979419655, 9.588395110663297416 ) ) ;
#26486 = CARTESIAN_POINT ( 'NONE',  ( 3.033707436314789785, 1.966763487489433970, -0.6469820378900912328 ) ) ;
#26487 = CARTESIAN_POINT ( 'NONE',  ( 5.203632029546647608, 4.965325544092860532, 1.040834085586084257E-14 ) ) ;
#26488 = CARTESIAN_POINT ( 'NONE',  ( -1.360316468750032870, 0.9427083336747503761, 0.7853790794158641564 ) ) ;
#26490 = B_SPLINE_CURVE_WITH_KNOTS ( 'NONE', 3,
 ( #79137, #29332, #97544, #177722, #161478, #109587, #178792, #162542, #145253, #159324, #62882, #196101, #46660, #30405 ),
 .UNSPECIFIED., .F., .F.,
 ( 4, 2, 2, 2, 2, 2, 4 ),
 ( 0.001731424703407325296, 0.001978656695461681377, 0.002225888687516038977, 0.002720352671624756344, 0.002967584663679115678, 0.003214816655733475012, 0.003709280639842193680 ),
 .UNSPECIFIED. ) ;
#26489 = CARTESIAN_POINT ( 'NONE',  ( 5.180389117862056914, 1.045492054797515946, 1.844774357600783121 ) ) ;
#26492 = PRESENTATION_LAYER_ASSIGNMENT (  '', '', ( #64532 ) ) ;
#26491 = CONTEXT_DEPENDENT_SHAPE_REPRESENTATION ( #92141, #173318 ) ;
#26493 = CARTESIAN_POINT ( 'NONE',  ( 0.4516242601883875274, 0.6054225165459875546, -1.828971364544299538 ) ) ;
#26494 = CARTESIAN_POINT ( 'NONE',  ( -3.820365424000704557, 7.679119771301277098, -0.7998128361456481317 ) ) ;
#26495 = CARTESIAN_POINT ( 'NONE',  ( 8.718056468787178659, 10.12981962079525289, 1.199719254218462483 ) ) ;
#26496 = CARTESIAN_POINT ( 'NONE',  ( 4.367134876933267407, 8.109091433148536865, 0.000000000000000000 ) ) ;
#26497 = CARTESIAN_POINT ( 'NONE',  ( 1.145612256460542211, 2.800000000000024247, -0.9666182179050045731 ) ) ;
#26498 = CARTESIAN_POINT ( 'NONE',  ( -4.822949958159302497, 6.649860922651058992, -1.599625672291256295 ) ) ;
#26499 = CARTESIAN_POINT ( 'NONE',  ( 0.0006278483607258588750, -1.039594266688011137, 1.963129682597685166 ) ) ;
#26500 = CARTESIAN_POINT ( 'NONE',  ( 1.887856735188620627, 1.451798466554796718, 1.525807353268118227 ) ) ;
#26501 = CARTESIAN_POINT ( 'NONE',  ( -3.820365424000704557, 7.679119771301277098, -0.7998128361456481317 ) ) ;
#26502 = CARTESIAN_POINT ( 'NONE',  ( 9.101601193475611140, 9.512956235343358102, -0.7998128361456221525 ) ) ;
#26503 = CARTESIAN_POINT ( 'NONE',  ( 6.121894333209238148, 1.833584433263518942, -0.3168336897404684382 ) ) ;
#26504 = CARTESIAN_POINT ( 'NONE',  ( 6.428537391173986038, 10.65171072301167854, 0.7998128361456462443 ) ) ;
#26505 =( NAMED_UNIT ( * ) SI_UNIT ( $, .STERADIAN. ) SOLID_ANGLE_UNIT ( ) );
#26506 = CARTESIAN_POINT ( 'NONE',  ( -3.959863383643135393, 6.777535159962392086, 1.199719254218452935 ) ) ;
#26507 = CARTESIAN_POINT ( 'NONE',  ( -9.056483424248693126, 10.62861408545402675, 1.082531754730558626 ) ) ;
#26508 = CARTESIAN_POINT ( 'NONE',  ( 0.05319811239242258627, 0.3688592364489845510, 2.088132107045739705 ) ) ;
#26509 = DIRECTION ( 'NONE',  ( 0.000000000000000000, 1.000000000000000000, 0.000000000000000000 ) ) ;
#26511 = CARTESIAN_POINT ( 'NONE',  ( 3.420314466093795414, 0.8798059112791326575, 1.753580237611163994 ) ) ;
#26510 = CARTESIAN_POINT ( 'NONE',  ( -1.225000000000028066, -0.2499999999999724665, -4.510281037539698445E-14 ) ) ;
#26512 = CARTESIAN_POINT ( 'NONE',  ( 0.4796413896344040029, 2.016494124141111399, -0.7793912508547717888 ) ) ;
#26513 = ADVANCED_FACE ( 'NONE', ( #100685 ), #182998, .T. ) ;
#26515 = CARTESIAN_POINT ( 'NONE',  ( -6.118227108790639690, 6.008232112836603633, 0.2598000991895776934 ) ) ;
#26514 = CARTESIAN_POINT ( 'NONE',  ( -4.014095998097799267, 6.840806543492835345, -1.199719254218450271 ) ) ;
#26516 = CARTESIAN_POINT ( 'NONE',  ( 1.364683531249988757, 1.384375000341421469, 0.000000000000000000 ) ) ;
#26517 = CARTESIAN_POINT ( 'NONE',  ( 2.273056812072488775, 1.069988629298643579, 1.372433606717870846 ) ) ;
#26518 = CARTESIAN_POINT ( 'NONE',  ( 6.643132081016124069, 7.813037518349371879, 1.082531754730558626 ) ) ;
#26519 = CARTESIAN_POINT ( 'NONE',  ( -11.24554764128284035, 7.016280722987462859, -5.611469924715791535 ) ) ;
#26520 = CIRCLE ( 'NONE', #147606, 0.2000000000000005107 ) ;
#26521 = CARTESIAN_POINT ( 'NONE',  ( 2.759138561942891421, -2.010518527590241966, -0.1511176148010634768 ) ) ;
#26522 = CARTESIAN_POINT ( 'NONE',  ( 6.825078400183545391, 2.405270491081310968, 2.624368679222242484 ) ) ;
#26523 = CARTESIAN_POINT ( 'NONE',  ( -5.157951095356222204, 4.982307464195829816, 0.000000000000000000 ) ) ;
#26524 = CARTESIAN_POINT ( 'NONE',  ( 2.096496217048297694, -0.5238668508756593178, -1.900535169118612755 ) ) ;
#26525 = COLOUR_RGB ( '', 0.09019608, 0.27058824, 0.51372549) ;
#26527 = CARTESIAN_POINT ( 'NONE',  ( -6.617788377246196951, 7.853746207276256719, -1.082531754730549967 ) ) ;
#26526 = CARTESIAN_POINT ( 'NONE',  ( 6.187759705938407073, 1.828009178079874841, -0.5617473972939349691 ) ) ;
#26528 = CARTESIAN_POINT ( 'NONE',  ( -4.950135482320918712, 7.828889591799445213, -1.082531754730549967 ) ) ;
#26529 = CARTESIAN_POINT ( 'NONE',  ( 5.688527969385528849, 8.794310509995222347, -1.199719254218452047 ) ) ;
#26530 = CARTESIAN_POINT ( 'NONE',  ( -6.818824913030298696, 6.919993584815607335, 0.7998128361456341429 ) ) ;
#26531 = CARTESIAN_POINT ( 'NONE',  ( 0.7506560300556723853, 1.990167900158135605, 0.3429568431373567483 ) ) ;
#26532 = SURFACE_STYLE_FILL_AREA ( #28681 ) ;
#26533 = CARTESIAN_POINT ( 'NONE',  ( 5.157380949817064852, -1.946147191792221953, -1.239698497533547661 ) ) ;
#26534 = CARTESIAN_POINT ( 'NONE',  ( 6.180128940399614912, -1.088687182605744042, -1.631870318916525120 ) ) ;
#26535 = CARTESIAN_POINT ( 'NONE',  ( 3.555471618195928496, 1.543666060651678551, 1.210462546525910010 ) ) ;
#26536 = CARTESIAN_POINT ( 'NONE',  ( 7.072549687823125097, 11.40305840243567381, -0.7998128361456291469 ) ) ;
#26537 = CARTESIAN_POINT ( 'NONE',  ( 0.8971115437808926396, -0.9091470795906559932, -1.799921601489597123 ) ) ;
#26538 = ORIENTED_EDGE ( 'NONE', *, *, #175957, .T. ) ;
#26539 = CARTESIAN_POINT ( 'NONE',  ( 0.7435476276109568294, 0.4067398897551637305, -2.077755800567067546 ) ) ;
#26541 = CARTESIAN_POINT ( 'NONE',  ( -5.693534442735004752, 8.729875052244421951, 1.199719254218452047 ) ) ;
#26540 = CARTESIAN_POINT ( 'NONE',  ( -3.327636637150278798, 5.969660945728899826, -1.199719254218452935 ) ) ;
#26542 = CARTESIAN_POINT ( 'NONE',  ( 2.150122221082468865, -1.423577340559305071, 1.167554138749152148 ) ) ;
#26543 = VERTEX_POINT ( 'NONE', #186189 ) ;
#26544 = CARTESIAN_POINT ( 'NONE',  ( 9.954141305008279872, 11.52356260170056679, 6.707419562446313321 ) ) ;
#26545 = CARTESIAN_POINT ( 'NONE',  ( 2.918346969001627045, -2.117983955170518851, 0.1081942149789016649 ) ) ;
#26546 = CARTESIAN_POINT ( 'NONE',  ( -1.499999999999997780, 3.931250000682819046, 1.214306433183764966E-14 ) ) ;
#26547 = CARTESIAN_POINT ( 'NONE',  ( 8.911787042884274257, 9.291506392986812912, 0.7998128361456462443 ) ) ;
#26548 = CARTESIAN_POINT ( 'NONE',  ( 7.523848900940885542, 7.742521570711348389, 0.7998128361456291469 ) ) ;
#26549 = CARTESIAN_POINT ( 'NONE',  ( 4.850885224688990860, -1.657504552092460504, 1.224352689660711535 ) ) ;
#26551 = CARTESIAN_POINT ( 'NONE',  ( 1.048114208743459619, -1.451426956872736262, 1.132798186660122441 ) ) ;
#26550 = CARTESIAN_POINT ( 'NONE',  ( -6.852756576703439961, 10.08230087520760954, 1.199719254218453823 ) ) ;
#26552 = CARTESIAN_POINT ( 'NONE',  ( -1.201851678989727383E-14, 4.696875000341419693, -1.575800808251660134 ) ) ;
#26553 = CARTESIAN_POINT ( 'NONE',  ( -1.558973042057849590, 8.694236233169934991, 2.500000000000010658 ) ) ;
#26554 = CARTESIAN_POINT ( 'NONE',  ( 2.861609313207599925, 6.434901926071078471, -0.3141389326147243088 ) ) ;
#26555 = AXIS2_PLACEMENT_3D ( 'NONE', #96198, #94068, #162247 ) ;
#26556 = CARTESIAN_POINT ( 'NONE',  ( 1.137671262558290763, -1.993743905544292927, 0.9465009238469668240 ) ) ;
#26557 = CARTESIAN_POINT ( 'NONE',  ( 2.232027051843707532, -1.476457111770380415, -1.714336117487671007 ) ) ;
#26558 = CARTESIAN_POINT ( 'NONE',  ( -9.354762803749327560, 10.01623748057011376, 0.7216878364870438212 ) ) ;
#26559 = CARTESIAN_POINT ( 'NONE',  ( 2.742218629285391174, 1.002941080561991161, -1.508394886552874237 ) ) ;
#26560 = CARTESIAN_POINT ( 'NONE',  ( 2.940549639715861030, -1.447296733178250250, 1.255168957218324666 ) ) ;
#26561 = CARTESIAN_POINT ( 'NONE',  ( 4.141125838365485201, -0.1998502692034490602, -2.060677327190631569 ) ) ;
#26562 = CARTESIAN_POINT ( 'NONE',  ( 1.364683531249988535, 3.467708333674749621, -0.7879004041258239610 ) ) ;
#26563 = EDGE_CURVE ( 'NONE', #137341, #101274, #118073, .T. ) ;
#26564 = CARTESIAN_POINT ( 'NONE',  ( 3.221511537501456690, -1.900432112322864464, 0.5242411554721800870 ) ) ;
#26565 = PRODUCT_DEFINITION ( 'UNKNOWN', '', #183724, #212877 ) ;
#26566 = CARTESIAN_POINT ( 'NONE',  ( 6.340456170274588743, 1.905924810476855580, 0.2800546826549690782 ) ) ;
#26567 = CARTESIAN_POINT ( 'NONE',  ( 4.258574955689950592, -1.386304660245713860, 1.256184814050688603 ) ) ;
#26569 = CARTESIAN_POINT ( 'NONE',  ( 4.607021725950278146, 8.475092030744066918, 0.2235605714990263060 ) ) ;
#26568 = CARTESIAN_POINT ( 'NONE',  ( 1.752963477315866658, 0.7269187894614470569, 2.190284518487267906 ) ) ;
#26570 = CARTESIAN_POINT ( 'NONE',  ( 3.367479257110431945, -0.3654178573793941398, 1.824635806631241808 ) ) ;
#26571 = CARTESIAN_POINT ( 'NONE',  ( 1.364683531249990311, 4.884375000341417916, 1.214306433183764966E-14 ) ) ;
#26572 = B_SPLINE_CURVE_WITH_KNOTS ( 'NONE', 3,
 ( #64419, #96949, #80675, #146765, #196553, #114309 ),
 .UNSPECIFIED., .F., .F.,
 ( 4, 2, 4 ),
 ( 0.000000000000000000, 0.0003144386176887254184, 0.0006288772353774508368 ),
 .UNSPECIFIED. ) ;
#26573 = CARTESIAN_POINT ( 'NONE',  ( -3.601662362724658895, 7.353689856487406473, -0.7998128361456281477 ) ) ;
#26574 = CARTESIAN_POINT ( 'NONE',  ( 6.986529229743720926, 7.045372277656132276, -0.7998128361456281477 ) ) ;
#26575 = FACE_OUTER_BOUND ( 'NONE', #198875, .T. ) ;
#26576 = B_SPLINE_CURVE_WITH_KNOTS ( 'NONE', 3,
 ( #165340, #131826, #197835, #34270, #16935, #100342 ),
 .UNSPECIFIED., .F., .F.,
 ( 4, 2, 4 ),
 ( 0.000000000000000000, 0.002403146417856977853, 0.004806292835713955706 ),
 .UNSPECIFIED. ) ;
#26577 = CARTESIAN_POINT ( 'NONE',  ( 0.5750072486576313091, -1.983761410860336527, -0.7076436626956124076 ) ) ;
#26578 = CARTESIAN_POINT ( 'NONE',  ( -1.364683531249997417, 4.071875000341417028, 1.214306433183764966E-14 ) ) ;
#26579 = CARTESIAN_POINT ( 'NONE',  ( 6.380167732536218494, -1.162327630155314484, 1.822330041786710098 ) ) ;
#26580 = CARTESIAN_POINT ( 'NONE',  ( 2.285534418239891785, 0.09939759515392716793, -2.118372479656557061 ) ) ;
#26581 = CARTESIAN_POINT ( 'NONE',  ( 6.111974619354628935, -0.6785462737385530296, 1.902425049502977528 ) ) ;
#26582 = CARTESIAN_POINT ( 'NONE',  ( -1.402160292154681736E-14, -0.1781249996585796136, 1.575800808251672791 ) ) ;
#26583 = AXIS2_PLACEMENT_3D ( 'NONE', #210551, #47017, #62187 ) ;
#26584 = CARTESIAN_POINT ( 'NONE',  ( -2.982430605326321427, 6.423326772948587227, -0.7216878364870267237 ) ) ;
#26585 = ADVANCED_FACE ( 'NONE', ( #135345 ), #111958, .T. ) ;
#26588 = CARTESIAN_POINT ( 'NONE',  ( 3.226477370372302644, 5.747678784534228313, 1.082531754730546636 ) ) ;
#26587 = CARTESIAN_POINT ( 'NONE',  ( -1.642778471874998480, -0.4010416661887096224, 2.845375778867863303 ) ) ;
#26586 = CARTESIAN_POINT ( 'NONE',  ( 7.198453214212898743, 7.362893269528701268, 0.7998128361456291469 ) ) ;
#26589 = CARTESIAN_POINT ( 'NONE',  ( -3.169574050544739841, 6.919863168935977527, -0.7998128361456481317 ) ) ;
#26590 = CARTESIAN_POINT ( 'NONE',  ( 5.137907791644652278, 2.014008302827663854, -0.1037760698975112861 ) ) ;
#26592 = CARTESIAN_POINT ( 'NONE',  ( -7.729556973122450714, 8.190440354830551328, 0.000000000000000000 ) ) ;
#26591 = CARTESIAN_POINT ( 'NONE',  ( -9.815740026613967828, 10.55404424057886636, -0.7216878364870267237 ) ) ;
#26593 = CARTESIAN_POINT ( 'NONE',  ( 4.882344714252594642, 4.868692719482363707, 0.000000000000000000 ) ) ;
#26595 = CARTESIAN_POINT ( 'NONE',  ( -1.364683531250014514, 11.33854166700806410, -0.7879004041258335089 ) ) ;
#26594 = CARTESIAN_POINT ( 'NONE',  ( 6.157120911006636277, -1.851533521339579380, -1.115484332758958974 ) ) ;
#26596 = CARTESIAN_POINT ( 'NONE',  ( -10.84254087577847869, 4.919568073182957413, 5.035408296252060545 ) ) ;
#26598 = CARTESIAN_POINT ( 'NONE',  ( 6.503528962204017994, -1.955192063461574259, 0.4926555484118036454 ) ) ;
#26597 = CARTESIAN_POINT ( 'NONE',  ( -5.205967797523171292, 9.017453497178271604, 0.000000000000000000 ) ) ;
#26599 = CARTESIAN_POINT ( 'NONE',  ( -1.364683531250012516, 1.342708333674755616, 0.7879004041258379498 ) ) ;
#26600 = CARTESIAN_POINT ( 'NONE',  ( -11.86239285000045918, 9.719999999999982876, 1.812080536912751061 ) ) ;
#26601 = CARTESIAN_POINT ( 'NONE',  ( 1.500000000000037748, 7.000000000000000000, 10.64483442802188051 ) ) ;
#26602 = CARTESIAN_POINT ( 'NONE',  ( 2.754212737529265986, 0.5811417601193774596, 1.624163882408189652 ) ) ;
#26603 = CARTESIAN_POINT ( 'NONE',  ( 6.210516883511641772, 9.403297576475722508, 1.199719254218452047 ) ) ;
#26604 = CARTESIAN_POINT ( 'NONE',  ( 6.042093733545556233, 7.078139439671806699, -1.199719254218452047 ) ) ;
#26605 = CARTESIAN_POINT ( 'NONE',  ( -0.6823417656250003738, 0.03020833367475134201, -1.181850606188749264 ) ) ;
#26606 = CARTESIAN_POINT ( 'NONE',  ( 1.035986422354659320, 1.742213337529074035, 0.3100009841157587154 ) ) ;
#26607 = CARTESIAN_POINT ( 'NONE',  ( 1.875641098811844154, 0.3420332329174725072, -1.983669356598726674 ) ) ;
#26608 = DIRECTION ( 'NONE',  ( 0.7071067811865489050, 0.000000000000000000, 0.7071067811865462405 ) ) ;
#26609 = CARTESIAN_POINT ( 'NONE',  ( 3.728129053633592704, 4.412200653069714207, -1.082531754730543083 ) ) ;
#26610 = CARTESIAN_POINT ( 'NONE',  ( 4.014836333542094238, 1.562590183666902943, -1.558512549626612342 ) ) ;
#26611 = CARTESIAN_POINT ( 'NONE',  ( 5.120078768083678789, 2.148437930330206136, -0.3118015998682179823 ) ) ;
#26612 = ORIENTED_EDGE ( 'NONE', *, *, #154830, .F. ) ;
#26613 = CARTESIAN_POINT ( 'NONE',  ( 1.499999999999985123, -0.9541666666666493990, -0.8660254037844323793 ) ) ;
#26614 = CARTESIAN_POINT ( 'NONE',  ( 9.219181267168295335, 9.858059021225592744, 1.040834085586084257E-14 ) ) ;
#26616 = CARTESIAN_POINT ( 'NONE',  ( 2.601185598297011570, -0.1948207814224910128, 2.006963067508853005 ) ) ;
#26615 = CARTESIAN_POINT ( 'NONE',  ( 3.457788318579996467, -1.606868461378293755, -1.383752881913953292 ) ) ;
#26618 = ORIENTED_EDGE ( 'NONE', *, *, #54713, .F. ) ;
#26617 = CARTESIAN_POINT ( 'NONE',  ( 3.621195883455626596, 1.556580008595293219, 0.9264731596013916493 ) ) ;
#26619 = CARTESIAN_POINT ( 'NONE',  ( 4.538947565524982686, 8.517465603079630299, 0.000000000000000000 ) ) ;
#26620 = VERTEX_POINT ( 'NONE', #101756 ) ;
#26621 = CARTESIAN_POINT ( 'NONE',  ( 0.5142528298564854605, 1.293200884458247657, -1.351890787750304135 ) ) ;
#26622 = CARTESIAN_POINT ( 'NONE',  ( 5.936143289257818978, 0.8957264799932495025, -1.590785280889392528 ) ) ;
#26624 = CARTESIAN_POINT ( 'NONE',  ( 1.252998012795783822, 0.1371590870133630458, -1.910833894730893601 ) ) ;
#26623 = CARTESIAN_POINT ( 'NONE',  ( -2.605138072120212200, 6.191078184115536232, -0.7998128361456281477 ) ) ;
#26625 = SURFACE_STYLE_USAGE ( .BOTH. , #42911 ) ;
#26626 = CARTESIAN_POINT ( 'NONE',  ( -3.895595285070201808, 2.800000000000024691, 0.7750000000000135669 ) ) ;
#26627 = CARTESIAN_POINT ( 'NONE',  ( 1.364683531249988535, 1.926041667008086211, 0.7879004041258500513 ) ) ;
#26628 = CARTESIAN_POINT ( 'NONE',  ( 6.773846765317306229, 0.000000000000000000, -6.773846765317331986 ) ) ;
#26629 = CARTESIAN_POINT ( 'NONE',  ( 7.349928672384119288, 8.707909884937221179, 1.082531754730549967 ) ) ;
#26630 = CARTESIAN_POINT ( 'NONE',  ( -5.478903473698255588, 7.485416367438324059, -1.443375672974066548 ) ) ;
#26631 = CARTESIAN_POINT ( 'NONE',  ( -6.261886844665283114, 8.398896966899865646, 1.599625672291269396 ) ) ;
#26632 = CARTESIAN_POINT ( 'NONE',  ( 2.496466685713152334, -1.086271176545396067, 1.821091972856798913 ) ) ;
#26634 = CARTESIAN_POINT ( 'NONE',  ( -10.61922739175395236, 7.618143447610075114, 4.514851702475597861 ) ) ;
#26633 = CARTESIAN_POINT ( 'NONE',  ( -0.1296875068447916890, 6.948706544289747988, -2.421546651465163347 ) ) ;
#26635 =( BOUNDED_SURFACE ( )  B_SPLINE_SURFACE ( 3, 2, ( 
 ( #79744, #213975, #130711 ),
 ( #145861, #113392, #80824 ),
 ( #146914, #64568, #65595 ),
 ( #44073, #101315, #99209 ),
 ( #68795, #51516, #2723 ),
 ( #35240, #167396, #182558 ) ),
 .UNSPECIFIED., .F., .F., .T. ) 
 B_SPLINE_SURFACE_WITH_KNOTS ( ( 4, 2, 4 ),
 ( 3, 3 ),
 ( 0.000000000000000000, 0.0003766365702389427796, 0.0007532731404778855592 ),
 ( 0.000000000000000000, 1.000000000000000000 ),
 .UNSPECIFIED. ) 
 GEOMETRIC_REPRESENTATION_ITEM ( )  RATIONAL_B_SPLINE_SURFACE ( (
 ( 1.000000000000000000, 0.7452309222762957264, 1.000000000000000000),
 ( 1.000000000000000000, 0.7451892422671803073, 1.000000000000000000),
 ( 1.000000000000000000, 0.7429606254238495522, 1.000000000000000000),
 ( 1.000000000000000000, 0.7311462761265991039, 1.000000000000000000),
 ( 1.000000000000000000, 0.7212257702791082803, 1.000000000000000000),
 ( 1.000000000000000000, 0.7071067811865475727, 1.000000000000000000) ) ) 
 REPRESENTATION_ITEM ( '' )  SURFACE ( )  );
#26636 = CARTESIAN_POINT ( 'NONE',  ( 4.323478126428228485, -1.887445700180546915, 0.5691147572158322676 ) ) ;
#26637 = CARTESIAN_POINT ( 'NONE',  ( 6.152599605923961157, 1.892562589925715466, 0.2737767527046449101 ) ) ;
#26638 = ORIENTED_EDGE ( 'NONE', *, *, #99699, .F. ) ;
#26639 = VECTOR ( 'NONE', #92054, 1000.000000000000000 ) ;
#26640 = CARTESIAN_POINT ( 'NONE',  ( 6.122275928298587466, 2.094602363090028785, 0.3085360351358697462 ) ) ;
#26641 = CARTESIAN_POINT ( 'NONE',  ( -0.5451172737955251035, 6.555825640206980331, -3.374434186942578684 ) ) ;
#26642 = CARTESIAN_POINT ( 'NONE',  ( 1.152881054890652957, -0.5012615762394446728, -2.008655542368184221 ) ) ;
#26643 = CARTESIAN_POINT ( 'NONE',  ( 3.064326467805338350, -1.794528509343394473, -0.7426413790867588682 ) ) ;
#26644 = ORIENTED_EDGE ( 'NONE', *, *, #42750, .T. ) ;
#26645 = CARTESIAN_POINT ( 'NONE',  ( 5.716698046817569434, 6.698511138489155137, -1.199719254218452047 ) ) ;
#26646 = CARTESIAN_POINT ( 'NONE',  ( 7.225569521440261767, 7.394528961293920233, -0.7998128361456341429 ) ) ;
#26648 = CARTESIAN_POINT ( 'NONE',  ( 6.063521013809720195, 8.097193820909906137, 1.599625672291281386 ) ) ;
#26647 = CARTESIAN_POINT ( 'NONE',  ( 3.609396000958647210, -2.059664220577660743, 0.3575658041875314219 ) ) ;
#26649 = CARTESIAN_POINT ( 'NONE',  ( 3.567203813726949058, 7.175838526074521440, 0.7216878364870257245 ) ) ;
#26651 = EDGE_LOOP ( 'NONE', ( #132755, #109795, #102613, #71124 ) ) ;
#26650 = CARTESIAN_POINT ( 'NONE',  ( 0.4865836442241474602, -1.705128007267729506, -0.6119416708995157883 ) ) ;
#26652 = CARTESIAN_POINT ( 'NONE',  ( 5.602238545945851023, -2.207063162045197924, -0.003355105161521874588 ) ) ;
#26653 = CARTESIAN_POINT ( 'NONE',  ( 3.009610312849396951, 6.452363523749469643, -0.06592220986071165023 ) ) ;
#26654 = CARTESIAN_POINT ( 'NONE',  ( 2.889901548669851383, 1.559680528474843841, 1.561422205034967314 ) ) ;
#26655 = DIRECTION ( 'NONE',  ( -0.7592566023653005702, 0.6507913734559640506, 0.000000000000000000 ) ) ;
#26656 = CARTESIAN_POINT ( 'NONE',  ( 1.506358462150747091, -1.903157483220425883, -0.1863595701613318389 ) ) ;
#26657 = CARTESIAN_POINT ( 'NONE',  ( 7.574201371528760163, 11.98831870009225931, 1.040834085586084257E-14 ) ) ;
#26658 = CARTESIAN_POINT ( 'NONE',  ( 4.809070886388271404, -1.664838503569150419, 1.230558894880565246 ) ) ;
#26660 = CARTESIAN_POINT ( 'NONE',  ( 2.377987466095924152, 1.329388817951412394, 1.704534938537699995 ) ) ;
#26659 = CARTESIAN_POINT ( 'NONE',  ( 9.602438852202270780, -9.449361760816692879, -0.1964824153909916216 ) ) ;
#26661 = CARTESIAN_POINT ( 'NONE',  ( 4.915667883426772633, -1.172277214026868464, -1.851500752446763709 ) ) ;
#26662 = VERTEX_POINT ( 'NONE', #34615 ) ;
#26663 = CARTESIAN_POINT ( 'NONE',  ( 10.55910270694468345, 11.21337466772398095, 0.7998128361456462443 ) ) ;
#26664 = CARTESIAN_POINT ( 'NONE',  ( 0.4379653042624709336, 3.065656782498147770, -0.4195809500674644865 ) ) ;
#26665 = LINE ( 'NONE', #90629, #134168 ) ;
#26666 = CARTESIAN_POINT ( 'NONE',  ( 4.980641328173811999, 6.904110530993182948, 1.599625672291269396 ) ) ;
#26667 = CARTESIAN_POINT ( 'NONE',  ( -3.285556943750000514, -2.676041666188707424, -1.896917185911906722 ) ) ;
#26668 = DIRECTION ( 'NONE',  ( -8.638326563840814399E-31, 0.000000000000000000, -1.000000000000000000 ) ) ;
#26669 = CARTESIAN_POINT ( 'NONE',  ( -9.192064960385334160, 9.826423329978791088, 0.7216878364870438212 ) ) ;
#26671 = CARTESIAN_POINT ( 'NONE',  ( 6.062430963966053632, 7.101866208495718702, -1.199719254218452047 ) ) ;
#26670 = AXIS2_PLACEMENT_3D ( 'NONE', #94989, #212957, #161035 ) ;
#26672 = CARTESIAN_POINT ( 'NONE',  ( 5.963751281166302043, -0.5086355806236466659, 2.006660534352236347 ) ) ;
#26673 = CARTESIAN_POINT ( 'NONE',  ( 4.213445252184796708, -0.3281303603181011108, 1.898201707710310826 ) ) ;
#26674 = EDGE_CURVE ( 'NONE', #45840, #15325, #53000, .T. ) ;
#26675 = CARTESIAN_POINT ( 'NONE',  ( 0.06993570063764525946, -0.9480199632962028611, 1.779638758220257522 ) ) ;
#26676 = DIRECTION ( 'NONE',  ( 0.000000000000000000, 0.000000000000000000, -1.000000000000000000 ) ) ;
#26677 = CARTESIAN_POINT ( 'NONE',  ( 3.798255590122797898, 7.583048621785260401, -0.7998128361456221525 ) ) ;
#26678 = DIRECTION ( 'NONE',  ( -1.000000000000000000, 0.000000000000000000, 0.000000000000000000 ) ) ;
#26679 = CARTESIAN_POINT ( 'NONE',  ( 5.084792200464717915, 1.883391756629303471, 0.5756752826196751549 ) ) ;
#26680 = CARTESIAN_POINT ( 'NONE',  ( 6.650320093084655326, -1.776417932240816011, 1.448308594842239838 ) ) ;
#26681 = CARTESIAN_POINT ( 'NONE',  ( 5.285714101943871590, 1.228958891529348785, 1.350286652578087665 ) ) ;
#26682 = CARTESIAN_POINT ( 'NONE',  ( 5.207740401424913124, 9.089797878388800711, -0.7216878364870458196 ) ) ;
#26683 = CARTESIAN_POINT ( 'NONE',  ( 4.487385655998888723, 4.337630808194552934, 0.7216878364870317197 ) ) ;
#26684 = CARTESIAN_POINT ( 'NONE',  ( -4.308458954092677651, 8.248562223075252220, -0.7998128361456362523 ) ) ;
#26685 = CARTESIAN_POINT ( 'NONE',  ( 5.554000203453580475, 6.508696987897830688, -1.199719254218452047 ) ) ;
#26686 = ORIENTED_EDGE ( 'NONE', *, *, #212483, .F. ) ;
#26688 = CARTESIAN_POINT ( 'NONE',  ( 5.941657920834610529, -1.894198565178412119, 0.6822040374353780523 ) ) ;
#26687 = CARTESIAN_POINT ( 'NONE',  ( 2.120424178990498731, 0.001545453418709194504, 1.841430844159386293 ) ) ;
#26689 = CARTESIAN_POINT ( 'NONE',  ( 0.9666848095895408388, 1.880238891319021111, 1.321614243928259880 ) ) ;
#26690 = CARTESIAN_POINT ( 'NONE',  ( 5.207842308544940124, 0.6190457291245822224, -1.861560318597937913 ) ) ;
#26691 = CARTESIAN_POINT ( 'NONE',  ( -5.259673527097670664, 8.223703984000886535, -1.199719254218446718 ) ) ;
#26692 = CARTESIAN_POINT ( 'NONE',  ( -4.229020061460118107, 7.343517960532632394, -0.8650006913940473385 ) ) ;
#26693 = CARTESIAN_POINT ( 'NONE',  ( -4.810445574750349174, 4.506608013497163334, 0.7998128361456341429 ) ) ;
#26695 = EDGE_CURVE ( 'NONE', #202678, #78316, #86573, .T. ) ;
#26694 = CARTESIAN_POINT ( 'NONE',  ( 0.6255436495894195481, 0.2045281481408110225, -2.060252820462626477 ) ) ;
#26696 = CARTESIAN_POINT ( 'NONE',  ( -4.390861645979385663, 6.216034235099629157, -1.599625672291271394 ) ) ;
#26698 = CARTESIAN_POINT ( 'NONE',  ( 0.1450994221751950586, -1.442925249786636943, -1.190247126510869613 ) ) ;
#26697 = CARTESIAN_POINT ( 'NONE',  ( 1.013356050919094198, -2.038958350640528661, 0.4616950316734638737 ) ) ;
#26699 = CARTESIAN_POINT ( 'NONE',  ( 1.084637062511532246, 2.992628807292006865, 1.105835307554805524 ) ) ;
#26700 = CARTESIAN_POINT ( 'NONE',  ( -1.364683531250012516, 3.342708333674756727, 0.7879004041258379498 ) ) ;
#26701 = CARTESIAN_POINT ( 'NONE',  ( 2.155425581425034487, 0.7450078602235529202, 1.573079536267004030 ) ) ;
#26702 = CARTESIAN_POINT ( 'NONE',  ( 5.473741331615251227, 7.409117525016355010, -1.599625672291262513 ) ) ;
#26704 = CARTESIAN_POINT ( 'NONE',  ( 1.534404370307017595, 8.695807324171010322, 2.514078760162040904 ) ) ;
#26703 = DIRECTION ( 'NONE',  ( -0.000000000000000000, -1.000000000000000000, 0.000000000000000000 ) ) ;
#26705 = CARTESIAN_POINT ( 'NONE',  ( 3.053030289171186684, -1.410389792183571966, -0.9926723171444253868 ) ) ;
#26706 = CARTESIAN_POINT ( 'NONE',  ( 2.454835928891830221, -1.908367152989149718, -1.077367144120815023 ) ) ;
#26707 = CARTESIAN_POINT ( 'NONE',  ( 5.777994779145079640, 1.311685685134782231, 1.774619457157788904 ) ) ;
#26708 = CARTESIAN_POINT ( 'NONE',  ( -11.30309668167796922, 5.150585336095395483, -5.742054036728553967 ) ) ;
#26709 = AXIS2_PLACEMENT_3D ( 'NONE', #107982, #110116, #92754 ) ;
#26710 = CARTESIAN_POINT ( 'NONE',  ( 2.219799714087321796, 0.3745715905324221162, -2.138378345340052444 ) ) ;
#26711 = CARTESIAN_POINT ( 'NONE',  ( 0.7151340513122245168, -0.2707656271505008982, 1.805370379145049275 ) ) ;
#26712 = CARTESIAN_POINT ( 'NONE',  ( 3.696581757058306383, 1.494387559712303526, -1.500228622805776624 ) ) ;
#26713 = CARTESIAN_POINT ( 'NONE',  ( 6.539320575229274901, 7.053161517996441532, 2.494893549996656912 ) ) ;
#26714 = VERTEX_POINT ( 'NONE', #84436 ) ;
#26716 = CARTESIAN_POINT ( 'NONE',  ( 0.6823417656249899377, 1.655208333674752730, 1.181850606188755259 ) ) ;
#26715 = CARTESIAN_POINT ( 'NONE',  ( 3.263489799031735750, 2.236134436263835568, -0.5039766086074470852 ) ) ;
#26717 = CARTESIAN_POINT ( 'NONE',  ( 0.000000000000000000, -5.166862915010159263, 0.000000000000000000 ) ) ;
#26718 = CARTESIAN_POINT ( 'NONE',  ( 4.650610384687404952, 5.384465856012134566, 1.199719254218462483 ) ) ;
#26719 = AXIS2_PLACEMENT_3D ( 'NONE', #191667, #174400, #96351 ) ;
#26720 = CARTESIAN_POINT ( 'NONE',  ( 6.129551335524713096, -0.2748284885467215943, 2.204153950570774345 ) ) ;
#26721 = CARTESIAN_POINT ( 'NONE',  ( -5.802526556968872207, 6.832331073627524454, 1.082531754730548412 ) ) ;
#26722 = CARTESIAN_POINT ( 'NONE',  ( 3.172244755917638770, 5.684407401003788607, -1.082531754730543083 ) ) ;
#26723 = CARTESIAN_POINT ( 'NONE',  ( -6.602457619730773608, 8.725953194484466380, 1.443375672974078761 ) ) ;
#26724 = ADVANCED_FACE ( 'NONE', ( #70292 ), #202424, .F. ) ;
#26725 = ORIENTED_EDGE ( 'NONE', *, *, #179909, .T. ) ;
#26726 = CARTESIAN_POINT ( 'NONE',  ( 4.588517629802620235, -0.5350896943857390564, 1.944070981013111155 ) ) ;
#26728 = CARTESIAN_POINT ( 'NONE',  ( 3.168856051829985532, 1.497182195067780386, -1.418930203433153903 ) ) ;
#26727 = CARTESIAN_POINT ( 'NONE',  ( 4.788000803920411386, 8.737751371215816576, 1.040834085586084257E-14 ) ) ;
#26729 = CARTESIAN_POINT ( 'NONE',  ( 8.018721507839716267, 8.319872945426633137, -0.7998128361456341429 ) ) ;
#26730 = CARTESIAN_POINT ( 'NONE',  ( 5.031484404002891431, 5.042689024191078673, 0.7216878364870328300 ) ) ;
#26731 = CARTESIAN_POINT ( 'NONE',  ( -3.285556943750000514, -3.638541666188706891, -1.896917185911906500 ) ) ;
#26732 = CARTESIAN_POINT ( 'NONE',  ( 1.364683531249988535, 5.655208333674751842, -0.7879004041258300672 ) ) ;
#26733 = CARTESIAN_POINT ( 'NONE',  ( 5.929655999079199269, 1.083026401007038952, -1.905042663481799403 ) ) ;
#26734 = CARTESIAN_POINT ( 'NONE',  ( 3.955704058034177351, -1.882473782773282700, -0.7231407674024927790 ) ) ;
#26735 = CARTESIAN_POINT ( 'NONE',  ( 2.700538275128167687, 1.556679782967337999, 0.9830204120172959525 ) ) ;
#26736 = AXIS2_PLACEMENT_3D ( 'NONE', #99710, #136491, #101841 ) ;
#26737 = CARTESIAN_POINT ( 'NONE',  ( 7.467843683028853263, 7.606905806488803101, 0.7998128361456341429 ) ) ;
#26738 = CARTESIAN_POINT ( 'NONE',  ( 6.352569596097208837, 0.5757234290239590102, 1.732508359437078482 ) ) ;
#26739 = CARTESIAN_POINT ( 'NONE',  ( -6.527360889975461156, 9.702672574024962415, 1.199719254218452047 ) ) ;
#26741 = CARTESIAN_POINT ( 'NONE',  ( -6.140917232347002042, 6.129101290685087911, -0.7998128361456362523 ) ) ;
#26740 = CARTESIAN_POINT ( 'NONE',  ( 5.928679764299940480, 2.178688510132809064, 0.6099592146414765104 ) ) ;
#26742 = CARTESIAN_POINT ( 'NONE',  ( 1.612088513325710126, -2.090005036333367539, 0.2590644908504329824 ) ) ;
#26743 = CARTESIAN_POINT ( 'NONE',  ( -6.635789839245807897, 6.706452665400368218, 0.7998128361456341429 ) ) ;
#26744 = CARTESIAN_POINT ( 'NONE',  ( 8.697719238366680372, 10.10609285197134533, 1.199719254218462483 ) ) ;
#26745 = CARTESIAN_POINT ( 'NONE',  ( 6.170369307550806148, 10.21286493553572328, 0.7216878364870317197 ) ) ;
#26746 =( LENGTH_UNIT ( ) NAMED_UNIT ( * ) SI_UNIT ( .MILLI., .METRE. ) );
#26747 = B_SPLINE_CURVE_WITH_KNOTS ( 'NONE', 3,
 ( #110888, #125027, #108758, #192049, #190984, #79389 ),
 .UNSPECIFIED., .F., .F.,
 ( 4, 2, 4 ),
 ( 0.001373143222731355991, 0.001435267353687973493, 0.001497391484644590995 ),
 .UNSPECIFIED. ) ;
#26748 = CARTESIAN_POINT ( 'NONE',  ( -8.538937818508475885, 8.856515631215026829, 1.040834085586084257E-14 ) ) ;
#26749 = CARTESIAN_POINT ( 'NONE',  ( -3.771179864959864680, 7.354219769063552015, -0.6724184775293801097 ) ) ;
#26750 = CARTESIAN_POINT ( 'NONE',  ( 6.927853306458743532, 9.105581495667113501, 1.443375672974076540 ) ) ;
#26751 = CARTESIAN_POINT ( 'NONE',  ( 4.078932850288060408, 7.722175824222965446, -0.6089670364913578604 ) ) ;
#26752 = CARTESIAN_POINT ( 'NONE',  ( -3.438964519360665051, 7.163875705896082913, -0.7998128361456281477 ) ) ;
#26753 = CARTESIAN_POINT ( 'NONE',  ( 2.918465973627711652, -2.218669909917521998, 0.1131645065166643205 ) ) ;
#26754 = CARTESIAN_POINT ( 'NONE',  ( 0.03028722099337673168, -1.361824662662258767, -1.737358624739212543 ) ) ;
#26755 = CARTESIAN_POINT ( 'NONE',  ( -6.784929528996132220, 6.880448970109080520, 0.000000000000000000 ) ) ;
#26756 = CARTESIAN_POINT ( 'NONE',  ( 6.484877546038077867, 6.460111979999551224, 1.040834085586084257E-14 ) ) ;
#26757 = CARTESIAN_POINT ( 'NONE',  ( 4.070719198475009293, 1.388998261151509039, -1.385754695631277844 ) ) ;
#26758 = CARTESIAN_POINT ( 'NONE',  ( 8.890396042259068210, 11.39521468743417998, -1.599625672291257406 ) ) ;
#26759 = CARTESIAN_POINT ( 'NONE',  ( -4.774234299259712877, 6.798759937490593153, 1.242976086189879759 ) ) ;
#26760 = CARTESIAN_POINT ( 'NONE',  ( 9.364998556596795254, 13.54474674066948481, 7.374496730960012236 ) ) ;
#26761 = CARTESIAN_POINT ( 'NONE',  ( 1.364683531249988757, 0.3843750003414206362, 0.000000000000000000 ) ) ;
#26762 = CARTESIAN_POINT ( 'NONE',  ( -5.478903473698260029, 6.525047153136981137, -1.082531754730549967 ) ) ;
#26764 = EDGE_LOOP ( 'NONE', ( #482, #82600, #143384, #88275 ) ) ;
#26763 = CARTESIAN_POINT ( 'NONE',  ( -5.097502569058207200, 8.890910730635814829, -0.7216878364870207285 ) ) ;
#26765 = CARTESIAN_POINT ( 'NONE',  ( 4.025719079702368752, -0.3592959752154977204, 2.089770972018199835 ) ) ;
#26766 = CARTESIAN_POINT ( 'NONE',  ( -6.134138155540168391, 6.121192367743780949, 0.000000000000000000 ) ) ;
#26767 = CARTESIAN_POINT ( 'NONE',  ( 4.293933718354110418, -0.8299404887524584051, 1.996233173270183681 ) ) ;
#26768 = CARTESIAN_POINT ( 'NONE',  ( 3.808014051635350672, 1.299385917162833692, -1.304790556973287163 ) ) ;
#26769 = CARTESIAN_POINT ( 'NONE',  ( 4.839077477813122918, -1.706110771555340744, -1.074664961451990308 ) ) ;
#26770 = CARTESIAN_POINT ( 'NONE',  ( -5.028543871580710700, 6.592580098690584478, 1.235119876028653918 ) ) ;
#26771 = CARTESIAN_POINT ( 'NONE',  ( -1.402160292154681736E-14, 0.6343750003414162508, 1.575800808251672791 ) ) ;
#26772 = CARTESIAN_POINT ( 'NONE',  ( 6.298757997817161502, 1.451094931915532404, 0.9604431249435537721 ) ) ;
#26773 = CARTESIAN_POINT ( 'NONE',  ( 3.334942599281629949, 5.874221551595115720, -1.082531754730543083 ) ) ;
#26774 = CARTESIAN_POINT ( 'NONE',  ( 1.499999999999993117, 11.85416666666666430, 0.8660254037844408170 ) ) ;
#26775 = CARTESIAN_POINT ( 'NONE',  ( 3.467792127863758456, 2.109446376165153847, -0.4717452660116944196 ) ) ;
#26776 = CARTESIAN_POINT ( 'NONE',  ( 5.975935433960425591, 1.776740614516297390, 0.9528632009266968517 ) ) ;
#26777 = CARTESIAN_POINT ( 'NONE',  ( -8.487040972030346353, 9.003895343564625620, 1.040834085586084257E-14 ) ) ;
#26778 = CARTESIAN_POINT ( 'NONE',  ( 2.887745953747706373, 1.527789104365802286, 1.529575784674996886 ) ) ;
#26779 = CARTESIAN_POINT ( 'NONE',  ( 3.268780567936521830, -1.820120084945201500, -0.7576984602858954920 ) ) ;
#26780 = CARTESIAN_POINT ( 'NONE',  ( 0.7105614292102403473, -2.296071549169254489, 0.2300874200455073904 ) ) ;
#26781 = CARTESIAN_POINT ( 'NONE',  ( 5.003436869212060323, -1.932333990966347503, 0.1943045992871711702 ) ) ;
#26784 = EDGE_LOOP ( 'NONE', ( #63024, #33922, #49454, #195898 ) ) ;
#26783 = CARTESIAN_POINT ( 'NONE',  ( -1.217358635584816495, 3.139784080462332927, 0.7750000000000083489 ) ) ;
#26782 = CARTESIAN_POINT ( 'NONE',  ( -8.554831740098665094, 11.00372300158037042, 1.443375672974064550 ) ) ;
#26785 = CARTESIAN_POINT ( 'NONE',  ( -6.282224075085783177, 8.422623735723785643, 1.599625672291269396 ) ) ;
#26786 = CARTESIAN_POINT ( 'NONE',  ( 0.07999999999998980149, -5.907420853759267843, -10.91970695577493800 ) ) ;
#26788 = VERTEX_POINT ( 'NONE', #68160 ) ;
#26787 = CARTESIAN_POINT ( 'NONE',  ( -5.492988512192097161, 6.437516681426083132, 1.199719254218452935 ) ) ;
#26789 = CARTESIAN_POINT ( 'NONE',  ( -8.324343128666356506, 8.814081192973304724, 1.040834085586084257E-14 ) ) ;
#26790 = CARTESIAN_POINT ( 'NONE',  ( 2.450463542074859724, 2.206263077450395738, 0.05474276496272853509 ) ) ;
#26791 = CARTESIAN_POINT ( 'NONE',  ( 3.285556943749998737, -0.6052083328553753416, -1.896917185911906500 ) ) ;
#26792 = CARTESIAN_POINT ( 'NONE',  ( 6.561383603009730336, 1.629167342741120406, 1.092533971175007723 ) ) ;
#26793 = CARTESIAN_POINT ( 'NONE',  ( -1.364683531249997417, 5.571875000341417916, 1.214306433183764966E-14 ) ) ;
#26794 = CARTESIAN_POINT ( 'NONE',  ( -1.201851678989727383E-14, 4.118750000682818602, -1.732050807568863648 ) ) ;
#26795 = CARTESIAN_POINT ( 'NONE',  ( 4.408913874118179699, 7.341020650511065782, -1.198271334459002802 ) ) ;
#26798 = CIRCLE ( 'NONE', #213554, 11.92000000000000171 ) ;
#26797 = CARTESIAN_POINT ( 'NONE',  ( 0.000000000000000000, 5.000000000000000888, 0.000000000000000000 ) ) ;
#26796 = CARTESIAN_POINT ( 'NONE',  ( 0.1749903794560228876, 5.724274800596795387, -2.549334106949477263 ) ) ;
#26799 = CARTESIAN_POINT ( 'NONE',  ( 5.788959344212086577, 1.397023377451442228, 1.199316859253784839 ) ) ;
#26800 = ORIENTED_EDGE ( 'NONE', *, *, #166752, .T. ) ;
#26801 = TRIMMED_CURVE ( 'NONE', #107431, ( PARAMETER_VALUE ( 0.000000000000000000 ), #41697 ), ( PARAMETER_VALUE ( 0.8956647938578647938 ), #38470 ), .T., .PARAMETER. ) ;
#26802 = CARTESIAN_POINT ( 'NONE',  ( 0.6801582343749883464, -0.6927083329919120347, -1.178068619123862515 ) ) ;
#26803 = UNCERTAINTY_MEASURE_WITH_UNIT (LENGTH_MEASURE( 1.000000000000000082E-05 ), #181442, 'distance_accuracy_value', 'NONE');
#26804 = CARTESIAN_POINT ( 'NONE',  ( -5.506582945444718824, 9.576097202994168001, 0.7998128361456481317 ) ) ;
#26805 = SURFACE_STYLE_FILL_AREA ( #121202 ) ;
#26806 = CARTESIAN_POINT ( 'NONE',  ( 6.187751663909415001, 2.028806014889028120, -0.6170373231123224000 ) ) ;
#26807 = CARTESIAN_POINT ( 'NONE',  ( 11.05652804041138282, 8.011784944665652830, -4.552175959553207640 ) ) ;
#26808 = CARTESIAN_POINT ( 'NONE',  ( 5.497994985541524215, 6.373081223675282736, -1.199719254218445830 ) ) ;
#26809 = CARTESIAN_POINT ( 'NONE',  ( 0.3564142383026321914, 0.7882222137287850927, 1.904402214580179331 ) ) ;
#26812 = CARTESIAN_POINT ( 'NONE',  ( 4.493604616018744835, -1.840970053361364656, -0.04044509776383875543 ) ) ;
#26811 = CARTESIAN_POINT ( 'NONE',  ( 2.049040314030759369, 1.621234533420016888, -0.9136741289750174300 ) ) ;
#26810 = CARTESIAN_POINT ( 'NONE',  ( -10.49167311136684688, 5.343773310534623455, 5.730690286876302331 ) ) ;
#26813 = CARTESIAN_POINT ( 'NONE',  ( 5.770966940911189447, 9.884545197705074671, -0.7998128361456291469 ) ) ;
#26814 = CARTESIAN_POINT ( 'NONE',  ( -9.472340321242439742, 14.62753308518765571, -7.367375265402272611 ) ) ;
#26815 = CARTESIAN_POINT ( 'NONE',  ( -4.945692173934974178, 8.992000979557944973, 0.000000000000000000 ) ) ;
#26816 = ORIENTED_EDGE ( 'NONE', *, *, #176013, .F. ) ;
#26817 = CARTESIAN_POINT ( 'NONE',  ( 4.740968412965463230, 0.3751893352213676591, 2.174603215771487630 ) ) ;
#26818 = CARTESIAN_POINT ( 'NONE',  ( 6.257125660641059461, -1.935629482380639033, -1.171090987803388606 ) ) ;
#26819 = CARTESIAN_POINT ( 'NONE',  ( -5.205967797967562483, 8.057084283395347768, 1.082531754730548412 ) ) ;
#26820 = CARTESIAN_POINT ( 'NONE',  ( 6.521734044569575062, -0.3839667898355834663, 1.776778520094610903 ) ) ;
#26821 = CARTESIAN_POINT ( 'NONE',  ( 6.315652784560811916, -1.257152391787072387, -1.445590397462018117 ) ) ;
#26822 = CARTESIAN_POINT ( 'NONE',  ( 3.903294069008342415, 8.999999999999998224, 0.7749999999999996891 ) ) ;
#26823 = EDGE_CURVE ( 'NONE', #111346, #120494, #125409, .T. ) ;
#26824 = FACE_OUTER_BOUND ( 'NONE', #2870, .T. ) ;
#26825 = CARTESIAN_POINT ( 'NONE',  ( 5.338497774373327509, 1.135723818413657549, -1.538349510941657838 ) ) ;
#26826 = DIRECTION ( 'NONE',  ( 1.000000000000000000, 0.000000000000000000, 0.000000000000000000 ) ) ;
#26827 = CARTESIAN_POINT ( 'NONE',  ( 1.252583056964752029, -1.476889893665521925, 1.148006582770304096 ) ) ;
#26828 = VECTOR ( 'NONE', #15734, 1000.000000000000000 ) ;
#26829 = CARTESIAN_POINT ( 'NONE',  ( 2.096888995370162156, 1.803417055948232761, 0.9023429676050932491 ) ) ;
#26831 = CARTESIAN_POINT ( 'NONE',  ( 3.738982163358902877, 0.3088429966837880070, 2.083174605729753992 ) ) ;
#26830 = CARTESIAN_POINT ( 'NONE',  ( -8.829384350997580455, 11.32403438096243775, 1.599625672291269396 ) ) ;
#26832 = CARTESIAN_POINT ( 'NONE',  ( 6.272618624616828953, 10.46980549536166016, 1.040834085586084257E-14 ) ) ;
#26834 = CARTESIAN_POINT ( 'NONE',  ( -7.557780564614042795, 10.90482886110335414, -1.199719254218446718 ) ) ;
#26833 = CARTESIAN_POINT ( 'NONE',  ( 0.7499999999999885647, -0.5166666666666444030, 1.299038105676657340 ) ) ;
#26835 = FACE_OUTER_BOUND ( 'NONE', #177169, .T. ) ;
#26836 = CARTESIAN_POINT ( 'NONE',  ( 3.111586589114573975, 1.594763109418888991, 1.239388640070989478 ) ) ;
#26837 = CARTESIAN_POINT ( 'NONE',  ( 0.6823417656249917140, 3.842708333674754506, 1.181850606188765695 ) ) ;
#26838 = CARTESIAN_POINT ( 'NONE',  ( 4.356247428692526569, 3.976710176429713250, 0.7998128361456341429 ) ) ;
#26839 = CARTESIAN_POINT ( 'NONE',  ( 3.989662644735529451, 1.562606173494068829, 1.493797087085822595 ) ) ;
#26840 = CARTESIAN_POINT ( 'NONE',  ( 11.18654035131437219, 1.000000000000000888, -4.041720556560823852 ) ) ;
#26841 = CARTESIAN_POINT ( 'NONE',  ( -1.001543065824772872E-14, 5.212500000000019895, 1.732050807568877637 ) ) ;
#26842 = CARTESIAN_POINT ( 'NONE',  ( 5.481239241674765950, 9.616805891921051952, -0.7998128361456481317 ) ) ;
#26843 = CARTESIAN_POINT ( 'NONE',  ( 8.907343734053986495, 9.494248565925552441, -0.7216878364870197293 ) ) ;
#26845 = CARTESIAN_POINT ( 'NONE',  ( 8.031406801462809497, 15.33901600305085822, -8.917679673117250516 ) ) ;
#26844 = CARTESIAN_POINT ( 'NONE',  ( 1.733130889747940495, -2.061367544037566280, -0.6818780404978814769 ) ) ;
#26847 = CARTESIAN_POINT ( 'NONE',  ( 0.8723036553972834950, -0.04505207493780280514, -1.840872848514919502 ) ) ;
#26846 = CARTESIAN_POINT ( 'NONE',  ( -5.748293942514169252, 9.650167333001109071, -0.7216878364870207285 ) ) ;
#26848 = CARTESIAN_POINT ( 'NONE',  ( 0.6823417656249882723, 2.676041667008084879, -1.181850606188749264 ) ) ;
#26849 = CARTESIAN_POINT ( 'NONE',  ( 2.542740116143254792, -1.820367712357463974, 1.220030464664762393 ) ) ;
#26850 = CYLINDRICAL_SURFACE ( 'NONE', #195076, 0.7499999999999997780 ) ;
#26851 = CARTESIAN_POINT ( 'NONE',  ( 3.169090989670137581, -2.089828869452925009, -0.8673982956902188679 ) ) ;
#26852 = CARTESIAN_POINT ( 'NONE',  ( -6.449928391799210736, 8.548002428564306143, -1.599625672291263179 ) ) ;
#26853 = CARTESIAN_POINT ( 'NONE',  ( -0.6823417656250212460, 5.363541667008087543, 1.181850606188767472 ) ) ;
#26854 = CARTESIAN_POINT ( 'NONE',  ( 4.909045613421183063, 8.010784895652180992, 0.9812996480243344477 ) ) ;
#26855 = CARTESIAN_POINT ( 'NONE',  ( -1.402160292154681736E-14, 11.81250000000000000, 1.732050807568881190 ) ) ;
#26856 = CARTESIAN_POINT ( 'NONE',  ( 5.546694241766559230, 9.485244025454063532, 0.000000000000000000 ) ) ;
#26857 = CARTESIAN_POINT ( 'NONE',  ( 4.305725593384774896, -1.765090080884828661, 0.1286423764911871492 ) ) ;
#26858 = CIRCLE ( 'NONE', #199852, 11.92000000000000171 ) ;
#26859 = CARTESIAN_POINT ( 'NONE',  ( 9.097684769969825780, 10.57271930550834860, -1.199719254218446718 ) ) ;
#26860 = CARTESIAN_POINT ( 'NONE',  ( 1.114449138222296742, -0.9466070430152218051, -1.881282081674582995 ) ) ;
#26863 = ADVANCED_FACE ( 'NONE', ( #109293 ), #73363, .T. ) ;
#26862 = CARTESIAN_POINT ( 'NONE',  ( 1.499999999999987121, 1.295833333333353377, -0.8660254037844253849 ) ) ;
#26861 = CARTESIAN_POINT ( 'NONE',  ( -1.364683531250000748, 10.10937500034139802, 0.000000000000000000 ) ) ;
#26864 = CARTESIAN_POINT ( 'NONE',  ( -5.093022980588950865, 5.970890227889075419, -1.199719254218453823 ) ) ;
#26865 = CARTESIAN_POINT ( 'NONE',  ( 6.362907676916636390, -0.1017654035869921675, -2.013986322929907757 ) ) ;
#26866 = ORIENTED_EDGE ( 'NONE', *, *, #124486, .T. ) ;
#26867 = CARTESIAN_POINT ( 'NONE',  ( 6.588899466561449536, 9.670504563421618016, -1.082531754730537088 ) ) ;
#26868 = AXIS2_PLACEMENT_3D ( 'NONE', #115909, #165667, #194971 ) ;
#26869 = CARTESIAN_POINT ( 'NONE',  ( 9.073431116043567002, 11.60875560684942265, -1.599625672291262513 ) ) ;
#26870 = CARTESIAN_POINT ( 'NONE',  ( 3.625732356982212412, -1.113523340526129335, -1.502988901547596567 ) ) ;
#26871 = CARTESIAN_POINT ( 'NONE',  ( 4.065334711822697678, 1.773058433220272789, 1.068561072119569744 ) ) ;
#26872 = CARTESIAN_POINT ( 'NONE',  ( -6.794044373779495771, 8.059378203231773341, 1.082531754730549078 ) ) ;
#26873 = CARTESIAN_POINT ( 'NONE',  ( -0.7500000000000006661, 10.73958333401613174, -1.299038105676657340 ) ) ;
#26874 = CARTESIAN_POINT ( 'NONE',  ( 7.944187942603509356, 11.35563746875774882, 1.199719254218460707 ) ) ;
#26875 = CARTESIAN_POINT ( 'NONE',  ( -5.056828107772880720, 5.001980335264189392, -0.7216878364870142892 ) ) ;
#26876 = CARTESIAN_POINT ( 'NONE',  ( 6.047819040147648373, 9.213483425884394507, 1.199719254218452047 ) ) ;
#26877 = EDGE_CURVE ( 'NONE', #182051, #73782, #170053, .T. ) ;
#26878 = DIRECTION ( 'NONE',  ( 0.000000000000000000, -1.000000000000000000, 0.000000000000000000 ) ) ;
#26879 = CARTESIAN_POINT ( 'NONE',  ( -1.201851678989727383E-14, 5.509375000341415252, -1.575800808251660134 ) ) ;
#26880 = CARTESIAN_POINT ( 'NONE',  ( 3.754310534785664899, -1.959519245081872585, -0.09869234604030494018 ) ) ;
#26881 = CARTESIAN_POINT ( 'NONE',  ( 2.372422516638694745, -0.4444355326964634090, 1.966343308868031103 ) ) ;
#26882 = CARTESIAN_POINT ( 'NONE',  ( -2.959422669532919326, 6.674686557755516780, 0.7998128361456352531 ) ) ;
#26883 = CARTESIAN_POINT ( 'NONE',  ( 6.639320575229253230, 6.038193673056964528, 2.491643636677738360 ) ) ;
#26884 = CARTESIAN_POINT ( 'NONE',  ( 0.7548939078372005618, -1.576849831105286537, -1.005952255950369301 ) ) ;
#26885 = CARTESIAN_POINT ( 'NONE',  ( -1.364683531249997417, 4.009375000341424133, 1.214306433183764966E-14 ) ) ;
#26886 = CARTESIAN_POINT ( 'NONE',  ( 3.217044422572811424, 1.584514289383936347, -1.241758421991135064 ) ) ;
#26888 = CARTESIAN_POINT ( 'NONE',  ( 3.251669871774115705, 2.065089526129770814, -0.4662906127247400945 ) ) ;
#26887 = CARTESIAN_POINT ( 'NONE',  ( -6.588899466561478846, 6.789396920517583922, 0.7216878364870317197 ) ) ;
#26889 = CARTESIAN_POINT ( 'NONE',  ( 9.117697077661663485, 4.000000000000000888, 7.300000000000000711 ) ) ;
#26890 = CARTESIAN_POINT ( 'NONE',  ( 5.371561628297467195, -0.3073141173523045167, 2.047320497149993646 ) ) ;
#26891 = CARTESIAN_POINT ( 'NONE',  ( 6.831329296439236032, 9.063246493969506545, -1.599625672291267398 ) ) ;
#26893 = CARTESIAN_POINT ( 'NONE',  ( 3.891353782322113375, 4.498666486585943147, -1.199719254218446718 ) ) ;
#26892 = CARTESIAN_POINT ( 'NONE',  ( 0.2575178465553956686, 2.067414111102347185, -0.3107122069949171395 ) ) ;
#26895 = ORIENTED_EDGE ( 'NONE', *, *, #121307, .F. ) ;
#26894 = CARTESIAN_POINT ( 'NONE',  ( 5.403274641334286699, 1.493489847867332854, 1.049580640413529276 ) ) ;
#26896 = CARTESIAN_POINT ( 'NONE',  ( 8.925345196497941558, 9.307324238869423283, 1.040834085586084257E-14 ) ) ;
#26897 = CARTESIAN_POINT ( 'NONE',  ( -3.231779075379149546, 6.036511184309975242, 0.9899555337401846344 ) ) ;
#26898 = CARTESIAN_POINT ( 'NONE',  ( 11.25411745265349239, 9.324508674553577237, -3.753762932364714811 ) ) ;
#26899 = CARTESIAN_POINT ( 'NONE',  ( -10.90754186426655004, 4.636108433425621733, 4.485516275142084730 ) ) ;
#26900 = CARTESIAN_POINT ( 'NONE',  ( 0.6823417656249969321, 11.58854166700806765, -1.181850606188757036 ) ) ;
#26901 = CARTESIAN_POINT ( 'NONE',  ( -0.04078422793344065045, -1.398654746659812043, -1.150989216800960335 ) ) ;
#26902 = CARTESIAN_POINT ( 'NONE',  ( -9.318531651294266638, 9.766041769465124034, -0.7998128361456291469 ) ) ;
#26903 = CARTESIAN_POINT ( 'NONE',  ( 4.808338034340912337, 8.761478140039733020, 1.040834085586084257E-14 ) ) ;
#26904 = CARTESIAN_POINT ( 'NONE',  ( 1.360316468749971586, 2.567708333674758148, -0.7853790794159302147 ) ) ;
#26905 = CARTESIAN_POINT ( 'NONE',  ( 4.677199806590210507, 4.559080650551097236, -0.7216878364870197293 ) ) ;
#26906 = CARTESIAN_POINT ( 'NONE',  ( 4.090809663021327758, 5.795697244990093644, 1.599625672291267398 ) ) ;
#26907 = VERTEX_POINT ( 'NONE', #26889 ) ;
#26908 = CARTESIAN_POINT ( 'NONE',  ( -5.074494633264801990, 9.142270515442742607, 0.7998128361456291469 ) ) ;
#26910 = CARTESIAN_POINT ( 'NONE',  ( 6.964048179274811012, 8.153752959689313684, 1.199719254218452047 ) ) ;
#26909 = CARTESIAN_POINT ( 'NONE',  ( 0.03130284803985262237, -9.439835433791190056, -9.605218923937751896 ) ) ;
#26911 = PRESENTATION_STYLE_ASSIGNMENT (( #123463 ) ) ;
#26912 = CARTESIAN_POINT ( 'NONE',  ( 0.1399997263885795207, 2.876830203203218694, -2.488333633689450597 ) ) ;
#26913 = CARTESIAN_POINT ( 'NONE',  ( -5.748293942514180799, 7.729428904398431222, -1.443375672974052559 ) ) ;
#26914 = CARTESIAN_POINT ( 'NONE',  ( 3.009020027229115879, 5.597941567487558778, -1.199719254218446718 ) ) ;
#26915 = CARTESIAN_POINT ( 'NONE',  ( 2.342574202377019521, -1.930441307185966515, -0.3890957575964202886 ) ) ;
#26916 = CARTESIAN_POINT ( 'NONE',  ( 3.638296137631126914, 0.7283958097016438593, 1.880429543521966007 ) ) ;
#26917 = CARTESIAN_POINT ( 'NONE',  ( -8.694856585065634746, 9.038420858865048757, 0.7998128361456462443 ) ) ;
#26918 = CARTESIAN_POINT ( 'NONE',  ( 6.827182134110235445, 0.5726250382554041174, 2.141766166723162002 ) ) ;
#26919 = CARTESIAN_POINT ( 'NONE',  ( 3.539196308827243787, -1.659330947522210886, -1.431560661003590695 ) ) ;
#26920 = CARTESIAN_POINT ( 'NONE',  ( -1.123270288250318494, 3.235197346350006331, -0.7749999999993560929 ) ) ;
#26921 = CARTESIAN_POINT ( 'NONE',  ( 1.975490806028988633, 1.844176287694970995, -0.5568081592420818238 ) ) ;
#26922 = CARTESIAN_POINT ( 'NONE',  ( -8.995998617867369873, 10.45408546138876993, 1.199719254218462483 ) ) ;
#26923 = CARTESIAN_POINT ( 'NONE',  ( 1.217358635584785631, 3.066465920220505570, 0.7750000000000065725 ) ) ;
#26924 = CARTESIAN_POINT ( 'NONE',  ( 0.2329586101569346424, 2.887341434808698981, -2.334705299551639079 ) ) ;
#26925 = CARTESIAN_POINT ( 'NONE',  ( 11.78331023100045627, 9.799999999999982947, 1.799999999999999600 ) ) ;
#26926 = CARTESIAN_POINT ( 'NONE',  ( 8.294891053462476904, 8.571794405328034827, 1.040834085586084257E-14 ) ) ;
#26927 = CARTESIAN_POINT ( 'NONE',  ( 6.010342169559767633, 5.906487374108181143, -0.7998128361456281477 ) ) ;
#26928 = CARTESIAN_POINT ( 'NONE',  ( -6.880414557363809358, -8.057948861126629225, 6.598949805828049797 ) ) ;
#26929 = CARTESIAN_POINT ( 'NONE',  ( 4.556949027968946631, 8.330541276023501140, -0.7216878364870357165 ) ) ;
#26930 = ORIENTED_EDGE ( 'NONE', *, *, #183143, .F. ) ;
#26932 = CARTESIAN_POINT ( 'NONE',  ( 2.596342214666306880, -1.033070880159161264, 1.727660946855133606 ) ) ;
#26931 = CARTESIAN_POINT ( 'NONE',  ( 5.952668924537682038, -1.582617586749142102, -0.9407850039931386910 ) ) ;
#26933 = CARTESIAN_POINT ( 'NONE',  ( 4.112918304081806475, 0.7786346584819616723, -2.162581562504022337 ) ) ;
#26935 = CARTESIAN_POINT ( 'NONE',  ( 2.078732565759545903, 1.734175166166322501, 0.6755533923482255343 ) ) ;
#26934 = CARTESIAN_POINT ( 'NONE',  ( -0.02900071798683095947, 1.997299723774683455, -2.587491137808914488 ) ) ;
#26936 = CARTESIAN_POINT ( 'NONE',  ( 0.000000000000000000, -0.8968749995220406390, -3.793834371823813001 ) ) ;
#26937 = CARTESIAN_POINT ( 'NONE',  ( -9.261794192842831563, -6.948429295162966035, 5.421010862427522170E-16 ) ) ;
#26938 = CARTESIAN_POINT ( 'NONE',  ( 10.15369940311294350, 1.000000000000000888, 6.195664267729887875 ) ) ;
#26939 = CARTESIAN_POINT ( 'NONE',  ( -6.832419346282942563, 10.05857410638369487, 1.199719254218453823 ) ) ;
#26940 = EDGE_CURVE ( 'NONE', #59934, #15524, #20191, .T. ) ;
#26941 = CARTESIAN_POINT ( 'NONE',  ( -6.129694847154222970, 7.284303755502281597, -1.082531754730549967 ) ) ;
#26943 = CARTESIAN_POINT ( 'NONE',  ( 3.994877460428855276, 1.580554378303768992, -1.000287695324620252 ) ) ;
#26942 = CARTESIAN_POINT ( 'NONE',  ( 5.407793395736015363, -0.9409669688741102433, -1.867122848840888416 ) ) ;
#26944 = CARTESIAN_POINT ( 'NONE',  ( 5.666945020832167224, 8.594891043404107478, 1.082531754730558626 ) ) ;
#26945 = ORIENTED_EDGE ( 'NONE', *, *, #55426, .F. ) ;
#26946 = CARTESIAN_POINT ( 'NONE',  ( -4.080641048033267992, 5.783833860837341412, 1.214306433183764966E-14 ) ) ;
#26947 = PLANE ( 'NONE',  #155153 ) ;
#26948 = CARTESIAN_POINT ( 'NONE',  ( 6.727182134110236689, 0.008744176509112643741, 1.710970312420513562 ) ) ;
#26949 = CARTESIAN_POINT ( 'NONE',  ( -6.521635583373313061, 7.567328587812373719, -1.199719254218446718 ) ) ;
#26950 = CARTESIAN_POINT ( 'NONE',  ( 1.177864744846460754, 1.312336027064511690, 1.133722492108141244 ) ) ;
#26951 = DIRECTION ( 'NONE',  ( 0.000000000000000000, 0.000000000000000000, -1.000000000000000000 ) ) ;
#26952 = DIRECTION ( 'NONE',  ( 0.000000000000000000, 0.000000000000000000, -1.000000000000000000 ) ) ;
#26953 = AXIS2_PLACEMENT_3D ( 'NONE', #110678, #161510, #95461 ) ;
#26954 = CARTESIAN_POINT ( 'NONE',  ( 5.559503684912662003, 1.770657277210012204, 1.256059096652543783 ) ) ;
#26955 = CARTESIAN_POINT ( 'NONE',  ( 3.967279163243800255, 0.2216459979678051528, -1.812115712870238537 ) ) ;
#26956 = CARTESIAN_POINT ( 'NONE',  ( 2.729291793292155432, 0.1011638768560127188, -1.959297240552673403 ) ) ;
#26957 = DIRECTION ( 'NONE',  ( 0.5994789404140898892, -1.444427003850258927E-16, 0.8003905296791063995 ) ) ;
#26958 = CARTESIAN_POINT ( 'NONE',  ( 8.372323551638698902, 9.726464550788689323, 1.199719254218462483 ) ) ;
#26959 = CARTESIAN_POINT ( 'NONE',  ( 2.772263606761758759, 2.110060413066455975, -0.2101530891244970389 ) ) ;
#26960 = CARTESIAN_POINT ( 'NONE',  ( 4.000000000000012434, 5.999999999999998224, -0.7500000000000006661 ) ) ;
#26961 = CARTESIAN_POINT ( 'NONE',  ( 0.4360851681528739587, -8.730413173480727096, -9.960047168614391211 ) ) ;
#26962 = CARTESIAN_POINT ( 'NONE',  ( -5.125485847170801357, 6.519186964134095597, -1.210412105186658094 ) ) ;
#26964 = AXIS2_PLACEMENT_3D ( 'NONE', #40550, #91442, #9099 ) ;
#26963 = AXIS2_PLACEMENT_3D ( 'NONE', #185194, #118150, #122447 ) ;
#26965 = CARTESIAN_POINT ( 'NONE',  ( 0.6728209460903146200, 1.430239379376567976, -1.496996390900617646 ) ) ;
#26967 = CARTESIAN_POINT ( 'NONE',  ( -1.402160292154681736E-14, 14.34375000068279249, 1.732050807568881190 ) ) ;
#26966 = CARTESIAN_POINT ( 'NONE',  ( -10.60720700236483971, 4.242771947286448686, 5.515665583366017977 ) ) ;
#26968 = ORIENTED_EDGE ( 'NONE', *, *, #91659, .F. ) ;
#26970 = EDGE_LOOP ( 'NONE', ( #52555, #113306, #91209, #193012 ) ) ;
#26969 = CARTESIAN_POINT ( 'NONE',  ( 3.176664282717697851, 1.000473465829452735, 1.983322933999843052 ) ) ;
#26971 = CARTESIAN_POINT ( 'NONE',  ( 0.7042444638330731532, 2.126757524241583486, 0.8727403922216511178 ) ) ;
#26973 = CARTESIAN_POINT ( 'NONE',  ( 0.2331563151865486683, 0.005903526429595904942, -1.945944850731482934 ) ) ;
#26972 = CARTESIAN_POINT ( 'NONE',  ( 3.816783937446950770, 4.411668334231586996, 1.199719254218464037 ) ) ;
#26975 = CARTESIAN_POINT ( 'NONE',  ( 3.475000000000000533, -1.954166666666666163, 2.006292185433948827 ) ) ;
#26974 = CARTESIAN_POINT ( 'NONE',  ( 5.713835393516482952, 5.630839145382857680, 0.7998128361456352531 ) ) ;
#26976 = CARTESIAN_POINT ( 'NONE',  ( 0.1331565106231363538, 2.033293680964400885, -2.362282156872722805 ) ) ;
#26977 = CARTESIAN_POINT ( 'NONE',  ( 5.706567001488551227, 1.626822141722890303, 0.8623401093873286349 ) ) ;
#26978 = CARTESIAN_POINT ( 'NONE',  ( -5.651877628014641886, 6.159505484824964405, -0.8148192377588457935 ) ) ;
#26979 = CARTESIAN_POINT ( 'NONE',  ( -0.1102773484824015326, 7.629137130509110243, -2.803480817674379288 ) ) ;
#26980 = CARTESIAN_POINT ( 'NONE',  ( 2.502614896622682661, 1.386922750403916105, -1.025098202461205865 ) ) ;
#26981 = CARTESIAN_POINT ( 'NONE',  ( 1.270720652900014791, -0.3006520276036573902, -1.993892820393451615 ) ) ;
#26982 = CARTESIAN_POINT ( 'NONE',  ( 1.845381457188604690, -1.911753278855784943, 1.209540087214598270 ) ) ;
#26983 = CARTESIAN_POINT ( 'NONE',  ( 4.969407589744497145, 0.2071734034183834172, -2.095845648730967792 ) ) ;
#26984 = CARTESIAN_POINT ( 'NONE',  ( -6.129694847154211423, 9.205042184104968328, -1.082531754730549967 ) ) ;
#26985 = CARTESIAN_POINT ( 'NONE',  ( 4.165142103487808889, 0.2181862141000940336, -1.756177202920036429 ) ) ;
#26987 = CARTESIAN_POINT ( 'NONE',  ( 6.532792773074245218, -2.049936377808206700, 1.026291560346163534 ) ) ;
#26986 = CARTESIAN_POINT ( 'NONE',  ( 6.556249800660121529, 9.806652646482286073, 1.199719254218452047 ) ) ;
#26988 = CARTESIAN_POINT ( 'NONE',  ( 4.646344025792163990, -1.477054284018078256, 1.098930429567553047 ) ) ;
#26989 = CARTESIAN_POINT ( 'NONE',  ( -6.084912014434944894, 5.993485526462540847, -0.7998128361456291469 ) ) ;
#26990 = CARTESIAN_POINT ( 'NONE',  ( 5.951666246274807115, 6.045958163516475636, 0.7216878364870317197 ) ) ;
#26991 = CARTESIAN_POINT ( 'NONE',  ( 1.499999999999990896, 3.775000000000021227, 1.214306433183764966E-14 ) ) ;
#26992 = CARTESIAN_POINT ( 'NONE',  ( 4.453197812796324762, 0.4814713343750369190, -2.137748681182355170 ) ) ;
#26993 = CYLINDRICAL_SURFACE ( 'NONE', #183941, 1.250000000000000000 ) ;
#26994 = CYLINDRICAL_SURFACE ( 'NONE', #201710, 1.250000000000000000 ) ;
#26995 = CARTESIAN_POINT ( 'NONE',  ( 4.475093801846619535, 1.891600172242546840, 0.8420093967692193759 ) ) ;
#26996 = CARTESIAN_POINT ( 'NONE',  ( 0.1281391398850126040, 2.011452084832816123, 0.1435147193784985509 ) ) ;
#26997 = CIRCLE ( 'NONE', #54680, 0.08000000000000020983 ) ;
#26998 = CARTESIAN_POINT ( 'NONE',  ( -0.6823417656249969321, 4.717708333674755394, -1.181850606188749264 ) ) ;
#26999 = CARTESIAN_POINT ( 'NONE',  ( 3.615773638797363798, -1.897832126884700932, 0.3302691188315133863 ) ) ;
#27000 = CARTESIAN_POINT ( 'NONE',  ( 1.364683531250000303, 8.505208333674730170, -0.7879004041258355073 ) ) ;
#27001 = CARTESIAN_POINT ( 'NONE',  ( -4.121315508874276112, 4.870918184183829602, -1.082531754730549967 ) ) ;
#27002 = CARTESIAN_POINT ( 'NONE',  ( 6.381110825713084189, -1.939362502171553482, -0.8581636585355473246 ) ) ;
#27003 = ORIENTED_EDGE ( 'NONE', *, *, #174535, .T. ) ;
#27005 = CARTESIAN_POINT ( 'NONE',  ( 6.875078400183573635, 7.629137130509068498, 2.744348168701661095 ) ) ;
#27004 = CARTESIAN_POINT ( 'NONE',  ( -3.201133666602369310, 6.748756687762456963, -0.7216878364870458196 ) ) ;
#27006 = CARTESIAN_POINT ( 'NONE',  ( 2.842405760359353106, 6.467890487061221272, -0.7998128361456291469 ) ) ;
#27007 = CARTESIAN_POINT ( 'NONE',  ( -1.284279953904135407, 3.128360285806111474, -0.7749999999999892530 ) ) ;
#27008 = DIRECTION ( 'NONE',  ( -0.6507913734559658270, 0.7592566023652989049, 0.000000000000000000 ) ) ;
#27009 = DIRECTION ( 'NONE',  ( -1.000000000000000000, -8.104628079763641167E-15, 0.000000000000000000 ) ) ;
#27010 = CARTESIAN_POINT ( 'NONE',  ( -6.305925513666572613, 6.529536985466737775, -1.006778644550405474E-06 ) ) ;
#27012 = CARTESIAN_POINT ( 'NONE',  ( 1.187862215860764126, -1.241893603568875681, -1.518774446641702580 ) ) ;
#27011 = AXIS2_PLACEMENT_3D ( 'NONE', #9345, #155602, #58096 ) ;
#27013 = CARTESIAN_POINT ( 'NONE',  ( 0.6823417656249882723, 1.738541667008083991, -1.181850606188749264 ) ) ;
#27014 = DIRECTION ( 'NONE',  ( 0.000000000000000000, 1.000000000000000000, 0.000000000000000000 ) ) ;
#27015 = CARTESIAN_POINT ( 'NONE',  ( 5.600043156098196917, 0.7966083592686534764, -1.793046234938546757 ) ) ;
#27016 = CARTESIAN_POINT ( 'NONE',  ( -10.13202086811422475, 10.71511252242175161, -0.7998128361456291469 ) ) ;
#27017 = CARTESIAN_POINT ( 'NONE',  ( -5.165293336682207581, 8.009630745229104676, 1.082531754730548412 ) ) ;
#27018 = CARTESIAN_POINT ( 'NONE',  ( 6.455963997168007396, 2.156291961557708525, -0.1537611777119098910 ) ) ;
#27020 = ORIENTED_EDGE ( 'NONE', *, *, #114510, .T. ) ;
#27019 = CARTESIAN_POINT ( 'NONE',  ( -9.093502852636577316, 1.000000000000000888, -7.666967846417613863 ) ) ;
#27021 = CARTESIAN_POINT ( 'NONE',  ( -1.364683531249997417, 4.759375000341424133, 1.214306433183764966E-14 ) ) ;
#27022 = CARTESIAN_POINT ( 'NONE',  ( 6.643826690903999577, 0.7566192825128185140, -1.820567107441137589 ) ) ;
#27023 = CARTESIAN_POINT ( 'NONE',  ( 6.503290690126083184, 1.715628873550764988, 0.2497197086974659863 ) ) ;
#27025 = CARTESIAN_POINT ( 'NONE',  ( 2.683357600500847262, 1.551837136583393839, 1.547750905674146971 ) ) ;
#27024 = CARTESIAN_POINT ( 'NONE',  ( -0.6801582343750161019, 0.6822916670080614310, 1.178068619123810334 ) ) ;
#27026 = CARTESIAN_POINT ( 'NONE',  ( 4.225798673374229431, -2.209433879803673673, 0.6658836873896284425 ) ) ;
#27027 = CARTESIAN_POINT ( 'NONE',  ( 5.975869988448771153, 1.224042345451004765, 1.657734310933855815 ) ) ;
#27028 = CARTESIAN_POINT ( 'NONE',  ( 1.781094086345108130, 1.339032250488644937, 1.406688339355038009 ) ) ;
#27029 = CARTESIAN_POINT ( 'NONE',  ( -5.056828107772848746, 8.843457192469559303, -0.7216878364870207285 ) ) ;
#27030 = SURFACE_SIDE_STYLE ('',( #108366 ) ) ;
#27031 = CARTESIAN_POINT ( 'NONE',  ( 4.974906307097914926, -1.534222593358970821, 1.464151343314526121 ) ) ;
#27032 =( LENGTH_UNIT ( ) NAMED_UNIT ( * ) SI_UNIT ( .MILLI., .METRE. ) );
#27033 = CARTESIAN_POINT ( 'NONE',  ( 2.092422861153935276, -0.4390285686692517175, 1.967888031366466395 ) ) ;
#27034 = CARTESIAN_POINT ( 'NONE',  ( -5.707619481228832115, 6.721606151930833661, -1.082531754730543971 ) ) ;
#27035 = CARTESIAN_POINT ( 'NONE',  ( 11.48788097203293823, 12.26956945602309723, -3.469500700354831491 ) ) ;
#27036 = CARTESIAN_POINT ( 'NONE',  ( 10.01963921569910632, 11.64833282552586091, 1.199719254218450271 ) ) ;
#27037 = CARTESIAN_POINT ( 'NONE',  ( 0.3459771380207553593, 1.820543102168985961, 0.1377627428671979182 ) ) ;
#27038 = CARTESIAN_POINT ( 'NONE',  ( -5.250750630242457362, 9.347902511916677426, 0.000000000000000000 ) ) ;
#27040 = CARTESIAN_POINT ( 'NONE',  ( -4.308458954092677651, 8.248562223075252220, -0.7998128361456361413 ) ) ;
#27039 = CARTESIAN_POINT ( 'NONE',  ( -4.702355942707336034, 8.355867970554191615, 0.6817663069898479700 ) ) ;
#27041 = DIRECTION ( 'NONE',  ( 8.638326563840814399E-31, -0.000000000000000000, 1.000000000000000000 ) ) ;
#27042 = ORIENTED_EDGE ( 'NONE', *, *, #153343, .T. ) ;
#27043 = CARTESIAN_POINT ( 'NONE',  ( 5.682513945847499137, -2.010110750271485447, -0.4539000206328601683 ) ) ;
#27044 = CARTESIAN_POINT ( 'NONE',  ( 4.108043207509617822, 7.655708725298683071, -0.6976724544028364283 ) ) ;
#27045 = UNCERTAINTY_MEASURE_WITH_UNIT (LENGTH_MEASURE( 1.000000000000000082E-05 ), #109827, 'distance_accuracy_value', 'NONE');
#27046 = CARTESIAN_POINT ( 'NONE',  ( 0.4644097342742973811, -8.233137084989863297, 9.488641820551102057 ) ) ;
#27047 = CARTESIAN_POINT ( 'NONE',  ( -4.277761160311629673, 4.949475094240346706, 1.199719254218462483 ) ) ;
#27048 = CARTESIAN_POINT ( 'NONE',  ( -2.993318053567081360, 6.714231172462041819, 0.000000000000000000 ) ) ;
#27049 = CARTESIAN_POINT ( 'NONE',  ( 5.074870355641393438, -1.461326316769593348, 1.394373881654621394 ) ) ;
#27051 = ORIENTED_EDGE ( 'NONE', *, *, #137968, .F. ) ;
#27050 = CARTESIAN_POINT ( 'NONE',  ( 1.499999999999989120, 0.5250000000000185629, 0.000000000000000000 ) ) ;
#27052 = AXIS2_PLACEMENT_3D ( 'NONE', #45796, #14313, #28456 ) ;
#27054 = CARTESIAN_POINT ( 'NONE',  ( 9.422553571817644524, 10.09532670998316384, 0.000000000000000000 ) ) ;
#27053 = CARTESIAN_POINT ( 'NONE',  ( -3.467853430045390706, 7.267855778353407459, 0.7998128361456352531 ) ) ;
#27055 = CARTESIAN_POINT ( 'NONE',  ( 6.096362627639171805, 10.26417349888772179, -0.7998128361456291469 ) ) ;
#27056 = CARTESIAN_POINT ( 'NONE',  ( 4.750885258907265651, -1.656392207783722315, 1.226022070186979063 ) ) ;
#27057 = CARTESIAN_POINT ( 'NONE',  ( 2.338517726396415863, 0.5350873343827439177, -1.944071628254496087 ) ) ;
#27058 = ORIENTED_EDGE ( 'NONE', *, *, #33667, .T. ) ;
#27059 = PRESENTATION_LAYER_ASSIGNMENT (  '', '', ( #213810 ) ) ;
#27060 =( BOUNDED_CURVE ( )  B_SPLINE_CURVE ( 2, ( #154230, #206965, #26081, #118585, #92196, #158245, #9834 ),
 .UNSPECIFIED., .F., .T. ) 
 B_SPLINE_CURVE_WITH_KNOTS ( ( 3, 2, 2, 3 ),
 ( 0.1625000000000003941, 0.1666666666666670182, 0.1708333333333336701, 0.1750000000000002942 ),
 .UNSPECIFIED. ) 
 CURVE ( )  GEOMETRIC_REPRESENTATION_ITEM ( )  RATIONAL_B_SPLINE_CURVE ( ( 0.9999999999999874545, 0.8660254037844512531, 1.000000000000000000, 0.8660254037844387076, 1.000000000000000000, 0.8660254037844289376, 1.000000000000009770 ) ) 
 REPRESENTATION_ITEM ( '' )  );
#27061 = CYLINDRICAL_SURFACE ( 'NONE', #201019, 1.224999999999996980 ) ;
#27062 = CARTESIAN_POINT ( 'NONE',  ( 2.842405760359353106, 6.467890487061221272, -0.7998128361456291469 ) ) ;
#27064 = VERTEX_POINT ( 'NONE', #94060 ) ;
#27063 = CARTESIAN_POINT ( 'NONE',  ( -0.06360284778254256255, 7.077111424250725591, -2.121658048144599018 ) ) ;
#27065 = CARTESIAN_POINT ( 'NONE',  ( 3.268907511149142575, -2.013924394373915128, 0.09611935726179518524 ) ) ;
#27066 = CARTESIAN_POINT ( 'NONE',  ( 1.974305314296275649, -0.08955604370030831318, -1.839086841257123073 ) ) ;
#27067 = CARTESIAN_POINT ( 'NONE',  ( 0.5754005350990994971, -2.174928102591418888, -0.7718245971977951703 ) ) ;
#27068 = CARTESIAN_POINT ( 'NONE',  ( 4.899292406491845497, 6.809203455697518947, -1.599625672291273171 ) ) ;
#27069 = ADVANCED_FACE ( 'NONE', ( #41042 ), #57276, .T. ) ;
#27070 = CARTESIAN_POINT ( 'NONE',  ( 3.075615952314793233, 2.053625483174918553, -0.6748976972978243394 ) ) ;
#27071 = CIRCLE ( 'NONE', #125074, 0.1000000000000000333 ) ;
#27072 = CARTESIAN_POINT ( 'NONE',  ( -6.388916700537716764, 8.476822122092563916, 1.599625672291283607 ) ) ;
#27073 = CARTESIAN_POINT ( 'NONE',  ( 2.407932310410058285, 0.5022953597978959683, 2.242707597164790734 ) ) ;
#27074 = EDGE_CURVE ( 'NONE', #147669, #132709, #153003, .T. ) ;
#27075 = ORIENTED_EDGE ( 'NONE', *, *, #202413, .F. ) ;
#27076 = LINE ( 'NONE', #138725, #73386 ) ;
#27077 = CARTESIAN_POINT ( 'NONE',  ( 1.445950363956361340, 1.868363765441739099, 0.09516058986362013750 ) ) ;
#27078 = CARTESIAN_POINT ( 'NONE',  ( 5.453970954872065846, 1.969229766360120149, -0.09616449669870225092 ) ) ;
#27080 = CARTESIAN_POINT ( 'NONE',  ( 7.904040366642678173, 12.16520482781775137, 0.7216878364870438212 ) ) ;
#27079 = CARTESIAN_POINT ( 'NONE',  ( -1.364683531250012516, 3.280208333674756727, 0.7879004041258379498 ) ) ;
#27082 = CARTESIAN_POINT ( 'NONE',  ( 0.8915962724085277902, 1.944627461026976034, -1.043433064090833140 ) ) ;
#27081 = CARTESIAN_POINT ( 'NONE',  ( -4.737684612971557740, 7.614716917520386374, 1.199719254218464037 ) ) ;
#27083 = CARTESIAN_POINT ( 'NONE',  ( 11.86145016429272836, 10.90000000000000036, -1.100000000000002087 ) ) ;
#27084 = CARTESIAN_POINT ( 'NONE',  ( 4.333802657862601215, 8.207853534148366492, 0.7998128361456462443 ) ) ;
#27085 = CARTESIAN_POINT ( 'NONE',  ( -5.168682875307782254, 7.053215992657626110, -1.599625672291256295 ) ) ;
#27086 = CARTESIAN_POINT ( 'NONE',  ( 6.539320575229251808, 6.034535422585679321, 2.798157489527762554 ) ) ;
#27087 = CARTESIAN_POINT ( 'NONE',  ( 4.944191625186433292, 1.966121618969366214, 0.1460544362237597982 ) ) ;
#27088 = CARTESIAN_POINT ( 'NONE',  ( 0.1059362375676886209, 1.575662574916199210, 1.419458935296296520 ) ) ;
#27089 = CARTESIAN_POINT ( 'NONE',  ( 4.336755680664809098, 2.262710760593138470, 0.4526611301470875870 ) ) ;
#27090 = ADVANCED_FACE ( 'NONE', ( #176358 ), #156922, .T. ) ;
#27091 = CARTESIAN_POINT ( 'NONE',  ( 2.817292378285217502, -1.792290562959488742, -1.020665671854523060 ) ) ;
#27092 = CARTESIAN_POINT ( 'NONE',  ( 5.639828713604826405, 9.523624565940227882, -0.7216878364870267237 ) ) ;
#27093 = CARTESIAN_POINT ( 'NONE',  ( 5.662465432362883355, 6.635239754958710989, 1.199719254218451159 ) ) ;
#27094 = CARTESIAN_POINT ( 'NONE',  ( 3.400062661977048428, 7.188766548940353829, -1.734723475976807094E-15 ) ) ;
#27095 = CARTESIAN_POINT ( 'NONE',  ( -1.364683531250012516, 2.592708333674753174, 0.7879004041258379498 ) ) ;
#27096 = CARTESIAN_POINT ( 'NONE',  ( -9.758535016135404305, 3.481548707830503631, -6.988337216065471758 ) ) ;
#27097 = CARTESIAN_POINT ( 'NONE',  ( 6.114364089638795186, 7.196141528409145671, 1.082531754730558626 ) ) ;
#27098 = CARTESIAN_POINT ( 'NONE',  ( 5.705598495378635171, -1.708133787927707647, -1.340148157549289953 ) ) ;
#27100 = CARTESIAN_POINT ( 'NONE',  ( 4.089279031174639201, -0.7008038172400687937, 1.702867937621636463 ) ) ;
#27099 = CARTESIAN_POINT ( 'NONE',  ( -4.500943810056945438, 5.313817868896925312, 1.082531754730560403 ) ) ;
#27102 = CARTESIAN_POINT ( 'NONE',  ( 11.78331023100045272, 12.29999999999998295, 1.799999999999999600 ) ) ;
#27101 = CARTESIAN_POINT ( 'NONE',  ( 1.364683531249990311, 5.363541667008086655, 0.7879004041258500513 ) ) ;
#27103 = CARTESIAN_POINT ( 'NONE',  ( 5.196902890030515643, 1.791362914573800369, 1.262263373074036688 ) ) ;
#27104 = CARTESIAN_POINT ( 'NONE',  ( 1.333477130264982380, 8.249568609204944281, -9.911050286642574036 ) ) ;
#27105 = CARTESIAN_POINT ( 'NONE',  ( 0.5974158272751062260, 1.880195615759198136, -1.258034406164424635 ) ) ;
#27106 = CARTESIAN_POINT ( 'NONE',  ( -4.144866890078757748, 7.628995377423835045, -0.8586628004631415845 ) ) ;
#27107 = CARTESIAN_POINT ( 'NONE',  ( 5.043764445095213489, 7.992138250556588552, 1.161813593947092382 ) ) ;
#27108 = CARTESIAN_POINT ( 'NONE',  ( -3.323157048681004699, 6.891117300187535655, -0.7216878364870458196 ) ) ;
#27109 = CARTESIAN_POINT ( 'NONE',  ( -7.550983558724452926, -6.148216694138056937, -7.550983558724408518 ) ) ;
#27110 = CARTESIAN_POINT ( 'NONE',  ( 1.217257651388839346, -1.727774110360464244, 0.3828142623626716867 ) ) ;
#27111 =( BOUNDED_CURVE ( )  B_SPLINE_CURVE ( 2, ( #41203, #204716, #87800, #203650, #107310, #56365, #173334 ),
 .UNSPECIFIED., .F., .T. ) 
 B_SPLINE_CURVE_WITH_KNOTS ( ( 3, 2, 2, 3 ),
 ( 0.1500000000000002165, 0.1541666666666668961, 0.1583333333333335480, 0.1625000000000002276 ),
 .UNSPECIFIED. ) 
 CURVE ( )  GEOMETRIC_REPRESENTATION_ITEM ( )  RATIONAL_B_SPLINE_CURVE ( ( 0.9999999999999928946, 0.8660254037844458130, 1.000000000000000000, 0.8660254037844387076, 1.000000000000000000, 0.8660254037844316022, 1.000000000000007105 ) ) 
 REPRESENTATION_ITEM ( '' )  );
#27113 = CARTESIAN_POINT ( 'NONE',  ( 5.268231569329090647, 2.010679013512342017, -0.1011730594673541789 ) ) ;
#27112 = AXIS2_PLACEMENT_3D ( 'NONE', #104778, #91743, #205446 ) ;
#27114 = CARTESIAN_POINT ( 'NONE',  ( 5.469824908109481854, 8.468880595181346393, -1.199719254218446718 ) ) ;
#27115 = CARTESIAN_POINT ( 'NONE',  ( 3.680784645728672810, -2.029037780879865416, -0.5636793167548505012 ) ) ;
#27116 = CARTESIAN_POINT ( 'NONE',  ( 2.741684679331716890, 1.906140283219289966, -0.1903247725174895544 ) ) ;
#27117 = CARTESIAN_POINT ( 'NONE',  ( 4.220665892555866883, 3.818531717603609987, -0.7998128361456211532 ) ) ;
#27118 = CARTESIAN_POINT ( 'NONE',  ( 4.492606276566666779, 1.931098607525572497, 0.3863565733641035616 ) ) ;
#27119 = CARTESIAN_POINT ( 'NONE',  ( 5.519787823685118333, -0.4868164491665989413, 1.960129884169951708 ) ) ;
#27120 = CARTESIAN_POINT ( 'NONE',  ( 1.779943879855113709, -1.003247456797161652, 1.578688272967261996 ) ) ;
#27123 = ORIENTED_EDGE ( 'NONE', *, *, #37635, .F. ) ;
#27122 = CARTESIAN_POINT ( 'NONE',  ( 1.687617486097678476, 1.829050272730630144, -0.5582976189952293389 ) ) ;
#27121 = CARTESIAN_POINT ( 'NONE',  ( 4.811038506879902421, 1.503007855926122405, 0.8461308117306536314 ) ) ;
#27125 = CARTESIAN_POINT ( 'NONE',  ( 5.178851490740207453, 5.144340948726102702, 0.7216878364870317197 ) ) ;
#27124 = CARTESIAN_POINT ( 'NONE',  ( 1.840723031453334935, 2.183200880077686978, 0.3216222850719457349 ) ) ;
#27126 = CARTESIAN_POINT ( 'NONE',  ( -1.364683531250012516, 2.342708333674752286, 0.7879004041258379498 ) ) ;
#27127 = CARTESIAN_POINT ( 'NONE',  ( 6.602011099637477010, 0.7519813002578833450, -1.812223124677159181 ) ) ;
#27128 = CARTESIAN_POINT ( 'NONE',  ( 8.938903350111612411, 9.323142084752035430, -0.7998128361456221525 ) ) ;
#27129 = CARTESIAN_POINT ( 'NONE',  ( 11.84668729410370602, 11.00620512324527134, 1.399999999999998357 ) ) ;
#27130 = DIRECTION ( 'NONE',  ( 0.000000000000000000, 0.000000000000000000, 1.000000000000000000 ) ) ;
#27131 = DIRECTION ( 'NONE',  ( -1.000000000000000000, 0.000000000000000000, 4.440892098500751393E-16 ) ) ;
#27132 = CARTESIAN_POINT ( 'NONE',  ( -10.35465518852992517, -5.836144560139977955, 0.4365953560983814041 ) ) ;
#27133 = EDGE_LOOP ( 'NONE', ( #28143, #191240, #191270, #78171, #165185 ) ) ;
#27134 = CARTESIAN_POINT ( 'NONE',  ( 1.732962091629593804, -1.965256999408044436, -0.6514315320021792921 ) ) ;
#27135 = CARTESIAN_POINT ( 'NONE',  ( 0.7499999999999885647, 2.566666666666689522, -1.299038105676658228 ) ) ;
#27136 = CARTESIAN_POINT ( 'NONE',  ( 6.124532705071213279, 8.168374127381657246, -1.599625672291262513 ) ) ;
#27137 = CARTESIAN_POINT ( 'NONE',  ( -6.527360889975461156, 9.702672574024962415, 1.199719254218452047 ) ) ;
#27138 = CARTESIAN_POINT ( 'NONE',  ( 5.174371902270911150, 6.065797303184739420, 1.199719254218452047 ) ) ;
#27140 = EDGE_CURVE ( 'NONE', #6643, #156, #156415, .T. ) ;
#27139 = CARTESIAN_POINT ( 'NONE',  ( 0.02995210924121824436, -1.980234168275105455, 0.3962368897427023806 ) ) ;
#27141 = SURFACE_STYLE_FILL_AREA ( #191768 ) ;
#27142 = CARTESIAN_POINT ( 'NONE',  ( 1.364683531249990311, 3.134375000341423245, 1.214306433183764966E-14 ) ) ;
#27143 = EDGE_CURVE ( 'NONE', #141262, #79190, #104938, .T. ) ;
#27145 = CARTESIAN_POINT ( 'NONE',  ( 2.737856954955798727, 5.281584649835344258, 1.199719254218452047 ) ) ;
#27144 = CARTESIAN_POINT ( 'NONE',  ( 2.609770642201841184, 0.3830433331901660354, 0.000000000000000000 ) ) ;
#27146 = CARTESIAN_POINT ( 'NONE',  ( 5.343124974464078747, -1.122324884721880078, 1.674632237393176792 ) ) ;
#27147 = CARTESIAN_POINT ( 'NONE',  ( 4.417137112658839015, -1.749089155124187389, 0.7819188135024003339 ) ) ;
#27148 =( NAMED_UNIT ( * ) SI_UNIT ( $, .STERADIAN. ) SOLID_ANGLE_UNIT ( ) );
#27149 = CARTESIAN_POINT ( 'NONE',  ( 3.017305944477025825, -2.111434807548946857, 0.5868732223921411251 ) ) ;
#27150 = CARTESIAN_POINT ( 'NONE',  ( 0.1335669894368317900, 1.324834237272943360, -2.404533294357531048 ) ) ;
#27151 = CARTESIAN_POINT ( 'NONE',  ( 1.499999999999987121, 0.7854166673494828999, 0.8660254037844524744 ) ) ;
#27152 = CARTESIAN_POINT ( 'NONE',  ( 5.607686816480834224, 1.527379804643314687, 1.311666717936723403 ) ) ;
#27153 = CARTESIAN_POINT ( 'NONE',  ( 1.687617486097678476, 1.829050272730630144, -0.5582976189952293389 ) ) ;
#27154 = CARTESIAN_POINT ( 'NONE',  ( -7.043624497499477499, 8.176315654292865887, 1.199719254218450271 ) ) ;
#27156 = CARTESIAN_POINT ( 'NONE',  ( 0.1754079408978586052, 1.496066871905444629, 1.352139405095334590 ) ) ;
#27155 = CARTESIAN_POINT ( 'NONE',  ( -3.470524135418306511, 5.072030796119872953, -1.443375672974053447 ) ) ;
#27157 = CARTESIAN_POINT ( 'NONE',  ( 0.6823417656249934904, 9.755208333674728394, 1.181850606188764807 ) ) ;
#27159 = CARTESIAN_POINT ( 'NONE',  ( -6.257970421159510188, 9.458660037064859694, 1.199719254218452047 ) ) ;
#27158 = CARTESIAN_POINT ( 'NONE',  ( 3.421503388043937832, -1.247306758965301521, -1.677755357943153447 ) ) ;
#27161 = VERTEX_POINT ( 'NONE', #60459 ) ;
#27160 = CARTESIAN_POINT ( 'NONE',  ( 1.658790106635851469, -1.476843439067159425, -0.8906862264850596844 ) ) ;
#27162 = CARTESIAN_POINT ( 'NONE',  ( 6.533471381225442798, -0.1521382079053348602, 2.086446650026114735 ) ) ;
#27163 = CARTESIAN_POINT ( 'NONE',  ( 6.308621549060418054, 6.254479983525607523, 0.7998128361456341429 ) ) ;
#27164 = CARTESIAN_POINT ( 'NONE',  ( 0.000000000000000000, 15.51887838114830132, 0.000000000000000000 ) ) ;
#27165 = CARTESIAN_POINT ( 'NONE',  ( -6.042630808230841359E-15, -2.318749999044084298, 3.474999999999999645 ) ) ;
#27166 = CARTESIAN_POINT ( 'NONE',  ( 7.037870247915954280, -8.233137084989836652, -6.381095703207985359 ) ) ;
#27167 = CARTESIAN_POINT ( 'NONE',  ( 4.008406971134620633, 7.828225232965717595, 0.7998128361456321445 ) ) ;
#27168 = CARTESIAN_POINT ( 'NONE',  ( -11.81907076198602802, 13.75731224596479052, -1.592066415281275349 ) ) ;
#27169 = CARTESIAN_POINT ( 'NONE',  ( 2.543383136322028282, -1.689629589678593558, 0.6535807426650240837 ) ) ;
#27170 = EDGE_LOOP ( 'NONE', ( #149907, #23554, #94920, #47415 ) ) ;
#27171 = CARTESIAN_POINT ( 'NONE',  ( 2.544126380858701797, 6.119897877643793116, 0.7998128361456462443 ) ) ;
#27172 = ORIENTED_EDGE ( 'NONE', *, *, #692, .F. ) ;
#27173 = CARTESIAN_POINT ( 'NONE',  ( 5.747730777550676073, 5.670383760089384495, 0.000000000000000000 ) ) ;
#27174 = CARTESIAN_POINT ( 'NONE',  ( 3.281707762122548555, 1.766655041338391907, -0.3996267988317265818 ) ) ;
#27175 = CARTESIAN_POINT ( 'NONE',  ( 6.539320575229216281, 4.696526872534390940, 2.559412612844500057 ) ) ;
#27176 = CARTESIAN_POINT ( 'NONE',  ( 1.500000000000001332, 9.156250000682799595, 0.000000000000000000 ) ) ;
#27177 = CARTESIAN_POINT ( 'NONE',  ( 4.006694938150886287, 7.586369203660299654, 0.2279062292016853508 ) ) ;
#27178 = VECTOR ( 'NONE', #132209, 1000.000000000000000 ) ;
#27179 = CARTESIAN_POINT ( 'NONE',  ( 3.930005801358939621, 1.032382326871328804, 1.548228005463901491 ) ) ;
#27180 = CARTESIAN_POINT ( 'NONE',  ( 1.897908843228306663, -0.9047085692259320133, -1.688519222619834892 ) ) ;
#27181 = CARTESIAN_POINT ( 'NONE',  ( 0.4635302585514287088, 1.806487598472360956, -0.2625014351145052438 ) ) ;
#27182 = CARTESIAN_POINT ( 'NONE',  ( 0.000000000000000000, 0.000000000000000000, -6.123233995736775897E-17 ) ) ;
#27183 = CARTESIAN_POINT ( 'NONE',  ( -6.102578539482539810, 6.292298848917299736, 0.000000000000000000 ) ) ;
#27184 = CARTESIAN_POINT ( 'NONE',  ( 5.309622429108474151, 7.625948988765205883, 1.230663689527239812 ) ) ;
#27185 = CARTESIAN_POINT ( 'NONE',  ( -11.33772467203841572, 10.09267152018144209, 3.599999999999999201 ) ) ;
#27186 = CARTESIAN_POINT ( 'NONE',  ( -6.328551337425281531, 6.876786110265634910, 0.7058904598814246256 ) ) ;
#27187 = CARTESIAN_POINT ( 'NONE',  ( -3.226477370372317743, 4.787309570232886280, 1.443375672974064550 ) ) ;
#27188 = CARTESIAN_POINT ( 'NONE',  ( 8.595506201384013778, 10.09080732544527592, 1.082531754730558626 ) ) ;
#27189 = CARTESIAN_POINT ( 'NONE',  ( 5.612145322048014862, 1.967363499941950034, -0.09270071294615632451 ) ) ;
#27190 = CARTESIAN_POINT ( 'NONE',  ( -3.391510981712833939, 7.108513245306943062, 0.7998128361456341429 ) ) ;
#27191 = CYLINDRICAL_SURFACE ( 'NONE', #17442, 1.500000000000000222 ) ;
#27192 = CARTESIAN_POINT ( 'NONE',  ( 0.6036074345479571779, -2.080388865039545454, 0.2067186989125231189 ) ) ;
#27193 = CARTESIAN_POINT ( 'NONE',  ( 8.945682426918439845, 9.331051007693339727, 1.040834085586084257E-14 ) ) ;
#27194 = CARTESIAN_POINT ( 'NONE',  ( 5.948256396973989446, 1.924214498663083139, 0.09423418586224258098 ) ) ;
#27195 = CARTESIAN_POINT ( 'NONE',  ( -4.934277840369690971, 7.844075682818238526, -1.199719254218452047 ) ) ;
#27196 = CARTESIAN_POINT ( 'NONE',  ( 1.078802750678783395, -0.04027803099338270881, -1.825304540826321542 ) ) ;
#27197 = CARTESIAN_POINT ( 'NONE',  ( 2.368051099418837069, 2.164043333312406503, -0.4318774905316472013 ) ) ;
#27198 = CARTESIAN_POINT ( 'NONE',  ( 11.88237264505823987, 12.34322961531682239, 0.9087825512662162097 ) ) ;
#27199 = CARTESIAN_POINT ( 'NONE',  ( 1.089939655121434203, 1.141396045679959004, 1.534244836814010693 ) ) ;
#27200 = CARTESIAN_POINT ( 'NONE',  ( 0.7484202955074462649, -1.954263247020354477, -0.2444711731117015785 ) ) ;
#27201 = CARTESIAN_POINT ( 'NONE',  ( 2.102980028956519476, -0.4233231936755370572, 1.895218400837359818 ) ) ;
#27202 = ORIENTED_EDGE ( 'NONE', *, *, #71349, .F. ) ;
#27203 = CARTESIAN_POINT ( 'NONE',  ( 0.4564073884281876214, 1.492024165150519055, 1.356095248386236074 ) ) ;
#27205 = CARTESIAN_POINT ( 'NONE',  ( 6.508657375787280763, 0.5831478024676381988, 1.767317905175052051 ) ) ;
#27204 = CARTESIAN_POINT ( 'NONE',  ( -4.945692173934974178, 8.992000979557944973, 0.000000000000000000 ) ) ;
#27206 = CARTESIAN_POINT ( 'NONE',  ( 3.898851692381625877, 6.706354853490643642, -1.199719254218452047 ) ) ;
#27207 = CARTESIAN_POINT ( 'NONE',  ( -11.44779963594988814, 13.40000000000000213, -3.600000000000000977 ) ) ;
#27208 = CARTESIAN_POINT ( 'NONE',  ( -7.583016927391839523, -5.196967604326691692, -7.968844136639799736 ) ) ;
#27209 = CARTESIAN_POINT ( 'NONE',  ( -4.069418662396130593, 7.899405539437467816, -0.7998128361456281477 ) ) ;
#27210 = CARTESIAN_POINT ( 'NONE',  ( -6.774234028683526532, 7.932303117332766718, 1.199719254218452047 ) ) ;
#27211 = CARTESIAN_POINT ( 'NONE',  ( 2.050558489324630251, -1.691691439650149897, 1.393213601605561180 ) ) ;
#27212 = CARTESIAN_POINT ( 'NONE',  ( 4.378920427533921078, 4.211088041652093494, 1.214306433183764966E-14 ) ) ;
#27213 = CARTESIAN_POINT ( 'NONE',  ( 5.826972158823246595, 10.02016096192762085, -0.7998128361456481317 ) ) ;
#27214 = CARTESIAN_POINT ( 'NONE',  ( 9.617648866954018771, -9.063431457505044975, -0.6035590660249217088 ) ) ;
#27215 = CARTESIAN_POINT ( 'NONE',  ( 3.316849939159485228, 1.650902842016691130, 0.7798126646740562995 ) ) ;
#27216 = DIRECTION ( 'NONE',  ( -5.176899690512889973E-31, 0.6299249119529756191, 0.7766560405359864694 ) ) ;
#27217 = CARTESIAN_POINT ( 'NONE',  ( -3.765413976293358278, 5.416068943807445635, 1.599625672291267398 ) ) ;
#27218 = CARTESIAN_POINT ( 'NONE',  ( -5.476171693740270463, 7.594609835490887306, -1.347918582746489902 ) ) ;
#27219 = CARTESIAN_POINT ( 'NONE',  ( 6.925078400183573457, 0.5887076473912872254, 1.908330883025354030 ) ) ;
#27220 = CARTESIAN_POINT ( 'NONE',  ( 9.887974103068218668, 10.43039129653476493, 0.7998128361456462443 ) ) ;
#27221 = CARTESIAN_POINT ( 'NONE',  ( 0.9965603196819513565, -0.4670424642401714288, -1.868911657674779958 ) ) ;
#27222 = CARTESIAN_POINT ( 'NONE',  ( 5.910985094894211755, -1.548708053515185812, 1.204094020389692377 ) ) ;
#27223 = CIRCLE ( 'NONE', #58311, 0.1599999999999999756 ) ;
#27224 = CARTESIAN_POINT ( 'NONE',  ( -1.500000000000008216, 14.75000000000000000, 3.469446951953614189E-15 ) ) ;
#27225 = CARTESIAN_POINT ( 'NONE',  ( -7.725448601688521322, 7.907444878258402809, 1.040834085586084257E-14 ) ) ;
#27226 = CARTESIAN_POINT ( 'NONE',  ( 4.286349120214771879, 8.152491073559232859, -0.7998128361456221525 ) ) ;
#27227 = CARTESIAN_POINT ( 'NONE',  ( 5.284801750429747536, 1.933107837519608685, -1.032524723389722787 ) ) ;
#27228 = CARTESIAN_POINT ( 'NONE',  ( 4.253507506385319381, 5.985511395581417204, 1.599625672291267175 ) ) ;
#27229 = CARTESIAN_POINT ( 'NONE',  ( 4.592674910654532816, 2.029287475768901228, 0.4089837765668055680 ) ) ;
#27230 = CARTESIAN_POINT ( 'NONE',  ( 0.6823417656249882723, 0.9885416670080832136, -1.181850606188749264 ) ) ;
#27231 = ORIENTED_EDGE ( 'NONE', *, *, #127420, .F. ) ;
#27232 = CARTESIAN_POINT ( 'NONE',  ( 4.395370282159323239, -0.9827166871091972400, -2.078181120130776272 ) ) ;
#27233 = CARTESIAN_POINT ( 'NONE',  ( 6.751597309925441159, 9.860318714012938912, -1.082531754730537088 ) ) ;
#27235 = CARTESIAN_POINT ( 'NONE',  ( 0.000000000000000000, 0.06698729810653621108, 0.000000000000000000 ) ) ;
#27234 = CARTESIAN_POINT ( 'NONE',  ( 4.095971805104276164, 7.792734516014745871, 0.7216878364870257245 ) ) ;
#27236 = B_SPLINE_CURVE_WITH_KNOTS ( 'NONE', 3,
 ( #54114, #71395, #4256, #19459, #200335, #203523 ),
 .UNSPECIFIED., .F., .F.,
 ( 4, 2, 4 ),
 ( 0.000000000000000000, 0.002037565947615824213, 0.004075131895231648427 ),
 .UNSPECIFIED. ) ;
#27237 = CARTESIAN_POINT ( 'NONE',  ( 6.620655732516659064, 6.039214117936751336, 2.421170424969817603 ) ) ;
#27238 = CARTESIAN_POINT ( 'NONE',  ( -5.576146316970437944, 9.727530813099326323, 0.000000000000000000 ) ) ;
#27239 = CARTESIAN_POINT ( 'NONE',  ( 5.191327941051770978, -0.6971716684453888035, 1.812662890818200756 ) ) ;
#27240 = VERTEX_POINT ( 'NONE', #124494 ) ;
#27241 = CARTESIAN_POINT ( 'NONE',  ( 8.825994812371966702, 12.28044913353391898, -1.082531754730543083 ) ) ;
#27242 = ADVANCED_FACE ( 'NONE', ( #11703 ), #190453, .F. ) ;
#27243 = EDGE_LOOP ( 'NONE', ( #151851, #145363, #68319, #56562 ) ) ;
#27244 = CARTESIAN_POINT ( 'NONE',  ( 4.640819915729988310, 1.831716588661407963, 0.5496940206762624959 ) ) ;
#27245 = CARTESIAN_POINT ( 'NONE',  ( 6.124008131756068174, -0.9624739961165188484, -1.431025375277717115 ) ) ;
#27246 = CARTESIAN_POINT ( 'NONE',  ( 4.048064755690682581, 0.9548552675892291175, 1.776167154503265566 ) ) ;
#27247 = CARTESIAN_POINT ( 'NONE',  ( -10.17947440576205054, 10.77047498301088346, 0.7998128361456462443 ) ) ;
#27248 = CARTESIAN_POINT ( 'NONE',  ( 1.001543065824772753E-15, -3.609374999522044547, 3.793834371823811669 ) ) ;
#27250 = CARTESIAN_POINT ( 'NONE',  ( 0.1976571007769452604, -1.769309276362411643, -0.05040135802934773979 ) ) ;
#27249 = CARTESIAN_POINT ( 'NONE',  ( 1.763735852432495754, 1.075751846022491964, 1.792481376920366687 ) ) ;
#27251 = CARTESIAN_POINT ( 'NONE',  ( 6.135388727473008785, 0.6351960432287793168, 1.913804721665197883 ) ) ;
#27253 = CARTESIAN_POINT ( 'NONE',  ( 3.345926335499046722, 2.292435215394402093, 0.0001471259066659902901 ) ) ;
#27252 = CARTESIAN_POINT ( 'NONE',  ( 5.194709132691408549, 6.089524072008651423, 1.199719254218452935 ) ) ;
#27254 = CARTESIAN_POINT ( 'NONE',  ( 1.921426573741076727, 1.003422016191083399, -1.421716384592019544 ) ) ;
#27255 = CARTESIAN_POINT ( 'NONE',  ( 2.742561299210785286, 1.174483946500170184, -1.765453564165630596 ) ) ;
#27256 = CARTESIAN_POINT ( 'NONE',  ( 6.773376349083131132, -7.215597533173308875, 6.661184041420955992 ) ) ;
#27257 = CARTESIAN_POINT ( 'NONE',  ( 0.5789038866980666942, 1.201919051685101270, -1.249903294292388667 ) ) ;
#27258 = CARTESIAN_POINT ( 'NONE',  ( 0.6801582343749883464, 2.588541667008101399, -1.178068619123865846 ) ) ;
#27259 = CARTESIAN_POINT ( 'NONE',  ( 1.398636348511049565, 0.3583461405318502102, 1.826042456754966681 ) ) ;
#27260 = CARTESIAN_POINT ( 'NONE',  ( 2.576841123524225452, 1.419588041764899611, -1.642854796848471244 ) ) ;
#27261 = CARTESIAN_POINT ( 'NONE',  ( 3.327361509216096191, -1.530157842762596143, -1.313544516083162028 ) ) ;
#27262 = CARTESIAN_POINT ( 'NONE',  ( 4.562500000000002665, -1.451031289061298857, -1.451031289060931595 ) ) ;
#27263 = AXIS2_PLACEMENT_3D ( 'NONE', #57880, #107772, #21075 ) ;
#27264 = CARTESIAN_POINT ( 'NONE',  ( -1.500000000000013101, 1.452083334016150085, 0.8660254037844403729 ) ) ;
#27265 = CARTESIAN_POINT ( 'NONE',  ( 6.234985708453399944, 0.1916802727454213762, 1.916943350541326030 ) ) ;
#27266 = CARTESIAN_POINT ( 'NONE',  ( -8.012344526598182026E-15, 14.54687500034139802, -1.575800808251669460 ) ) ;
#27267 = CARTESIAN_POINT ( 'NONE',  ( 2.971146563671855034, -1.679565462486251048, 1.453923022682623856 ) ) ;
#27268 = ORIENTED_EDGE ( 'NONE', *, *, #47118, .T. ) ;
#27269 = SURFACE_SIDE_STYLE ('',( #138921 ) ) ;
#27270 = SURFACE_STYLE_FILL_AREA ( #212406 ) ;
#27271 = CARTESIAN_POINT ( 'NONE',  ( 7.889955328148847258, 11.29236608522730911, -1.199719254218446718 ) ) ;
#27272 = CARTESIAN_POINT ( 'NONE',  ( -1.364683531250000748, -0.9906249996585805295, 0.000000000000000000 ) ) ;
#27273 = CARTESIAN_POINT ( 'NONE',  ( -0.1044638861024569515, -0.1585131741546479955, -2.186235582987208659 ) ) ;
#27274 = CARTESIAN_POINT ( 'NONE',  ( 4.351973852746993110, -0.7528527933186466292, 1.811862133468461922 ) ) ;
#27276 = CARTESIAN_POINT ( 'NONE',  ( -5.246642258808529746, 9.064907035344523578, 0.000000000000000000 ) ) ;
#27275 = CARTESIAN_POINT ( 'NONE',  ( 10.05978679165993483, 11.79913468076720306, 1.082531754730548412 ) ) ;
#27277 = EDGE_CURVE ( 'NONE', #122390, #83476, #63019, .T. ) ;
#27278 = CARTESIAN_POINT ( 'NONE',  ( 1.220000000000003526, 6.400000000000022560, 1.229247124133362667E-14 ) ) ;
#27279 = CARTESIAN_POINT ( 'NONE',  ( 5.395900114300756556, -0.8213888976819706533, 2.108206106441696370 ) ) ;
#27280 = CIRCLE ( 'NONE', #144978, 0.08000000000000020983 ) ;
#27281 = CARTESIAN_POINT ( 'NONE',  ( 2.348159106025033083, -0.8842165242596754515, 1.863692774951962727 ) ) ;
#27282 = CARTESIAN_POINT ( 'NONE',  ( -6.566226467720086113, 6.555019055295208119, 1.040834085586084257E-14 ) ) ;
#27283 = ORIENTED_EDGE ( 'NONE', *, *, #66555, .T. ) ;
#27284 = CARTESIAN_POINT ( 'NONE',  ( -1.499999999999997780, 2.681250000682818158, 1.214306433183764966E-14 ) ) ;
#27285 = CARTESIAN_POINT ( 'NONE',  ( 3.690566713891149320, -0.3619836066245524786, -1.835009008997898761 ) ) ;
#27286 = CARTESIAN_POINT ( 'NONE',  ( 2.672175078814063909, 1.228020439816409848, 1.224710958539473094 ) ) ;
#27287 = CARTESIAN_POINT ( 'NONE',  ( 6.181208317857348256, 1.509947553572440704, 1.588605474358975478 ) ) ;
#27288 = CARTESIAN_POINT ( 'NONE',  ( 0.9739772326014315418, 2.126351460888118883, -0.5901193814053447007 ) ) ;
#27289 = CARTESIAN_POINT ( 'NONE',  ( 4.469695567000064429, 2.097540297429688838, -0.5223010940857697459 ) ) ;
#27290 = CARTESIAN_POINT ( 'NONE',  ( 5.665949523032352886, -1.230194547739250854, 1.502597557546548446 ) ) ;
#27291 = CARTESIAN_POINT ( 'NONE',  ( 6.928203230275514990, 15.46950125723224723, 9.797958971132709749 ) ) ;
#27292 = SURFACE_SIDE_STYLE ('',( #175702 ) ) ;
#27293 = CARTESIAN_POINT ( 'NONE',  ( 11.04536101718726293, 10.90000000000000036, -1.100000000000002087 ) ) ;
#27294 = CARTESIAN_POINT ( 'NONE',  ( -0.06985027309261250539, -2.078401542846250116, 0.4200961532789050379 ) ) ;
#27295 = CARTESIAN_POINT ( 'NONE',  ( -1.360316468750040642, 2.161458333674780352, 0.7853790794158861388 ) ) ;
#27296 = FILL_AREA_STYLE ('',( #91269 ) ) ;
#27297 = CARTESIAN_POINT ( 'NONE',  ( -7.479294296233107708, 11.87759377891399204, 0.7998128361456481317 ) ) ;
#27298 = CARTESIAN_POINT ( 'NONE',  ( 7.644099680006512187, 7.812537802962739697, 1.040834085586084257E-14 ) ) ;
#27299 = CARTESIAN_POINT ( 'NONE',  ( -6.471393748265538370, 5.229711127717889596, -2.499999999999995115 ) ) ;
#27300 = CARTESIAN_POINT ( 'NONE',  ( 3.457459740917231628, 0.4424662778084071935, -1.771134634090239190 ) ) ;
#27301 = B_SPLINE_CURVE_WITH_KNOTS ( 'NONE', 3,
 ( #65400, #85945, #17709, #82739, #167198 ),
 .UNSPECIFIED., .F., .F.,
 ( 4, 1, 4 ),
 ( 7.342161860471412858E-17, 3.079525422763246153E-06, 6.159050845453070644E-06 ),
 .UNSPECIFIED. ) ;
#27302 = CARTESIAN_POINT ( 'NONE',  ( 2.345003271878861373, 0.4830727525354863716, 2.153096645625157457 ) ) ;
#27303 = ORIENTED_EDGE ( 'NONE', *, *, #89264, .F. ) ;
#27304 = CARTESIAN_POINT ( 'NONE',  ( -7.608060475923978494, 8.905100639113307182, 1.199719254218452047 ) ) ;
#27305 = UNCERTAINTY_MEASURE_WITH_UNIT (LENGTH_MEASURE( 1.000000000000000082E-05 ), #197918, 'distance_accuracy_value', 'NONE');
#27306 = CARTESIAN_POINT ( 'NONE',  ( 3.285556943750000514, -2.501041666188708046, 1.896917185911906500 ) ) ;
#27307 = CARTESIAN_POINT ( 'NONE',  ( -8.505042434474312074, 8.816971016508505343, -0.7998128361456291469 ) ) ;
#27308 = CARTESIAN_POINT ( 'NONE',  ( 0.8791727066333665519, -1.827835516345464484, -0.8596444897858869227 ) ) ;
#27309 = CARTESIAN_POINT ( 'NONE',  ( 0.6629299983115041206, 0.6194173074674096391, 2.027988828570789437 ) ) ;
#27310 = EDGE_CURVE ( 'NONE', #127442, #51151, #192197, .T. ) ;
#27311 = CARTESIAN_POINT ( 'NONE',  ( -1.000000000000017097, 5.868705557303652398, 4.125226524755080781 ) ) ;
#27312 = CARTESIAN_POINT ( 'NONE',  ( -5.773793314573309132, 7.829454515125894964, 1.599625672291263179 ) ) ;
#27313 = CARTESIAN_POINT ( 'NONE',  ( 2.623689330893996363, 1.826062842344724269, -0.3576783775682371158 ) ) ;
#27314 = CARTESIAN_POINT ( 'NONE',  ( 8.367353357928214663, 12.91366268422496688, 1.040834085586084257E-14 ) ) ;
#27315 = COLOUR_RGB ( '', 0.40784314, 0.44705882, 0.49803922) ;
#27316 = CARTESIAN_POINT ( 'NONE',  ( 0.6730137850648570952, -2.035850703004048246, -0.7271551459356735414 ) ) ;
#27317 = DIRECTION ( 'NONE',  ( -0.000000000000000000, -1.000000000000000000, -0.000000000000000000 ) ) ;
#27318 = ORIENTED_EDGE ( 'NONE', *, *, #175406, .F. ) ;
#27319 = ORIENTED_EDGE ( 'NONE', *, *, #18383, .F. ) ;
#27320 = CARTESIAN_POINT ( 'NONE',  ( -4.055860508782465068, 7.883587693554856557, 1.040834085586084257E-14 ) ) ;
#27321 = CARTESIAN_POINT ( 'NONE',  ( -10.14557902172788495, 10.73093036830436553, 1.040834085586084257E-14 ) ) ;
#27322 = CARTESIAN_POINT ( 'NONE',  ( 3.633261591126951018, -1.686358373764598406, 0.7000054678709469735 ) ) ;
#27324 = CARTESIAN_POINT ( 'NONE',  ( -5.775737613422593952, 6.228167737865282660, -1.031624843267029190 ) ) ;
#27323 = CARTESIAN_POINT ( 'NONE',  ( -5.224688093219839402, 7.188831756880171397, -1.599625672291271394 ) ) ;
#27325 = CARTESIAN_POINT ( 'NONE',  ( 5.561552386509557522, 7.525632394756676113, -1.337405013919689800 ) ) ;
#27326 = CARTESIAN_POINT ( 'NONE',  ( 6.802112138117927920, -1.802125342305498146, 0.9040232568291312054 ) ) ;
#27327 = CARTESIAN_POINT ( 'NONE',  ( 5.648353745280480176, -1.448853643138726000, 1.135948691490688667 ) ) ;
#27328 = CARTESIAN_POINT ( 'NONE',  ( -0.02319159430947541692, 2.051704324979522820, -2.228571760951563618 ) ) ;
#27329 = CARTESIAN_POINT ( 'NONE',  ( 4.125798732227327292, -2.208944405816467338, 0.6678306985251744043 ) ) ;
#27330 = CARTESIAN_POINT ( 'NONE',  ( 5.020262018810099924, 9.078999131912302900, 0.7998128361456331437 ) ) ;
#27331 = CARTESIAN_POINT ( 'NONE',  ( 0.8079727292511580394, -2.051105382888893658, 0.1991618667988598601 ) ) ;
#27332 = CARTESIAN_POINT ( 'NONE',  ( 7.494959990256193194, 7.638541498254023843, -0.7998128361456281477 ) ) ;
#27333 = CARTESIAN_POINT ( 'NONE',  ( 1.874458991091961568, -0.09742729390963811298, -1.939748921942837878 ) ) ;
#27334 = AXIS2_PLACEMENT_3D ( 'NONE', #141452, #59078, #105735 ) ;
#27335 = CARTESIAN_POINT ( 'NONE',  ( 5.589350027729360626, 1.375356176494828553, -1.841343765151080003 ) ) ;
#27336 = CARTESIAN_POINT ( 'NONE',  ( 11.86145016429273191, 10.19999999999999929, 1.099999999999996758 ) ) ;
#27337 = CARTESIAN_POINT ( 'NONE',  ( -5.725286006720766707, 9.901527117808042178, 0.7998128361456291469 ) ) ;
#27338 = CARTESIAN_POINT ( 'NONE',  ( 4.574985519202336981, -0.0001439422951596270033, -1.870836309977530920 ) ) ;
#27339 = ORIENTED_EDGE ( 'NONE', *, *, #205468, .F. ) ;
#27342 = CARTESIAN_POINT ( 'NONE',  ( -5.204350862799341115, 7.165104988056252289, -1.599625672291271394 ) ) ;
#27341 = CARTESIAN_POINT ( 'NONE',  ( 1.499999999999989120, 1.806250000682817269, 0.000000000000000000 ) ) ;
#27340 = CARTESIAN_POINT ( 'NONE',  ( 2.197387184563174944, 1.746976956643018442, -0.7784620831182070821 ) ) ;
#27343 = CARTESIAN_POINT ( 'NONE',  ( 3.897267319706390065, 1.864829029706360330, -1.179861312946443697 ) ) ;
#27344 = CARTESIAN_POINT ( 'NONE',  ( -1.225000000000022293, 0.2916666673494853756, -0.7072540797573118043 ) ) ;
#27345 = CARTESIAN_POINT ( 'NONE',  ( 6.883263157960364254, 2.447565407927353220, 2.329071302269662080 ) ) ;
#27346 = CARTESIAN_POINT ( 'NONE',  ( -0.2108831679771168421, 6.948330828014878335, -2.492181822431015270 ) ) ;
#27347 = CARTESIAN_POINT ( 'NONE',  ( 5.736508391913541338, 6.825586224388162648, -1.082531754730548412 ) ) ;
#27348 = CARTESIAN_POINT ( 'NONE',  ( -6.739811759324840779, 7.035737605399991601, -0.7216878364870338292 ) ) ;
#27349 = CARTESIAN_POINT ( 'NONE',  ( 1.809780422520257170, -1.956919260803160032, 0.2374922769308157044 ) ) ;
#27350 = CARTESIAN_POINT ( 'NONE',  ( 2.186954941700581134, -2.263197366206463279, -0.4496495349725088686 ) ) ;
#27352 = ADVANCED_FACE ( 'NONE', ( #95122 ), #214299, .T. ) ;
#27351 = CARTESIAN_POINT ( 'NONE',  ( 2.224987305166142626, -1.792472147789250236, -0.7979012372742313453 ) ) ;
#27353 = DIRECTION ( 'NONE',  ( 0.000000000000000000, 0.000000000000000000, -1.000000000000000000 ) ) ;
#27354 = CARTESIAN_POINT ( 'NONE',  ( 5.981316409642544407, -0.05633626937831189702, 2.061977559458886056 ) ) ;
#27355 = CARTESIAN_POINT ( 'NONE',  ( 4.039966587192259873, 5.736380323189513852, 1.443375672974062551 ) ) ;
#27356 = CARTESIAN_POINT ( 'NONE',  ( 3.854704076794239764, -1.883312302057647880, -0.7212934815618715634 ) ) ;
#27357 = CARTESIAN_POINT ( 'NONE',  ( 3.718679271898170491, 7.560485927181699317, 0.7998128361456271485 ) ) ;
#27358 = ORIENTED_EDGE ( 'NONE', *, *, #43686, .T. ) ;
#27359 = CARTESIAN_POINT ( 'NONE',  ( 0.6823417656249917140, 5.655208333674749177, 1.181850606188765695 ) ) ;
#27360 = DIRECTION ( 'NONE',  ( 2.486899575160350966E-14, 0.000000000000000000, -1.000000000000000000 ) ) ;
#27361 = CARTESIAN_POINT ( 'NONE',  ( 9.317477881089539338, 11.89347683273640932, 1.599625672291279388 ) ) ;
#27362 = CARTESIAN_POINT ( 'NONE',  ( 2.096751143937364947, 2.146985459555655673, 0.3218790139906148040 ) ) ;
#27363 = CARTESIAN_POINT ( 'NONE',  ( 5.398914348987485567, 6.259949555863199677, 2.419999999999999485 ) ) ;
#27364 = CARTESIAN_POINT ( 'NONE',  ( -8.165961478353519709, 14.48012443953052397, -8.838024359600046509 ) ) ;
#27365 = CARTESIAN_POINT ( 'NONE',  ( -3.094265954482870118, 2.800000000000024691, 2.490342512183699508 ) ) ;
#27366 = CARTESIAN_POINT ( 'NONE',  ( 1.967826412060974084, 0.9573937279930484490, 1.606809688844474726 ) ) ;
#27367 = MECHANICAL_DESIGN_GEOMETRIC_PRESENTATION_REPRESENTATION (  '', ( #207328 ), #16979 ) ;
#27368 = CARTESIAN_POINT ( 'NONE',  ( 6.327428285124779173, -2.037722512857220725, 0.7216720553550812767 ) ) ;
#27370 = CARTESIAN_POINT ( 'NONE',  ( 6.827182134110231893, 2.454327069706051745, 2.294502690501096787 ) ) ;
#27369 = CARTESIAN_POINT ( 'NONE',  ( -11.35610322553117513, 13.61421628929174865, -3.553412924323506861 ) ) ;
#27371 = CARTESIAN_POINT ( 'NONE',  ( -1.364683531250000748, 0.5093750003414208027, 0.000000000000000000 ) ) ;
#27372 = EDGE_CURVE ( 'NONE', #29604, #122503, #99369, .T. ) ;
#27373 = CARTESIAN_POINT ( 'NONE',  ( 2.666550042863625958, 0.6461651886627232111, 1.799920402468312197 ) ) ;
#27374 = CARTESIAN_POINT ( 'NONE',  ( 4.346413238989558003, 0.4729554063761501892, 1.705410949051559877 ) ) ;
#27375 = CARTESIAN_POINT ( 'NONE',  ( 1.664566505720616929, 0.6010121217654046388, 1.815428919054395518 ) ) ;
#27376 = CARTESIAN_POINT ( 'NONE',  ( -4.608882153641705059, 7.464447381635583412, -1.199719254218452047 ) ) ;
#27377 = CARTESIAN_POINT ( 'NONE',  ( 6.573869778094940663, -0.8146055380063941254, 1.732351315116484880 ) ) ;
#27378 = CARTESIAN_POINT ( 'NONE',  ( 0.7499999999999885647, -0.2666666666666442365, 1.299038105676657340 ) ) ;
#27379 = CARTESIAN_POINT ( 'NONE',  ( 0.7837444799244470683, -1.966470238067185905, 0.6478734989143407619 ) ) ;
#27380 = CARTESIAN_POINT ( 'NONE',  ( -0.7500000000000215383, 5.691666666666685082, 1.299038105676671107 ) ) ;
#27381 = CARTESIAN_POINT ( 'NONE',  ( 5.102362337376947998, -0.6309395149336484154, -1.761181640970375106 ) ) ;
#27382 = CARTESIAN_POINT ( 'NONE',  ( 1.892912435568369744, 1.589020553905008626, -0.8988452475950716725 ) ) ;
#27384 = CARTESIAN_POINT ( 'NONE',  ( 4.622017735560743468, 8.339529265130579461, 0.3277269337885590494 ) ) ;
#27383 = CARTESIAN_POINT ( 'NONE',  ( 6.235036409211808461, 0.2120174297785166195, 2.196685143856290878 ) ) ;
#27385 = COLOUR_RGB ( '', 0.31764706, 0.68627451, 0.89019608) ;
#27386 = CARTESIAN_POINT ( 'NONE',  ( 0.6823417656249899377, 5.488541667008087543, -1.181850606188754593 ) ) ;
#27387 = CARTESIAN_POINT ( 'NONE',  ( 2.541531169099729759, 1.886825176844410645, -0.8337591773379445792 ) ) ;
#27388 = CARTESIAN_POINT ( 'NONE',  ( -8.050844288416501016, 8.287073179441051707, 1.040834085586084257E-14 ) ) ;
#27389 = CARTESIAN_POINT ( 'NONE',  ( 0.000000000000000000, 0.5000000000000004441, 0.000000000000000000 ) ) ;
#27390 = CARTESIAN_POINT ( 'NONE',  ( 8.646349277213076334, 11.11049346154719508, 1.599625672291281386 ) ) ;
#27391 = CARTESIAN_POINT ( 'NONE',  ( 1.422919017935823982, 3.797748325714608519, -0.5004465702263648508 ) ) ;
#27392 = CARTESIAN_POINT ( 'NONE',  ( 0.000000000000000000, 5.868705557303649734, -4.125226524755057689 ) ) ;
#27393 = CARTESIAN_POINT ( 'NONE',  ( 7.180978637093494044, 8.406838493811077839, -1.199719254218452047 ) ) ;
#27394 = ORIENTED_EDGE ( 'NONE', *, *, #85738, .T. ) ;
#27395 = CARTESIAN_POINT ( 'NONE',  ( 5.037584538744971141, 1.933038169019934527, -0.7419538039311265321 ) ) ;
#27396 = CARTESIAN_POINT ( 'NONE',  ( 0.6823417656249882723, 0.1552083336747514530, 1.181850606188755259 ) ) ;
#27397 = CARTESIAN_POINT ( 'NONE',  ( 2.530746307392011563, 2.096003997654236173, 0.5278882200696957128 ) ) ;
#27398 = CARTESIAN_POINT ( 'NONE',  ( -4.695470500997839025, 8.269974592382618894, -0.5850018098894956831 ) ) ;
#27400 = EDGE_CURVE ( 'NONE', #102205, #211122, #45931, .T. ) ;
#27399 = CARTESIAN_POINT ( 'NONE',  ( 3.510419912045096069, -2.017469964673058946, -0.09679370177045029666 ) ) ;
#27401 = CARTESIAN_POINT ( 'NONE',  ( 6.720655732516679137, 7.052218778754904882, 2.671889809988809983 ) ) ;
#27402 = EDGE_CURVE ( 'NONE', #159043, #103805, #203550, .T. ) ;
#27405 = CARTESIAN_POINT ( 'NONE',  ( 7.456621297836078632, 8.762108271306003004, 1.082531754730558626 ) ) ;
#27404 = CARTESIAN_POINT ( 'NONE',  ( -3.475000000000000533, -1.750000000000001554, 0.000000000000000000 ) ) ;
#27403 = SURFACE_SIDE_STYLE ('',( #143335 ) ) ;
#27406 = CARTESIAN_POINT ( 'NONE',  ( -6.851666526859749418, 9.086973262793417661, -1.599625672291271394 ) ) ;
#27407 = CARTESIAN_POINT ( 'NONE',  ( 0.9191581010105540628, -1.820984308097562954, 0.8666112775468015617 ) ) ;
#27409 = CARTESIAN_POINT ( 'NONE',  ( 6.374583145400191775, -0.1054333438532777389, -2.189162923280890904 ) ) ;
#27408 = CARTESIAN_POINT ( 'NONE',  ( -3.906720819032141190, 7.709591388846142479, -0.7998128361456281477 ) ) ;
#27410 = CARTESIAN_POINT ( 'NONE',  ( -1.499999999999997780, 4.931250000682820378, 1.214306433183764966E-14 ) ) ;
#27411 = CARTESIAN_POINT ( 'NONE',  ( 4.324404969281474109, -0.8226261416362996570, -1.726585468271451651 ) ) ;
#27412 = CARTESIAN_POINT ( 'NONE',  ( -4.683370693966717901, 4.898792820011970583, -0.6382510007943015262 ) ) ;
#27413 = CARTESIAN_POINT ( 'NONE',  ( 5.138177029454829459, 8.938364267765221527, 0.7216878364870438212 ) ) ;
#27415 = CARTESIAN_POINT ( 'NONE',  ( 3.585564690064909854, -0.5826378547920657569, 1.930424337232887977 ) ) ;
#27414 = CARTESIAN_POINT ( 'NONE',  ( -7.809133291347029271, 12.05447990663947877, 0.000000000000000000 ) ) ;
#27416 = CARTESIAN_POINT ( 'NONE',  ( -0.6823417656250039265, 14.13020833367473195, -1.181850606188755259 ) ) ;
#27417 = CARTESIAN_POINT ( 'NONE',  ( 5.280183324938524159, -0.9553487854751692154, 1.435786287184135368 ) ) ;
#27418 = CARTESIAN_POINT ( 'NONE',  ( 6.607619761813720238, 8.802252036906432764, 1.599625672291268286 ) ) ;
#27419 = CARTESIAN_POINT ( 'NONE',  ( 2.184835310096557404, 5.700724961754617404, 1.040834085586084257E-14 ) ) ;
#27420 = CARTESIAN_POINT ( 'NONE',  ( -1.499999999999997780, 3.931250000682819046, 1.214306433183764966E-14 ) ) ;
#27421 = CARTESIAN_POINT ( 'NONE',  ( 3.866346082213562685, -1.258301477641217803, 1.384200088751494251 ) ) ;
#27422 = DIRECTION ( 'NONE',  ( 0.9366510587354612838, 2.168404344971001926E-14, 0.3502638921866474409 ) ) ;
#27423 = CARTESIAN_POINT ( 'NONE',  ( 1.305626334525695986, -1.629615561912756805, -1.276682400165381148 ) ) ;
#27424 = STYLED_ITEM ( 'NONE', ( #34451 ), #210156 ) ;
#27425 = CARTESIAN_POINT ( 'NONE',  ( -0.1054627972275519465, 3.385846599571567417, -2.076146368081344118 ) ) ;
#27426 = ORIENTED_EDGE ( 'NONE', *, *, #4041, .F. ) ;
#27427 = CARTESIAN_POINT ( 'NONE',  ( 6.059207019112636594, -1.526464042762348594, 0.9750640111952106892 ) ) ;
#27428 = CARTESIAN_POINT ( 'NONE',  ( 3.040771591214902259, 6.769593633051179005, -0.7998128361456362523 ) ) ;
#27429 = DIRECTION ( 'NONE',  ( -3.330669073875485398E-16, 1.665334536937734071E-16, 1.000000000000000000 ) ) ;
#27430 = CARTESIAN_POINT ( 'NONE',  ( 0.2986855335190057859, -0.2218818089524568216, -1.797891974444510765 ) ) ;
#27431 = CARTESIAN_POINT ( 'NONE',  ( 5.844973620822844218, 5.991759777147701804, 0.7216878364870328300 ) ) ;
#27432 = CARTESIAN_POINT ( 'NONE',  ( 11.52856953056122791, 8.442533071845224057, -3.352610243527511358 ) ) ;
#27433 = ORIENTED_EDGE ( 'NONE', *, *, #30312, .F. ) ;
#27435 = CARTESIAN_POINT ( 'NONE',  ( 7.995557903757111617, 10.35123685918189729, 1.599625672291281386 ) ) ;
#27434 = CARTESIAN_POINT ( 'NONE',  ( 0.7484013653801385724, -1.946605496936428370, -0.2438083268051088881 ) ) ;
#27436 = CARTESIAN_POINT ( 'NONE',  ( 4.798395639560619763, 1.317935440718048135, -1.390428439694970431 ) ) ;
#27437 = CARTESIAN_POINT ( 'NONE',  ( 4.202664430556254160, 5.926194473780837413, 1.443375672974062551 ) ) ;
#27438 = CARTESIAN_POINT ( 'NONE',  ( -5.536209915801717507, 7.449110030843877794, 1.248366777010925910 ) ) ;
#27439 = CARTESIAN_POINT ( 'NONE',  ( 6.827182134110222123, -0.006956174471953178659, 2.188967759425272330 ) ) ;
#27441 = ORIENTED_EDGE ( 'NONE', *, *, #132097, .F. ) ;
#27440 = CARTESIAN_POINT ( 'NONE',  ( 4.514501963670558560, 8.210743357683563559, 1.040834085586084257E-14 ) ) ;
#27442 = CARTESIAN_POINT ( 'NONE',  ( -9.164948653157999559, 10.75515685251491504, -1.082531754730539753 ) ) ;
#27443 = CARTESIAN_POINT ( 'NONE',  ( 1.903414394802248166, 1.797162532295241366, 1.201017911493490020 ) ) ;
#27444 = CARTESIAN_POINT ( 'NONE',  ( -3.474632506852224356, 7.275764701294714420, -0.7998128361456481317 ) ) ;
#27445 = CARTESIAN_POINT ( 'NONE',  ( 6.156811154381533591, 9.236677875870187293, -1.082531754730548412 ) ) ;
#27446 = CARTESIAN_POINT ( 'NONE',  ( -4.060830702492950195, 4.696389560118578999, -1.199719254218452047 ) ) ;
#27447 = CARTESIAN_POINT ( 'NONE',  ( 4.998959831394860664, 1.517082468864182632, -1.015166198912627049 ) ) ;
#27448 = CARTESIAN_POINT ( 'NONE',  ( 8.392483990243823300, 12.96120414926864761, -8.512620520037069483 ) ) ;
#27449 = CARTESIAN_POINT ( 'NONE',  ( 0.7199194774221047144, -1.050951492028269874, -1.667678589039832904 ) ) ;
#27450 = CARTESIAN_POINT ( 'NONE',  ( 3.199369407753744454, 1.726971514772487559, -0.8218122705464236954 ) ) ;
#27451 = ORIENTED_EDGE ( 'NONE', *, *, #180525, .T. ) ;
#27452 = CARTESIAN_POINT ( 'NONE',  ( 0.000000000000000000, 9.799999999999998934, 0.000000000000000000 ) ) ;
#27453 = CARTESIAN_POINT ( 'NONE',  ( 3.789471415310685654, -1.820739144500636231, 0.7515243927636706678 ) ) ;
#27454 = ORIENTED_EDGE ( 'NONE', *, *, #102591, .T. ) ;
#27455 = CARTESIAN_POINT ( 'NONE',  ( 6.110880135979408045, -0.2334805506369178330, 1.927903797987507106 ) ) ;
#27456 = ORIENTED_EDGE ( 'NONE', *, *, #80770, .F. ) ;
#27457 = CARTESIAN_POINT ( 'NONE',  ( -6.961185525973791144, 7.086080966583015339, 0.7998128361456341429 ) ) ;
#27459 = CARTESIAN_POINT ( 'NONE',  ( 6.310795917644286490, -0.5669512758468171487, -2.043305014803979525 ) ) ;
#27458 = CARTESIAN_POINT ( 'NONE',  ( -6.310394152517827315, 6.326824364217716656, 0.7998128361456281477 ) ) ;
#27460 = CARTESIAN_POINT ( 'NONE',  ( 5.831415467209187575, 9.817418788470464008, 0.000000000000000000 ) ) ;
#27462 = ORIENTED_EDGE ( 'NONE', *, *, #108943, .F. ) ;
#27461 = CARTESIAN_POINT ( 'NONE',  ( 3.826736342760712173, 1.350229473097919630, -1.354399478966497261 ) ) ;
#27463 = DIRECTION ( 'NONE',  ( -0.000000000000000000, -1.000000000000000000, -0.000000000000000000 ) ) ;
#27464 = CARTESIAN_POINT ( 'NONE',  ( 3.390420931869152721, 6.113185632892752075, -1.199719254218452047 ) ) ;
#27465 = CIRCLE ( 'NONE', #183007, 0.9475805310473219834 ) ;
#27466 = CARTESIAN_POINT ( 'NONE',  ( 7.462104991928524278, -5.166862915010159263, 8.081892667527540652 ) ) ;
#27467 = CARTESIAN_POINT ( 'NONE',  ( 5.303390062791992321, 1.774253655011595709, -0.9511161165304935494 ) ) ;
#27468 = CARTESIAN_POINT ( 'NONE',  ( 0.007473969438204840048, 8.279395425053873936, 1.999986034896453324 ) ) ;
#27469 = CARTESIAN_POINT ( 'NONE',  ( 6.270122753791413928, 0.9430518052575274091, 1.563124558401955300 ) ) ;
#27470 = CARTESIAN_POINT ( 'NONE',  ( 2.207561477879273593, -1.661462528888792090, -1.235070534849058044 ) ) ;
#27471 = CARTESIAN_POINT ( 'NONE',  ( -6.548225005720456515, 10.58342024007512983, 0.000000000000000000 ) ) ;
#27472 = ADVANCED_FACE ( 'NONE', ( #161171 ), #64718, .T. ) ;
#27473 = CARTESIAN_POINT ( 'NONE',  ( -6.329889402343163773, 6.869280899661572626, -0.6830204514151876349 ) ) ;
#27474 = CARTESIAN_POINT ( 'NONE',  ( 1.225000000000000311, 1.874999999999994671, -1.734723475976807094E-15 ) ) ;
#27475 = CARTESIAN_POINT ( 'NONE',  ( 6.508674657442179878, 1.384610780642284711, -1.258058027910214927 ) ) ;
#27476 = CARTESIAN_POINT ( 'NONE',  ( 5.636439174979242850, 7.598931675607687453, -1.599625672291262513 ) ) ;
#27477 = FACE_OUTER_BOUND ( 'NONE', #63136, .T. ) ;
#27478 = CARTESIAN_POINT ( 'NONE',  ( 4.746763178560250651, 7.591621904078704297, 1.082531754730549078 ) ) ;
#27479 = CARTESIAN_POINT ( 'NONE',  ( 3.297657676621871925, 4.870353260857385180, 1.599625672291267398 ) ) ;
#27480 = CARTESIAN_POINT ( 'NONE',  ( 0.6823417656249969321, 11.33854166700806765, -1.181850606188757036 ) ) ;
#27481 = CARTESIAN_POINT ( 'NONE',  ( -4.894657149733403045, 5.669187081899118574, -1.199719254218446718 ) ) ;
#27483 = CARTESIAN_POINT ( 'NONE',  ( -5.607179047703544583, 8.699403434699558346, 1.199719254218454489 ) ) ;
#27482 = SURFACE_STYLE_USAGE ( .BOTH. , #175891 ) ;
#27484 = CIRCLE ( 'NONE', #72457, 12.00000000000000178 ) ;
#27485 = CARTESIAN_POINT ( 'NONE',  ( 4.236742506082516790, 1.733672338021419179, -0.04812345329192367627 ) ) ;
#27486 = CARTESIAN_POINT ( 'NONE',  ( -3.879604511804807032, 7.677955697080923514, 0.7998128361456341429 ) ) ;
#27487 = CARTESIAN_POINT ( 'NONE',  ( 0.8310238944931707117, -1.948087850137161459, -0.7009411469260096172 ) ) ;
#27488 = CARTESIAN_POINT ( 'NONE',  ( 3.321969493568678988, 0.9498371968033242352, -1.892263307760349900 ) ) ;
#27489 = CARTESIAN_POINT ( 'NONE',  ( 8.101160479365381306, 9.410107633136481908, -1.199719254218446718 ) ) ;
#27490 = CARTESIAN_POINT ( 'NONE',  ( -1.201851678989727383E-14, 3.821875000341422801, 1.575800808251672791 ) ) ;
#27491 = CARTESIAN_POINT ( 'NONE',  ( 6.930528400284448054, -1.278709912597691511, 1.628784411136071197 ) ) ;
#27492 = CARTESIAN_POINT ( 'NONE',  ( 5.327099315257549428, 6.547468694062620997, 1.346473575380419563 ) ) ;
#27493 = CARTESIAN_POINT ( 'NONE',  ( 5.666945020832181434, 5.713783400500082266, 0.7216878364870317197 ) ) ;
#27495 = CARTESIAN_POINT ( 'NONE',  ( 0.05278957052760185897, 0.3289079202175131389, 1.883742972368242174 ) ) ;
#27494 = CARTESIAN_POINT ( 'NONE',  ( 3.475000000000000533, -1.924999999999999600, 0.000000000000000000 ) ) ;
#27496 = CARTESIAN_POINT ( 'NONE',  ( 3.345926335499046722, 2.292435215394402093, 0.0001471259066659902901 ) ) ;
#27497 = CARTESIAN_POINT ( 'NONE',  ( 0.9788029507734037349, -0.04229004422508231970, -1.825371421953936757 ) ) ;
#27498 = CARTESIAN_POINT ( 'NONE',  ( 3.744317949583543470, 1.018843395500759197, -1.618198357137661469 ) ) ;
#27499 = CARTESIAN_POINT ( 'NONE',  ( 4.694866332082116678, 8.699370830729650450, 0.7998128361456341429 ) ) ;
#27500 = CARTESIAN_POINT ( 'NONE',  ( 7.117667457050084856, 7.406292909420979953, -0.7216878364870257245 ) ) ;
#27501 = CARTESIAN_POINT ( 'NONE',  ( -8.727698198895085469, 11.20540053684285553, -1.599625672291263179 ) ) ;
#27502 = CARTESIAN_POINT ( 'NONE',  ( 2.250246052928657203, 0.9454230575737303521, -1.777374461261713279 ) ) ;
#27503 = CARTESIAN_POINT ( 'NONE',  ( 2.324987154519737143, -1.791562868964852395, -0.7996954790665599111 ) ) ;
#27504 = CARTESIAN_POINT ( 'NONE',  ( -8.239604668803112375, 10.63595808506888396, -1.599625672291263179 ) ) ;
#27505 = CARTESIAN_POINT ( 'NONE',  ( -5.364222332501225488, 9.410009821226765325, 0.7998128361456481317 ) ) ;
#27506 = CARTESIAN_POINT ( 'NONE',  ( -11.63061636551515043, 7.359134869736937645, 2.774776728778091783 ) ) ;
#27508 = CARTESIAN_POINT ( 'NONE',  ( 3.027930095613054817, 0.9845384034416431174, -1.470494568931050905 ) ) ;
#27507 = CARTESIAN_POINT ( 'NONE',  ( 4.734370563723459213, 0.3569306294452011530, 2.059774728693287038 ) ) ;
#27509 = CARTESIAN_POINT ( 'NONE',  ( -11.33772463945037146, 13.39999999999998259, 3.599999999999999201 ) ) ;
#27510 = CARTESIAN_POINT ( 'NONE',  ( 6.281209671116547710, 1.576043917979405684, 1.664718807710400705 ) ) ;
#27511 = CARTESIAN_POINT ( 'NONE',  ( 5.085792842222247145, -1.727793525551263087, -0.2079256833047369302 ) ) ;
#27512 = ADVANCED_FACE ( 'NONE', ( #146009 ), #193484, .T. ) ;
#27513 = CARTESIAN_POINT ( 'NONE',  ( 7.228468454380276853, 11.58496363008569574, 1.040834085586084257E-14 ) ) ;
#27514 = LINE ( 'NONE', #64292, #132646 ) ;
#27515 = CARTESIAN_POINT ( 'NONE',  ( 6.063786081214013635, 1.415308013037285484, -1.001223213843880799 ) ) ;
#27516 = CARTESIAN_POINT ( 'NONE',  ( 6.403528931544730796, -1.954801056786956259, 0.4946215565981848528 ) ) ;
#27517 = CARTESIAN_POINT ( 'NONE',  ( 5.652828992512394457, -0.5219723807755486389, -2.107401415877676598 ) ) ;
#27518 = DIRECTION ( 'NONE',  ( -0.7592566023652971285, -0.6507913734559680474, 0.000000000000000000 ) ) ;
#27519 = CARTESIAN_POINT ( 'NONE',  ( 0.3392563814038212500, -1.792290195912203954, -1.127034558586788249 ) ) ;
#27520 = CARTESIAN_POINT ( 'NONE',  ( 5.156250000000004441, -1.895863743163967108, 0.7852924748302536617 ) ) ;
#27521 = CARTESIAN_POINT ( 'NONE',  ( -1.001543065824772872E-14, 5.243750000682815937, 1.732050807568877637 ) ) ;
#27522 = CARTESIAN_POINT ( 'NONE',  ( 3.469672154888691296, 1.879743449303279634, -0.4207095485242727806 ) ) ;
#27523 = CARTESIAN_POINT ( 'NONE',  ( -0.7500000000000179856, 11.32291666734946212, 1.299038105676658228 ) ) ;
#27524 = CARTESIAN_POINT ( 'NONE',  ( -0.1102773484824119410, -0.006951161900758255283, -2.203378182130751206 ) ) ;
#27525 = VERTEX_POINT ( 'NONE', #141516 ) ;
#27526 = CARTESIAN_POINT ( 'NONE',  ( -1.001543065824772872E-14, 4.212500000000023448, 1.732050807568877637 ) ) ;
#27527 = CARTESIAN_POINT ( 'NONE',  ( 4.801558957534076022, 8.753569217098425170, 0.7998128361456462443 ) ) ;
#27528 = B_SPLINE_CURVE_WITH_KNOTS ( 'NONE', 3,
 ( #79666, #211784, #160928, #28792, #63422, #131665, #78595, #197668, #11457, #178252 ),
 .UNSPECIFIED., .F., .F.,
 ( 4, 3, 3, 4 ),
 ( 1.626303258728287225E-19, 4.381009615557519019E-05, 0.0001116909227615702350, 0.0001805408983559123135 ),
 .UNSPECIFIED. ) ;
#27529 = EDGE_CURVE ( 'NONE', #1110, #188860, #115784, .T. ) ;
#27530 = CARTESIAN_POINT ( 'NONE',  ( 2.719623178692368359, 1.877883874979644263, 1.186199984364836313 ) ) ;
#27532 = CARTESIAN_POINT ( 'NONE',  ( -0.02900071798685525254, 1.326456003635017922, -2.425894103910302135 ) ) ;
#27531 = AXIS2_PLACEMENT_3D ( 'NONE', #64759, #112514, #33325 ) ;
#27533 = CARTESIAN_POINT ( 'NONE',  ( 8.120970824905713314, 8.576813505252564696, 1.040834085586084257E-14 ) ) ;
#27534 = ADVANCED_FACE ( 'NONE', ( #92741 ), #57018, .T. ) ;
#27535 = CARTESIAN_POINT ( 'NONE',  ( -9.178506806327330736, 10.77097469787910455, 1.082531754730558626 ) ) ;
#27536 = CARTESIAN_POINT ( 'NONE',  ( 7.675324359112103423, 8.127168971818530707, 0.7216878364870267237 ) ) ;
#27537 = CARTESIAN_POINT ( 'NONE',  ( 0.5455463417442986129, -1.458554840210561476, 1.392547631435703037 ) ) ;
#27539 = CARTESIAN_POINT ( 'NONE',  ( 5.934046607644717142, 1.225649100846971651, 1.658920436798372311 ) ) ;
#27538 = CARTESIAN_POINT ( 'NONE',  ( 8.432281472695482449, 11.92507992053172572, 1.199719254218450271 ) ) ;
#27540 = CARTESIAN_POINT ( 'NONE',  ( -11.48243876534946040, 12.30000000000000071, -3.200000000000001510 ) ) ;
#27541 = CARTESIAN_POINT ( 'NONE',  ( -3.602716132929368875, 5.226254793216122074, 1.599625672291267398 ) ) ;
#27542 = FACE_OUTER_BOUND ( 'NONE', #14392, .T. ) ;
#27543 = CARTESIAN_POINT ( 'NONE',  ( -1.201851678989727383E-14, 1.571875000341420581, 1.575800808251672791 ) ) ;
#27544 = CARTESIAN_POINT ( 'NONE',  ( 6.907498162232361238, -0.4094499450241483318, 1.831839262316947270 ) ) ;
#27545 = CARTESIAN_POINT ( 'NONE',  ( 5.818968308277153056, 0.8464176696867716787, -1.513466976307031642 ) ) ;
#27546 = CARTESIAN_POINT ( 'NONE',  ( 5.442807971621070884, -1.376865196755885146, -1.064510927867247769 ) ) ;
#27547 = CARTESIAN_POINT ( 'NONE',  ( 2.648291651658631007, 0.7751803744074429181, 2.157441745960963164 ) ) ;
#27548 = CARTESIAN_POINT ( 'NONE',  ( 1.364683531249986537, -0.3864583329919166199, 0.7879004041258500513 ) ) ;
#27549 = CARTESIAN_POINT ( 'NONE',  ( 1.728195974063054141, 0.1793598003074353686, 1.832383557197496460 ) ) ;
#27550 = CARTESIAN_POINT ( 'NONE',  ( 9.368847842243145152, 10.88907622316056312, 1.199719254218453823 ) ) ;
#27551 = SURFACE_SIDE_STYLE ('',( #43830 ) ) ;
#27552 = CARTESIAN_POINT ( 'NONE',  ( 2.502731746374619259, 1.467688513602287470, -1.085450786651315225 ) ) ;
#27553 = CARTESIAN_POINT ( 'NONE',  ( 3.656875104409584853, 1.122498086849915921, 1.674887873639265390 ) ) ;
#27554 = CARTESIAN_POINT ( 'NONE',  ( -3.809477975315625375, 4.507107728365378208, 1.082531754730558626 ) ) ;
#27555 = CARTESIAN_POINT ( 'NONE',  ( 7.577342237528466029, 14.99429123645997919, -10.16790800466224987 ) ) ;
#27556 = CARTESIAN_POINT ( 'NONE',  ( 4.928798221971478988, 2.014404525830254311, 0.6141583887315901213 ) ) ;
#27557 = CARTESIAN_POINT ( 'NONE',  ( -4.889686956022917919, 8.856385215335397021, 1.214306433183764966E-14 ) ) ;
#27558 = CARTESIAN_POINT ( 'NONE',  ( 9.188757668294085690, 13.26368734670581340, 9.042387243776373040 ) ) ;
#27559 = CARTESIAN_POINT ( 'NONE',  ( 3.016144355299533952, 2.060630728401948275, -0.2003171163396169074 ) ) ;
#27560 = CARTESIAN_POINT ( 'NONE',  ( 3.167801447087334576, 6.847518788243868393, -0.7998128361456291469 ) ) ;
#27561 = CARTESIAN_POINT ( 'NONE',  ( -0.6801582343750334214, 1.213541667008023683, 1.178068619123810334 ) ) ;
#27562 = CARTESIAN_POINT ( 'NONE',  ( 4.934296419935966682, -1.134874685878878520, -1.791058398909770588 ) ) ;
#27563 = CARTESIAN_POINT ( 'NONE',  ( 0.7328819429333592872, 0.1407736501095498138, 1.921419779381093207 ) ) ;
#27564 = ORIENTED_EDGE ( 'NONE', *, *, #66694, .T. ) ;
#27565 = CARTESIAN_POINT ( 'NONE',  ( -3.806807270387036368, 7.663301925418665839, 0.000000000000000000 ) ) ;
#27566 = CARTESIAN_POINT ( 'NONE',  ( 9.260382613333817403, 10.76253345609967660, -1.199719254218446718 ) ) ;
#27567 = CARTESIAN_POINT ( 'NONE',  ( 6.034787771414195312, 6.213209619504250547, -0.7216878364870458196 ) ) ;
#27568 = CARTESIAN_POINT ( 'NONE',  ( 3.475000000000000533, -0.8020833323774190227, -2.006292185433951047 ) ) ;
#27569 = CARTESIAN_POINT ( 'NONE',  ( -4.741601036477307574, 6.554953847355395880, 1.599625672291267398 ) ) ;
#27570 = CARTESIAN_POINT ( 'NONE',  ( 5.713165544288242970, 1.732532623411761286, -1.222520872474173848 ) ) ;
#27571 = CARTESIAN_POINT ( 'NONE',  ( 1.430846025165666280, 2.029450977514839938, 0.5621798225463514598 ) ) ;
#27572 = CARTESIAN_POINT ( 'NONE',  ( -5.764151584465413869, 6.753873599078290546, -1.199719254218453823 ) ) ;
#27573 = CARTESIAN_POINT ( 'NONE',  ( 6.414979237560321401, 10.63589287712906462, 1.040834085586084257E-14 ) ) ;
#27574 = CARTESIAN_POINT ( 'NONE',  ( 6.649252725998297642, 1.619456339520190413, -0.9165514639192672286 ) ) ;
#27575 = CARTESIAN_POINT ( 'NONE',  ( 8.101160479365381306, 9.410107633136481908, -1.199719254218446718 ) ) ;
#27576 = CYLINDRICAL_SURFACE ( 'NONE', #164598, 1.224999999999996980 ) ;
#27577 = CARTESIAN_POINT ( 'NONE',  ( -4.228163802615396705, 6.026220084508304708, -1.599625672291271394 ) ) ;
#27578 = CARTESIAN_POINT ( 'NONE',  ( -4.274898507010545856, 3.881803101134051470, -0.7998128361456221525 ) ) ;
#27580 = CARTESIAN_POINT ( 'NONE',  ( -0.1577409392781377873, -1.310076727147227560, -1.668215054097483385 ) ) ;
#27579 =( GEOMETRIC_REPRESENTATION_CONTEXT ( 3 ) GLOBAL_UNCERTAINTY_ASSIGNED_CONTEXT ( ( #626 ) ) GLOBAL_UNIT_ASSIGNED_CONTEXT ( ( #100266, #134926, #1670 ) ) REPRESENTATION_CONTEXT ( 'NONE', 'WORKASPACE' ) );
#27581 = CARTESIAN_POINT ( 'NONE',  ( -3.023105066167326882, 5.702484939155337607, -7.499999999999997335 ) ) ;
#27583 = CARTESIAN_POINT ( 'NONE',  ( 2.400770673373255448, 0.4268909467371252431, 1.914702609522442867 ) ) ;
#27582 = CARTESIAN_POINT ( 'NONE',  ( -1.360316468750013108, 2.921875000341411788, -1.734723475976807094E-14 ) ) ;
#27584 = CARTESIAN_POINT ( 'NONE',  ( 1.534274790466340299, 1.065227450066742687, -1.880959520452238465 ) ) ;
#27586 = CARTESIAN_POINT ( 'NONE',  ( -5.789194372615304118, 6.219231786955013774, 1.015549131865096211 ) ) ;
#27585 = CARTESIAN_POINT ( 'NONE',  ( -5.152980901645737077, 8.169505597632108262, -1.199719254218453823 ) ) ;
#27587 = CARTESIAN_POINT ( 'NONE',  ( -1.364683531250014514, 1.238541667008091096, -0.7879004041258289570 ) ) ;
#27588 = CARTESIAN_POINT ( 'NONE',  ( 2.952174690553764691, 1.223825555390768871, 1.228469256970601498 ) ) ;
#27589 = CARTESIAN_POINT ( 'NONE',  ( 2.114833760799132989, -1.688328753782810221, 0.4216566245275765179 ) ) ;
#27590 = CARTESIAN_POINT ( 'NONE',  ( 5.775410249741494972, 8.721433810464993996, -1.082531754730537088 ) ) ;
#27591 = CARTESIAN_POINT ( 'NONE',  ( -11.03396297008821847, 6.349565552376400746, 6.086320354413141231 ) ) ;
#27592 = CARTESIAN_POINT ( 'NONE',  ( 1.774767310740913207, -2.001205085354029301, 0.2439901982170673833 ) ) ;
#27593 = CARTESIAN_POINT ( 'NONE',  ( 6.825078400183511640, 3.690008145721306310, 2.558400262806997283 ) ) ;
#27594 = CARTESIAN_POINT ( 'NONE',  ( -3.688700311369816909, 6.461178242310183784, -1.199719254218450271 ) ) ;
#27595 = CARTESIAN_POINT ( 'NONE',  ( 1.551575459862795325, 0.5740822587161975576, -1.886020533208163430 ) ) ;
#27597 = CARTESIAN_POINT ( 'NONE',  ( -5.722950238744243023, 7.770137593325314285, 1.443375672974058777 ) ) ;
#27596 = CARTESIAN_POINT ( 'NONE',  ( 5.379139070037473935, -1.731557697741787916, -0.8120211572784155063 ) ) ;
#27598 = CARTESIAN_POINT ( 'NONE',  ( -4.462041952228942954, 8.219816354326809460, -0.7216878364870338292 ) ) ;
#27599 = CARTESIAN_POINT ( 'NONE',  ( 6.550524494058025837, 7.671308660269694712, -1.199719254218452047 ) ) ;
#27600 = CARTESIAN_POINT ( 'NONE',  ( -6.740338644649361832, 7.892758502626242567, -1.199719254218452047 ) ) ;
#27601 = CARTESIAN_POINT ( 'NONE',  ( 1.190109814708179670, 1.204940744830071075, 1.620691797242173937 ) ) ;
#27602 =( NAMED_UNIT ( * ) PLANE_ANGLE_UNIT ( ) SI_UNIT ( $, .RADIAN. ) );
#27603 = CARTESIAN_POINT ( 'NONE',  ( 5.772612788190349953, -1.469667252935745960, 1.779063562929294129 ) ) ;
#27605 = EDGE_CURVE ( 'NONE', #132967, #87946, #90720, .T. ) ;
#27604 = CARTESIAN_POINT ( 'NONE',  ( 6.232861002365865488, -1.862453515449840724, -0.6167318247369477646 ) ) ;
#27606 = CARTESIAN_POINT ( 'NONE',  ( 3.133595828963112950, 1.864314371477162169, -0.6108997337519045390 ) ) ;
#27607 = CARTESIAN_POINT ( 'NONE',  ( 8.503988664269582998, 10.94440607977979063, 1.599625672291281386 ) ) ;
#27608 = CARTESIAN_POINT ( 'NONE',  ( 0.4752326960846975923, -2.001511663014220677, -0.2440270837566413387 ) ) ;
#27609 = ORIENTED_EDGE ( 'NONE', *, *, #30193, .F. ) ;
#27610 = CARTESIAN_POINT ( 'NONE',  ( 1.763061546204633290, -0.1096309319212440264, -2.114649557665876145 ) ) ;
#27612 = CARTESIAN_POINT ( 'NONE',  ( -8.182509401047415309, 9.505014708432145909, 1.199719254218462483 ) ) ;
#27611 = CARTESIAN_POINT ( 'NONE',  ( -5.122283107864663343, 4.870418468797203637, 0.000000000000000000 ) ) ;
#27613 = CARTESIAN_POINT ( 'NONE',  ( 1.991909005812149358, -0.4902695928585449892, -1.774584731258487036 ) ) ;
#27614 = ORIENTED_EDGE ( 'NONE', *, *, #40619, .F. ) ;
#27615 = CARTESIAN_POINT ( 'NONE',  ( 11.92546669328318565, 7.608715049294008992, 0.8935118259774108562 ) ) ;
#27616 = CARTESIAN_POINT ( 'NONE',  ( 2.971057270251746818, -1.603071526910588629, 1.388259434452358665 ) ) ;
#27617 = CARTESIAN_POINT ( 'NONE',  ( -1.201851678989727383E-14, 4.368750000682820378, -1.732050807568863648 ) ) ;
#27618 = CARTESIAN_POINT ( 'NONE',  ( 6.414979237560321401, 10.63589287712906462, 1.040834085586084257E-14 ) ) ;
#27619 = CARTESIAN_POINT ( 'NONE',  ( 8.188198428010544205, 8.517596018959260107, 0.000000000000000000 ) ) ;
#27620 = CARTESIAN_POINT ( 'NONE',  ( 3.268875894143012939, -1.902732241629549348, -0.7919657925325486181 ) ) ;
#27621 = COLOUR_RGB ( '', 0.72549020, 0.75294118, 0.79215686) ;
#27623 = CARTESIAN_POINT ( 'NONE',  ( 0.5734669319550633748, -1.023298125840161887, 1.530493987491374330 ) ) ;
#27622 = CARTESIAN_POINT ( 'NONE',  ( -7.069687034522070590, 10.33538640932937724, -1.199719254218440723 ) ) ;
#27624 = CARTESIAN_POINT ( 'NONE',  ( 1.364683531249990311, 4.134375000341417028, 1.214306433183764966E-14 ) ) ;
#27625 = CARTESIAN_POINT ( 'NONE',  ( -0.02244404828157658613, -0.004869073801674199918, -2.189079685368473527 ) ) ;
#27626 = CARTESIAN_POINT ( 'NONE',  ( 1.390391755498380011, 4.148600085824341477, 0.5639175007713970178 ) ) ;
#27627 = CARTESIAN_POINT ( 'NONE',  ( 0.4873205249028254027, -0.2742316277877173691, -2.189713876267186166 ) ) ;
#27628 = CARTESIAN_POINT ( 'NONE',  ( 3.128476345081227628, 1.259638568860393493, -1.879123747193896632 ) ) ;
#27629 = CARTESIAN_POINT ( 'NONE',  ( -9.490344339885981029, 10.17441593939621924, -0.7216878364870267237 ) ) ;
#27630 = CARTESIAN_POINT ( 'NONE',  ( 2.179683618226692321, 1.775955819808447966, -0.3565394459093262358 ) ) ;
#27631 = CARTESIAN_POINT ( 'NONE',  ( 3.415159944131008096, -1.768026670962073110, 0.7381028802780668086 ) ) ;
#27632 = CARTESIAN_POINT ( 'NONE',  ( 3.789561645344252661, -1.914057400617325433, 0.7896510022299551013 ) ) ;
#27633 = CARTESIAN_POINT ( 'NONE',  ( -1.364683531250012516, 2.301041667008087988, -0.7879004041258289570 ) ) ;
#27634 = CARTESIAN_POINT ( 'NONE',  ( 2.887526864075397715, 1.393042391738574137, 1.395278474455765805 ) ) ;
#27635 = CARTESIAN_POINT ( 'NONE',  ( 0.09454951164026764721, -0.4206464163897213893, -1.887090839307656864 ) ) ;
#27636 = CARTESIAN_POINT ( 'NONE',  ( 2.465516990510143280, 1.834972510290140191, -0.3627323784974947340 ) ) ;
#27637 = MECHANICAL_DESIGN_GEOMETRIC_PRESENTATION_REPRESENTATION (  '', ( #124515 ), #24213 ) ;
#27639 = CARTESIAN_POINT ( 'NONE',  ( 4.913571454530422322, 8.125067815752732514, -1.031885869761673069 ) ) ;
#27638 = CARTESIAN_POINT ( 'NONE',  ( 2.737322364211117520, 0.2836107604972230578, 2.290143083710040717 ) ) ;
#27640 = CARTESIAN_POINT ( 'NONE',  ( 2.488518357381704238, 1.804271297518467820, 0.4556280478851971183 ) ) ;
#27641 = CARTESIAN_POINT ( 'NONE',  ( 0.6823417656249899377, 2.342708333674753618, 1.181850606188767472 ) ) ;
#27642 = CARTESIAN_POINT ( 'NONE',  ( 6.373490837812130216, -0.2564121905142978664, 2.046633738985944806 ) ) ;
#27643 = CARTESIAN_POINT ( 'NONE',  ( -4.249591082879585535, 7.045274465746411252, 1.199719254218464037 ) ) ;
#27644 = CARTESIAN_POINT ( 'NONE',  ( 6.100279051144945619, 9.204410428722734849, -1.199719254218440723 ) ) ;
#27645 = CARTESIAN_POINT ( 'NONE',  ( -1.393530502278612637, 3.362191428456961617, -0.1277288169565338194 ) ) ;
#27646 =( BOUNDED_CURVE ( )  B_SPLINE_CURVE ( 2, ( #206898, #154970, #171208 ),
 .UNSPECIFIED., .F., .T. ) 
 B_SPLINE_CURVE_WITH_KNOTS ( ( 3, 3 ),
 ( 0.2500000000000002776, 0.2551636414462434277 ),
 .UNSPECIFIED. ) 
 CURVE ( )  GEOMETRIC_REPRESENTATION_ITEM ( )  RATIONAL_B_SPLINE_CURVE ( ( 0.9999999999999955591, 0.9169843866685133404, 0.9368478601411348583 ) ) 
 REPRESENTATION_ITEM ( '' )  );
#27647 = CARTESIAN_POINT ( 'NONE',  ( 0.2586047683651994666, 0.8082109201883975746, 1.945024607815620366 ) ) ;
#27648 = CARTESIAN_POINT ( 'NONE',  ( 1.364683531249990311, 3.696875000341416584, 1.214306433183764966E-14 ) ) ;
#27649 = CARTESIAN_POINT ( 'NONE',  ( 6.503215372615936296, 1.793156143535659330, 1.206815395834538451 ) ) ;
#27650 = B_SPLINE_CURVE_WITH_KNOTS ( 'NONE', 3,
 ( #206665, #176322, #174208, #25781, #160061, #192542, #91893, #157949, #28998, #126581, #109257, #10594 ),
 .UNSPECIFIED., .F., .F.,
 ( 4, 2, 2, 2, 2, 4 ),
 ( 0.000000000000000000, 0.0006161371811066557137, 0.001232274362213311427, 0.001540342952766639338, 0.001848411543319967466, 0.002464548724426622421 ),
 .UNSPECIFIED. ) ;
#27652 = EDGE_CURVE ( 'NONE', #27064, #34845, #63936, .T. ) ;
#27651 = CARTESIAN_POINT ( 'NONE',  ( -0.01731643392406666954, -1.316173432332496507, 1.532187831819804780 ) ) ;
#27653 = CARTESIAN_POINT ( 'NONE',  ( 1.364683531249986981, -1.115624999658580752, 0.000000000000000000 ) ) ;
#27654 = CARTESIAN_POINT ( 'NONE',  ( -4.446711195602252253, 6.210915699667823198, -1.443375672974053447 ) ) ;
#27655 = ADVANCED_FACE ( 'NONE', ( #110104 ), #173752, .T. ) ;
#27658 = CARTESIAN_POINT ( 'NONE',  ( 4.378920427533921078, 4.211088041652093494, 1.214306433183764966E-14 ) ) ;
#27657 = CARTESIAN_POINT ( 'NONE',  ( 6.925078400183531713, 7.629137130509067610, 2.355651831298340326 ) ) ;
#27656 = CARTESIAN_POINT ( 'NONE',  ( 5.013482942003290255, 9.071090208970993274, -0.7998128361456481317 ) ) ;
#27659 = FACE_OUTER_BOUND ( 'NONE', #128417, .T. ) ;
#27660 = CARTESIAN_POINT ( 'NONE',  ( 4.311732611912100666, -1.244383703160652610, -1.586670621409623116 ) ) ;
#27661 = CARTESIAN_POINT ( 'NONE',  ( -7.527801604085656351, 9.805521176231838609, 1.599625672291295375 ) ) ;
#27663 = CARTESIAN_POINT ( 'NONE',  ( -7.119440060507479018, 8.439006504414422238, 1.082531754730549078 ) ) ;
#27662 = CARTESIAN_POINT ( 'NONE',  ( -10.30383355670593737, 11.12348669235284504, -0.7216878364870267237 ) ) ;
#27664 = CARTESIAN_POINT ( 'NONE',  ( 4.779848517908583894, 4.883929213520019630, -0.7538207499340529028 ) ) ;
#27666 = CARTESIAN_POINT ( 'NONE',  ( 0.6823417656249969321, 10.02604166700806587, -1.181850606188757036 ) ) ;
#27665 = CARTESIAN_POINT ( 'NONE',  ( 5.840740251263128791, 0.4172088472891195554, 2.120894824392767664 ) ) ;
#27667 = CARTESIAN_POINT ( 'NONE',  ( 10.00050683067318502, 3.975933801733730011, -5.773795310722014129 ) ) ;
#27668 = CARTESIAN_POINT ( 'NONE',  ( -9.809487834687324437, 11.40315621434539395, 1.199719254218462483 ) ) ;
#27670 = CARTESIAN_POINT ( 'NONE',  ( -0.1411974294642202310, -0.0004739540254597266757, -1.900147702309512132 ) ) ;
#27669 = CARTESIAN_POINT ( 'NONE',  ( -6.860062538390436337, 7.105753837651378468, 1.040834085586084257E-14 ) ) ;
#27671 = CARTESIAN_POINT ( 'NONE',  ( -1.402160292154681736E-14, 0.7593750003414168059, -1.575800808251659024 ) ) ;
#27672 = DIRECTION ( 'NONE',  ( 0.6483454320283799088, 0.000000000000000000, -0.7613463080411786432 ) ) ;
#27673 = PLANE ( 'NONE',  #176250 ) ;
#27674 = CARTESIAN_POINT ( 'NONE',  ( 1.400563108759992792, 1.411875272319111696, -0.9905557981151734692 ) ) ;
#27675 = CARTESIAN_POINT ( 'NONE',  ( 6.912678218121202534, 9.158153569265168770, 1.599625672291268286 ) ) ;
#27676 = CARTESIAN_POINT ( 'NONE',  ( 4.681308178468477799, 8.683552984847038303, 0.000000000000000000 ) ) ;
#27677 = CARTESIAN_POINT ( 'NONE',  ( -0.6823417656250003738, -0.9697916663252494907, -1.181850606188749264 ) ) ;
#27678 = CARTESIAN_POINT ( 'NONE',  ( 0.4909911900966601461, 1.305473228555413812, 1.195063304280475025 ) ) ;
#27679 = CARTESIAN_POINT ( 'NONE',  ( 2.156891369321057628, 0.4431265858878992159, 1.963560470019373172 ) ) ;
#27680 = SURFACE_STYLE_FILL_AREA ( #78559 ) ;
#27681 = CARTESIAN_POINT ( 'NONE',  ( 4.735508036034060453, -2.019198892066270457, 0.8907332283012432406 ) ) ;
#27682 = CARTESIAN_POINT ( 'NONE',  ( 5.331008558256671748, -2.041869270619638854, -0.7380826535893101337 ) ) ;
#27683 = ORIENTED_EDGE ( 'NONE', *, *, #113758, .F. ) ;
#27684 = CARTESIAN_POINT ( 'NONE',  ( -0.7500000000000249800, -0.5583333333333134751, 1.299038105676659116 ) ) ;
#27685 = CARTESIAN_POINT ( 'NONE',  ( 7.361714222096048310, 10.57212177821199184, -1.082531754730537976 ) ) ;
#27687 = CARTESIAN_POINT ( 'NONE',  ( 2.513296185832504470, -1.880429104915388727, 0.7283969491318904588 ) ) ;
#27686 = CARTESIAN_POINT ( 'NONE',  ( 3.246849895443252532, 2.069243461727567013, 0.4626693848822636124 ) ) ;
#27689 = ORIENTED_EDGE ( 'NONE', *, *, #82128, .F. ) ;
#27688 = CARTESIAN_POINT ( 'NONE',  ( 3.638735373827857167, 1.721918111813141916, 0.5631709482423822299 ) ) ;
#27690 = CARTESIAN_POINT ( 'NONE',  ( 7.035755370848908896, 7.173079118937375931, 0.7998128361456352531 ) ) ;
#27691 = ORIENTED_EDGE ( 'NONE', *, *, #73601, .T. ) ;
#27692 = AXIS2_PLACEMENT_3D ( 'NONE', #12285, #62128, #142345 ) ;
#27693 = CARTESIAN_POINT ( 'NONE',  ( -10.79920600060118119, -6.027819618361849763, 1.138412281109779656E-15 ) ) ;
#27694 = CARTESIAN_POINT ( 'NONE',  ( 5.015626762051672571, 7.938982758113895422, 1.199719254218462483 ) ) ;
#27695 = ADVANCED_FACE ( 'NONE', ( #208574 ), #60207, .F. ) ;
#27696 = CARTESIAN_POINT ( 'NONE',  ( 6.551389018236878137, -1.469694460105780642, -1.082916835497591324 ) ) ;
#27698 = CARTESIAN_POINT ( 'NONE',  ( 1.692462117551472911, 1.416773270106906235, -1.289619884002331407 ) ) ;
#27697 = CARTESIAN_POINT ( 'NONE',  ( -3.578462479003122976, 6.262291094557191684, 1.199719254218464037 ) ) ;
#27699 = CARTESIAN_POINT ( 'NONE',  ( -10.10707714348148301, 4.359868340440408829, -5.857196085253971063 ) ) ;
#27700 = DIRECTION ( 'NONE',  ( 1.000000000000000000, 1.725633230170963762E-31, 8.638326563840814399E-31 ) ) ;
#27701 = CARTESIAN_POINT ( 'NONE',  ( 1.364683531249988535, 1.426041667008083991, 0.7879004041258500513 ) ) ;
#27702 = DIRECTION ( 'NONE',  ( -0.000000000000000000, -1.000000000000000000, -0.000000000000000000 ) ) ;
#27703 = CARTESIAN_POINT ( 'NONE',  ( -7.486073373039941359, 11.88550270185529278, -0.7998128361456291469 ) ) ;
#27704 = ORIENTED_EDGE ( 'NONE', *, *, #90295, .T. ) ;
#27705 = CARTESIAN_POINT ( 'NONE',  ( 5.348557406608104969, 0.6236849695623291057, 2.069784783864880851 ) ) ;
#27706 = CARTESIAN_POINT ( 'NONE',  ( -4.326460416536637155, 8.061637896019123062, 0.000000000000000000 ) ) ;
#27707 = CARTESIAN_POINT ( 'NONE',  ( -5.752402313948099533, 9.933162809573264695, -0.7998128361456362523 ) ) ;
#27708 = CARTESIAN_POINT ( 'NONE',  ( 2.935903058640790597, -2.042584291827519660, 0.5695675404085094318 ) ) ;
#27710 = CARTESIAN_POINT ( 'NONE',  ( -10.85768919388902809, 5.702095803505641491, 6.451939001899068771 ) ) ;
#27709 = CARTESIAN_POINT ( 'NONE',  ( -0.1298852118744257267, 5.725805934370246320, -2.320586200942467148 ) ) ;
#27711 = CARTESIAN_POINT ( 'NONE',  ( 4.094965523422711584, 1.667053662060855812, -1.051937181705852931 ) ) ;
#27712 = CARTESIAN_POINT ( 'NONE',  ( -0.01731850797281712928, -1.311767784893268285, 1.527291784361783922 ) ) ;
#27713 = ORIENTED_EDGE ( 'NONE', *, *, #202741, .T. ) ;
#27714 = CARTESIAN_POINT ( 'NONE',  ( 5.225823379661913570, 0.8554599082026111967, -1.936989086107894664 ) ) ;
#27715 =( NAMED_UNIT ( * ) PLANE_ANGLE_UNIT ( ) SI_UNIT ( $, .RADIAN. ) );
#27716 = CARTESIAN_POINT ( 'NONE',  ( 0.1392002015415672034, -0.1474423581745692435, -2.037351525059682977 ) ) ;
#27717 = CARTESIAN_POINT ( 'NONE',  ( 2.818227900350485982, 1.828750386608999356, 0.6536940613037258707 ) ) ;
#27718 = ORIENTED_EDGE ( 'NONE', *, *, #18997, .T. ) ;
#27719 = CARTESIAN_POINT ( 'NONE',  ( -4.299226640135908717, 7.262029271172127487, -0.9639859114825770625 ) ) ;
#27720 = CARTESIAN_POINT ( 'NONE',  ( 7.523848900940885542, 7.742521570711348389, 0.7998128361456291469 ) ) ;
#27722 = CARTESIAN_POINT ( 'NONE',  ( 6.819914962873951936, 7.915321197229798322, -1.199719254218446718 ) ) ;
#27721 = CARTESIAN_POINT ( 'NONE',  ( 4.013684974745008738, -1.074646439955847965, -1.793145193944564175 ) ) ;
#27723 = CARTESIAN_POINT ( 'NONE',  ( 3.404505970362959655, 6.986024375483197879, 0.7216878364870257245 ) ) ;
#27725 = ORIENTED_EDGE ( 'NONE', *, *, #209210, .T. ) ;
#27724 = CARTESIAN_POINT ( 'NONE',  ( 0.1877650794145177826, 1.041282258498995361, 1.482055844031314518 ) ) ;
#27726 = CARTESIAN_POINT ( 'NONE',  ( 5.145248760827346501, -1.894204247122273088, 1.132176536499051700 ) ) ;
#27727 = CARTESIAN_POINT ( 'NONE',  ( -0.1480828224388838488, -6.655928102867010310, -10.87712779691733722 ) ) ;
#27728 = CARTESIAN_POINT ( 'NONE',  ( 2.591098708763440062, -0.3764507303484417311, -2.174265822884546395 ) ) ;
#27729 = CARTESIAN_POINT ( 'NONE',  ( 7.313733799568044702, 10.62010763521636214, 1.199719254218460707 ) ) ;
#27730 = CARTESIAN_POINT ( 'NONE',  ( -5.886439722289627419, 6.118937485343679761, -0.7679415244158314113 ) ) ;
#27731 = CARTESIAN_POINT ( 'NONE',  ( 1.330556988563241561, 1.283596529665396169, -1.417643162000304935 ) ) ;
#27732 =( BOUNDED_SURFACE ( )  B_SPLINE_SURFACE ( 1, 2, ( 
 ( #156997, #8584, #206781, #59471, #25894, #125630, #43250, #58414, #126694, #175377, #142901, #92004, #188401, #124568, #190528, #108299, #44308, #158064, #88795, #9650, #6437, #109369, #93067, #204633, #22683, #154853, #72513, #56284, #40038, #106149, #172173, #131983, #161248, #94138, #177500, #29113, #48573, #197991, #12834, #130941, #111493, #13902, #179632, #97329, #95196, #110430, #147142, #148204, #16027, #78908, #214204, #211034, #180683, #79983, #145030, #96264, #62660, #196934, #82111, #128818, #61606, #193732, #194801, #32309, #212098, #162316, #178568, #160177, #31254, #65835, #46437, #195878, #112555, #146086, #176434, #30175, #163385, #164439, #14959, #81057, #47516, #213168, #63735, #28045, #129893, #113628, #77850, #11777, #143973, #209966, #127776, #64797, #45377, #114691, #98376, #152463, #18165, #166578, #184937, #69046, #5104, #100503, #1907, #167640, #17095, #67967, #183883, #151405, #136224, #199039, #150339, #201182, #52820, #182813, #21361, #19242, #102649, #118958, #36561, #168705, #50687, #86394, #165502, #186007, #71180, #103720, #83174, #202245, #117891, #116812, #200119, #70111, #134110, #34429, #84253, #85322, #51772, #137299, #49619, #830, #35495, #4043, #101573, #2978, #169771, #115744, #135166, #20309, #53896, #120032, #149257, #66900, #87468, #37642, #153535, #133040, #181733, #33365, #99447, #22433, #39785, #6184, #138360, #106973, #26721, #188153, #191340, #8336, #158867, #74421, #204378, #203316, #187083, #57098, #76537, #43006, #109119, #38716, #41939, #105890, #24578, #171916, #56034, #73328, #54966, #190281, #174076, #23512, #170843, #40868, #157812, #89617, #122187, #154605, #9411, #108051, #175133, #155668, #206534, #172997, #7252, #139430, #205465, #123264, #189229, #90685, #156746, #104796, #140520, #72252, #88543, #25648, #207599, #58164, #124322, #91759, #75482, #141593, #59219, #125377, #92822, #10463, #121118, #209721, #93893, #142648, #161000, #179392, #159932, #94952, #29938, #28865, #14723, #178330, #31012, #80814, #126446, #112315, #129651, #111250, #208657, #127525, #193496, #210800, #45138, #61367, #177253, #96022, #98146, #60287, #12592, #176194, #192409, #164195, #44065, #11535, #62423, #97087, #78666, #144793, #48332, #15782, #162074, #128588, #13664, #194554, #110183, #27795, #114442, #143728, #79736, #77605, #46197, #146905, #145852, #211859, #63496, #195636, #47269, #113384, #180443, #163140, #130702, #212924, #64558, #196693, #32059, #81867, #65586, #150076, #169510, #135957, #201972, #131733, #134907, #198787, #117632, #66639, #148997, #166313, #147953, #68787, #52561, #50436, #49378, #133854, #36299, #116555, #573, #33120, #102375, #200913, #53630, #132784, #85060, #51507, #182549, #34173, #100245, #17903, #83988, #1648, #67706, #197739, #199864, #99198, #115496, #118693, #86131, #183623, #35231, #16842, #181491, #18976, #101306, #167386, #2714, #82924, #151146, #184677, #165249, #213966, #168445, #20044, #152204, #3772, #69846, #119762, #185741, #37375, #103450, #8071, #153260, #89351, #40599, #5912, #21092, #88269, #154337, #39513, #71986, #138095, #204108, #155399, #25393, #87196, #121916, #120845, #137025, #107789, #54694, #206273, #23239, #55760, #105611, #140251, #187885, #22154, #171642, #6981, #73062, #170573, #188959, #4835, #139161, #203052, #205191, #56832, #124061, #70915, #123003, #173814, #106705, #172729, #74157, #57897, #24307, #186819, #41678, #38447, #104527, #90412, #156482, #190026, #91492, #79769, #47304, #110216, #127558, #93923, #60318, #96055, #128620, #193527, #145883, #159963, #45169, #11568, #176223, #158899, #177286, #195669, #27825, #111281, #46232, #28901, #31045, #194586, #113418, #97121, #142679, #112349, #211892, #94986, #10495, #143760, #209755, #12627, #61396, #77638, #161032, #178362, #114479, #76568, #78698, #192441, #208690, #212955, #126477, #163173, #144825, #210832, #62457, #179425, #29969, #162108, #13697, #63531, #129685, #180477, #44096, #14758, #80849, #146940, #64594, #130733, #196726, #32094, #48366, #100283, #199900, #166349, #65620, #197773, #3812, #99235, #51546, #49410, #131769, #184713, #181526 ),
 ( #17940, #185780, #152240, #69884, #147989, #151182, #608, #133893, #82959, #165284, #182587, #164228, #85097, #68823, #118728, #16878, #1689, #167425, #2754, #149032, #119801, #134945, #135996, #202010, #66675, #53669, #198827, #35267, #15816, #117670, #200951, #132823, #36337, #98180, #50472, #115531, #33154, #116593, #168483, #183663, #150116, #84026, #81901, #19017, #213999, #34210, #101344, #67743, #52600, #102415, #20082, #86170, #91534, #90455, #8112, #188998, #24345, #171681, #103490, #170612, #55800, #4876, #75259, #125161, #207384, #59005, #22199, #157593, #206313, #39552, #140294, #5953, #154376, #172771, #56871, #37414, #88312, #204145, #155438, #70955, #121955, #23278, #139200, #124102, #186859, #138136, #40641, #106744, #72024, #9188, #7023, #156521, #74200, #57937, #190065, #38489, #41717, #153300, #173852, #169551, #104567, #137065, #141373, #89390, #187921, #73099, #107827, #25428, #21132, #87236, #205230, #203090, #54735, #120885, #105653, #123047, #144571, #27569, #43851, #162922, #112102, #108895, #11308, #26498, #79525, #178105, #158648, #13449, #93667, #14502, #179169, #63274, #60070, #128372, #212706, #159709, #174918, #109965, #175976, #129436, #64347, #77386, #80594, #94734, #29721, #194339, #95803, #45981, #126226, #145643, #92605, #113165, #146690, #143502, #10246, #30793, #177030, #209499, #28647, #161859, #211638, #195419, #47049, #111025, #191120, #96872, #42786, #76322, #142427, #210585, #61139, #127301, #208436, #192187, #193272, #44917, #160780, #12373, #78453, #62215, #167176, #181279, #102170, #118485, #2502, #213754, #67501, #151995, #32905, #114234, #197526, #49170, #68574, #3567, #98983, #150939, #131523, #33963, #199646, #117418, #115288, #130493, #18765, #168237, #36086, #165036, #19836, #16629, #133647, #196480, #149868, #183415, #82713, #134701, #85922, #148790, #81651, #65377, #360, #200706, #17689, #182335, #198578, #180232, #51293, #48122, #66432, #1436, #132575, #166103, #31855, #50225, #35018, #184469, #101089, #84849, #52357, #97931, #116344, #163989, #100040, #83775, #15564, #147738, #157339, #25178, #91280, #202841, #123850, #24102, #71774, #172517, #38238, #186612, #204979, #89141, #69641, #120634, #21945, #187673, #37164, #88055, #203909, #171436, #156270, #4629, #170360, #6776, #72851, #54490, #41463, #104311, #20886, #153053, #154127, #140033, #23026, #121711, #137890, #53413, #138958, #107572, #5697, #155195, #55556, #105398, #189813, #39303, #56624, #173606, #122789, #40387, #188748, #106491, #90206, #135749, #7852, #73939, #103242, #201773, #119550, #185536, #169302, #206058, #86983, #57693, #70701, #136814, #191929, #125972, #144322, #28384, #178919, #59818, #175715, #127042, #190869, #27307, #143249, #110769, #95552, #158394, #109711, #160519, #12123, #142169, #195160, #193002, #61957, #78195, #210320, #128115, #9992, #45726, #124906, #145387, #30534, #76069, #42533, #63012, #209239, #93412, #60883, #194073, #111845, #177850, #29462, #44655, #46795, #13193, #112908, #161604, #174665, #176769, #43593, #208185, #96614, #79270, #141117, #159450, #58754, #211386, #129182, #108637, #8927, #11048, #75008, #207128, #26239, #92356, #77127, #94479, #213505, #146433, #15311, #81400, #100839, #184215, #65126, #183162, #163730, #66176, #17436, #149601, #147483, #35838, #199390, #200456, #68322, #131284, #52102, #48911, #99785, #14238, #182076, #1186, #197271, #34766, #49967, #109, #16375, #212447, #83520, #118231, #115031, #33708, #181030, #198327, #134453, #32647, #67250, #2246, #133385, #51036, #165851, #117159, #82454, #80332, #98724, #164783, #130233, #162668, #64091, #196226, #47868, #148543, #113979, #166924, #132321, #18518, #116086, #84596, #150684, #179976, #31597, #97673, #54237, #5444, #69386, #120375, #21690, #203653, #188492, #36902, #202585, #39053, #105138, #20639, #73676, #71523, #154939, #171178, #22769, #88885, #102984, #138700, #3317, #23847, #57433, #169042, #135494, #156005, #87802, #186350, #153875, #72600, #6523, #204718, #122531, #137634, #139775, #106234, #205802, #56368, #53165, #55303, #152798, #86728, #123594, #40124, #19587 ) ),
 .UNSPECIFIED., .F., .F., .T. ) 
 B_SPLINE_SURFACE_WITH_KNOTS ( ( 2, 2 ),
 ( 3, 2, 2, 2, 2, 2, 2, 2, 2, 2, 2, 2, 2, 2, 2, 2, 2, 2, 2, 2, 2, 2, 2, 2, 2, 2, 2, 2, 2, 2, 2, 2, 2, 2, 2, 2, 2, 2, 2, 2, 2, 2, 2, 2, 2, 2, 2, 2, 2, 2, 2, 2, 2, 2, 2, 2, 2, 2, 2, 2, 2, 2, 2, 2, 2, 2, 2, 2, 2, 2, 2, 2, 2, 2, 2, 2, 2, 2, 2, 2, 2, 2, 2, 2, 2, 2, 2, 2, 2, 2, 2, 2, 2, 2, 2, 2, 2, 2, 2, 2, 2, 2, 2, 2, 2, 2, 2, 2, 2, 2, 2, 2, 2, 2, 2, 2, 2, 2, 2, 2, 2, 2, 2, 2, 2, 2, 2, 2, 2, 2, 2, 2, 2, 2, 2, 2, 2, 2, 2, 2, 2, 2, 2, 2, 2, 2, 2, 2, 2, 2, 2, 2, 2, 2, 2, 2, 2, 2, 2, 2, 2, 2, 2, 2, 2, 2, 2, 2, 2, 2, 2, 2, 2, 2, 2, 2, 2, 2, 2, 2, 2, 2, 2, 2, 2, 2, 2, 2, 2, 2, 2, 2, 2, 2, 2, 2, 2, 2, 2, 2, 2, 2, 2, 2, 2, 2, 2, 2, 2, 2, 2, 2, 2, 2, 2, 2, 2, 2, 2, 2, 2, 2, 2, 2, 2, 2, 2, 2, 2, 2, 2, 2, 2, 2, 2, 2, 2, 2, 2, 2, 3 ),
 ( 0.000000000000000000, 1.000000000000000000 ),
 ( 0.000000000000000000, 0.004166666666666666609, 0.008333333333333333218, 0.01250000000000000069, 0.01666666666666666644, 0.02083333333333333218, 0.02500000000000000139, 0.02916666666666666713, 0.03333333333333333287, 0.03749999999999999861, 0.04166666666666666435, 0.04583333333333333010, 0.05000000000000000278, 0.05416666666666666852, 0.05833333333333333426, 0.06250000000000000000, 0.06666666666666666574, 0.07083333333333333148, 0.07499999999999999722, 0.07916666666666666297, 0.08333333333333332871, 0.08749999999999999445, 0.09166666666666666019, 0.09583333333333333981, 0.1000000000000000056, 0.1041666666666666713, 0.1083333333333333370, 0.1125000000000000028, 0.1166666666666666685, 0.1208333333333333343, 0.1250000000000000000, 0.1291666666666666796, 0.1333333333333333315, 0.1375000000000000111, 0.1416666666666666630, 0.1458333333333333426, 0.1499999999999999944, 0.1541666666666666741, 0.1583333333333333259, 0.1625000000000000056, 0.1666666666666666574, 0.1708333333333333370, 0.1749999999999999889, 0.1791666666666666685, 0.1833333333333333204, 0.1875000000000000000, 0.1916666666666666796, 0.1958333333333333315, 0.2000000000000000111, 0.2041666666666666630, 0.2083333333333333426, 0.2124999999999999944, 0.2166666666666666741, 0.2208333333333333259, 0.2250000000000000056, 0.2291666666666666574, 0.2333333333333333370, 0.2374999999999999889, 0.2416666666666666685, 0.2458333333333333204, 0.2500000000000000000, 0.2541666666666666519, 0.2583333333333333592, 0.2625000000000000111, 0.2666666666666666630, 0.2708333333333333148, 0.2750000000000000222, 0.2791666666666666741, 0.2833333333333333259, 0.2874999999999999778, 0.2916666666666666852, 0.2958333333333333370, 0.2999999999999999889, 0.3041666666666666408, 0.3083333333333333481, 0.3125000000000000000, 0.3166666666666666519, 0.3208333333333333592, 0.3250000000000000111, 0.3291666666666666630, 0.3333333333333333148, 0.3375000000000000222, 0.3416666666666666741, 0.3458333333333333259, 0.3499999999999999778, 0.3541666666666666852, 0.3583333333333333370, 0.3624999999999999889, 0.3666666666666666408, 0.3708333333333333481, 0.3750000000000000000, 0.3791666666666666519, 0.3833333333333333592, 0.3875000000000000111, 0.3916666666666666630, 0.3958333333333333148, 0.4000000000000000222, 0.4041666666666666741, 0.4083333333333333259, 0.4124999999999999778, 0.4166666666666666852, 0.4208333333333333370, 0.4249999999999999889, 0.4291666666666666408, 0.4333333333333333481, 0.4375000000000000000, 0.4416666666666666519, 0.4458333333333333592, 0.4500000000000000111, 0.4541666666666666630, 0.4583333333333333148, 0.4625000000000000222, 0.4666666666666666741, 0.4708333333333333259, 0.4749999999999999778, 0.4791666666666666852, 0.4833333333333333370, 0.4874999999999999889, 0.4916666666666666408, 0.4958333333333333481, 0.5000000000000000000, 0.5041666666666666519, 0.5083333333333333037, 0.5124999999999999556, 0.5166666666666667185, 0.5208333333333333703, 0.5250000000000000222, 0.5291666666666666741, 0.5333333333333333259, 0.5374999999999999778, 0.5416666666666666297, 0.5458333333333332815, 0.5500000000000000444, 0.5541666666666666963, 0.5583333333333333481, 0.5625000000000000000, 0.5666666666666666519, 0.5708333333333333037, 0.5749999999999999556, 0.5791666666666667185, 0.5833333333333333703, 0.5875000000000000222, 0.5916666666666666741, 0.5958333333333333259, 0.5999999999999999778, 0.6041666666666666297, 0.6083333333333332815, 0.6125000000000000444, 0.6166666666666666963, 0.6208333333333333481, 0.6250000000000000000, 0.6291666666666666519, 0.6333333333333333037, 0.6374999999999999556, 0.6416666666666667185, 0.6458333333333333703, 0.6500000000000000222, 0.6541666666666666741, 0.6583333333333333259, 0.6624999999999999778, 0.6666666666666666297, 0.6708333333333332815, 0.6750000000000000444, 0.6791666666666666963, 0.6833333333333333481, 0.6875000000000000000, 0.6916666666666666519, 0.6958333333333333037, 0.6999999999999999556, 0.7041666666666667185, 0.7083333333333333703, 0.7125000000000000222, 0.7166666666666666741, 0.7208333333333333259, 0.7249999999999999778, 0.7291666666666666297, 0.7333333333333332815, 0.7375000000000000444, 0.7416666666666666963, 0.7458333333333333481, 0.7500000000000000000, 0.7541666666666666519, 0.7583333333333333037, 0.7624999999999999556, 0.7666666666666667185, 0.7708333333333333703, 0.7750000000000000222, 0.7791666666666666741, 0.7833333333333333259, 0.7874999999999999778, 0.7916666666666666297, 0.7958333333333332815, 0.8000000000000000444, 0.8041666666666666963, 0.8083333333333333481, 0.8125000000000000000, 0.8166666666666666519, 0.8208333333333333037, 0.8249999999999999556, 0.8291666666666667185, 0.8333333333333333703, 0.8375000000000000222, 0.8416666666666666741, 0.8458333333333333259, 0.8499999999999999778, 0.8541666666666666297, 0.8583333333333332815, 0.8625000000000000444, 0.8666666666666666963, 0.8708333333333333481, 0.8750000000000000000, 0.8791666666666666519, 0.8833333333333333037, 0.8874999999999999556, 0.8916666666666667185, 0.8958333333333333703, 0.9000000000000000222, 0.9041666666666666741, 0.9083333333333333259, 0.9124999999999999778, 0.9166666666666666297, 0.9208333333333332815, 0.9250000000000000444, 0.9291666666666666963, 0.9333333333333333481, 0.9375000000000000000, 0.9416666666666666519, 0.9458333333333333037, 0.9499999999999999556, 0.9541666666666667185, 0.9583333333333333703, 0.9625000000000000222, 0.9666666666666666741, 0.9708333333333333259, 0.9749999999999999778, 0.9791666666666666297, 0.9833333333333332815, 0.9875000000000000444, 0.9916666666666666963, 0.9958333333333333481, 1.000000000000000000 ),
 .UNSPECIFIED. ) 
 GEOMETRIC_REPRESENTATION_ITEM ( )  RATIONAL_B_SPLINE_SURFACE ( (
 ( 1.000000000000000000, 0.8660254037844387076, 1.000000000000000000, 0.8660254037844387076, 1.000000000000000000, 0.8660254037844387076, 1.000000000000000000, 0.8660254037844387076, 1.000000000000000000, 0.8660254037844387076, 1.000000000000000000, 0.8660254037844387076, 1.000000000000000000, 0.8660254037844387076, 1.000000000000000000, 0.8660254037844387076, 1.000000000000000000, 0.8660254037844387076, 1.000000000000000000, 0.8660254037844387076, 1.000000000000000000, 0.8660254037844387076, 1.000000000000000000, 0.8660254037844387076, 1.000000000000000000, 0.8660254037844387076, 1.000000000000000000, 0.8660254037844387076, 1.000000000000000000, 0.8660254037844387076, 1.000000000000000000, 0.8660254037844387076, 1.000000000000000000, 0.8660254037844387076, 1.000000000000000000, 0.8660254037844387076, 1.000000000000000000, 0.8660254037844387076, 1.000000000000000000, 0.8660254037844387076, 1.000000000000000000, 0.8660254037844387076, 1.000000000000000000, 0.8660254037844387076, 1.000000000000000000, 0.8660254037844387076, 1.000000000000000000, 0.8660254037844387076, 1.000000000000000000, 0.8660254037844387076, 1.000000000000000000, 0.8660254037844387076, 1.000000000000000000, 0.8660254037844387076, 1.000000000000000000, 0.8660254037844387076, 1.000000000000000000, 0.8660254037844387076, 1.000000000000000000, 0.8660254037844387076, 1.000000000000000000, 0.8660254037844387076, 1.000000000000000000, 0.8660254037844387076, 1.000000000000000000, 0.8660254037844387076, 1.000000000000000000, 0.8660254037844387076, 1.000000000000000000, 0.8660254037844387076, 1.000000000000000000, 0.8660254037844387076, 1.000000000000000000, 0.8660254037844387076, 1.000000000000000000, 0.8660254037844387076, 1.000000000000000000, 0.8660254037844387076, 1.000000000000000000, 0.8660254037844387076, 1.000000000000000000, 0.8660254037844387076, 1.000000000000000000, 0.8660254037844387076, 1.000000000000000000, 0.8660254037844387076, 1.000000000000000000, 0.8660254037844387076, 1.000000000000000000, 0.8660254037844387076, 1.000000000000000000, 0.8660254037844387076, 1.000000000000000000, 0.8660254037844387076, 1.000000000000000000, 0.8660254037844387076, 1.000000000000000000, 0.8660254037844387076, 1.000000000000000000, 0.8660254037844387076, 1.000000000000000000, 0.8660254037844387076, 1.000000000000000000, 0.8660254037844387076, 1.000000000000000000, 0.8660254037844387076, 1.000000000000000000, 0.8660254037844387076, 1.000000000000000000, 0.8660254037844387076, 1.000000000000000000, 0.8660254037844387076, 1.000000000000000000, 0.8660254037844387076, 1.000000000000000000, 0.8660254037844387076, 1.000000000000000000, 0.8660254037844387076, 1.000000000000000000, 0.8660254037844387076, 1.000000000000000000, 0.8660254037844387076, 1.000000000000000000, 0.8660254037844387076, 1.000000000000000000, 0.8660254037844387076, 1.000000000000000000, 0.8660254037844387076, 1.000000000000000000, 0.8660254037844387076, 1.000000000000000000, 0.8660254037844387076, 1.000000000000000000, 0.8660254037844387076, 1.000000000000000000, 0.8660254037844387076, 1.000000000000000000, 0.8660254037844387076, 1.000000000000000000, 0.8660254037844387076, 1.000000000000000000, 0.8660254037844387076, 1.000000000000000000, 0.8660254037844387076, 1.000000000000000000, 0.8660254037844387076, 1.000000000000000000, 0.8660254037844387076, 1.000000000000000000, 0.8660254037844387076, 1.000000000000000000, 0.8660254037844387076, 1.000000000000000000, 0.8660254037844387076, 1.000000000000000000, 0.8660254037844387076, 1.000000000000000000, 0.8660254037844387076, 1.000000000000000000, 0.8660254037844387076, 1.000000000000000000, 0.8660254037844387076, 1.000000000000000000, 0.8660254037844387076, 1.000000000000000000, 0.8660254037844387076, 1.000000000000000000, 0.8660254037844387076, 1.000000000000000000, 0.8660254037844387076, 1.000000000000000000, 0.8660254037844387076, 1.000000000000000000, 0.8660254037844387076, 1.000000000000000000, 0.8660254037844387076, 1.000000000000000000, 0.8660254037844387076, 1.000000000000000000, 0.8660254037844387076, 1.000000000000000000, 0.8660254037844387076, 1.000000000000000000, 0.8660254037844387076, 1.000000000000000000, 0.8660254037844387076, 1.000000000000000000, 0.8660254037844387076, 1.000000000000000000, 0.8660254037844387076, 1.000000000000000000, 0.8660254037844387076, 1.000000000000000000, 0.8660254037844387076, 1.000000000000000000, 0.8660254037844387076, 1.000000000000000000, 0.8660254037844387076, 1.000000000000000000, 0.8660254037844387076, 1.000000000000000000, 0.8660254037844387076, 1.000000000000000000, 0.8660254037844387076, 1.000000000000000000, 0.8660254037844387076, 1.000000000000000000, 0.8660254037844387076, 1.000000000000000000, 0.8660254037844387076, 1.000000000000000000, 0.8660254037844387076, 1.000000000000000000, 0.8660254037844387076, 1.000000000000000000, 0.8660254037844387076, 1.000000000000000000, 0.8660254037844387076, 1.000000000000000000, 0.8660254037844387076, 1.000000000000000000, 0.8660254037844387076, 1.000000000000000000, 0.8660254037844387076, 1.000000000000000000, 0.8660254037844387076, 1.000000000000000000, 0.8660254037844387076, 1.000000000000000000, 0.8660254037844387076, 1.000000000000000000, 0.8660254037844387076, 1.000000000000000000, 0.8660254037844387076, 1.000000000000000000, 0.8660254037844387076, 1.000000000000000000, 0.8660254037844387076, 1.000000000000000000, 0.8660254037844387076, 1.000000000000000000, 0.8660254037844387076, 1.000000000000000000, 0.8660254037844387076, 1.000000000000000000, 0.8660254037844387076, 1.000000000000000000, 0.8660254037844387076, 1.000000000000000000, 0.8660254037844387076, 1.000000000000000000, 0.8660254037844387076, 1.000000000000000000, 0.8660254037844387076, 1.000000000000000000, 0.8660254037844387076, 1.000000000000000000, 0.8660254037844387076, 1.000000000000000000, 0.8660254037844387076, 1.000000000000000000, 0.8660254037844387076, 1.000000000000000000, 0.8660254037844387076, 1.000000000000000000, 0.8660254037844387076, 1.000000000000000000, 0.8660254037844387076, 1.000000000000000000, 0.8660254037844387076, 1.000000000000000000, 0.8660254037844387076, 1.000000000000000000, 0.8660254037844387076, 1.000000000000000000, 0.8660254037844387076, 1.000000000000000000, 0.8660254037844387076, 1.000000000000000000, 0.8660254037844387076, 1.000000000000000000, 0.8660254037844387076, 1.000000000000000000, 0.8660254037844387076, 1.000000000000000000, 0.8660254037844387076, 1.000000000000000000, 0.8660254037844387076, 1.000000000000000000, 0.8660254037844387076, 1.000000000000000000, 0.8660254037844387076, 1.000000000000000000, 0.8660254037844387076, 1.000000000000000000, 0.8660254037844387076, 1.000000000000000000, 0.8660254037844387076, 1.000000000000000000, 0.8660254037844387076, 1.000000000000000000, 0.8660254037844387076, 1.000000000000000000, 0.8660254037844387076, 1.000000000000000000, 0.8660254037844387076, 1.000000000000000000, 0.8660254037844387076, 1.000000000000000000, 0.8660254037844387076, 1.000000000000000000, 0.8660254037844387076, 1.000000000000000000, 0.8660254037844387076, 1.000000000000000000, 0.8660254037844387076, 1.000000000000000000, 0.8660254037844387076, 1.000000000000000000, 0.8660254037844387076, 1.000000000000000000, 0.8660254037844387076, 1.000000000000000000, 0.8660254037844387076, 1.000000000000000000, 0.8660254037844387076, 1.000000000000000000, 0.8660254037844387076, 1.000000000000000000, 0.8660254037844387076, 1.000000000000000000, 0.8660254037844387076, 1.000000000000000000, 0.8660254037844387076, 1.000000000000000000, 0.8660254037844387076, 1.000000000000000000, 0.8660254037844387076, 1.000000000000000000, 0.8660254037844387076, 1.000000000000000000, 0.8660254037844387076, 1.000000000000000000, 0.8660254037844387076, 1.000000000000000000, 0.8660254037844387076, 1.000000000000000000, 0.8660254037844387076, 1.000000000000000000, 0.8660254037844387076, 1.000000000000000000, 0.8660254037844387076, 1.000000000000000000, 0.8660254037844387076, 1.000000000000000000, 0.8660254037844387076, 1.000000000000000000, 0.8660254037844387076, 1.000000000000000000, 0.8660254037844387076, 1.000000000000000000, 0.8660254037844387076, 1.000000000000000000, 0.8660254037844387076, 1.000000000000000000, 0.8660254037844387076, 1.000000000000000000, 0.8660254037844387076, 1.000000000000000000, 0.8660254037844387076, 1.000000000000000000, 0.8660254037844387076, 1.000000000000000000, 0.8660254037844387076, 1.000000000000000000, 0.8660254037844387076, 1.000000000000000000, 0.8660254037844387076, 1.000000000000000000, 0.8660254037844387076, 1.000000000000000000, 0.8660254037844387076, 1.000000000000000000, 0.8660254037844387076, 1.000000000000000000, 0.8660254037844387076, 1.000000000000000000, 0.8660254037844387076, 1.000000000000000000, 0.8660254037844387076, 1.000000000000000000, 0.8660254037844387076, 1.000000000000000000, 0.8660254037844387076, 1.000000000000000000, 0.8660254037844387076, 1.000000000000000000, 0.8660254037844387076, 1.000000000000000000, 0.8660254037844387076, 1.000000000000000000, 0.8660254037844387076, 1.000000000000000000, 0.8660254037844387076, 1.000000000000000000, 0.8660254037844387076, 1.000000000000000000, 0.8660254037844387076, 1.000000000000000000, 0.8660254037844387076, 1.000000000000000000, 0.8660254037844387076, 1.000000000000000000, 0.8660254037844387076, 1.000000000000000000, 0.8660254037844387076, 1.000000000000000000, 0.8660254037844387076, 1.000000000000000000, 0.8660254037844387076, 1.000000000000000000, 0.8660254037844387076, 1.000000000000000000, 0.8660254037844387076, 1.000000000000000000, 0.8660254037844387076, 1.000000000000000000, 0.8660254037844387076, 1.000000000000000000, 0.8660254037844387076, 1.000000000000000000, 0.8660254037844387076, 1.000000000000000000, 0.8660254037844387076, 1.000000000000000000, 0.8660254037844387076, 1.000000000000000000, 0.8660254037844387076, 1.000000000000000000, 0.8660254037844387076, 1.000000000000000000, 0.8660254037844387076, 1.000000000000000000, 0.8660254037844387076, 1.000000000000000000, 0.8660254037844387076, 1.000000000000000000, 0.8660254037844387076, 1.000000000000000000, 0.8660254037844387076, 1.000000000000000000, 0.8660254037844387076, 1.000000000000000000, 0.8660254037844387076, 1.000000000000000000, 0.8660254037844387076, 1.000000000000000000, 0.8660254037844387076, 1.000000000000000000, 0.8660254037844387076, 1.000000000000000000, 0.8660254037844387076, 1.000000000000000000, 0.8660254037844387076, 1.000000000000000000, 0.8660254037844387076, 1.000000000000000000, 0.8660254037844387076, 1.000000000000000000, 0.8660254037844387076, 1.000000000000000000, 0.8660254037844387076, 1.000000000000000000, 0.8660254037844387076, 1.000000000000000000, 0.8660254037844387076, 1.000000000000000000, 0.8660254037844387076, 1.000000000000000000, 0.8660254037844387076, 1.000000000000000000),
 ( 1.000000000000000000, 0.8660254037844387076, 1.000000000000000000, 0.8660254037844387076, 1.000000000000000000, 0.8660254037844387076, 1.000000000000000000, 0.8660254037844387076, 1.000000000000000000, 0.8660254037844387076, 1.000000000000000000, 0.8660254037844387076, 1.000000000000000000, 0.8660254037844387076, 1.000000000000000000, 0.8660254037844387076, 1.000000000000000000, 0.8660254037844387076, 1.000000000000000000, 0.8660254037844387076, 1.000000000000000000, 0.8660254037844387076, 1.000000000000000000, 0.8660254037844387076, 1.000000000000000000, 0.8660254037844387076, 1.000000000000000000, 0.8660254037844387076, 1.000000000000000000, 0.8660254037844387076, 1.000000000000000000, 0.8660254037844387076, 1.000000000000000000, 0.8660254037844387076, 1.000000000000000000, 0.8660254037844387076, 1.000000000000000000, 0.8660254037844387076, 1.000000000000000000, 0.8660254037844387076, 1.000000000000000000, 0.8660254037844387076, 1.000000000000000000, 0.8660254037844387076, 1.000000000000000000, 0.8660254037844387076, 1.000000000000000000, 0.8660254037844387076, 1.000000000000000000, 0.8660254037844387076, 1.000000000000000000, 0.8660254037844387076, 1.000000000000000000, 0.8660254037844387076, 1.000000000000000000, 0.8660254037844387076, 1.000000000000000000, 0.8660254037844387076, 1.000000000000000000, 0.8660254037844387076, 1.000000000000000000, 0.8660254037844387076, 1.000000000000000000, 0.8660254037844387076, 1.000000000000000000, 0.8660254037844387076, 1.000000000000000000, 0.8660254037844387076, 1.000000000000000000, 0.8660254037844387076, 1.000000000000000000, 0.8660254037844387076, 1.000000000000000000, 0.8660254037844387076, 1.000000000000000000, 0.8660254037844387076, 1.000000000000000000, 0.8660254037844387076, 1.000000000000000000, 0.8660254037844387076, 1.000000000000000000, 0.8660254037844387076, 1.000000000000000000, 0.8660254037844387076, 1.000000000000000000, 0.8660254037844387076, 1.000000000000000000, 0.8660254037844387076, 1.000000000000000000, 0.8660254037844387076, 1.000000000000000000, 0.8660254037844387076, 1.000000000000000000, 0.8660254037844387076, 1.000000000000000000, 0.8660254037844387076, 1.000000000000000000, 0.8660254037844387076, 1.000000000000000000, 0.8660254037844387076, 1.000000000000000000, 0.8660254037844387076, 1.000000000000000000, 0.8660254037844387076, 1.000000000000000000, 0.8660254037844387076, 1.000000000000000000, 0.8660254037844387076, 1.000000000000000000, 0.8660254037844387076, 1.000000000000000000, 0.8660254037844387076, 1.000000000000000000, 0.8660254037844387076, 1.000000000000000000, 0.8660254037844387076, 1.000000000000000000, 0.8660254037844387076, 1.000000000000000000, 0.8660254037844387076, 1.000000000000000000, 0.8660254037844387076, 1.000000000000000000, 0.8660254037844387076, 1.000000000000000000, 0.8660254037844387076, 1.000000000000000000, 0.8660254037844387076, 1.000000000000000000, 0.8660254037844387076, 1.000000000000000000, 0.8660254037844387076, 1.000000000000000000, 0.8660254037844387076, 1.000000000000000000, 0.8660254037844387076, 1.000000000000000000, 0.8660254037844387076, 1.000000000000000000, 0.8660254037844387076, 1.000000000000000000, 0.8660254037844387076, 1.000000000000000000, 0.8660254037844387076, 1.000000000000000000, 0.8660254037844387076, 1.000000000000000000, 0.8660254037844387076, 1.000000000000000000, 0.8660254037844387076, 1.000000000000000000, 0.8660254037844387076, 1.000000000000000000, 0.8660254037844387076, 1.000000000000000000, 0.8660254037844387076, 1.000000000000000000, 0.8660254037844387076, 1.000000000000000000, 0.8660254037844387076, 1.000000000000000000, 0.8660254037844387076, 1.000000000000000000, 0.8660254037844387076, 1.000000000000000000, 0.8660254037844387076, 1.000000000000000000, 0.8660254037844387076, 1.000000000000000000, 0.8660254037844387076, 1.000000000000000000, 0.8660254037844387076, 1.000000000000000000, 0.8660254037844387076, 1.000000000000000000, 0.8660254037844387076, 1.000000000000000000, 0.8660254037844387076, 1.000000000000000000, 0.8660254037844387076, 1.000000000000000000, 0.8660254037844387076, 1.000000000000000000, 0.8660254037844387076, 1.000000000000000000, 0.8660254037844387076, 1.000000000000000000, 0.8660254037844387076, 1.000000000000000000, 0.8660254037844387076, 1.000000000000000000, 0.8660254037844387076, 1.000000000000000000, 0.8660254037844387076, 1.000000000000000000, 0.8660254037844387076, 1.000000000000000000, 0.8660254037844387076, 1.000000000000000000, 0.8660254037844387076, 1.000000000000000000, 0.8660254037844387076, 1.000000000000000000, 0.8660254037844387076, 1.000000000000000000, 0.8660254037844387076, 1.000000000000000000, 0.8660254037844387076, 1.000000000000000000, 0.8660254037844387076, 1.000000000000000000, 0.8660254037844387076, 1.000000000000000000, 0.8660254037844387076, 1.000000000000000000, 0.8660254037844387076, 1.000000000000000000, 0.8660254037844387076, 1.000000000000000000, 0.8660254037844387076, 1.000000000000000000, 0.8660254037844387076, 1.000000000000000000, 0.8660254037844387076, 1.000000000000000000, 0.8660254037844387076, 1.000000000000000000, 0.8660254037844387076, 1.000000000000000000, 0.8660254037844387076, 1.000000000000000000, 0.8660254037844387076, 1.000000000000000000, 0.8660254037844387076, 1.000000000000000000, 0.8660254037844387076, 1.000000000000000000, 0.8660254037844387076, 1.000000000000000000, 0.8660254037844387076, 1.000000000000000000, 0.8660254037844387076, 1.000000000000000000, 0.8660254037844387076, 1.000000000000000000, 0.8660254037844387076, 1.000000000000000000, 0.8660254037844387076, 1.000000000000000000, 0.8660254037844387076, 1.000000000000000000, 0.8660254037844387076, 1.000000000000000000, 0.8660254037844387076, 1.000000000000000000, 0.8660254037844387076, 1.000000000000000000, 0.8660254037844387076, 1.000000000000000000, 0.8660254037844387076, 1.000000000000000000, 0.8660254037844387076, 1.000000000000000000, 0.8660254037844387076, 1.000000000000000000, 0.8660254037844387076, 1.000000000000000000, 0.8660254037844387076, 1.000000000000000000, 0.8660254037844387076, 1.000000000000000000, 0.8660254037844387076, 1.000000000000000000, 0.8660254037844387076, 1.000000000000000000, 0.8660254037844387076, 1.000000000000000000, 0.8660254037844387076, 1.000000000000000000, 0.8660254037844387076, 1.000000000000000000, 0.8660254037844387076, 1.000000000000000000, 0.8660254037844387076, 1.000000000000000000, 0.8660254037844387076, 1.000000000000000000, 0.8660254037844387076, 1.000000000000000000, 0.8660254037844387076, 1.000000000000000000, 0.8660254037844387076, 1.000000000000000000, 0.8660254037844387076, 1.000000000000000000, 0.8660254037844387076, 1.000000000000000000, 0.8660254037844387076, 1.000000000000000000, 0.8660254037844387076, 1.000000000000000000, 0.8660254037844387076, 1.000000000000000000, 0.8660254037844387076, 1.000000000000000000, 0.8660254037844387076, 1.000000000000000000, 0.8660254037844387076, 1.000000000000000000, 0.8660254037844387076, 1.000000000000000000, 0.8660254037844387076, 1.000000000000000000, 0.8660254037844387076, 1.000000000000000000, 0.8660254037844387076, 1.000000000000000000, 0.8660254037844387076, 1.000000000000000000, 0.8660254037844387076, 1.000000000000000000, 0.8660254037844387076, 1.000000000000000000, 0.8660254037844387076, 1.000000000000000000, 0.8660254037844387076, 1.000000000000000000, 0.8660254037844387076, 1.000000000000000000, 0.8660254037844387076, 1.000000000000000000, 0.8660254037844387076, 1.000000000000000000, 0.8660254037844387076, 1.000000000000000000, 0.8660254037844387076, 1.000000000000000000, 0.8660254037844387076, 1.000000000000000000, 0.8660254037844387076, 1.000000000000000000, 0.8660254037844387076, 1.000000000000000000, 0.8660254037844387076, 1.000000000000000000, 0.8660254037844387076, 1.000000000000000000, 0.8660254037844387076, 1.000000000000000000, 0.8660254037844387076, 1.000000000000000000, 0.8660254037844387076, 1.000000000000000000, 0.8660254037844387076, 1.000000000000000000, 0.8660254037844387076, 1.000000000000000000, 0.8660254037844387076, 1.000000000000000000, 0.8660254037844387076, 1.000000000000000000, 0.8660254037844387076, 1.000000000000000000, 0.8660254037844387076, 1.000000000000000000, 0.8660254037844387076, 1.000000000000000000, 0.8660254037844387076, 1.000000000000000000, 0.8660254037844387076, 1.000000000000000000, 0.8660254037844387076, 1.000000000000000000, 0.8660254037844387076, 1.000000000000000000, 0.8660254037844387076, 1.000000000000000000, 0.8660254037844387076, 1.000000000000000000, 0.8660254037844387076, 1.000000000000000000, 0.8660254037844387076, 1.000000000000000000, 0.8660254037844387076, 1.000000000000000000, 0.8660254037844387076, 1.000000000000000000, 0.8660254037844387076, 1.000000000000000000, 0.8660254037844387076, 1.000000000000000000, 0.8660254037844387076, 1.000000000000000000, 0.8660254037844387076, 1.000000000000000000, 0.8660254037844387076, 1.000000000000000000, 0.8660254037844387076, 1.000000000000000000, 0.8660254037844387076, 1.000000000000000000, 0.8660254037844387076, 1.000000000000000000, 0.8660254037844387076, 1.000000000000000000, 0.8660254037844387076, 1.000000000000000000, 0.8660254037844387076, 1.000000000000000000, 0.8660254037844387076, 1.000000000000000000, 0.8660254037844387076, 1.000000000000000000, 0.8660254037844387076, 1.000000000000000000, 0.8660254037844387076, 1.000000000000000000, 0.8660254037844387076, 1.000000000000000000, 0.8660254037844387076, 1.000000000000000000, 0.8660254037844387076, 1.000000000000000000, 0.8660254037844387076, 1.000000000000000000, 0.8660254037844387076, 1.000000000000000000, 0.8660254037844387076, 1.000000000000000000, 0.8660254037844387076, 1.000000000000000000, 0.8660254037844387076, 1.000000000000000000, 0.8660254037844387076, 1.000000000000000000, 0.8660254037844387076, 1.000000000000000000, 0.8660254037844387076, 1.000000000000000000, 0.8660254037844387076, 1.000000000000000000, 0.8660254037844387076, 1.000000000000000000, 0.8660254037844387076, 1.000000000000000000, 0.8660254037844387076, 1.000000000000000000, 0.8660254037844387076, 1.000000000000000000, 0.8660254037844387076, 1.000000000000000000, 0.8660254037844387076, 1.000000000000000000, 0.8660254037844387076, 1.000000000000000000, 0.8660254037844387076, 1.000000000000000000, 0.8660254037844387076, 1.000000000000000000, 0.8660254037844387076, 1.000000000000000000, 0.8660254037844387076, 1.000000000000000000, 0.8660254037844387076, 1.000000000000000000, 0.8660254037844387076, 1.000000000000000000, 0.8660254037844387076, 1.000000000000000000, 0.8660254037844387076, 1.000000000000000000, 0.8660254037844387076, 1.000000000000000000, 0.8660254037844387076, 1.000000000000000000, 0.8660254037844387076, 1.000000000000000000, 0.8660254037844387076, 1.000000000000000000, 0.8660254037844387076, 1.000000000000000000) ) ) 
 REPRESENTATION_ITEM ( '' )  SURFACE ( )  );
#27733 = CARTESIAN_POINT ( 'NONE',  ( 7.910292558569346433, 11.31609285405122556, -1.199719254218446718 ) ) ;
#27734 = CARTESIAN_POINT ( 'NONE',  ( 5.125469573878929097, 0.2063957376101481500, -2.060066405364005426 ) ) ;
#27736 = CARTESIAN_POINT ( 'NONE',  ( 2.905317003618158367, 1.825515667692039878, 1.157497049167732550 ) ) ;
#27735 = CARTESIAN_POINT ( 'NONE',  ( -3.026510298046701575, 6.452477208712732448, 0.6266050759124314196 ) ) ;
#27737 = CARTESIAN_POINT ( 'NONE',  ( 4.599289333468261631, -0.5842463895667610041, 2.112197083089427885 ) ) ;
#27738 = EDGE_LOOP ( 'NONE', ( #82038, #130191, #36784, #207268 ) ) ;
#27739 = CARTESIAN_POINT ( 'NONE',  ( 10.01963921569910632, 11.64833282552586091, 1.199719254218450271 ) ) ;
#27740 = DIRECTION ( 'NONE',  ( -1.000000000000000000, 5.578564026256504688E-16, 0.000000000000000000 ) ) ;
#27741 = CARTESIAN_POINT ( 'NONE',  ( -5.583800452342470244, 15.44693297529254394, 10.58116637897097156 ) ) ;
#27742 = CARTESIAN_POINT ( 'NONE',  ( 3.088225128862704949, 6.824956093640315302, 0.7998128361456281477 ) ) ;
#27743 = CARTESIAN_POINT ( 'NONE',  ( -1.642778471875000035, -2.355208332855376341, -2.845375778867859751 ) ) ;
#27744 = CARTESIAN_POINT ( 'NONE',  ( -3.546339698426324460, 6.295090860542775779, -1.199719254218450271 ) ) ;
#27745 = CARTESIAN_POINT ( 'NONE',  ( 0.3521856818783953846, 0.1948384997633167970, -2.006960225185448810 ) ) ;
#27746 = CARTESIAN_POINT ( 'NONE',  ( -7.646435448427427062, 10.90429654226522693, 1.082531754730549967 ) ) ;
#27747 = CARTESIAN_POINT ( 'NONE',  ( 6.059568310664962709, 6.034194215389424798, 0.7998128361456352531 ) ) ;
#27748 = CARTESIAN_POINT ( 'NONE',  ( 5.735237735067806319, -0.04509738862551111033, -2.069921269439451539 ) ) ;
#27749 = CARTESIAN_POINT ( 'NONE',  ( 4.266181944680371707, 0.9094715277466745018, 1.698315803094905041 ) ) ;
#27750 = CARTESIAN_POINT ( 'NONE',  ( 6.591443028821331040, -0.4675721919094841250, 2.072835713318227135 ) ) ;
#27751 = CARTESIAN_POINT ( 'NONE',  ( -8.597841969360544567, 13.18256606422934674, 0.7998128361456341429 ) ) ;
#27752 = CARTESIAN_POINT ( 'NONE',  ( 6.647575389402066826, 6.649926130590872120, 1.040834085586084257E-14 ) ) ;
#27753 = CARTESIAN_POINT ( 'NONE',  ( 1.499999999999993117, 13.10416666666666963, 0.8660254037844408170 ) ) ;
#27754 = CARTESIAN_POINT ( 'NONE',  ( 5.067230186376567858, 1.711625542863755012, 0.9741009975822639833 ) ) ;
#27755 = CARTESIAN_POINT ( 'NONE',  ( 0.7619990552875830492, 1.083242598816274382, 1.904929396514772444 ) ) ;
#27756 = CARTESIAN_POINT ( 'NONE',  ( 3.914527900857078357, 1.289819402409349669, -1.292354223553587644 ) ) ;
#27757 = CARTESIAN_POINT ( 'NONE',  ( 5.831415467653547680, 8.857049574687536619, -1.082531754730548412 ) ) ;
#27758 = CARTESIAN_POINT ( 'NONE',  ( 4.514501963226220660, 4.369266499959774563, -0.7216878364870197293 ) ) ;
#27759 = CARTESIAN_POINT ( 'NONE',  ( -5.607179047703544583, 8.699403434699558346, 1.199719254218454489 ) ) ;
#27760 = CARTESIAN_POINT ( 'NONE',  ( 6.201928923608456046, 6.200281597156833691, 0.7998128361456352531 ) ) ;
#27761 = ORIENTED_EDGE ( 'NONE', *, *, #74029, .F. ) ;
#27763 = CARTESIAN_POINT ( 'NONE',  ( 4.974862723197266412, -1.455255168294814272, 1.391337642457886270 ) ) ;
#27762 = CARTESIAN_POINT ( 'NONE',  ( 2.454439063956286304, -1.602943312447857593, -0.9057913635923324769 ) ) ;
#27764 = CARTESIAN_POINT ( 'NONE',  ( 1.230279809073684172, -2.078304686880276808, -0.9817359432500573080 ) ) ;
#27765 = CARTESIAN_POINT ( 'NONE',  ( 5.559412779221331924, 1.601624451964112739, 1.132529127964493121 ) ) ;
#27766 = CARTESIAN_POINT ( 'NONE',  ( -6.742482464697739708, 6.760651051769146491, 0.7998128361456341429 ) ) ;
#27767 = CARTESIAN_POINT ( 'NONE',  ( 0.2333690889706925564, 0.2409277441041447754, -2.087868073146467829 ) ) ;
#27768 = CARTESIAN_POINT ( 'NONE',  ( -4.973143418114339021, 4.696422164088486895, 0.7998128361456341429 ) ) ;
#27769 = CARTESIAN_POINT ( 'NONE',  ( 0.1333692844072559280, 0.001398348041498076455, -2.053671342968105051 ) ) ;
#27770 = CARTESIAN_POINT ( 'NONE',  ( -3.447516199624892419, 7.244129009529488350, 0.7998128361456352531 ) ) ;
#27772 = CARTESIAN_POINT ( 'NONE',  ( 6.819227944281511355, -0.1297537616256147774, 1.740395163524804945 ) ) ;
#27771 = CARTESIAN_POINT ( 'NONE',  ( 0.9957797365991372107, -2.090933974770115444, 0.003689723154384760839 ) ) ;
#27773 = DIRECTION ( 'NONE',  ( 0.000000000000000000, 8.546850786086437571E-32, 1.000000000000000000 ) ) ;
#27774 = EDGE_LOOP ( 'NONE', ( #26392, #129913 ) ) ;
#27775 = CARTESIAN_POINT ( 'NONE',  ( 1.944474315927123387, -1.398120440366573680, -1.036317219087657504 ) ) ;
#27776 = CARTESIAN_POINT ( 'NONE',  ( 6.661133543015731462, 6.665743976473484267, -0.7998128361456281477 ) ) ;
#27778 = CARTESIAN_POINT ( 'NONE',  ( 1.571977147778452544, 8.681624870483057421, 2.500282472944442613 ) ) ;
#27777 = DIRECTION ( 'NONE',  ( 1.040834085586084257E-15, 1.000000000000000000, -4.622230424712076367E-32 ) ) ;
#27779 = CARTESIAN_POINT ( 'NONE',  ( 3.123388959964632949, -1.662097631915793183, 0.4608284732507839654 ) ) ;
#27780 = CARTESIAN_POINT ( 'NONE',  ( 3.210657068901449307, 1.982179491636561819, 0.9350799695589939731 ) ) ;
#27781 = CARTESIAN_POINT ( 'NONE',  ( 4.477303810882872881, 0.001702072213635372200, -2.207063162522747479 ) ) ;
#27782 = CARTESIAN_POINT ( 'NONE',  ( -9.812680342707254866, 4.108039100808300148, -6.337802944732694677 ) ) ;
#27784 = CARTESIAN_POINT ( 'NONE',  ( 2.588947950494639993, 2.104950400290429791, 0.5311738530254602741 ) ) ;
#27783 = B_SPLINE_CURVE_WITH_KNOTS ( 'NONE', 3,
 ( #46806, #84606, #130244, #14251, #165862, #133396, #17448, #150695, #83531, #1196 ),
 .UNSPECIFIED., .F., .F.,
 ( 4, 1, 1, 1, 1, 1, 1, 4 ),
 ( 0.000000000000000000, 0.09705918685507786137, 0.1907419858981972138, 0.2602182418918835838, 0.3625179829595637226, 0.5215049497019805802, 0.7338397267804015467, 1.000000000000000000 ),
 .UNSPECIFIED. ) ;
#27785 = CARTESIAN_POINT ( 'NONE',  ( 0.6096330727367264002, -1.817201089070449971, 0.1759225495863714350 ) ) ;
#27786 = CARTESIAN_POINT ( 'NONE',  ( 3.661412522060889074, 1.992289893316813609, -0.7171584230975246443 ) ) ;
#27787 = CARTESIAN_POINT ( 'NONE',  ( 6.639320575229256782, 2.986994467643698137, 2.250762793112503157 ) ) ;
#27788 = ORIENTED_EDGE ( 'NONE', *, *, #144165, .F. ) ;
#27790 = CARTESIAN_POINT ( 'NONE',  ( 0.6823417656249882723, 0.9885416670080832136, -1.181850606188749264 ) ) ;
#27789 = CARTESIAN_POINT ( 'NONE',  ( 4.212625126225740146, 2.095743129530680537, 0.9292526312315220194 ) ) ;
#27791 = FACE_OUTER_BOUND ( 'NONE', #209897, .T. ) ;
#27792 = CARTESIAN_POINT ( 'NONE',  ( 3.005103603723342953, 6.657704637652544832, -0.7998128361456291469 ) ) ;
#27793 = EDGE_CURVE ( 'NONE', #141010, #68973, #45732, .T. ) ;
#27794 = CARTESIAN_POINT ( 'NONE',  ( 5.672587799981195111, 0.8983335965149964464, 2.031727793752806210 ) ) ;
#27795 = CARTESIAN_POINT ( 'NONE',  ( -6.724481002698126098, 8.868313807946373473, -1.443375672974059665 ) ) ;
#27796 = CARTESIAN_POINT ( 'NONE',  ( 3.470524135418292300, 5.072030796119872953, -1.443375672974057666 ) ) ;
#27797 = CARTESIAN_POINT ( 'NONE',  ( -5.870317324592812191, 7.871789516823500144, -1.443375672974051449 ) ) ;
#27798 = CARTESIAN_POINT ( 'NONE',  ( 6.825078400183548055, 3.702925343214446663, 2.370119418288775925 ) ) ;
#27799 = ORIENTED_EDGE ( 'NONE', *, *, #159108, .F. ) ;
#27800 = CARTESIAN_POINT ( 'NONE',  ( 4.465470312728934132, -1.956561007648183192, -0.4872041746135646889 ) ) ;
#27802 = CARTESIAN_POINT ( 'NONE',  ( 2.623947407551871169, 2.023649216642096960, -0.3979924315659318923 ) ) ;
#27801 = CARTESIAN_POINT ( 'NONE',  ( 4.964256800898067645, 8.943383367689749619, 0.7998128361456462443 ) ) ;
#27803 = LINE ( 'NONE', #110192, #137156 ) ;
#27804 = CARTESIAN_POINT ( 'NONE',  ( 5.045042557616584489, 5.058506870073687267, 0.000000000000000000 ) ) ;
#27805 = CARTESIAN_POINT ( 'NONE',  ( 1.642778471875001811, -3.492708332855375630, 2.845375778867859751 ) ) ;
#27806 = CARTESIAN_POINT ( 'NONE',  ( 1.364683531249990311, 4.634375000341417916, 1.214306433183764966E-14 ) ) ;
#27807 = CARTESIAN_POINT ( 'NONE',  ( 5.560537033210596114, -1.979929515673630513, -0.9395970221138388867 ) ) ;
#27808 = CARTESIAN_POINT ( 'NONE',  ( 2.777970385693105726, 1.728001979019553325, -1.038993764437286416 ) ) ;
#27809 = CARTESIAN_POINT ( 'NONE',  ( 1.768857366986800184, 1.761637791510446860, -0.5354853023365884201 ) ) ;
#27810 = CARTESIAN_POINT ( 'NONE',  ( 6.446011968293428041, 9.607765498729298415, -1.199719254218440723 ) ) ;
#27811 = EDGE_CURVE ( 'NONE', #34393, #193316, #58954, .T. ) ;
#27812 = CARTESIAN_POINT ( 'NONE',  ( 6.475623784153278883, 1.746001614453606576, -0.5331787911772439825 ) ) ;
#27813 = CARTESIAN_POINT ( 'NONE',  ( -0.05159450770049476415, -2.057278634402651907, -1.025749021234131364 ) ) ;
#27814 = CARTESIAN_POINT ( 'NONE',  ( -6.204827856548512877, 10.39071626594860476, -0.7998128361456291469 ) ) ;
#27816 = CARTESIAN_POINT ( 'NONE',  ( -3.657667580636712934, 7.489305620709952649, -0.7998128361456481317 ) ) ;
#27815 = CARTESIAN_POINT ( 'NONE',  ( 6.016560025881092066, 1.524636124814653382, -1.671835012792993735 ) ) ;
#27817 = CARTESIAN_POINT ( 'NONE',  ( 2.420660912963272349, 1.375124471020009231, -1.595256772795665023 ) ) ;
#27818 = CARTESIAN_POINT ( 'NONE',  ( -6.099189001301292379, 8.209082816308541197, 1.599625672291263179 ) ) ;
#27819 = CARTESIAN_POINT ( 'NONE',  ( 7.832860060393120882, 10.16142270859057462, 1.599625672291281386 ) ) ;
#27820 = CARTESIAN_POINT ( 'NONE',  ( 6.414416072596830887, 8.576847732820027659, -1.443375672974078761 ) ) ;
#27821 = CARTESIAN_POINT ( 'NONE',  ( -6.530223543276495235, 10.77034456713125188, -0.7998128361456291469 ) ) ;
#27822 = DIRECTION ( 'NONE',  ( -5.578564026256490882E-16, -1.000000000000000000, -9.066213480720158442E-32 ) ) ;
#27823 = CARTESIAN_POINT ( 'NONE',  ( 6.426201622753093368, 10.44105962661321563, 1.040834085586084257E-14 ) ) ;
#27824 = CARTESIAN_POINT ( 'NONE',  ( 4.184706906298553797, 7.590773377710720915, -0.8858016571234141878 ) ) ;
#27825 = CARTESIAN_POINT ( 'NONE',  ( -8.351459436338030784, 11.72682452816096976, -1.082531754730543971 ) ) ;
#27827 = CARTESIAN_POINT ( 'NONE',  ( 3.059039825962418746, 0.5433887813283566626, 2.153793114424791710 ) ) ;
#27826 = CARTESIAN_POINT ( 'NONE',  ( 1.969135536805465492, -1.636093909763213228, 1.349083368969570262 ) ) ;
#27828 = DIRECTION ( 'NONE',  ( -0.6483454320283800199, 0.000000000000000000, 0.7613463080411786432 ) ) ;
#27830 = CARTESIAN_POINT ( 'NONE',  ( -6.394605727500880299, 7.489403432619674561, -1.199719254218452047 ) ) ;
#27829 = CIRCLE ( 'NONE', #139027, 2.025000000000006573 ) ;
#27831 = CARTESIAN_POINT ( 'NONE',  ( 6.173040012923759257, 6.096301524699504704, -0.7998128361456281477 ) ) ;
#27832 = CARTESIAN_POINT ( 'NONE',  ( 4.369553226407375313, -0.3375162941181614751, 1.932460123137308861 ) ) ;
#27833 = CARTESIAN_POINT ( 'NONE',  ( 8.106885785967500979, 11.54545161934907682, 1.199719254218460707 ) ) ;
#27834 = CARTESIAN_POINT ( 'NONE',  ( -5.443780329924999606, 6.294985656096041993, 1.034245658874383578 ) ) ;
#27835 = CARTESIAN_POINT ( 'NONE',  ( 4.356247428692526569, 3.976710176429713250, 0.7998128361456341429 ) ) ;
#27836 = CARTESIAN_POINT ( 'NONE',  ( -0.6823417656250246877, 0.3010416670080895418, 1.181850606188755259 ) ) ;
#27837 = CARTESIAN_POINT ( 'NONE',  ( -3.675669043080673770, 7.302381293653823491, 0.000000000000000000 ) ) ;
#27839 = ORIENTED_EDGE ( 'NONE', *, *, #61445, .T. ) ;
#27838 = CARTESIAN_POINT ( 'NONE',  ( -5.572037945536512105, 9.444535336527177805, 0.000000000000000000 ) ) ;
#27840 = CARTESIAN_POINT ( 'NONE',  ( 3.129257641292593650, 1.918792544363761454, 0.9031103230835100248 ) ) ;
#27841 = CARTESIAN_POINT ( 'NONE',  ( -3.637330350216213759, 7.465578851886037093, -0.7998128361456481317 ) ) ;
#27842 = CARTESIAN_POINT ( 'NONE',  ( 3.959979445722985325, 2.145676688911036578, -0.2621329562078680842 ) ) ;
#27843 = CARTESIAN_POINT ( 'NONE',  ( 3.509164994824386596, -1.813400730843343966, 0.3181347684400454012 ) ) ;
#27844 = CARTESIAN_POINT ( 'NONE',  ( -4.638859928512265363, 6.918491158249495676, 1.209939204767721987 ) ) ;
#27845 = CARTESIAN_POINT ( 'NONE',  ( -0.6823417656250246877, 0.6135416670080897639, 1.181850606188755259 ) ) ;
#27846 = CARTESIAN_POINT ( 'NONE',  ( 5.577983363897286218, -1.699187140184825751, -0.3753857801653339710 ) ) ;
#27847 = CYLINDRICAL_SURFACE ( 'NONE', #212136, 0.08000000000000020983 ) ;
#27848 = CARTESIAN_POINT ( 'NONE',  ( 2.901081683644312736, 6.328419697652925002, 0.7216878364870338292 ) ) ;
#27849 = CARTESIAN_POINT ( 'NONE',  ( 11.39332173424661754, 7.468513200851135458, 3.792645573777906343 ) ) ;
#27850 = VECTOR ( 'NONE', #128531, 1000.000000000000114 ) ;
#27851 = CARTESIAN_POINT ( 'NONE',  ( 3.415052781332720055, 1.953485055394106107, 0.9259690932504063277 ) ) ;
#27852 = CARTESIAN_POINT ( 'NONE',  ( 5.448592227559037049, 1.351948914259465173, 1.495821383734573073 ) ) ;
#27853 = CARTESIAN_POINT ( 'NONE',  ( -7.578644679914719795, 9.864838098032418401, 1.443375672974090751 ) ) ;
#27854 = CARTESIAN_POINT ( 'NONE',  ( 2.272554088390315030, -1.330374092946192688, 1.703740541667747133 ) ) ;
#27855 = CARTESIAN_POINT ( 'NONE',  ( 3.866447834861338695, -1.326295688514609550, 1.458626262776492544 ) ) ;
#27856 = CARTESIAN_POINT ( 'NONE',  ( -0.1114211809780316365, -0.4883405756051837354, -2.144353428667714390 ) ) ;
#27857 = CARTESIAN_POINT ( 'NONE',  ( 4.212401414637350072, 1.776917926058638963, 0.7840673734914437309 ) ) ;
#27860 = ORIENTED_EDGE ( 'NONE', *, *, #156157, .T. ) ;
#27859 = CARTESIAN_POINT ( 'NONE',  ( 8.081892667527538876, -5.166862915010159263, -7.462104991928523390 ) ) ;
#27858 = CARTESIAN_POINT ( 'NONE',  ( -7.985389288324692636, 11.29974268881207067, -1.082531754730543083 ) ) ;
#27861 = CARTESIAN_POINT ( 'NONE',  ( -7.618755976236585958, 7.853246491889623648, 0.000000000000000000 ) ) ;
#27862 = CARTESIAN_POINT ( 'NONE',  ( 8.283668668269706714, 8.766627655843896250, 1.040834085586084257E-14 ) ) ;
#27864 = VERTEX_POINT ( 'NONE', #195557 ) ;
#27863 = CARTESIAN_POINT ( 'NONE',  ( -5.490125858891038213, 5.369844688319787451, -0.7998128361456362523 ) ) ;
#27865 = CARTESIAN_POINT ( 'NONE',  ( -8.148087131688692253, 10.52918762510205042, -1.443375672974058777 ) ) ;
#27866 = CARTESIAN_POINT ( 'NONE',  ( 1.782535857997105566, -1.180187651135233384, 1.864495428577646274 ) ) ;
#27868 = ADVANCED_FACE ( 'NONE', ( #95944 ), #13588, .F. ) ;
#27867 = CARTESIAN_POINT ( 'NONE',  ( -3.285556943749998737, -0.7802083328553744979, 1.896917185911908499 ) ) ;
#27869 = CARTESIAN_POINT ( 'NONE',  ( 6.702011072381410806, 0.7537920952922130269, -1.811353739714548272 ) ) ;
#27870 = CARTESIAN_POINT ( 'NONE',  ( -1.364683531250010295, 4.842708333674756283, 0.7879004041258379498 ) ) ;
#27871 = CARTESIAN_POINT ( 'NONE',  ( -1.201851678989727383E-14, 3.743750000682817269, 1.732050807568877637 ) ) ;
#27872 = CARTESIAN_POINT ( 'NONE',  ( 5.302928268938337020, 6.565392180301311775, -1.356678214699511775 ) ) ;
#27874 = CARTESIAN_POINT ( 'NONE',  ( -4.009193028827814587, 7.297902834095492786, -0.7581239365674132813 ) ) ;
#27873 = CARTESIAN_POINT ( 'NONE',  ( 6.007671464186845611, 6.181573927739023588, 0.7216878364870273899 ) ) ;
#27875 = CARTESIAN_POINT ( 'NONE',  ( 5.753808258465379133, 0.7501079416377672837, 1.681592913607635964 ) ) ;
#27876 = ORIENTED_EDGE ( 'NONE', *, *, #97341, .T. ) ;
#27877 = CARTESIAN_POINT ( 'NONE',  ( 0.6801582343749952297, -0.9427083329919122567, -1.178068619123855409 ) ) ;
#27878 = CARTESIAN_POINT ( 'NONE',  ( -8.843996274815957293, 9.212417163573759282, 1.040834085586084257E-14 ) ) ;
#27879 = DIRECTION ( 'NONE',  ( 0.000000000000000000, 8.546850786086437571E-32, 1.000000000000000000 ) ) ;
#27880 = CARTESIAN_POINT ( 'NONE',  ( 6.240501835383900797, 1.219778281852833546, -1.734492557903525523 ) ) ;
#27881 = CARTESIAN_POINT ( 'NONE',  ( 0.000000000000000000, 13.49999999999999822, -1.500000000000000222 ) ) ;
#27882 = CARTESIAN_POINT ( 'NONE',  ( 5.847644326195776010, 5.716673223516856694, -0.7998128361456281477 ) ) ;
#27883 = CARTESIAN_POINT ( 'NONE',  ( 0.1454761644432709389, -1.592655978506152703, -1.307672486379028332 ) ) ;
#27886 = CARTESIAN_POINT ( 'NONE',  ( 4.089279031174639201, -0.7008038172400687937, 1.702867937621636463 ) ) ;
#27885 = CARTESIAN_POINT ( 'NONE',  ( 2.224856516622634395, -1.700045390792026989, -0.7576570785256631080 ) ) ;
#27884 = CARTESIAN_POINT ( 'NONE',  ( 3.673896439623286714, 4.156855427197417185, -0.9999999999999940048 ) ) ;
#27887 = CARTESIAN_POINT ( 'NONE',  ( 5.960781091502512119, 10.10599504006161986, 0.7998128361456462443 ) ) ;
#27888 = CARTESIAN_POINT ( 'NONE',  ( -9.608223705539561621, 15.11771569533321724, -7.189021993664028720 ) ) ;
#27889 = B_SPLINE_CURVE_WITH_KNOTS ( 'NONE', 3,
 ( #111170, #15708, #78591, #194478, #30935, #46121 ),
 .UNSPECIFIED., .F., .F.,
 ( 4, 2, 4 ),
 ( 0.000000000000000000, 0.0003346294579448533951, 0.0006692589158897067902 ),
 .UNSPECIFIED. ) ;
#27890 = AXIS2_PLACEMENT_3D ( 'NONE', #204407, #41962, #88573 ) ;
#27891 = CARTESIAN_POINT ( 'NONE',  ( -6.903036488013351679, 8.082572653217566128, -1.199719254218452047 ) ) ;
#27893 = ORIENTED_EDGE ( 'NONE', *, *, #198557, .F. ) ;
#27892 = CARTESIAN_POINT ( 'NONE',  ( -10.67552548858665418, -7.034525073436785902, -2.052149754785371264E-12 ) ) ;
#27894 = CARTESIAN_POINT ( 'NONE',  ( 4.723365791888975096, -0.1103408873950258995, 2.204240794804641190 ) ) ;
#27895 = CARTESIAN_POINT ( 'NONE',  ( 6.555986116969920730, 2.257040928323080564, -0.1566935481548906162 ) ) ;
#27896 = CARTESIAN_POINT ( 'NONE',  ( -5.910991785878170646, 7.919243054989755670, -1.443375672974059665 ) ) ;
#27897 = CARTESIAN_POINT ( 'NONE',  ( 5.502179438505619302, -0.8068474266363240277, 1.622048611428918319 ) ) ;
#27898 = CARTESIAN_POINT ( 'NONE',  ( 6.421099303836709460, -1.707838190419972424, 0.8681067396549295712 ) ) ;
#27899 = LINE ( 'NONE', #127629, #57661 ) ;
#27900 = CARTESIAN_POINT ( 'NONE',  ( 5.629731426258720361, -1.187751674602673058, -1.445209747047627946 ) ) ;
#27901 = CARTESIAN_POINT ( 'NONE',  ( 5.162724115531082347, 0.5589384127702141658, 1.828758346017298697 ) ) ;
#27902 = CYLINDRICAL_SURFACE ( 'NONE', #116300, 1.250000000000000000 ) ;
#27903 = CARTESIAN_POINT ( 'NONE',  ( 0.8834254411415434216, 1.253375741028007084, 1.388844808110502038 ) ) ;
#27904 = CARTESIAN_POINT ( 'NONE',  ( 0.7785302072789467287, -0.4946362931835950327, -1.954778448132548752 ) ) ;
#27906 = CARTESIAN_POINT ( 'NONE',  ( 4.072956574305106159, -1.964985935830084740, -0.7583447493727160094 ) ) ;
#27905 = CARTESIAN_POINT ( 'NONE',  ( -8.469039510030723861, 13.03229652834454733, 1.040834085586084257E-14 ) ) ;
#27907 = CARTESIAN_POINT ( 'NONE',  ( 9.908311333488716954, 10.45411806535867782, 0.7998128361456462443 ) ) ;
#27909 = CARTESIAN_POINT ( 'NONE',  ( -9.528683032306089373, 10.01121838064558744, 0.7998128361456462443 ) ) ;
#27908 = CARTESIAN_POINT ( 'NONE',  ( 1.499999999999989120, 0.2750000000000182854, 0.000000000000000000 ) ) ;
#27910 = DIRECTION ( 'NONE',  ( -0.000000000000000000, -1.000000000000000000, -0.000000000000000000 ) ) ;
#27912 = EDGE_CURVE ( 'NONE', #194519, #25559, #27889, .T. ) ;
#27911 = CARTESIAN_POINT ( 'NONE',  ( 3.006122514718052585, -0.8146449015280079475, 1.848388696978587875 ) ) ;
#27913 = CARTESIAN_POINT ( 'NONE',  ( 1.364683531249988535, 4.113541667008088432, 0.7879004041258500513 ) ) ;
#27914 = CARTESIAN_POINT ( 'NONE',  ( 4.220665892555866883, 3.818531717603609987, -0.7998128361456211532 ) ) ;
#27915 = CARTESIAN_POINT ( 'NONE',  ( 4.692742333269261934, -0.4685372120167423660, -2.110058259655919422 ) ) ;
#27916 = CARTESIAN_POINT ( 'NONE',  ( 11.21996551234715866, 1.000000000000000888, -3.949207502427110938 ) ) ;
#27917 = CARTESIAN_POINT ( 'NONE',  ( -1.500000000000011324, 4.879166666666690411, -0.8660254037844313801 ) ) ;
#27919 = CARTESIAN_POINT ( 'NONE',  ( -9.578206935421272661, -9.746166700192988586, 0.1671882239536542636 ) ) ;
#27918 = CARTESIAN_POINT ( 'NONE',  ( 5.820193082016415609, 10.01225203898631655, 0.000000000000000000 ) ) ;
#27920 =( BOUNDED_CURVE ( )  B_SPLINE_CURVE ( 3, ( #197847, #149104, #49479, #115599 ),
 .UNSPECIFIED., .F., .T. ) 
 B_SPLINE_CURVE_WITH_KNOTS ( ( 4, 4 ),
 ( 0.4999999999999984457, 1.000000000000000000 ),
 .UNSPECIFIED. ) 
 CURVE ( )  GEOMETRIC_REPRESENTATION_ITEM ( )  RATIONAL_B_SPLINE_CURVE ( ( 1.000000000000001998, 0.3333333333333333703, 0.3333333333333313164, 1.000000000000000000 ) ) 
 REPRESENTATION_ITEM ( '' )  );
#27921 = CARTESIAN_POINT ( 'NONE',  ( 6.900736999231407154, 10.99468423250458038, -0.7216878364870267237 ) ) ;
#27923 = CARTESIAN_POINT ( 'NONE',  ( 9.176494415247189451, 14.33413921510887334, -7.733462363332296086 ) ) ;
#27922 = CARTESIAN_POINT ( 'NONE',  ( 1.188188303608740615, -1.377055334905618933, -1.678633986682298573 ) ) ;
#27924 = CARTESIAN_POINT ( 'NONE',  ( -6.155038550924159857, 8.203964280876741455, 1.443375672974078761 ) ) ;
#27925 = EDGE_CURVE ( 'NONE', #66068, #30840, #127444, .T. ) ;
#27926 = CARTESIAN_POINT ( 'NONE',  ( -0.6823417656250003738, 2.217708333674753174, -1.181850606188749264 ) ) ;
#27927 = CARTESIAN_POINT ( 'NONE',  ( 1.734175692058033347, 2.168326105380265378, 0.3173973903456903112 ) ) ;
#27928 = CARTESIAN_POINT ( 'NONE',  ( 6.883263157960366030, 0.5727201817382967519, 2.105997115537924902 ) ) ;
#27929 = CARTESIAN_POINT ( 'NONE',  ( 2.764839853141934256, -1.560785778453818828, 1.638175023747280523 ) ) ;
#27930 = CARTESIAN_POINT ( 'NONE',  ( -7.854251061018346469, 8.057714414143200443, -0.7998128361456291469 ) ) ;
#27931 = CARTESIAN_POINT ( 'NONE',  ( 4.680875185974167074, 1.673856063443099895, -1.124242729735332347 ) ) ;
#27932 = CARTESIAN_POINT ( 'NONE',  ( 1.364683531249990311, 4.196875000341417028, 1.214306433183764966E-14 ) ) ;
#27933 = CARTESIAN_POINT ( 'NONE',  ( 5.067666882003905471, 7.850148838107081417, 1.122879199148843377 ) ) ;
#27934 = CARTESIAN_POINT ( 'NONE',  ( -6.009258394948636914E-15, 12.68749999999999645, -1.732050807568875195 ) ) ;
#27935 = CARTESIAN_POINT ( 'NONE',  ( 5.383996398402570271, 9.295429874862735531, 0.000000000000000000 ) ) ;
#27936 = CARTESIAN_POINT ( 'NONE',  ( 4.323360031453548302, -1.693909316728856806, 0.5125324126216290743 ) ) ;
#27937 = CARTESIAN_POINT ( 'NONE',  ( 8.934986926605834157, 10.38290515491702770, -1.199719254218446718 ) ) ;
#27938 = CARTESIAN_POINT ( 'NONE',  ( 0.3761801408644695477, 1.212865950663596371, 1.721436218156185305 ) ) ;
#27940 = CARTESIAN_POINT ( 'NONE',  ( 1.499999999999987121, 0.7541666666666868579, 0.8660254037844524744 ) ) ;
#27939 = CARTESIAN_POINT ( 'NONE',  ( -1.364683531250000748, 9.109375000341396245, 0.000000000000000000 ) ) ;
#27941 = CARTESIAN_POINT ( 'NONE',  ( -5.483346782084204563, 5.361935765378481378, 0.000000000000000000 ) ) ;
#27942 = CARTESIAN_POINT ( 'NONE',  ( 5.888296041240274725, -0.7283935311428509918, -1.880430420734761965 ) ) ;
#27943 = EDGE_LOOP ( 'NONE', ( #92721, #122147, #75961, #69505 ) ) ;
#27944 = CARTESIAN_POINT ( 'NONE',  ( 9.935427640716063991, 10.48575375712389679, -0.7998128361456281477 ) ) ;
#27945 = CARTESIAN_POINT ( 'NONE',  ( 3.924554409752772699, 1.776107677202539925, 0.5873546117282566481 ) ) ;
#27946 = CARTESIAN_POINT ( 'NONE',  ( 4.838769763947080804, -2.006773940031422399, -0.5081810985937407210 ) ) ;
#27948 = EDGE_CURVE ( 'NONE', #169987, #179933, #149191, .T. ) ;
#27947 = AXIS2_PLACEMENT_3D ( 'NONE', #160470, #45674, #112854 ) ;
#27949 = CARTESIAN_POINT ( 'NONE',  ( -6.590672069574513792, 6.861741300691274859, 0.000000000000000000 ) ) ;
#27950 = SURFACE_SIDE_STYLE ('',( #123419 ) ) ;
#27951 = CARTESIAN_POINT ( 'NONE',  ( 7.065770611016287006, 11.39514947949436774, 1.040834085586084257E-14 ) ) ;
#27952 = CARTESIAN_POINT ( 'NONE',  ( -9.829825065107822724, 11.42688298316931572, 1.199719254218462483 ) ) ;
#27953 = CARTESIAN_POINT ( 'NONE',  ( 8.154303043976348420, 8.478051404252736845, 0.7998128361456281477 ) ) ;
#27954 = CARTESIAN_POINT ( 'NONE',  ( -4.698419658905671703, 6.826623453404498498, -1.249972656429306772 ) ) ;
#27955 = CARTESIAN_POINT ( 'NONE',  ( -1.364683531249997417, 5.821875000341418804, 1.214306433183764966E-14 ) ) ;
#27956 = CARTESIAN_POINT ( 'NONE',  ( 3.596105239937871456, 0.8843387906064968940, -1.751336483779348585 ) ) ;
#27957 = CARTESIAN_POINT ( 'NONE',  ( 0.9485920322965734064, 1.351945250224910744, 1.495824703658617638 ) ) ;
#27958 = DIRECTION ( 'NONE',  ( 0.000000000000000000, 0.000000000000000000, 1.000000000000000000 ) ) ;
#27960 = CARTESIAN_POINT ( 'NONE',  ( 6.639320575229280763, 7.629137130509070275, 2.496737603865983424 ) ) ;
#27959 = CARTESIAN_POINT ( 'NONE',  ( 7.964525173024008531, 11.37936423758166526, 1.199719254218460707 ) ) ;
#27961 = CARTESIAN_POINT ( 'NONE',  ( 1.352582913587907942, -1.478046865151939615, 1.146363905606573086 ) ) ;
#27962 = CARTESIAN_POINT ( 'NONE',  ( 1.364683531249988535, 3.613541667008086211, 0.7879004041258500513 ) ) ;
#27963 = CARTESIAN_POINT ( 'NONE',  ( 2.935794159824364868, -1.939102465223912830, 0.5408614042671439082 ) ) ;
#27965 = CARTESIAN_POINT ( 'NONE',  ( 2.337658655405081110, 0.5614262474852428353, -2.041391482465891194 ) ) ;
#27964 = CARTESIAN_POINT ( 'NONE',  ( -5.260200412422196159, 9.080724881227137502, -0.7216878364870207285 ) ) ;
#27966 = CARTESIAN_POINT ( 'NONE',  ( -5.823017895876262173, 7.308274721394978357, -1.333157625313810879 ) ) ;
#27967 = CARTESIAN_POINT ( 'NONE',  ( 4.334477209444560053, -1.194628513295314942, 1.690740121169509447 ) ) ;
#27968 = CARTESIAN_POINT ( 'NONE',  ( 7.343676480457483002, 8.596652644402405841, -1.199719254218452047 ) ) ;
#27970 = CARTESIAN_POINT ( 'NONE',  ( -0.5445930744354052777, 3.250057683544617326, 0.3999999999999455103 ) ) ;
#27969 = CARTESIAN_POINT ( 'NONE',  ( 0.4508687890585044711, -1.768401812538191287, -1.115020903081758608 ) ) ;
#27972 = ORIENTED_EDGE ( 'NONE', *, *, #202320, .F. ) ;
#27971 = CARTESIAN_POINT ( 'NONE',  ( 4.788025880137685597, -0.8597811773201522456, 1.610451283527076116 ) ) ;
#27973 = CARTESIAN_POINT ( 'NONE',  ( 7.564559641420864899, 10.91273778404466199, -1.199719254218446718 ) ) ;
#27974 = CARTESIAN_POINT ( 'NONE',  ( 4.856179778084614540, 5.010200168423447842, 0.6077543439236311462 ) ) ;
#27975 = CARTESIAN_POINT ( 'NONE',  ( 12.13020669054560408, 8.043700598764450760, -3.170917236059372257 ) ) ;
#27976 = VECTOR ( 'NONE', #131648, 1000.000000000000000 ) ;
#27977 = CARTESIAN_POINT ( 'NONE',  ( 6.001041448284401447, 1.807427358944500684, -1.265864663738118345 ) ) ;
#27978 = CARTESIAN_POINT ( 'NONE',  ( -1.364683531250014514, 11.40104166700806410, -0.7879004041258335089 ) ) ;
#27979 = CARTESIAN_POINT ( 'NONE',  ( 5.496708366351358066, -1.866603419165157041, -0.4147590543357379533 ) ) ;
#27980 = CARTESIAN_POINT ( 'NONE',  ( -7.323375529675950624, 11.69568855126397011, -0.7998128361456291469 ) ) ;
#27981 = CARTESIAN_POINT ( 'NONE',  ( 7.494959990256193194, 7.638541498254023843, -0.7998128361456281477 ) ) ;
#27982 = CARTESIAN_POINT ( 'NONE',  ( -11.89839339040395316, 11.32877468403921561, -1.560885614203537219 ) ) ;
#27983 = CARTESIAN_POINT ( 'NONE',  ( -3.895996091634230218, 7.334980739573080832, 0.5863762202383783206 ) ) ;
#27984 = CARTESIAN_POINT ( 'NONE',  ( 4.467575310902914154, 5.170924936596891008, 1.199719254218464037 ) ) ;
#27985 = ORIENTED_EDGE ( 'NONE', *, *, #167881, .T. ) ;
#27986 = AXIS2_PLACEMENT_3D ( 'NONE', #167124, #306, #69583 ) ;
#27987 = CARTESIAN_POINT ( 'NONE',  ( -6.831329296439251131, 9.063246493969506545, -1.599625672291271394 ) ) ;
#27988 = CARTESIAN_POINT ( 'NONE',  ( 0.07680821025393690105, 0.005952109439256307241, -1.810863387344714193 ) ) ;
#27989 = CARTESIAN_POINT ( 'NONE',  ( 5.345657705538078730, 9.458627433094950021, 0.7998128361456331437 ) ) ;
#27990 = CARTESIAN_POINT ( 'NONE',  ( -0.4000000000000131783, 3.372708439410149417, -0.5000000000000160982 ) ) ;
#27991 = CARTESIAN_POINT ( 'NONE',  ( -5.631831469557842418, 7.372220891417233801, 1.235678285582973546 ) ) ;
#27992 = CARTESIAN_POINT ( 'NONE',  ( -5.260200412422200600, 8.120355666925794580, -1.082531754730544860 ) ) ;
#27993 = CARTESIAN_POINT ( 'NONE',  ( 4.684505768721569652, 5.424010470718658716, -1.199719254218452047 ) ) ;
#27994 = CARTESIAN_POINT ( 'NONE',  ( 2.852355409199380798, -1.963852837454314271, -0.1495663577412101042 ) ) ;
#27995 = CARTESIAN_POINT ( 'NONE',  ( 3.128529964930275131, 0.4926631579876327716, 1.955168413974050834 ) ) ;
#27996 = CARTESIAN_POINT ( 'NONE',  ( -7.019370843573183194, 9.212351955633947043, 1.599625672291283607 ) ) ;
#27997 = CARTESIAN_POINT ( 'NONE',  ( 5.285699784481295183, 7.260012063351913625, 1.599625672291268286 ) ) ;
#27998 = CARTESIAN_POINT ( 'NONE',  ( 6.827182134110199030, -0.004087946457608306570, 2.088967824442849341 ) ) ;
#27999 = CARTESIAN_POINT ( 'NONE',  ( 3.170069416559752273, -1.305109287949431929, 1.760291797049506446 ) ) ;
#28000 = CYLINDRICAL_SURFACE ( 'NONE', #71035, 0.3999999999999996891 ) ;
#28001 = CARTESIAN_POINT ( 'NONE',  ( 2.080962409574789174, -0.09239518442967499523, -1.924287757472051164 ) ) ;
#28002 = CARTESIAN_POINT ( 'NONE',  ( -8.670602931139386627, 10.07445716020612103, 1.199719254218462483 ) ) ;
#28003 =( NAMED_UNIT ( * ) SI_UNIT ( $, .STERADIAN. ) SOLID_ANGLE_UNIT ( ) );
#28004 = CARTESIAN_POINT ( 'NONE',  ( 0.2329586101569527945, 4.095490909754247788, -2.400670182941808672 ) ) ;
#28005 = CARTESIAN_POINT ( 'NONE',  ( 2.943528747942701695, 6.448217615992859919, 0.000000000000000000 ) ) ;
#28006 = CARTESIAN_POINT ( 'NONE',  ( 7.796102023057898123, 9.054206100777749455, -1.199719254218441611 ) ) ;
#28007 = CARTESIAN_POINT ( 'NONE',  ( -6.471393748263779777, 5.229711127719298247, -2.499999999999995115 ) ) ;
#28008 = CARTESIAN_POINT ( 'NONE',  ( 6.075462232699553766, 6.260663157670496304, -0.7216878364870458196 ) ) ;
#28009 = VERTEX_POINT ( 'NONE', #65516 ) ;
#28011 = CARTESIAN_POINT ( 'NONE',  ( 1.682290626080079621, 1.036857497476886936, 1.725414394560653042 ) ) ;
#28010 = CARTESIAN_POINT ( 'NONE',  ( 6.286648950733226826, 1.598451336667701339, -0.9137711784916457969 ) ) ;
#28012 = CARTESIAN_POINT ( 'NONE',  ( 4.429307823785958220, 1.078883539000154324, 2.029420160895245129 ) ) ;
#28014 = CARTESIAN_POINT ( 'NONE',  ( 2.518200207203071805, 0.7905618127436510045, 1.684796146788158699 ) ) ;
#28013 = CARTESIAN_POINT ( 'NONE',  ( -0.02919842301641034990, 1.352617229779122132, -2.329362550481127947 ) ) ;
#28015 = CARTESIAN_POINT ( 'NONE',  ( 3.285556943750000514, -1.363541666188709423, 1.896917185911906500 ) ) ;
#28016 = DIRECTION ( 'NONE',  ( 0.000000000000000000, 0.000000000000000000, -1.000000000000000000 ) ) ;
#28017 = CARTESIAN_POINT ( 'NONE',  ( 5.203337695038355193, 1.683698669361912259, -0.9069238330124268499 ) ) ;
#28018 = CARTESIAN_POINT ( 'NONE',  ( -7.049349804101573191, 10.31165964050546258, -1.199719254218440723 ) ) ;
#28019 = CARTESIAN_POINT ( 'NONE',  ( -5.980555157403903976, 6.149938236492225485, 0.000000000000000000 ) ) ;
#28022 = CARTESIAN_POINT ( 'NONE',  ( 3.608139902456270143, -0.7572706533398064765, -1.710698989992056607 ) ) ;
#28021 = CARTESIAN_POINT ( 'NONE',  ( 4.810148555269133652, 1.440736570533694527, -1.515338330687252988 ) ) ;
#28020 = B_SPLINE_CURVE_WITH_KNOTS ( 'NONE', 3,
 ( #33760, #98780, #99837, #135544, #50018, #20690, #1236 ),
 .UNSPECIFIED., .F., .F.,
 ( 4, 3, 4 ),
 ( 3.314949680322580664E-05, 0.0009000000012044581665, 0.001958074173707496923 ),
 .UNSPECIFIED. ) ;
#28023 = CARTESIAN_POINT ( 'NONE',  ( 5.165293337126522388, 8.969999960048859577, 1.040834085586084257E-14 ) ) ;
#28024 = VERTEX_POINT ( 'NONE', #197664 ) ;
#28025 = CARTESIAN_POINT ( 'NONE',  ( -1.436838838544810093, 7.449283400311735193, 4.203727439823581769 ) ) ;
#28026 = CARTESIAN_POINT ( 'NONE',  ( 0.03146710860973583185, -8.100320323339554207, -10.94525894661336629 ) ) ;
#28027 = CARTESIAN_POINT ( 'NONE',  ( 5.654863297658344834, -1.355735166614827625, 1.066293663406183256 ) ) ;
#28028 = CARTESIAN_POINT ( 'NONE',  ( -7.074657228232555717, 7.148188275893099686, 1.040834085586084257E-14 ) ) ;
#28029 = CARTESIAN_POINT ( 'NONE',  ( 1.898628203569406203, -0.8177110325628260679, -1.529257715385720307 ) ) ;
#28030 = CARTESIAN_POINT ( 'NONE',  ( -11.80248046418316044, 11.29999999999999893, -1.695421849633145017 ) ) ;
#28031 = CARTESIAN_POINT ( 'NONE',  ( -1.499999999999998002, 8.226407212580417294, -3.114167208185186553 ) ) ;
#28032 = CARTESIAN_POINT ( 'NONE',  ( 6.280482454654814362, -0.5424645211669875122, -1.942098458069536848 ) ) ;
#28033 = CONICAL_SURFACE ( 'NONE', #14253, 3.000000000000000000, 0.7853981633974523868 ) ;
#28034 = DIRECTION ( 'NONE',  ( 0.000000000000000000, 1.000000000000000000, 0.000000000000000000 ) ) ;
#28035 = CARTESIAN_POINT ( 'NONE',  ( 6.245025782124020708, -0.3104734683975469145, -2.148636169971326559 ) ) ;
#28036 = CARTESIAN_POINT ( 'NONE',  ( 4.037589748876240670, -1.260430739550026269, -1.321009972365666307 ) ) ;
#28037 = CARTESIAN_POINT ( 'NONE',  ( 2.342563710341159400, -1.922903400459201828, -0.3876519335672747313 ) ) ;
#28038 = CARTESIAN_POINT ( 'NONE',  ( -0.08807185805374209697, -1.306980724784766013, -1.666505321573110265 ) ) ;
#28039 = VECTOR ( 'NONE', #108177, 1000.000000000000000 ) ;
#28040 = CARTESIAN_POINT ( 'NONE',  ( 1.836970198721030181E-16, 13.49999999999999822, 1.500000000000000222 ) ) ;
#28041 = CARTESIAN_POINT ( 'NONE',  ( -4.207966135563084187, 7.175396087857926375, 2.420000000000000373 ) ) ;
#28042 = CARTESIAN_POINT ( 'NONE',  ( 8.938903350111612411, 9.323142084752035430, -0.7998128361456221525 ) ) ;
#28043 = EDGE_CURVE ( 'NONE', #118869, #207685, #91032, .T. ) ;
#28044 = CARTESIAN_POINT ( 'NONE',  ( 2.315225504062240702, 1.701464259299827919, -1.265282535349021575 ) ) ;
#28045 = CARTESIAN_POINT ( 'NONE',  ( -3.280709984826970516, 6.771319382366015383, 0.7216878364870317197 ) ) ;
#28046 = LINE ( 'NONE', #24833, #28564 ) ;
#28047 = CARTESIAN_POINT ( 'NONE',  ( -5.029675114306419559, 6.591709307070120261, -1.234896939913838754 ) ) ;
#28048 = CARTESIAN_POINT ( 'NONE',  ( 6.948074912775242140, -0.9353680688231647000, 1.957065181168372581 ) ) ;
#28050 = CARTESIAN_POINT ( 'NONE',  ( -0.7500000000000006661, 13.48958333401613352, -1.299038105676657340 ) ) ;
#28049 = CARTESIAN_POINT ( 'NONE',  ( -10.46840923150435643, 4.018901537134061286, 5.775382485202497307 ) ) ;
#28052 = VERTEX_POINT ( 'NONE', #68711 ) ;
#28051 = CARTESIAN_POINT ( 'NONE',  ( 3.616091037371416572, -0.6436381315554053906, 2.126022720447027670 ) ) ;
#28053 = CARTESIAN_POINT ( 'NONE',  ( 1.038157343047078296, -1.808118644657311203, 1.419311033984706816 ) ) ;
#28055 = CARTESIAN_POINT ( 'NONE',  ( 5.664908073332702187, 1.565568307794177327, -1.342975779555633187 ) ) ;
#28054 = CARTESIAN_POINT ( 'NONE',  ( 4.196412238629597447, 4.854568018944682706, -1.199719254218452047 ) ) ;
#28057 = CARTESIAN_POINT ( 'NONE',  ( 1.737500000000001155, -2.333333333333333037, 3.009438278150922130 ) ) ;
#28056 = CARTESIAN_POINT ( 'NONE',  ( 5.228604516725597229, 6.129068686715179126, -1.199719254218450271 ) ) ;
#28058 = CARTESIAN_POINT ( 'NONE',  ( 0.2329586101569527945, 4.095490909754247788, -2.400670182941808672 ) ) ;
#28059 = CARTESIAN_POINT ( 'NONE',  ( 5.214338956685347526, 1.703448749313410282, 0.6994016148276983591 ) ) ;
#28060 = CARTESIAN_POINT ( 'NONE',  ( 4.593150236022219428E-15, -8.011313137147251240, -11.00000000000000178 ) ) ;
#28061 = CARTESIAN_POINT ( 'NONE',  ( 5.203632029546647608, 4.965325544092860532, 1.040834085586084257E-14 ) ) ;
#28062 = CARTESIAN_POINT ( 'NONE',  ( 2.414726000362901637, 1.539333419754819854, 0.7781589270328890251 ) ) ;
#28063 = CARTESIAN_POINT ( 'NONE',  ( 1.147673126774436225, 1.985868168208399842, -0.3494872464938902357 ) ) ;
#28064 = CARTESIAN_POINT ( 'NONE',  ( 2.901363961662834168, -1.135721475377445167, -1.998492394250019233 ) ) ;
#28065 = CARTESIAN_POINT ( 'NONE',  ( 2.091474534086060544, 1.969063197997424686, -1.113951356575371365 ) ) ;
#28066 = CARTESIAN_POINT ( 'NONE',  ( 4.986996339425863844, -0.2567466434181593371, -2.090293495131962942 ) ) ;
#28067 = CARTESIAN_POINT ( 'NONE',  ( -7.444835747679825033, 7.858265591814152629, 0.000000000000000000 ) ) ;
#28068 = CARTESIAN_POINT ( 'NONE',  ( 3.637761035129345455, 0.7980134727624802471, -1.579695959945091044 ) ) ;
#28070 = CARTESIAN_POINT ( 'NONE',  ( 0.04153208042980033321, -1.776208762584199574, -1.448543121555950774 ) ) ;
#28069 = CARTESIAN_POINT ( 'NONE',  ( 5.533136087708556694, 5.627949321847663278, 0.000000000000000000 ) ) ;
#28071 = CARTESIAN_POINT ( 'NONE',  ( 4.347483306186128438, 1.840691044367316120, -0.04759384897683878457 ) ) ;
#28072 = CARTESIAN_POINT ( 'NONE',  ( -3.438964519360665051, 7.163875705896082913, -0.7998128361456281477 ) ) ;
#28073 = UNCERTAINTY_MEASURE_WITH_UNIT (LENGTH_MEASURE( 1.000000000000000082E-05 ), #48390, 'distance_accuracy_value', 'NONE');
#28074 = CARTESIAN_POINT ( 'NONE',  ( 6.466876083594112146, 6.647036307055676829, -0.7216878364870257245 ) ) ;
#28075 = CARTESIAN_POINT ( 'NONE',  ( -1.499999999999997780, 3.150000000000020783, 1.214306433183764966E-14 ) ) ;
#28076 = CARTESIAN_POINT ( 'NONE',  ( 4.839868765920234850, 2.185429510258177110, 0.1630863781024796955 ) ) ;
#28077 = CARTESIAN_POINT ( 'NONE',  ( -3.249150368769345043, 6.942425863539538611, 0.7998128361456341429 ) ) ;
#28078 = DIRECTION ( 'NONE',  ( 0.000000000000000000, 1.485208455481716197E-16, -1.000000000000000000 ) ) ;
#28079 = CARTESIAN_POINT ( 'NONE',  ( 1.364683531249990311, 4.613541667008083103, 0.7879004041258500513 ) ) ;
#28080 = CARTESIAN_POINT ( 'NONE',  ( 3.000521647167487593, -0.5595019940488660248, -1.843462078654713343 ) ) ;
#28081 = CARTESIAN_POINT ( 'NONE',  ( 1.364683531249997417, 8.484375000341396245, 2.602085213965210642E-15 ) ) ;
#28082 = CARTESIAN_POINT ( 'NONE',  ( -4.012850279964973232, 4.744375417122949301, 1.082531754730560403 ) ) ;
#28083 = CARTESIAN_POINT ( 'NONE',  ( 0.08853117554794007193, 1.285972019905703201, 1.811169930398129013 ) ) ;
#28084 = ORIENTED_EDGE ( 'NONE', *, *, #125699, .F. ) ;
#28086 = CARTESIAN_POINT ( 'NONE',  ( 1.500000000000035971, 8.500000000000000000, 9.886859966642587594 ) ) ;
#28085 = CARTESIAN_POINT ( 'NONE',  ( 4.137367429043227851, 8.820713629714100890, 0.7750000000000002442 ) ) ;
#28088 = ADVANCED_FACE ( 'NONE', ( #103376 ), #151075, .T. ) ;
#28087 = CARTESIAN_POINT ( 'NONE',  ( 5.529027716274630855, 5.344953845275508542, 1.040834085586084257E-14 ) ) ;
#28089 = DIRECTION ( 'NONE',  ( 0.000000000000000000, 0.000000000000000000, 1.000000000000000000 ) ) ;
#28090 = CARTESIAN_POINT ( 'NONE',  ( 0.2198916526692429596, 6.505559487570201860, -3.126830488621899384 ) ) ;
#28091 = CARTESIAN_POINT ( 'NONE',  ( 3.570880328030153539, 7.341005539872356600, 0.2896471194287209006 ) ) ;
#28092 = CARTESIAN_POINT ( 'NONE',  ( 1.328483007144948935, -1.247240240105648379, 1.514344512384787622 ) ) ;
#28093 = CARTESIAN_POINT ( 'NONE',  ( -1.364683531250000748, 1.571875000341421691, 0.000000000000000000 ) ) ;
#28094 = CARTESIAN_POINT ( 'NONE',  ( 6.819229411136438657, -0.1619093195798972928, 2.126376854085454404 ) ) ;
#28095 = CARTESIAN_POINT ( 'NONE',  ( 6.039501783790233169, 1.813256598412491982, -0.7494862575098264479 ) ) ;
#28096 = CARTESIAN_POINT ( 'NONE',  ( -8.784793466650835825, 12.33634391347959713, 1.199719254218462483 ) ) ;
#28097 = AXIS2_PLACEMENT_3D ( 'NONE', #67295, #133434, #17484 ) ;
#28098 = CARTESIAN_POINT ( 'NONE',  ( -6.249945625775490399, 7.354319987235250267, 1.082531754730549967 ) ) ;
#28099 = CARTESIAN_POINT ( 'NONE',  ( 5.700121470611750674, -2.161883445634639411, -0.004416275431240455560 ) ) ;
#28101 = ORIENTED_EDGE ( 'NONE', *, *, #3854, .T. ) ;
#28100 = CARTESIAN_POINT ( 'NONE',  ( 0.08058606168048106089, -5.741816521215585389, -10.99970480906930526 ) ) ;
#28102 = CARTESIAN_POINT ( 'NONE',  ( 1.364683531249988535, 3.863541667008087543, 0.7879004041258500513 ) ) ;
#28103 = CARTESIAN_POINT ( 'NONE',  ( 0.5439545674776785633, 1.865077268347898665, 0.1441030193207945287 ) ) ;
#28104 = CARTESIAN_POINT ( 'NONE',  ( 6.063786081214013635, 1.415308013037285484, -1.001223213843880799 ) ) ;
#28106 = CARTESIAN_POINT ( 'NONE',  ( 2.947022816757136621, -1.793111998972513277, -1.259777465452505796 ) ) ;
#28105 = CARTESIAN_POINT ( 'NONE',  ( -0.6801582343750143256, 0.3489583336747370534, -1.178068619123865846 ) ) ;
#28107 = CARTESIAN_POINT ( 'NONE',  ( 4.928937574911031128, 2.206605557787114869, 0.6751633795739877542 ) ) ;
#28108 = CARTESIAN_POINT ( 'NONE',  ( 6.063760116591036642, 2.031045510622536909, -0.3477994121598385613 ) ) ;
#28109 = CARTESIAN_POINT ( 'NONE',  ( 1.658044662407763381, -1.373417096361102097, 1.373162012216273320 ) ) ;
#28110 = CARTESIAN_POINT ( 'NONE',  ( -5.870317324592811303, 8.832158731124840401, -1.082531754730537976 ) ) ;
#28111 = PRODUCT_DEFINITION_SHAPE ( 'NONE', 'NONE',  #214418 ) ;
#28112 = CARTESIAN_POINT ( 'NONE',  ( 5.591005849568446706, 5.791977450266268868, -0.7139200525481930182 ) ) ;
#28113 = CARTESIAN_POINT ( 'NONE',  ( 5.678019686890188211, 2.088907387943875982, -0.3644037002746222664 ) ) ;
#28114 = SURFACE_STYLE_USAGE ( .BOTH. , #44380 ) ;
#28115 = CARTESIAN_POINT ( 'NONE',  ( 1.969375177810539945, -1.978050944945686673, -0.3905967402937361443 ) ) ;
#28116 = CARTESIAN_POINT ( 'NONE',  ( -4.378920427089552092, 8.052564898339037214, 0.7216878364870317197 ) ) ;
#28117 = CARTESIAN_POINT ( 'NONE',  ( 5.754950181447250124, -1.742976869204535983, 1.353379275444612562 ) ) ;
#28118 = CARTESIAN_POINT ( 'NONE',  ( -4.707509334217570007, 5.241700920597089031, 1.110557563554106952 ) ) ;
#28119 = CARTESIAN_POINT ( 'NONE',  ( -3.383843058911719215, -3.076622456046647969, 0.6547969591862352612 ) ) ;
#28120 = CARTESIAN_POINT ( 'NONE',  ( -0.02319159430949970999, 0.003959926571647092407, -1.810968101872318714 ) ) ;
#28121 = CARTESIAN_POINT ( 'NONE',  ( -6.291865805193673111, 9.498204651771386509, -1.199719254218452047 ) ) ;
#28123 = CARTESIAN_POINT ( 'NONE',  ( -4.281342646865346602, 8.216926531310035031, 0.7998128361456350310 ) ) ;
#28122 = CARTESIAN_POINT ( 'NONE',  ( -4.651396499164954790, 8.416516698401213858, 0.5247324002638984464 ) ) ;
#28124 = CARTESIAN_POINT ( 'NONE',  ( -10.89402507593495351, 4.580915115640823210, 4.512369680550198936 ) ) ;
#28125 = ORIENTED_EDGE ( 'NONE', *, *, #40765, .F. ) ;
#28126 = CARTESIAN_POINT ( 'NONE',  ( 4.311438335051980708, -0.3541389166773502573, 2.030069380940119572 ) ) ;
#28127 = CARTESIAN_POINT ( 'NONE',  ( -8.054952659850432184, 8.570068656013202002, 0.000000000000000000 ) ) ;
#28128 = CARTESIAN_POINT ( 'NONE',  ( 0.1331565106231328843, 0.003911343561965873426, -1.946049565259087455 ) ) ;
#28129 = CARTESIAN_POINT ( 'NONE',  ( -5.752737250900127997, 5.605948302338584099, 0.000000000000000000 ) ) ;
#28130 = CARTESIAN_POINT ( 'NONE',  ( -5.792162442946777290, 6.216820166843662676, 1.023959129923063260 ) ) ;
#28131 = CARTESIAN_POINT ( 'NONE',  ( 4.758466132964124462, 2.014421802844321707, 0.1462751549737814905 ) ) ;
#28132 = CARTESIAN_POINT ( 'NONE',  ( -1.500000000000015099, 0.6291666666666863028, -0.8660254037844313801 ) ) ;
#28134 = CARTESIAN_POINT ( 'NONE',  ( 7.768458830950378591, 12.00702636951006497, 1.040834085586084257E-14 ) ) ;
#28133 = CARTESIAN_POINT ( 'NONE',  ( -5.061990249855848667, 6.999017606288844284, -1.599625672291271394 ) ) ;
#28135 = CARTESIAN_POINT ( 'NONE',  ( 6.123478934866503742, 10.29580919065294431, 0.7998128361456462443 ) ) ;
#28136 = CIRCLE ( 'NONE', #128569, 9.499999999999991118 ) ;
#28137 = CARTESIAN_POINT ( 'NONE',  ( 4.627839754413318296, -1.266395719900258232, -1.625807017514354191 ) ) ;
#28138 = CARTESIAN_POINT ( 'NONE',  ( 3.147111449167848019, 0.9091449406319618287, 1.799922684605055556 ) ) ;
#28139 = ORIENTED_EDGE ( 'NONE', *, *, #138594, .F. ) ;
#28140 = CARTESIAN_POINT ( 'NONE',  ( 6.727182134110200273, -0.004969159814478123736, 2.189081792362323586 ) ) ;
#28141 = CARTESIAN_POINT ( 'NONE',  ( 4.976006071415387311, 5.764094157194782575, 1.199719254218462483 ) ) ;
#28143 = ORIENTED_EDGE ( 'NONE', *, *, #7522, .T. ) ;
#28142 = CARTESIAN_POINT ( 'NONE',  ( -0.4909524369919514020, 7.516007857510251355, -2.014442075801170073 ) ) ;
#28144 = CARTESIAN_POINT ( 'NONE',  ( 2.847029653296664353, -1.038834691150035461, 1.727737368502464621 ) ) ;
#28145 = CARTESIAN_POINT ( 'NONE',  ( 2.554438963407625884, -1.601868926591401232, -0.9074879233003438905 ) ) ;
#28146 = CARTESIAN_POINT ( 'NONE',  ( 1.085104692462773412, -2.252536170888468359, -0.5009029511823160918 ) ) ;
#28147 = CARTESIAN_POINT ( 'NONE',  ( 4.736594563127852098, 6.619389305106191834, -1.599625672291273171 ) ) ;
#28148 = CARTESIAN_POINT ( 'NONE',  ( 3.110779230992101407, 1.568002374463087989, -1.488160049990403078 ) ) ;
#28149 = CARTESIAN_POINT ( 'NONE',  ( -5.201524489137236529, 9.220195670635433771, 0.7998128361456481317 ) ) ;
#28150 =( GEOMETRIC_REPRESENTATION_CONTEXT ( 3 ) GLOBAL_UNCERTAINTY_ASSIGNED_CONTEXT ( ( #102735 ) ) GLOBAL_UNIT_ASSIGNED_CONTEXT ( ( #68448, #86857, #188616 ) ) REPRESENTATION_CONTEXT ( 'NONE', 'WORKASPACE' ) );
#28151 = ORIENTED_EDGE ( 'NONE', *, *, #100532, .T. ) ;
#28152 = CARTESIAN_POINT ( 'NONE',  ( 1.224999999999974332, 2.374999999999988454, -3.295974604355933479E-14 ) ) ;
#28153 = CARTESIAN_POINT ( 'NONE',  ( 0.9537216069140028729, 1.868711056098860235, -0.08788249432020722729 ) ) ;
#28154 = CARTESIAN_POINT ( 'NONE',  ( 6.139525842074132100, -1.427670353879314957, -1.359795004109279004 ) ) ;
#28156 = CARTESIAN_POINT ( 'NONE',  ( 8.148087131688683371, 10.52918762510205042, -1.443375672974063439 ) ) ;
#28155 = CARTESIAN_POINT ( 'NONE',  ( -0.6823417656249969321, 3.967708333674754950, -1.181850606188749264 ) ) ;
#28158 = CARTESIAN_POINT ( 'NONE',  ( 0.9970219447392356660, -0.5395372827587068265, -2.139793933917451874 ) ) ;
#28157 = CARTESIAN_POINT ( 'NONE',  ( -6.738566041191992539, 7.820414121934134322, 1.199719254218450271 ) ) ;
#28159 = CARTESIAN_POINT ( 'NONE',  ( 6.584440175795505112, 1.195396180001909059, -1.690200020538407566 ) ) ;
#28160 = CARTESIAN_POINT ( 'NONE',  ( 7.318703993278529829, 7.432909501780090800, 1.040834085586084257E-14 ) ) ;
#28161 = CARTESIAN_POINT ( 'NONE',  ( -4.089755892816631544, 7.923132308261379819, -0.7998128361456281477 ) ) ;
#28162 = CARTESIAN_POINT ( 'NONE',  ( 6.639320575229256782, 3.683803431435454190, 2.717262547424610375 ) ) ;
#28163 = CARTESIAN_POINT ( 'NONE',  ( 4.926621433916460902, 1.886357061574754690, 0.5729670753305516895 ) ) ;
#28164 = CARTESIAN_POINT ( 'NONE',  ( 6.504167520383483669, -0.8605252283936345448, 1.825738368183300153 ) ) ;
#28165 = CARTESIAN_POINT ( 'NONE',  ( -1.500000000000015099, -0.08958333265051321437, -0.8660254037844383745 ) ) ;
#28166 = CARTESIAN_POINT ( 'NONE',  ( 4.916800105644766994, 1.594097815661306816, -1.668853466001555486 ) ) ;
#28167 = CARTESIAN_POINT ( 'NONE',  ( 2.219651360329556233, 0.3568934070868194919, -2.031323280462021152 ) ) ;
#28168 = CARTESIAN_POINT ( 'NONE',  ( 7.348156068926750883, 8.635565504245116486, -1.082531754730537976 ) ) ;
#28169 = CARTESIAN_POINT ( 'NONE',  ( 5.611095471209277541, 7.639640364534566075, 1.599625672291268286 ) ) ;
#28170 = CARTESIAN_POINT ( 'NONE',  ( 3.711900195091365262, 7.552577004240394132, -0.7998128361456362523 ) ) ;
#28171 = CARTESIAN_POINT ( 'NONE',  ( -1.364683531250012516, 2.342708333674752286, 0.7879004041258379498 ) ) ;
#28172 = CARTESIAN_POINT ( 'NONE',  ( 4.686278372178935392, 5.496354851410763409, 1.199719254218452047 ) ) ;
#28173 = CARTESIAN_POINT ( 'NONE',  ( 5.124618875841165710, 8.922546421882614709, 1.040834085586084257E-14 ) ) ;
#28174 = CARTESIAN_POINT ( 'NONE',  ( 4.949771893170417769, 1.605651206033286815, 1.461634471724428064 ) ) ;
#28176 = CARTESIAN_POINT ( 'NONE',  ( 4.300242120186610784, 1.420457692841030850, -1.171515996850613694 ) ) ;
#28175 = CARTESIAN_POINT ( 'NONE',  ( -3.633221978782299910, 5.261844946711204507, -1.443375672974053447 ) ) ;
#28177 = EDGE_CURVE ( 'NONE', #94850, #103686, #148927, .T. ) ;
#28179 = CARTESIAN_POINT ( 'NONE',  ( 6.620655732516644854, 2.103946135090263514, 2.037628900882877847 ) ) ;
#28178 = CARTESIAN_POINT ( 'NONE',  ( 1.364683531249988535, 5.655208333674751842, -0.7879004041258300672 ) ) ;
#28180 = CARTESIAN_POINT ( 'NONE',  ( 6.005464345382193869, -2.175231771021503668, 0.2666438670960933344 ) ) ;
#28181 = LINE ( 'NONE', #128965, #74335 ) ;
#28182 = CARTESIAN_POINT ( 'NONE',  ( 6.473497647428577473, 2.167417048064937291, -0.6491153028224846411 ) ) ;
#28183 = ORIENTED_EDGE ( 'NONE', *, *, #54696, .T. ) ;
#28184 = CARTESIAN_POINT ( 'NONE',  ( -3.976739547089790161, 7.847837856468413698, 0.08243740857501527519 ) ) ;
#28185 = CARTESIAN_POINT ( 'NONE',  ( 5.568688238291347403, 7.519645578322940338, 1.337618216391135428 ) ) ;
#28186 = CARTESIAN_POINT ( 'NONE',  ( -5.628043163004235794, 5.738674243025936761, 0.7216878364870257245 ) ) ;
#28187 = CARTESIAN_POINT ( 'NONE',  ( -0.008366613517340566394, 2.629643693813620953, 12.00001160347414775 ) ) ;
#28188 = CARTESIAN_POINT ( 'NONE',  ( 0.4086181399716379281, 1.536643064871806574, 0.8779792868154213670 ) ) ;
#28189 = AXIS2_PLACEMENT_3D ( 'NONE', #125705, #210049, #175453 ) ;
#28190 = CARTESIAN_POINT ( 'NONE',  ( 4.969394074578011633, -1.701821450762316612, -1.075051190359946895 ) ) ;
#28191 = B_SPLINE_CURVE_WITH_KNOTS ( 'NONE', 3,
 ( #155350, #154289, #21047, #55712 ),
 .UNSPECIFIED., .F., .F.,
 ( 4, 4 ),
 ( 0.000000000000000000, 0.0004044236633722958431 ),
 .UNSPECIFIED. ) ;
#28192 = CARTESIAN_POINT ( 'NONE',  ( 4.984594031318565932, 8.967110136513669616, 0.7998128361456462443 ) ) ;
#28193 = CARTESIAN_POINT ( 'NONE',  ( 4.471769775969771210, 2.043305595564361088, -0.5093722314385378258 ) ) ;
#28194 = CARTESIAN_POINT ( 'NONE',  ( 2.214329231836575040, 1.858617268789555466, 0.4632827458446056035 ) ) ;
#28195 = AXIS2_PLACEMENT_3D ( 'NONE', #52231, #16504, #82585 ) ;
#28196 = DIRECTION ( 'NONE',  ( 0.000000000000000000, 0.000000000000000000, -1.000000000000000000 ) ) ;
#28197 = CARTESIAN_POINT ( 'NONE',  ( 3.332427603156477680, -1.175354876789212799, 1.580226413267592500 ) ) ;
#28198 = CARTESIAN_POINT ( 'NONE',  ( 5.203380996274193038, 1.779418458119955915, -0.9556711282029080046 ) ) ;
#28199 = CARTESIAN_POINT ( 'NONE',  ( 1.973319494866377699, 1.790917844098998124, -0.5403536831049270406 ) ) ;
#28202 = ORIENTED_EDGE ( 'NONE', *, *, #58359, .F. ) ;
#28201 = CARTESIAN_POINT ( 'NONE',  ( 1.054777118923880597, 0.3758132965740559883, 1.874924941132802836 ) ) ;
#28200 = CARTESIAN_POINT ( 'NONE',  ( 5.215364217145412873, -0.2476331258763775356, 1.706884187403294728 ) ) ;
#28204 = CARTESIAN_POINT ( 'NONE',  ( 4.609409038966229666, 6.400729850259146758, -1.443375672974051449 ) ) ;
#28203 = CARTESIAN_POINT ( 'NONE',  ( 1.155211076828046579, -1.737760091701185505, 1.360235214042208263 ) ) ;
#28205 = CARTESIAN_POINT ( 'NONE',  ( -1.364683531250012516, 2.592708333674753174, 0.7879004041258379498 ) ) ;
#28206 = CARTESIAN_POINT ( 'NONE',  ( 7.884230021546724920, 9.157022099014721306, 1.199719254218462483 ) ) ;
#28207 = DIRECTION ( 'NONE',  ( 0.2460297208025344073, -9.436895709313838482E-16, 0.9692622846690297500 ) ) ;
#28208 = FILL_AREA_STYLE_COLOUR ( '', #71333 ) ;
#28209 = CARTESIAN_POINT ( 'NONE',  ( 1.423205080756849483, 7.980384757729337863, -10.65537363484302524 ) ) ;
#28210 = FACE_OUTER_BOUND ( 'NONE', #8888, .T. ) ;
#28211 = EDGE_CURVE ( 'NONE', #38245, #152353, #33045, .T. ) ;
#28212 = ORIENTED_EDGE ( 'NONE', *, *, #17058, .F. ) ;
#28213 = CARTESIAN_POINT ( 'NONE',  ( 2.436061438456170958, 1.271862942251865691, 1.633573898902056731 ) ) ;
#28214 = CARTESIAN_POINT ( 'NONE',  ( -1.500000000000013101, 3.629166666666692187, -0.8660254037844313801 ) ) ;
#28215 = CARTESIAN_POINT ( 'NONE',  ( 5.880485940025228508, 7.883652901494672349, 1.599625672291267398 ) ) ;
#28216 = CARTESIAN_POINT ( 'NONE',  ( -6.714312387265696458, 8.856450423275211037, 1.599625672291283607 ) ) ;
#28217 = CARTESIAN_POINT ( 'NONE',  ( 3.607351389687783794, 6.366271167014519783, 1.199719254218451159 ) ) ;
#28218 = CARTESIAN_POINT ( 'NONE',  ( 6.129554906816851556, -0.2598956320666659381, 2.104415924757463419 ) ) ;
#28219 = CARTESIAN_POINT ( 'NONE',  ( 11.94105721237523277, 13.40000000000000036, 1.187919463087248273 ) ) ;
#28220 = CARTESIAN_POINT ( 'NONE',  ( -1.201851678989727383E-14, 3.196875000341420137, -1.575800808251660134 ) ) ;
#28222 = CARTESIAN_POINT ( 'NONE',  ( 4.033714395265605823, 4.664753868353354704, -1.199719254218446718 ) ) ;
#28221 = DIRECTION ( 'NONE',  ( 0.2684563758389248433, 0.000000000000000000, 0.9632918427306597087 ) ) ;
#28223 = CARTESIAN_POINT ( 'NONE',  ( 3.954453749441131816, 1.458333106491338960, 1.392332789497241263 ) ) ;
#28224 = CARTESIAN_POINT ( 'NONE',  ( 4.680823747822191017, 1.589204433792507087, -1.069448900409355030 ) ) ;
#28225 = FILL_AREA_STYLE_COLOUR ( '', #13720 ) ;
#28226 = CARTESIAN_POINT ( 'NONE',  ( 2.402122600552298870, -0.8417629408748151798, -2.023652355447075557 ) ) ;
#28227 = CARTESIAN_POINT ( 'NONE',  ( 0.1333692844072767447, 1.351132181276387678, -2.308013766563504987 ) ) ;
#28228 = CARTESIAN_POINT ( 'NONE',  ( 1.499999999999989120, 0.5562500006828161592, 0.000000000000000000 ) ) ;
#28229 = CARTESIAN_POINT ( 'NONE',  ( 5.185796262198086204, 1.939088309008336397, -0.5409127675100529054 ) ) ;
#28230 = CARTESIAN_POINT ( 'NONE',  ( -5.506582945444718824, 9.576097202994168001, 0.7998128361456481317 ) ) ;
#28232 = CARTESIAN_POINT ( 'NONE',  ( 0.03478015955125923070, -1.617804660175032661, 1.203375172262765913 ) ) ;
#28231 = DIRECTION ( 'NONE',  ( 1.000000000000000000, -0.000000000000000000, -0.000000000000000000 ) ) ;
#28233 = CARTESIAN_POINT ( 'NONE',  ( -0.6823417656250003738, 9.213541667008065872, 1.181850606188754593 ) ) ;
#28235 = CARTESIAN_POINT ( 'NONE',  ( -6.095272577795516789, 9.268845886473535245, 1.199719254218452047 ) ) ;
#28234 = CARTESIAN_POINT ( 'NONE',  ( 3.105106965723201551, -0.4054212715494521224, 2.050880055191468543 ) ) ;
#28237 = VERTEX_POINT ( 'NONE', #3700 ) ;
#28236 = CARTESIAN_POINT ( 'NONE',  ( 2.361930338997704659, 0.7344707938763440636, 1.560707491107244715 ) ) ;
#28238 = CARTESIAN_POINT ( 'NONE',  ( 5.713165544288242970, 1.732532623411761286, -1.222520872474173848 ) ) ;
#28239 = CARTESIAN_POINT ( 'NONE',  ( 5.229694566569264680, 7.124396299129368337, 1.599625672291267398 ) ) ;
#28240 = CARTESIAN_POINT ( 'NONE',  ( 7.032125997333287692, 15.00041888085534758, 9.944927957745147040 ) ) ;
#28241 = CARTESIAN_POINT ( 'NONE',  ( 7.626802973668208807, -6.615717645446816064, 7.927630635717502372 ) ) ;
#28242 = FACE_OUTER_BOUND ( 'NONE', #174602, .T. ) ;
#28243 = CARTESIAN_POINT ( 'NONE',  ( 7.657657833620182153, 7.828355648845348291, -0.7998128361456281477 ) ) ;
#28244 = VERTEX_POINT ( 'NONE', #184605 ) ;
#28245 = CARTESIAN_POINT ( 'NONE',  ( 1.274519002043996707, 3.984210321688911094, -0.4828173461639029274 ) ) ;
#28246 = ORIENTED_EDGE ( 'NONE', *, *, #147535, .F. ) ;
#28247 = CARTESIAN_POINT ( 'NONE',  ( 1.383166562764587271, 0.1333312229490003775, -1.806600723499194538 ) ) ;
#28248 = CARTESIAN_POINT ( 'NONE',  ( -4.855791571988752331, 8.816840600628864877, 0.7998128361456481317 ) ) ;
#28249 = EDGE_LOOP ( 'NONE', ( #44108, #63980, #98141, #104247, #95306, #50558 ) ) ;
#28250 = CARTESIAN_POINT ( 'NONE',  ( 3.837121167867449945, 4.435395103055503441, 1.199719254218464037 ) ) ;
#28251 = VERTEX_POINT ( 'NONE', #35154 ) ;
#28252 = CARTESIAN_POINT ( 'NONE',  ( 6.222266154028957885, 6.224008365980749247, 0.7998128361456352531 ) ) ;
#28253 = CARTESIAN_POINT ( 'NONE',  ( 2.807043740381453656, 1.552634882062135624, -0.9328946631028020020 ) ) ;
#28254 = CARTESIAN_POINT ( 'NONE',  ( 6.639320575229259447, 0.002292789353198348111, 1.996863816985874118 ) ) ;
#28255 = PRESENTATION_STYLE_ASSIGNMENT (( #190735 ) ) ;
#28256 = CARTESIAN_POINT ( 'NONE',  ( 4.002655450416458649, 7.592114961386800864, 0.1875155472659401079 ) ) ;
#28257 = CARTESIAN_POINT ( 'NONE',  ( 4.527703488433511225, 1.805393378231552326, -0.4512502670087223944 ) ) ;
#28258 = CARTESIAN_POINT ( 'NONE',  ( 1.142033650006045731, 0.7776438622074226537, 1.750858609485239192 ) ) ;
#28259 = CARTESIAN_POINT ( 'NONE',  ( 1.324926479183065497, -0.04897172810776688479, 1.825096452545173609 ) ) ;
#28260 = CARTESIAN_POINT ( 'NONE',  ( -10.38819714233664193, 3.487142912321087973, 5.997628416523025585 ) ) ;
#28261 = CARTESIAN_POINT ( 'NONE',  ( -10.14058302375764420, 3.661560415210057151, -6.348512455255221454 ) ) ;
#28262 = VECTOR ( 'NONE', #105485, 1000.000000000000000 ) ;
#28263 = CARTESIAN_POINT ( 'NONE',  ( 5.614387949662905442, 7.370906683214474953, 1.237392280610301931 ) ) ;
#28264 = CARTESIAN_POINT ( 'NONE',  ( 4.796824973295459316, 8.251456047330133714, 0.8599625132450954279 ) ) ;
#28265 = CARTESIAN_POINT ( 'NONE',  ( -4.297571505851936813, 4.116180966356429494, 1.214306433183764966E-14 ) ) ;
#28266 = CARTESIAN_POINT ( 'NONE',  ( 8.270110514656034084, 9.711179024262627024, 1.082531754730558626 ) ) ;
#28267 = CARTESIAN_POINT ( 'NONE',  ( 6.051603174176475086, 1.488812912110796249, 1.289293616420229549 ) ) ;
#28268 = CARTESIAN_POINT ( 'NONE',  ( -4.283486466913726254, 7.084819080452935403, -1.199719254218452047 ) ) ;
#28269 = DIRECTION ( 'NONE',  ( -0.9982742078614211811, 0.000000000000000000, 0.05872483221476467591 ) ) ;
#28270 = CARTESIAN_POINT ( 'NONE',  ( 0.7618063994256699667, 1.031939465966443814, 1.818122583218291677 ) ) ;
#28271 = CARTESIAN_POINT ( 'NONE',  ( 6.611572464958476836, 10.86525164242692298, 0.7998128361456462443 ) ) ;
#28272 = CARTESIAN_POINT ( 'NONE',  ( 5.192375284248013756, -1.911820684568351192, -0.2360692857661383648 ) ) ;
#28273 = CARTESIAN_POINT ( 'NONE',  ( -5.799137018343247796, 7.788745826199009237, -1.599625672291256295 ) ) ;
#28274 = CARTESIAN_POINT ( 'NONE',  ( 0.8502975112493587062, 0.5252643332615304361, 1.748389446526978031 ) ) ;
#28275 = CARTESIAN_POINT ( 'NONE',  ( 2.702037527177497012, -0.6914408288211832954, 2.095836555436859872 ) ) ;
#28276 = CARTESIAN_POINT ( 'NONE',  ( -0.08783152977152529350, -1.912005390248720627, -0.04503566501021933483 ) ) ;
#28277 = CARTESIAN_POINT ( 'NONE',  ( 0.9241884870439884825, 0.9676023207046909880, 1.715383555584276909 ) ) ;
#28278 = CARTESIAN_POINT ( 'NONE',  ( 2.612754452619329371, -0.1881026344860724786, 1.932912858947251511 ) ) ;
#28279 = CARTESIAN_POINT ( 'NONE',  ( 0.8431247865267020858, -1.122328847578180078, 1.674629589540656216 ) ) ;
#28281 = CARTESIAN_POINT ( 'NONE',  ( 5.084723738625635647, 1.780007044882421008, 0.5427147737909858716 ) ) ;
#28280 = CARTESIAN_POINT ( 'NONE',  ( -4.308458954092677651, 8.248562223075252220, -0.7998128361456362523 ) ) ;
#28282 = CARTESIAN_POINT ( 'NONE',  ( 5.899733120602060232, 6.912052057904395141, -1.199719254218452047 ) ) ;
#28283 = DIRECTION ( 'NONE',  ( 0.000000000000000000, -1.000000000000000000, 0.000000000000000000 ) ) ;
#28284 = CARTESIAN_POINT ( 'NONE',  ( 10.72180055030867329, 11.40318881831530540, 0.7998128361456341429 ) ) ;
#28285 = CARTESIAN_POINT ( 'NONE',  ( -5.590039407536138150, 5.416134151747256986, 0.000000000000000000 ) ) ;
#28286 = CARTESIAN_POINT ( 'NONE',  ( -7.449279056065764237, 7.655523418356991350, 0.7998128361456341429 ) ) ;
#28287 = CARTESIAN_POINT ( 'NONE',  ( 1.154151856878969928, 0.8927059368322427524, 2.001694687108931170 ) ) ;
#28288 = CARTESIAN_POINT ( 'NONE',  ( 3.633221978782282147, 5.261844946711204507, -1.443375672974057666 ) ) ;
#28289 = CIRCLE ( 'NONE', #149351, 0.5000000000000011102 ) ;
#28290 = CARTESIAN_POINT ( 'NONE',  ( 8.039058738260216330, 8.343599714250547805, -0.7998128361456341429 ) ) ;
#28291 = DIRECTION ( 'NONE',  ( -0.000000000000000000, -1.000000000000000000, -0.000000000000000000 ) ) ;
#28292 = CARTESIAN_POINT ( 'NONE',  ( 3.141029808440584326, -1.609794727316344209, 0.8612202190056221784 ) ) ;
#28293 = CARTESIAN_POINT ( 'NONE',  ( -4.009460741339347045, 5.700790169694431420, -1.599625672291256295 ) ) ;
#28294 = CARTESIAN_POINT ( 'NONE',  ( -5.328968068096138211, 7.722205811214136517, -1.323081262718794893 ) ) ;
#28295 = DIRECTION ( 'NONE',  ( -0.9999980456341537316, 0.000000000000000000, -0.001977050295958555567 ) ) ;
#28296 = CARTESIAN_POINT ( 'NONE',  ( 10.06423010004587759, 10.63602329300870153, 0.000000000000000000 ) ) ;
#28297 = CARTESIAN_POINT ( 'NONE',  ( 1.365712245162364225, 1.898099017218597195, -0.3287360691993664874 ) ) ;
#28298 = CARTESIAN_POINT ( 'NONE',  ( 5.084793414397763556, 1.876112756342168675, 0.5732009990792874543 ) ) ;
#28299 = MECHANICAL_DESIGN_GEOMETRIC_PRESENTATION_REPRESENTATION (  '', ( #38659 ), #7081 ) ;
#28300 = CARTESIAN_POINT ( 'NONE',  ( -8.362681821530818738, 8.650883634741092010, -0.7998128361456291469 ) ) ;
#28301 = CARTESIAN_POINT ( 'NONE',  ( 6.335737856287750880, 6.286115675290828264, -0.7998128361456281477 ) ) ;
#28302 = EDGE_CURVE ( 'NONE', #154544, #150426, #199787, .T. ) ;
#28303 = CARTESIAN_POINT ( 'NONE',  ( 5.407841436338867602, -0.9846607899807978681, -1.957994596084790206 ) ) ;
#28304 = CARTESIAN_POINT ( 'NONE',  ( 5.345992642490140057, 5.131412925860272090, 1.040834085586084257E-14 ) ) ;
#28305 = CARTESIAN_POINT ( 'NONE',  ( 3.485274717979901293, 0.04603381543630095940, 2.069897711131869933 ) ) ;
#28307 = CARTESIAN_POINT ( 'NONE',  ( -1.364683531250000748, 0.8218750003414210248, 0.000000000000000000 ) ) ;
#28306 = CARTESIAN_POINT ( 'NONE',  ( 4.000000000000012434, 0.000000000000000000, -0.7500000000000006661 ) ) ;
#28308 = ORIENTED_EDGE ( 'NONE', *, *, #22894, .F. ) ;
#28309 = CARTESIAN_POINT ( 'NONE',  ( 3.639517500262396954, 0.8282738168534724554, 2.144427848026169592 ) ) ;
#28311 = ORIENTED_EDGE ( 'NONE', *, *, #51004, .T. ) ;
#28310 = CARTESIAN_POINT ( 'NONE',  ( 7.619319141200070256, 8.951922421897323900, 1.082531754730558626 ) ) ;
#28313 = CARTESIAN_POINT ( 'NONE',  ( 3.285556943750000514, -1.363541666188709423, 1.896917185911906500 ) ) ;
#28312 = CARTESIAN_POINT ( 'NONE',  ( 5.397554552016226914, 6.430140077841320689, 1.082531754730549078 ) ) ;
#28314 = CARTESIAN_POINT ( 'NONE',  ( -7.834948807406196813, -5.743759731405707392, -7.720982915751337217 ) ) ;
#28315 = DIRECTION ( 'NONE',  ( 0.000000000000000000, 1.000000000000000000, 0.000000000000000000 ) ) ;
#28316 = CARTESIAN_POINT ( 'NONE',  ( 3.591681417399609888, -1.939766604489696622, -0.09448766823863874453 ) ) ;
#28318 = ADVANCED_FACE ( 'NONE', ( #99123 ), #46748, .T. ) ;
#28317 = CARTESIAN_POINT ( 'NONE',  ( 10.34450801710256584, 11.17094022948226240, 0.7216878364870438212 ) ) ;
#28319 = VERTEX_POINT ( 'NONE', #133780 ) ;
#28320 = CARTESIAN_POINT ( 'NONE',  ( 5.256085721135645095, 0.7693902824621422498, -1.750971482026221437 ) ) ;
#28321 = CARTESIAN_POINT ( 'NONE',  ( 6.141572722362285575, -1.252861708448499201, -1.185644778512841002 ) ) ;
#28322 = CARTESIAN_POINT ( 'NONE',  ( 5.067592334412735156, 1.357865985192594049, 1.490972259599516070 ) ) ;
#28323 = CARTESIAN_POINT ( 'NONE',  ( 0.5773502691896124084, -2.500000000000002220, -0.9999999999999991118 ) ) ;
#28324 = CARTESIAN_POINT ( 'NONE',  ( 2.157103830005083100, -1.704838622333640030, 1.401371054633032909 ) ) ;
#28326 = CARTESIAN_POINT ( 'NONE',  ( -3.851925040058345573, 5.587274861525073355, -1.443375672974078761 ) ) ;
#28325 = CARTESIAN_POINT ( 'NONE',  ( -10.15522075183580419, 11.80651128435196462, 1.199719254218462483 ) ) ;
#28328 = CARTESIAN_POINT ( 'NONE',  ( 0.6195364366361589825, -0.9414703481081601044, -1.498462015107356882 ) ) ;
#28327 = CARTESIAN_POINT ( 'NONE',  ( 1.921934154048171584, 1.202774473455773041, -1.709796194579858319 ) ) ;
#28329 = CARTESIAN_POINT ( 'NONE',  ( 5.801407773674092105, 1.352156682446105984, -1.496049708713815374 ) ) ;
#28331 = CARTESIAN_POINT ( 'NONE',  ( 3.293229231460121031, 1.807080150709074129, 1.410200864199236293 ) ) ;
#28330 = CARTESIAN_POINT ( 'NONE',  ( 4.064412189046650248, 7.963840997188264659, 0.7998128361456271485 ) ) ;
#28332 = CARTESIAN_POINT ( 'NONE',  ( 0.5854151811709865649, -1.726609166672494311, -0.2174223460936832719 ) ) ;
#28333 = CARTESIAN_POINT ( 'NONE',  ( 2.848016566918720294, -1.427295477286108394, -1.568503593382633454 ) ) ;
#28334 = CARTESIAN_POINT ( 'NONE',  ( -1.123270288249905713, 3.300000000000025135, 0.7750000000000119016 ) ) ;
#28335 = CARTESIAN_POINT ( 'NONE',  ( 1.457864220016273693, 1.308402020977760261, 1.137755859488085886 ) ) ;
#28336 = CARTESIAN_POINT ( 'NONE',  ( -0.6801582343750022241, 1.130208333674734167, -1.178068619123841643 ) ) ;
#28337 = CARTESIAN_POINT ( 'NONE',  ( -11.43195036480940452, 12.44475503714751596, 3.649565797774462883 ) ) ;
#28338 =( BOUNDED_CURVE ( )  B_SPLINE_CURVE ( 3, ( #191291, #124271, #61313, #90633 ),
 .UNSPECIFIED., .F., .T. ) 
 B_SPLINE_CURVE_WITH_KNOTS ( ( 4, 4 ),
 ( 0.000000000000000000, 0.4999999999999948930 ),
 .UNSPECIFIED. ) 
 CURVE ( )  GEOMETRIC_REPRESENTATION_ITEM ( )  RATIONAL_B_SPLINE_CURVE ( ( 1.000000000000000444, 0.3333333333333403092, 0.3333333333333334814, 0.9999999999999936717 ) ) 
 REPRESENTATION_ITEM ( '' )  );
#28339 = CARTESIAN_POINT ( 'NONE',  ( 0.8542542287434266024, -0.7813174834335520069, 2.025881038206469587 ) ) ;
#28340 = CARTESIAN_POINT ( 'NONE',  ( 3.309780021317248355, -1.205041885261768808, -1.616693488061982098 ) ) ;
#28341 = CARTESIAN_POINT ( 'NONE',  ( 5.343750000000003553, 1.895863743164196258, 0.7852924748297027691 ) ) ;
#28342 = AXIS2_PLACEMENT_3D ( 'NONE', #155968, #139738, #43298 ) ;
#28343 = CARTESIAN_POINT ( 'NONE',  ( 0.7499999999999885647, 1.597916667349486008, -1.299038105676652899 ) ) ;
#28344 = CARTESIAN_POINT ( 'NONE',  ( 6.252564000042572623, 0.6067452241035797833, 1.828529084590237774 ) ) ;
#28345 = CARTESIAN_POINT ( 'NONE',  ( -1.402160292154681736E-14, 13.42187500034140157, 1.575800808251682339 ) ) ;
#28346 = CARTESIAN_POINT ( 'NONE',  ( 3.691809873939347675, 2.090716244852005357, -0.7509968985505171002 ) ) ;
#28347 = ORIENTED_EDGE ( 'NONE', *, *, #2148, .F. ) ;
#28348 = CARTESIAN_POINT ( 'NONE',  ( -1.402160292154681736E-14, -0.6624999999999758860, -1.732050807568870754 ) ) ;
#28350 = EDGE_CURVE ( 'NONE', #2366, #111968, #84984, .T. ) ;
#28349 = CARTESIAN_POINT ( 'NONE',  ( 7.242026607993941489, 11.60078147596829901, 0.7998128361456462443 ) ) ;
#28351 = CYLINDRICAL_SURFACE ( 'NONE', #7604, 0.3999999999999997446 ) ;
#28352 = CARTESIAN_POINT ( 'NONE',  ( 4.897892112245933127, -0.5929259483795108476, -1.636466244661118452 ) ) ;
#28353 = CARTESIAN_POINT ( 'NONE',  ( 4.932062528313535310, 1.127988425013145779, 1.604980062286972542 ) ) ;
#28355 = CARTESIAN_POINT ( 'NONE',  ( -5.585596099150191840, 7.539614753807099667, -1.443375672974052559 ) ) ;
#28354 = CARTESIAN_POINT ( 'NONE',  ( 3.358669367883368118, 4.941533567329135401, -1.599625672291262513 ) ) ;
#28356 = DIRECTION ( 'NONE',  ( 1.000000000000000000, -0.000000000000000000, -0.000000000000000000 ) ) ;
#28357 = CARTESIAN_POINT ( 'NONE',  ( 5.009165025557245521, 1.964990322317389015, 1.121224042300600576 ) ) ;
#28358 = CARTESIAN_POINT ( 'NONE',  ( 1.961455461422195068, 1.713676499688887800, 1.147740006246004585 ) ) ;
#28359 = CARTESIAN_POINT ( 'NONE',  ( -7.555971681517696936, 7.709721804725773175, 0.7998128361456462443 ) ) ;
#28360 = ORIENTED_EDGE ( 'NONE', *, *, #40097, .F. ) ;
#28362 = ADVANCED_FACE ( 'NONE', ( #200837 ), #102301, .F. ) ;
#28361 = CARTESIAN_POINT ( 'NONE',  ( 1.499999999999989120, 1.785416667349487563, 0.8660254037844524744 ) ) ;
#28363 = CARTESIAN_POINT ( 'NONE',  ( 4.042156614576187579, 1.861303109871172312, 0.1859210194900539903 ) ) ;
#28364 = CARTESIAN_POINT ( 'NONE',  ( 2.953449220662739183, -1.603453536992532902, -0.6609773998737851208 ) ) ;
#28365 = CARTESIAN_POINT ( 'NONE',  ( 6.216381822182693639, 2.044192415450503120, 0.7905562269360306704 ) ) ;
#28366 = CARTESIAN_POINT ( 'NONE',  ( 0.9915960798324228165, 1.945464911009102460, -1.041603813667857370 ) ) ;
#28367 = CARTESIAN_POINT ( 'NONE',  ( 3.661132068870280420, -1.905464569931826446, -1.020879743040298271 ) ) ;
#28368 = CARTESIAN_POINT ( 'NONE',  ( 4.874914055504836696, 1.811399353594527639, -0.7004420144864877962 ) ) ;
#28369 = EDGE_CURVE ( 'NONE', #97972, #102205, #156576, .T. ) ;
#28371 = UNCERTAINTY_MEASURE_WITH_UNIT (LENGTH_MEASURE( 1.000000000000000082E-05 ), #141855, 'distance_accuracy_value', 'NONE');
#28370 = CARTESIAN_POINT ( 'NONE',  ( 11.86239285000045740, 12.22000000000000064, -1.812080536912752837 ) ) ;
#28372 = CARTESIAN_POINT ( 'NONE',  ( -0.08726289061519039436, -1.242903867559573161, -1.588418431006669351 ) ) ;
#28373 = DIRECTION ( 'NONE',  ( 1.000000000000000000, 0.000000000000000000, -0.000000000000000000 ) ) ;
#28374 = DIRECTION ( 'NONE',  ( 0.000000000000000000, 1.000000000000000000, 0.000000000000000000 ) ) ;
#28375 = CARTESIAN_POINT ( 'NONE',  ( 6.258435431136967431, 1.928752767684217106, -0.5880170417187426946 ) ) ;
#28376 = CARTESIAN_POINT ( 'NONE',  ( -8.666686507633592385, 11.13422023037111330, 1.599625672291269396 ) ) ;
#28377 = CARTESIAN_POINT ( 'NONE',  ( 8.444030743212801227, 8.745790710036752458, 0.7998128361456462443 ) ) ;
#28378 = CARTESIAN_POINT ( 'NONE',  ( 11.55950211276791251, 9.719999999999998863, -3.221476510067114329 ) ) ;
#28379 = CARTESIAN_POINT ( 'NONE',  ( 3.123480263227970344, -1.759325740769552393, 0.4874977319994436287 ) ) ;
#28380 = CARTESIAN_POINT ( 'NONE',  ( 2.573496151666111231, 0.1090403232480302298, -2.204208057042057245 ) ) ;
#28381 = ORIENTED_EDGE ( 'NONE', *, *, #89939, .F. ) ;
#28382 = CARTESIAN_POINT ( 'NONE',  ( -5.628043163004235794, 5.738674243025936761, 0.7216878364870257245 ) ) ;
#28383 = CARTESIAN_POINT ( 'NONE',  ( 1.642778471875001811, -2.530208332855374387, 2.845375778867859751 ) ) ;
#28384 = CARTESIAN_POINT ( 'NONE',  ( -6.320072162264675164, 10.52516795595079557, 0.7998128361456481317 ) ) ;
#28385 = CARTESIAN_POINT ( 'NONE',  ( 0.6682303662221461549, 2.017294962401328107, -0.1032846847020176678 ) ) ;
#28386 = CARTESIAN_POINT ( 'NONE',  ( 0.8035760164417544704, 1.868272328500224289, -1.003034915376184388 ) ) ;
#28387 = CARTESIAN_POINT ( 'NONE',  ( 0.7124089920921370389, 15.00000000000000711, -12.66466791154696558 ) ) ;
#28388 = EDGE_LOOP ( 'NONE', ( #159563, #111733, #30659, #133270 ) ) ;
#28389 = CARTESIAN_POINT ( 'NONE',  ( -4.098307573080856692, 8.003385611894792362, 0.7998128361456352531 ) ) ;
#28390 = CARTESIAN_POINT ( 'NONE',  ( 2.166652004499136197, 1.382927810177040584, -1.245475062859234372 ) ) ;
#28391 = STYLED_ITEM ( 'NONE', ( #128509 ), #27868 ) ;
#28392 = CARTESIAN_POINT ( 'NONE',  ( 3.330499290451326200, 7.037332938835193730, -0.7998128361456291469 ) ) ;
#28393 = CARTESIAN_POINT ( 'NONE',  ( 1.024558638192473170, 1.287004556549703693, -1.736669753874709343 ) ) ;
#28394 = CARTESIAN_POINT ( 'NONE',  ( 5.695935454815424848, 1.779625283580280382, 0.9480427965274510482 ) ) ;
#28395 = ORIENTED_EDGE ( 'NONE', *, *, #212736, .F. ) ;
#28396 = ORIENTED_EDGE ( 'NONE', *, *, #95435, .T. ) ;
#28397 = CARTESIAN_POINT ( 'NONE',  ( -10.30827686509187835, 10.92074451889568643, 1.040834085586084257E-14 ) ) ;
#28398 = CARTESIAN_POINT ( 'NONE',  ( 3.580510235063854019, -1.759844519496515325, -0.4856381957471164745 ) ) ;
#28401 = ORIENTED_EDGE ( 'NONE', *, *, #99577, .F. ) ;
#28400 = CARTESIAN_POINT ( 'NONE',  ( -5.194998520284300980, 6.641152480062820551, -1.419077516013200313 ) ) ;
#28399 = CARTESIAN_POINT ( 'NONE',  ( -4.034433228518296666, 6.864533312316751790, -1.199719254218450271 ) ) ;
#28402 = CARTESIAN_POINT ( 'NONE',  ( 6.564609147483420060, 6.793222102749934876, 0.3624652974001541517 ) ) ;
#28403 = CARTESIAN_POINT ( 'NONE',  ( 5.870470189955956819, -0.4925641237488035395, 1.954873771647095415 ) ) ;
#28404 = CARTESIAN_POINT ( 'NONE',  ( 6.105383947169263692, -1.826632712061267094, 0.2301338403083788009 ) ) ;
#28405 = CARTESIAN_POINT ( 'NONE',  ( -0.02319159430947542386, 5.725354828811364705, -2.405035539666657840 ) ) ;
#28406 = CARTESIAN_POINT ( 'NONE',  ( 4.477368160356545168, 0.002844634383740093052, -2.307868969966973438 ) ) ;
#28407 = CARTESIAN_POINT ( 'NONE',  ( 4.369470645354133431, 8.319742529546998000, 0.7998128361456271485 ) ) ;
#28408 = CARTESIAN_POINT ( 'NONE',  ( 6.503215372615936296, 1.793156143535659108, 1.206815395834538451 ) ) ;
#28409 = CARTESIAN_POINT ( 'NONE',  ( 6.174848896020108668, 9.291408581077091000, 1.199719254218460707 ) ) ;
#28410 = CARTESIAN_POINT ( 'NONE',  ( 2.753386078659710190, 1.932462020465589125, -0.1930240951200749566 ) ) ;
#28411 = ORIENTED_EDGE ( 'NONE', *, *, #34950, .F. ) ;
#28412 = CARTESIAN_POINT ( 'NONE',  ( 4.675370021169432455, -0.9774931845568238797, -2.080278028362152032 ) ) ;
#28413 = CARTESIAN_POINT ( 'NONE',  ( 0.1751657365761550289, 0.002452341591364583847, -2.044164811867712483 ) ) ;
#28414 = CARTESIAN_POINT ( 'NONE',  ( -7.937372586157736443, 8.224965870130965584, 0.7998128361456341429 ) ) ;
#28415 = TOROIDAL_SURFACE ( 'NONE', #149470, 11.91999999999999993, 0.08000000000000000167 ) ;
#28416 = CARTESIAN_POINT ( 'NONE',  ( 4.223419137798128276, -1.790188510885984297, 0.5427707113358354318 ) ) ;
#28417 = ORIENTED_EDGE ( 'NONE', *, *, #158884, .T. ) ;
#28420 = CARTESIAN_POINT ( 'NONE',  ( -5.367048706163331850, 7.354919138647580290, -1.599625672291271394 ) ) ;
#28419 = CARTESIAN_POINT ( 'NONE',  ( 1.499999999999987121, 0.8270833340161471980, -0.8660254037844253849 ) ) ;
#28418 = CARTESIAN_POINT ( 'NONE',  ( 2.232540727315056373, 1.246330492051262784, -1.450604739030990187 ) ) ;
#28421 = CARTESIAN_POINT ( 'NONE',  ( 3.721466898765386500, -0.1629207441977159332, 2.200919931280575170 ) ) ;
#28422 = CARTESIAN_POINT ( 'NONE',  ( 6.883263157960418432, 2.078485899884211285, 2.154856264959764012 ) ) ;
#28423 = CARTESIAN_POINT ( 'NONE',  ( -0.2108831679771168421, 7.629137130509075604, -2.497154329497493386 ) ) ;
#28424 = CARTESIAN_POINT ( 'NONE',  ( 5.899206235277530297, 7.015400374979486209, -1.082531754730548412 ) ) ;
#28425 = CARTESIAN_POINT ( 'NONE',  ( -6.916067756302494374, 7.241369601873926420, 0.000000000000000000 ) ) ;
#28426 = CARTESIAN_POINT ( 'NONE',  ( 1.300003668391478406, -1.971530339922975550, -0.004173579811568225127 ) ) ;
#28427 = CARTESIAN_POINT ( 'NONE',  ( 1.325685429717119446, -0.05423940138811130657, 2.307114084963398870 ) ) ;
#28428 = CARTESIAN_POINT ( 'NONE',  ( 2.717183929654675811, -1.705535211757349456, -0.9694657131227711888 ) ) ;
#28429 = CARTESIAN_POINT ( 'NONE',  ( -4.936050443827081580, 7.916420063510339666, 1.199719254218452935 ) ) ;
#28430 = CARTESIAN_POINT ( 'NONE',  ( 5.893442400364165223, -1.866981718288396763, 0.8769185494091299438 ) ) ;
#28431 = CARTESIAN_POINT ( 'NONE',  ( 3.362058906508953449, 6.866226457661676719, -0.7216878364870267237 ) ) ;
#28432 = CARTESIAN_POINT ( 'NONE',  ( 4.854701522145073334, 7.821512988214679218, -1.199719254218450271 ) ) ;
#28433 = EDGE_LOOP ( 'NONE', ( #87024, #72556, #110733, #61974 ) ) ;
#28434 = CARTESIAN_POINT ( 'NONE',  ( 1.499999999999996891, 10.14583333333333570, -0.8660254037844378194 ) ) ;
#28435 = DIRECTION ( 'NONE',  ( 0.000000000000000000, 1.000000000000000000, 0.000000000000000000 ) ) ;
#28436 = CARTESIAN_POINT ( 'NONE',  ( 9.642873567817520808, 12.27310513391906532, 1.599625672291279388 ) ) ;
#28437 = CARTESIAN_POINT ( 'NONE',  ( 1.674930785650229792, 1.460053457903678131, -1.606915656648603141 ) ) ;
#28438 = CARTESIAN_POINT ( 'NONE',  ( 0.000000000000000000, -1.500000000000001332, 0.000000000000000000 ) ) ;
#28439 = EDGE_CURVE ( 'NONE', #185232, #33711, #87119, .T. ) ;
#28440 = LINE ( 'NONE', #97728, #192970 ) ;
#28441 = CARTESIAN_POINT ( 'NONE',  ( 3.040157689216971715, 1.855973101128991054, 0.2326549598439253685 ) ) ;
#28442 = CARTESIAN_POINT ( 'NONE',  ( 6.239563118392394969, -1.560868990211834895, -1.495623836407403262 ) ) ;
#28443 = CIRCLE ( 'NONE', #38950, 1.857347330825974252 ) ;
#28445 = CARTESIAN_POINT ( 'NONE',  ( 6.727182134110222478, 0.005875948494733079785, 1.810970247402940547 ) ) ;
#28444 = CARTESIAN_POINT ( 'NONE',  ( -0.02224634325197898804, 1.983040877609225872, -2.702260234736663325 ) ) ;
#28446 = CARTESIAN_POINT ( 'NONE',  ( 1.364683531249986981, -1.115624999658580752, 0.000000000000000000 ) ) ;
#28447 = CARTESIAN_POINT ( 'NONE',  ( -1.749999999999999778, 2.143131898507868051E-16, 0.000000000000000000 ) ) ;
#28448 = CARTESIAN_POINT ( 'NONE',  ( 2.262237773093742188, 1.911903731097279513, 0.04523801603947830152 ) ) ;
#28449 = CARTESIAN_POINT ( 'NONE',  ( 4.610057705051894494, -0.7578761767026606089, -1.599493228202266470 ) ) ;
#28450 = CARTESIAN_POINT ( 'NONE',  ( 1.875505643822904300, 0.3255412885708880433, -1.884197853084010443 ) ) ;
#28451 = CARTESIAN_POINT ( 'NONE',  ( -4.394814349124112951, 8.279033840620114049, -0.7998128361456281477 ) ) ;
#28452 = CARTESIAN_POINT ( 'NONE',  ( 0.05764063133973944958, 1.105241252117078909, 1.564514492536345891 ) ) ;
#28453 = CARTESIAN_POINT ( 'NONE',  ( -1.402160292154681736E-14, -0.6624999999999758860, -1.732050807568870754 ) ) ;
#28454 = CARTESIAN_POINT ( 'NONE',  ( 0.6079806153083644471, 0.6509857562557037625, -1.965403638620793147 ) ) ;
#28455 = CARTESIAN_POINT ( 'NONE',  ( -1.201851678989727383E-14, 5.337500000000020783, -1.732050807568863648 ) ) ;
#28456 = DIRECTION ( 'NONE',  ( 1.000000000000000000, 0.000000000000000000, -0.000000000000000000 ) ) ;
#28457 = CARTESIAN_POINT ( 'NONE',  ( 5.401189721097995111, 1.529905263132097071, 1.076157610686766075 ) ) ;
#28458 = CARTESIAN_POINT ( 'NONE',  ( 1.752308680507021155, 0.5713779359179693706, 1.734036872924920702 ) ) ;
#28460 = CARTESIAN_POINT ( 'NONE',  ( 4.635702676548680401, 8.322458603728597026, -0.3981331281527732968 ) ) ;
#28459 = CARTESIAN_POINT ( 'NONE',  ( 4.283934280384479543, 1.440456688004333019, 1.672026782002330458 ) ) ;
#28461 = CARTESIAN_POINT ( 'NONE',  ( -1.001543065824772872E-14, 5.384375000341415252, 1.575800808251672791 ) ) ;
#28462 = CARTESIAN_POINT ( 'NONE',  ( 3.455586768955606125, 1.624414792841613941, 1.271063249801159145 ) ) ;
#28463 = B_SPLINE_CURVE_WITH_KNOTS ( 'NONE', 3,
 ( #65616, #113415, #99232, #33151, #14755, #128617 ),
 .UNSPECIFIED., .F., .F.,
 ( 4, 2, 4 ),
 ( 0.000000000000000000, 0.0003129200374289441730, 0.0006258400748578883460 ),
 .UNSPECIFIED. ) ;
#28464 = CARTESIAN_POINT ( 'NONE',  ( -7.181014916732457287, 11.52960116949655678, -0.7998128361456291469 ) ) ;
#28465 = DIRECTION ( 'NONE',  ( 3.491481338843133355E-15, 0.000000000000000000, 1.000000000000000000 ) ) ;
#28466 = CARTESIAN_POINT ( 'NONE',  ( 1.399605654164548296, 3.350766839404967889, -0.07230550894161540121 ) ) ;
#28467 = DIRECTION ( 'NONE',  ( 0.000000000000000000, 1.000000000000000000, 0.000000000000000000 ) ) ;
#28468 = CARTESIAN_POINT ( 'NONE',  ( 6.424584688029230328, 8.588711117491191871, 1.599625672291268286 ) ) ;
#28469 = EDGE_LOOP ( 'NONE', ( #198400, #85054, #56342, #204712, #100510, #163393, #120446 ) ) ;
#28470 = CARTESIAN_POINT ( 'NONE',  ( 5.266107318980479235, -2.060723932065291031, 0.1993833602659672022 ) ) ;
#28471 = CARTESIAN_POINT ( 'NONE',  ( -1.402160292154681736E-14, 0.1343750003414218575, 1.575800808251672791 ) ) ;
#28472 = CARTESIAN_POINT ( 'NONE',  ( 3.128364550451453230, 1.203671540783244565, -1.795256801906938815 ) ) ;
#28473 = CARTESIAN_POINT ( 'NONE',  ( -4.616709804987970678, 8.367809121204862421, 0.2297300046584915267 ) ) ;
#28474 = CARTESIAN_POINT ( 'NONE',  ( 2.736978119973699108, 1.902454848370996210, 0.6784627630139413723 ) ) ;
#28475 = CARTESIAN_POINT ( 'NONE',  ( 6.720655732516647163, 2.019696082639847567, 2.477441386028636394 ) ) ;
#28476 = EDGE_LOOP ( 'NONE', ( #173645, #138257, #162010, #128864, #71602, #67861 ) ) ;
#28479 = CARTESIAN_POINT ( 'NONE',  ( 8.283668668269706714, 8.766627655843892697, 1.040834085586084257E-14 ) ) ;
#28478 = CARTESIAN_POINT ( 'NONE',  ( -1.737500000000000266, -1.808333333333332016, -3.009438278150923907 ) ) ;
#28477 = CARTESIAN_POINT ( 'NONE',  ( 10.53927507717371803, 2.018041202054265071, 6.084853302869627889 ) ) ;
#28480 = CARTESIAN_POINT ( 'NONE',  ( -3.485854892044998543, 6.120562236477518070, -1.082531754730546636 ) ) ;
#28481 = CARTESIAN_POINT ( 'NONE',  ( 1.288296401830712368, -0.7303101666344159471, -1.879802715551846859 ) ) ;
#28483 = CARTESIAN_POINT ( 'NONE',  ( 6.023007056224171762, -2.064090639567913499, 0.7368321019862942300 ) ) ;
#28482 = CARTESIAN_POINT ( 'NONE',  ( -5.687809136132860210, 6.594531066031826150, -1.199719254218446718 ) ) ;
#28484 = CARTESIAN_POINT ( 'NONE',  ( 1.499999999999989120, 5.035416667349487341, 0.8660254037844524744 ) ) ;
#28485 = CARTESIAN_POINT ( 'NONE',  ( 4.763870730211980487, 0.5944114921396548290, -1.817767169311027997 ) ) ;
#28486 = CARTESIAN_POINT ( 'NONE',  ( -4.009460741339347045, 5.700790169694431420, -1.599625672291256295 ) ) ;
#28487 = CARTESIAN_POINT ( 'NONE',  ( 5.788968402910802169, 8.737251655829183505, 1.082531754730558626 ) ) ;
#28489 = CARTESIAN_POINT ( 'NONE',  ( 3.110954007106698338, 0.05231540665236523308, 2.015913653835194719 ) ) ;
#28488 = CARTESIAN_POINT ( 'NONE',  ( -9.178506806327330736, 10.77097469787910455, 1.082531754730558626 ) ) ;
#28490 = CARTESIAN_POINT ( 'NONE',  ( 0.6823417656249934904, 13.75520833367473195, 1.181850606188764807 ) ) ;
#28491 = CARTESIAN_POINT ( 'NONE',  ( -4.516801452008150086, 5.298631777878131111, 1.199719254218452935 ) ) ;
#28492 = CARTESIAN_POINT ( 'NONE',  ( 5.069259022003644866, 0.1660796517843898534, -1.716765078168249969 ) ) ;
#28493 = CARTESIAN_POINT ( 'NONE',  ( 6.363572996767764778, 8.517530811019446091, -1.599625672291283607 ) ) ;
#28494 = CARTESIAN_POINT ( 'NONE',  ( 2.900554798319789906, 5.471398800426671372, 1.199719254218452047 ) ) ;
#28495 = CARTESIAN_POINT ( 'NONE',  ( 10.95308175811721085, 12.30000000000000071, -1.800000000000001155 ) ) ;
#28496 = DIRECTION ( 'NONE',  ( -3.491481338843133750E-15, -0.000000000000000000, -1.000000000000000000 ) ) ;
#28498 = TOROIDAL_SURFACE ( 'NONE', #166873, 0.8299999999999998490, 0.08000000000000000167 ) ;
#28497 = CARTESIAN_POINT ( 'NONE',  ( 0.6376584384039893916, 1.932990051301992418, -0.7417924570976215382 ) ) ;
#28499 = CARTESIAN_POINT ( 'NONE',  ( 6.883263157960362477, -0.004191378316371896506, 2.053658919477070910 ) ) ;
#28500 = ORIENTED_EDGE ( 'NONE', *, *, #38304, .F. ) ;
#28501 = CARTESIAN_POINT ( 'NONE',  ( 6.463521484642490655, -1.459484751789320134, -1.072804587801470921 ) ) ;
#28503 = CARTESIAN_POINT ( 'NONE',  ( 5.071631979963703962, 8.074598522336444262, 1.199719254218451159 ) ) ;
#28502 = TOROIDAL_SURFACE ( 'NONE', #163318, 10.89999999999920632, 0.2000000000000000111 ) ;
#28504 = DIRECTION ( 'NONE',  ( -0.000000000000000000, -1.000000000000000000, -0.000000000000000000 ) ) ;
#28505 = CARTESIAN_POINT ( 'NONE',  ( 0.7909136568654427935, -0.04542554662571558072, -1.811195533156365611 ) ) ;
#28506 = CARTESIAN_POINT ( 'NONE',  ( 4.706088717274896638, 7.544168365912456764, 1.082531754730548412 ) ) ;
#28507 = CARTESIAN_POINT ( 'NONE',  ( 11.08477547810399244, 9.249705336231610175, 4.599939534163192789 ) ) ;
#28508 = CARTESIAN_POINT ( 'NONE',  ( 3.117305861062225958, -2.111875107304355570, 0.5849144002756587746 ) ) ;
#28509 = EDGE_LOOP ( 'NONE', ( #176987, #95263, #69460, #132137 ) ) ;
#28510 = ADVANCED_FACE ( 'NONE', ( #136955 ), #202981, .T. ) ;
#28512 = CARTESIAN_POINT ( 'NONE',  ( 9.752392566931574081, 10.27221283770866300, -0.7998128361456281477 ) ) ;
#28511 = CARTESIAN_POINT ( 'NONE',  ( 0.4319881149899909567, 1.126445828788334991, 1.606065282034954578 ) ) ;
#28513 = CARTESIAN_POINT ( 'NONE',  ( 5.220295459014530515, 1.888029131402849670, 0.3228437444452412763 ) ) ;
#28514 = CARTESIAN_POINT ( 'NONE',  ( -1.500000000000021760, 7.809254910133661909, 3.635752117228817859 ) ) ;
#28515 = CARTESIAN_POINT ( 'NONE',  ( -6.394499343358424959, 6.826875778244118287, 0.5478302896938479494 ) ) ;
#28516 = FACE_OUTER_BOUND ( 'NONE', #112147, .T. ) ;
#28517 = CARTESIAN_POINT ( 'NONE',  ( -1.364683531250000748, -0.4906249996585801409, 0.000000000000000000 ) ) ;
#28519 = ORIENTED_EDGE ( 'NONE', *, *, #74682, .F. ) ;
#28518 = CARTESIAN_POINT ( 'NONE',  ( 5.395781948558860286, 6.357795697149212444, -1.082531754730542195 ) ) ;
#28520 = B_SPLINE_CURVE_WITH_KNOTS ( 'NONE', 3,
 ( #173146, #86540, #54046, #120183 ),
 .UNSPECIFIED., .F., .F.,
 ( 4, 4 ),
 ( 0.000000000000000000, 6.033646489354577163E-05 ),
 .UNSPECIFIED. ) ;
#28521 = CARTESIAN_POINT ( 'NONE',  ( -8.676855123066019360, 11.14608361504227574, -1.443375672974059665 ) ) ;
#28522 = CARTESIAN_POINT ( 'NONE',  ( 2.096749907087645415, -0.5762017740289017143, -2.083436276955972222 ) ) ;
#28523 = CARTESIAN_POINT ( 'NONE',  ( -3.447516199624892419, 7.244129009529488350, 0.7998128361456352531 ) ) ;
#28524 = CARTESIAN_POINT ( 'NONE',  ( 3.984117037569365305, 5.741498858621315371, 1.599625672291261402 ) ) ;
#28525 = CARTESIAN_POINT ( 'NONE',  ( 1.606192798902779328, -0.6535759462080005244, -1.704761432720684144 ) ) ;
#28526 = CARTESIAN_POINT ( 'NONE',  ( 0.1059362375676886209, 1.575662574916199210, 1.419458935296296520 ) ) ;
#28527 = CARTESIAN_POINT ( 'NONE',  ( 4.401258566127845384, 1.466438172381477223, 1.087111955044787859 ) ) ;
#28529 = CARTESIAN_POINT ( 'NONE',  ( 11.62511067571025336, 6.983149424372863123, -1.890548432371299103 ) ) ;
#28528 =( BOUNDED_CURVE ( )  B_SPLINE_CURVE ( 2, ( #210288, #97642, #61928, #81368, #147448 ),
 .UNSPECIFIED., .F., .T. ) 
 B_SPLINE_CURVE_WITH_KNOTS ( ( 3, 2, 3 ),
 ( 0.2458537933072449944, 0.2500000000000000000, 0.2548141018745767039 ),
 .UNSPECIFIED. ) 
 CURVE ( )  GEOMETRIC_REPRESENTATION_ITEM ( )  RATIONAL_B_SPLINE_CURVE ( ( 0.9330143170877186476, 0.9333416359014268249, 1.000000000000000000, 0.9226039174255613595, 0.9346300651406820315 ) ) 
 REPRESENTATION_ITEM ( '' )  );
#28530 = ORIENTED_EDGE ( 'NONE', *, *, #115651, .F. ) ;
#28531 = CARTESIAN_POINT ( 'NONE',  ( 3.560960244297206589, 1.554118163632215444, -1.209804376587125807 ) ) ;
#28532 = ORIENTED_EDGE ( 'NONE', *, *, #73745, .T. ) ;
#28533 = CARTESIAN_POINT ( 'NONE',  ( 6.304245038521663957, 1.436082020041820506, -1.307557180447990186 ) ) ;
#28534 = ORIENTED_EDGE ( 'NONE', *, *, #5768, .T. ) ;
#28535 = CARTESIAN_POINT ( 'NONE',  ( -5.424143973919053785, 8.485862515284315677, 1.199719254218454489 ) ) ;
#28537 = CARTESIAN_POINT ( 'NONE',  ( -0.6125000000000019318, 1.270833334016133076, -1.060881119635938008 ) ) ;
#28536 = CARTESIAN_POINT ( 'NONE',  ( -4.261005416444848315, 8.193199762486115034, 0.7998128361456352531 ) ) ;
#28538 = CARTESIAN_POINT ( 'NONE',  ( 7.309254211098760834, 8.660456346770972758, 1.082531754730549967 ) ) ;
#28540 = EDGE_LOOP ( 'NONE', ( #68633, #118952, #15431, #194700 ) ) ;
#28539 = CARTESIAN_POINT ( 'NONE',  ( 3.633378786761193968, -0.1378984027537045187, 1.907353237798288470 ) ) ;
#28541 = CARTESIAN_POINT ( 'NONE',  ( 5.337709665475443011, 6.539638787446115487, -1.341754179669167213 ) ) ;
#28542 = ADVANCED_FACE ( 'NONE', ( #154267 ), #207394, .T. ) ;
#28543 = CYLINDRICAL_SURFACE ( 'NONE', #149661, 1.500000000000000222 ) ;
#28544 = CARTESIAN_POINT ( 'NONE',  ( 4.577813143269636065, 5.369812084349879555, -1.199719254218450271 ) ) ;
#28545 = AXIS2_PLACEMENT_3D ( 'NONE', #119688, #132710, #116483 ) ;
#28546 = CARTESIAN_POINT ( 'NONE',  ( 5.074862666803740652, -1.456563189067984876, 1.389812660683345191 ) ) ;
#28547 = CARTESIAN_POINT ( 'NONE',  ( 0.1333542156527477984, 0.001576319744088546491, -2.046049510433407548 ) ) ;
#28548 = CARTESIAN_POINT ( 'NONE',  ( 5.848246728868278232, 1.823843535133644389, 0.08496628090458313576 ) ) ;
#28549 = CARTESIAN_POINT ( 'NONE',  ( 0.6079806153083644471, 0.6509857562557037625, -1.965403638620793147 ) ) ;
#28550 = CARTESIAN_POINT ( 'NONE',  ( -8.378575743565381373, 8.877352577022161739, 0.7216878364870438212 ) ) ;
#28551 = CARTESIAN_POINT ( 'NONE',  ( -6.405493493895330737, 6.819705373682535487, -0.5214928506756879578 ) ) ;
#28552 = CARTESIAN_POINT ( 'NONE',  ( -0.3282377607281340426, 2.113835450998172050, 1.224999999999984768 ) ) ;
#28553 = CARTESIAN_POINT ( 'NONE',  ( 6.473518811298506925, 1.789458955665638618, -0.5451884755478533240 ) ) ;
#28554 = CARTESIAN_POINT ( 'NONE',  ( 6.745345117998789775, 7.828323044875442172, 1.199719254218462483 ) ) ;
#28555 = CARTESIAN_POINT ( 'NONE',  ( -3.598799709423620374, 6.286017863381107240, 1.199719254218464037 ) ) ;
#28556 = CYLINDRICAL_SURFACE ( 'NONE', #116874, 0.08000000000000020983 ) ;
#28557 = CARTESIAN_POINT ( 'NONE',  ( 1.364683531249996529, 12.27604166700806054, 0.7879004041258405033 ) ) ;
#28558 = CARTESIAN_POINT ( 'NONE',  ( -5.057354993097396445, 5.859001232490445688, -1.199719254218446718 ) ) ;
#28560 = CARTESIAN_POINT ( 'NONE',  ( -7.957709816578236506, 8.248692638954882028, 0.7998128361456341429 ) ) ;
#28559 = CARTESIAN_POINT ( 'NONE',  ( 1.946706258587953764, 3.753940929402488358, -0.4616008842494966902 ) ) ;
#28561 = CARTESIAN_POINT ( 'NONE',  ( 4.201623210320468260, 1.587898197979008774, 0.6974748919710629380 ) ) ;
#28562 = CIRCLE ( 'NONE', #149630, 11.92000000000000171 ) ;
#28563 = CARTESIAN_POINT ( 'NONE',  ( -5.440899717785814715, 5.242137847038546461, 0.7998128361456341429 ) ) ;
#28564 = VECTOR ( 'NONE', #190529, 1000.000000000000000 ) ;
#28565 = CARTESIAN_POINT ( 'NONE',  ( 1.129834432590616000, 1.996231214973245516, -0.5485114149718294252 ) ) ;
#28566 = CARTESIAN_POINT ( 'NONE',  ( 3.708711176059620751, 2.011172256762243649, 0.6619615953592747903 ) ) ;
#28567 = CARTESIAN_POINT ( 'NONE',  ( 4.517891501851804215, 6.293959390292322986, -1.599625672291255185 ) ) ;
#28568 = CARTESIAN_POINT ( 'NONE',  ( 7.401861798056875053, 10.72292363345333399, -1.199719254218441611 ) ) ;
#28569 = CARTESIAN_POINT ( 'NONE',  ( 0.3999999999999698241, 3.999999999999968914, -0.5000000000000368594 ) ) ;
#28570 = CARTESIAN_POINT ( 'NONE',  ( 0.8308272516417656295, -1.852502698908803591, -0.6688572162713811720 ) ) ;
#28571 = CARTESIAN_POINT ( 'NONE',  ( 4.081185262901700028, 7.719248740676039056, 0.6171906885068592086 ) ) ;
#28572 = CARTESIAN_POINT ( 'NONE',  ( 5.694061328059515148, 5.745419092265303007, -0.7216878364870207285 ) ) ;
#28574 = CARTESIAN_POINT ( 'NONE',  ( 0.000000000000000000, 1.000000000000000888, 0.000000000000000000 ) ) ;
#28573 = CARTESIAN_POINT ( 'NONE',  ( 3.475000000000000533, -2.654166666666666785, 2.006292185433948827 ) ) ;
#28575 = CARTESIAN_POINT ( 'NONE',  ( 3.187719515414323190, -0.9288583595017800842, 2.095805606604860039 ) ) ;
#28576 = CARTESIAN_POINT ( 'NONE',  ( 0.8381832108898427114, 1.798179982845280467, 0.3147962740308178353 ) ) ;
#28577 = CARTESIAN_POINT ( 'NONE',  ( 3.252119977711815491, 0.8557668478980616777, -1.710280963351323846 ) ) ;
#28578 = CARTESIAN_POINT ( 'NONE',  ( 6.852720297064418986, 6.959538199522133262, 0.7998128361456331437 ) ) ;
#28580 = EDGE_CURVE ( 'NONE', #79633, #5587, #107713, .T. ) ;
#28579 = CARTESIAN_POINT ( 'NONE',  ( 6.602457619730767391, 7.765583980183128787, 1.082531754730558626 ) ) ;
#28581 = CARTESIAN_POINT ( 'NONE',  ( -9.345647958521597687, 9.797677461230342999, 0.7998128361456462443 ) ) ;
#28582 = CARTESIAN_POINT ( 'NONE',  ( 2.109637220322407192, 1.559014694980038085, 1.273805747723085746 ) ) ;
#28583 = CARTESIAN_POINT ( 'NONE',  ( 1.938261246079517219, -1.053878627966830184, 1.654468565904606558 ) ) ;
#28584 = CARTESIAN_POINT ( 'NONE',  ( -9.321394304595349567, 10.83371376257142416, 1.199719254218462483 ) ) ;
#28585 = CARTESIAN_POINT ( 'NONE',  ( -7.823218330285243383, 9.085841792542966644, -1.199719254218446718 ) ) ;
#28586 = CARTESIAN_POINT ( 'NONE',  ( -11.45712800319830116, 6.924314249384663889, 3.420032739606327699 ) ) ;
#28588 = CARTESIAN_POINT ( 'NONE',  ( 3.819032205515503708, -0.1302183858614604506, 1.765120429581680916 ) ) ;
#28587 = CARTESIAN_POINT ( 'NONE',  ( 5.542948256250054051, -1.647469546829454234, -1.286982348046373570 ) ) ;
#28589 = CARTESIAN_POINT ( 'NONE',  ( 1.000000047849766815, 15.00000000000000355, 11.64874984998672325 ) ) ;
#28591 = CARTESIAN_POINT ( 'NONE',  ( 0.1116237293282626442, -2.148295633857814746, 0.4319020730012904097 ) ) ;
#28590 =( NAMED_UNIT ( * ) SI_UNIT ( $, .STERADIAN. ) SOLID_ANGLE_UNIT ( ) );
#28592 = CARTESIAN_POINT ( 'NONE',  ( 4.751753191611454596, 0.6700524488352653796, 1.606376638082593455 ) ) ;
#28593 = VECTOR ( 'NONE', #183309, 1000.000000000000114 ) ;
#28594 = CARTESIAN_POINT ( 'NONE',  ( 9.240045382913317340, 10.73880668727576015, -1.199719254218446718 ) ) ;
#28595 = DIRECTION ( 'NONE',  ( 0.000000000000000000, 0.000000000000000000, 1.000000000000000000 ) ) ;
#28596 = CARTESIAN_POINT ( 'NONE',  ( 4.604694260812782325, 0.7408162341489711311, -1.567766963475358599 ) ) ;
#28597 = CARTESIAN_POINT ( 'NONE',  ( 4.352125359537689420, -0.8347222424532302343, 2.004499096949263759 ) ) ;
#28598 = CARTESIAN_POINT ( 'NONE',  ( 2.900554798319789906, 5.471398800426671372, 1.199719254218452047 ) ) ;
#28599 = CARTESIAN_POINT ( 'NONE',  ( 0.5502106600992883179, 1.049441996780882125, 1.838938355043976847 ) ) ;
#28600 = CARTESIAN_POINT ( 'NONE',  ( 5.937500000000004441, 1.451031289060873863, -1.451031289061349927 ) ) ;
#28601 = CARTESIAN_POINT ( 'NONE',  ( 1.499999999999990896, 5.556250000682820378, 1.214306433183764966E-14 ) ) ;
#28602 = CARTESIAN_POINT ( 'NONE',  ( 2.889578633693023590, 1.361086032938205070, 1.363490106525049317 ) ) ;
#28603 = CARTESIAN_POINT ( 'NONE',  ( -0.7500000000000006661, 9.989583334016129967, -1.299038105676657340 ) ) ;
#28604 = CARTESIAN_POINT ( 'NONE',  ( 0.1182595804350913826, -0.5859369620430117109, 2.142582832819041716 ) ) ;
#28605 = ORIENTED_EDGE ( 'NONE', *, *, #184032, .F. ) ;
#28606 = CARTESIAN_POINT ( 'NONE',  ( -0.2411972340275865823, -0.002466136893032512371, -1.900252416837118208 ) ) ;
#28607 = CARTESIAN_POINT ( 'NONE',  ( 1.499999999999987121, 2.545833333333351156, -0.8660254037844262731 ) ) ;
#28608 = CARTESIAN_POINT ( 'NONE',  ( 5.229694566569264680, 7.124396299129368337, 1.599625672291267398 ) ) ;
#28609 = CARTESIAN_POINT ( 'NONE',  ( 2.473529351063200377, -1.934054200746947227, -1.092377531094531173 ) ) ;
#28610 = CARTESIAN_POINT ( 'NONE',  ( 7.131225611108085616, 10.30321839872603462, 1.082531754730558626 ) ) ;
#28611 = CARTESIAN_POINT ( 'NONE',  ( -9.775065565328603157, 11.46695991671396087, -1.082531754730537976 ) ) ;
#28612 = CARTESIAN_POINT ( 'NONE',  ( 5.252858170651868441, 5.093032385374103299, -0.7998128361456481317 ) ) ;
#28613 = CARTESIAN_POINT ( 'NONE',  ( 0.3346115673153668424, 0.6298721381652396811, -1.915601020889952322 ) ) ;
#28615 = CARTESIAN_POINT ( 'NONE',  ( 5.213357787468869020, -1.740689653174596563, -1.106377904087485486 ) ) ;
#28614 = CARTESIAN_POINT ( 'NONE',  ( 8.971744963941056028, 11.49012176272984931, 1.599625672291281386 ) ) ;
#28616 = SURFACE_SIDE_STYLE ('',( #179139 ) ) ;
#28617 = CARTESIAN_POINT ( 'NONE',  ( -4.440459003675619520, 5.139289244831666714, 1.199719254218462483 ) ) ;
#28619 = EDGE_CURVE ( 'NONE', #180436, #179865, #149607, .T. ) ;
#28618 = CARTESIAN_POINT ( 'NONE',  ( 0.7499999999999902300, 5.097916667349482012, -1.299038105676658228 ) ) ;
#28620 = CARTESIAN_POINT ( 'NONE',  ( 1.364683531249986537, 1.655208333674748955, -0.7879004041258239610 ) ) ;
#28621 = CARTESIAN_POINT ( 'NONE',  ( 6.919227945209173392, -0.1346273106918663420, 1.840389347376285345 ) ) ;
#28622 = CARTESIAN_POINT ( 'NONE',  ( 5.502511934227880097, -1.689919030931926969, 0.3883318411201929776 ) ) ;
#28623 = CARTESIAN_POINT ( 'NONE',  ( 5.407646374456077432, -0.7895141955979433357, -1.551160667784831748 ) ) ;
#28624 = CARTESIAN_POINT ( 'NONE',  ( 3.052548088455210973, -1.734419513972422555, 1.498989523525402934 ) ) ;
#28625 = CARTESIAN_POINT ( 'NONE',  ( -0.6823417656250003738, -1.032291666325242607, -1.181850606188749264 ) ) ;
#28626 = CARTESIAN_POINT ( 'NONE',  ( 2.747807751077631977, 0.6205313035267927546, 1.733543155639664990 ) ) ;
#28627 = EDGE_CURVE ( 'NONE', #96195, #89267, #156404, .T. ) ;
#28628 = CARTESIAN_POINT ( 'NONE',  ( 9.073431116043567002, 11.60875560684942265, -1.599625672291262513 ) ) ;
#28629 = CARTESIAN_POINT ( 'NONE',  ( -9.857709926548130497, 3.999999999999961808, -6.855924459378331726 ) ) ;
#28630 = CARTESIAN_POINT ( 'NONE',  ( 2.151128115021032627, -1.464471472660273665, -1.089769533225225073 ) ) ;
#28631 = CARTESIAN_POINT ( 'NONE',  ( 2.215470409936692420, 1.956561601830292485, 0.4872017847364697452 ) ) ;
#28632 = CARTESIAN_POINT ( 'NONE',  ( -4.297571505407598025, 5.076550180139354218, 1.082531754730558626 ) ) ;
#28633 = CARTESIAN_POINT ( 'NONE',  ( 7.434378667490904924, 15.94454736155378960, -9.015675578808581392 ) ) ;
#28634 = CARTESIAN_POINT ( 'NONE',  ( 4.717860591023939953, -2.065837571889141078, 0.4082076317219375250 ) ) ;
#28635 = CARTESIAN_POINT ( 'NONE',  ( -5.388475986427523345, 8.373973519885682393, 1.199719254218452047 ) ) ;
#28636 = CARTESIAN_POINT ( 'NONE',  ( 8.794449440816208607, 13.45178754580079072, 7.697256810998330145 ) ) ;
#28637 = CARTESIAN_POINT ( 'NONE',  ( 2.699741690289765295, -1.532448122638006671, -1.392287113214360827 ) ) ;
#28638 = CARTESIAN_POINT ( 'NONE',  ( 4.379447312414087357, 5.068108938359919158, -1.199719254218452047 ) ) ;
#28639 = CARTESIAN_POINT ( 'NONE',  ( 1.360316468749957597, -0.2239583329919110355, 0.7853790794158921340 ) ) ;
#28640 = CARTESIAN_POINT ( 'NONE',  ( 5.215537505735290402, 1.733765862324820439, 1.220609238144418240 ) ) ;
#28641 = CARTESIAN_POINT ( 'NONE',  ( 6.252569598636129378, 0.5776572744066664766, 1.731972519516040032 ) ) ;
#28642 = ORIENTED_EDGE ( 'NONE', *, *, #100675, .F. ) ;
#28643 = CARTESIAN_POINT ( 'NONE',  ( -4.132202957115018727, 8.042930226601317401, 0.000000000000000000 ) ) ;
#28644 = CARTESIAN_POINT ( 'NONE',  ( 9.480175724453529185, 12.08329098332774265, 1.599625672291279388 ) ) ;
#28645 = CARTESIAN_POINT ( 'NONE',  ( 6.712695452097489301, 7.964471127936110229, -1.082531754730548412 ) ) ;
#28646 = CARTESIAN_POINT ( 'NONE',  ( -3.474999999999998312, -1.677083332377419023, 2.006292185433951047 ) ) ;
#28647 = CARTESIAN_POINT ( 'NONE',  ( -4.771579997005698459, 7.654261532226910525, -1.199719254218452047 ) ) ;
#28648 = CARTESIAN_POINT ( 'NONE',  ( 6.504144398916748671, -0.9053081408615070158, 1.915699539216948688 ) ) ;
#28649 = CARTESIAN_POINT ( 'NONE',  ( 0.9035134896902213830, 1.721610636892715984, 1.212602220121623775 ) ) ;
#28650 = CARTESIAN_POINT ( 'NONE',  ( -4.468294144155606773, 7.370704380560280100, 1.199719254218452935 ) ) ;
#28651 = CARTESIAN_POINT ( 'NONE',  ( 7.892817981449907982, 12.36003807833360391, 0.7998128361456462443 ) ) ;
#28652 = CARTESIAN_POINT ( 'NONE',  ( 5.119887769377023723, 1.841019424034021412, -0.2705144023524996277 ) ) ;
#28653 = CARTESIAN_POINT ( 'NONE',  ( 7.391166297744269365, 11.77477778067701664, 1.040834085586084257E-14 ) ) ;
#28654 = CARTESIAN_POINT ( 'NONE',  ( 4.888763274855682184, 4.911624973226616397, -0.7238686217227735531 ) ) ;
#28655 = EDGE_CURVE ( 'NONE', #205382, #97972, #102687, .T. ) ;
#28656 = CARTESIAN_POINT ( 'NONE',  ( -4.767627293860968507, 5.591261926706423857, -1.199719254218453823 ) ) ;
#28657 = CARTESIAN_POINT ( 'NONE',  ( -2.117044542028253318, 5.621635732341564662, -0.7998128361456281477 ) ) ;
#28658 = AXIS2_PLACEMENT_3D ( 'NONE', #22698, #88810, #157013 ) ;
#28659 = LINE ( 'NONE', #84592, #40504 ) ;
#28661 = CARTESIAN_POINT ( 'NONE',  ( 2.330453122711079850, -1.209328770571056921, 1.544706564130463811 ) ) ;
#28660 = CARTESIAN_POINT ( 'NONE',  ( -7.694415870955439551, 8.935572256658169010, 1.199719254218462483 ) ) ;
#28662 = CARTESIAN_POINT ( 'NONE',  ( 0.8136072859011161951, -0.3160970183575459447, 2.138355382504661506 ) ) ;
#28663 = AXIS2_PLACEMENT_3D ( 'NONE', #103076, #201605, #185370 ) ;
#28665 = CARTESIAN_POINT ( 'NONE',  ( -6.126391799051042142, 6.003160260013642890, 0.2011063304240209848 ) ) ;
#28664 = CARTESIAN_POINT ( 'NONE',  ( -4.773352600463090845, 7.726605912919016106, 1.199719254218452935 ) ) ;
#28666 = CARTESIAN_POINT ( 'NONE',  ( 0.6823417656249882723, 1.426041667008083547, -1.181850606188749264 ) ) ;
#28667 = CARTESIAN_POINT ( 'NONE',  ( 2.829097238278361459, -1.198370081129100262, 1.253277946039689450 ) ) ;
#28668 = CARTESIAN_POINT ( 'NONE',  ( 1.903882329689795094, 1.290680248512179551, -1.167607185883823728 ) ) ;
#28669 = CARTESIAN_POINT ( 'NONE',  ( 6.968527767744093993, 10.11340424813470662, 1.082531754730558626 ) ) ;
#28670 = CARTESIAN_POINT ( 'NONE',  ( -11.52114515671133610, 8.081606464056415362, 2.192706985476595261 ) ) ;
#28671 = CARTESIAN_POINT ( 'NONE',  ( 0.9661724576192336489, 1.646585359754201061, 1.163093122096101162 ) ) ;
#28672 = CARTESIAN_POINT ( 'NONE',  ( 6.825078400183588023, 2.959908325773926041, 2.496992193004472504 ) ) ;
#28673 = CARTESIAN_POINT ( 'NONE',  ( -5.632486471834530661, 5.535932070087196344, -0.7998128361456362523 ) ) ;
#28674 = CARTESIAN_POINT ( 'NONE',  ( 1.393369717069929514, 1.491581312685308580, 1.289216981855696664 ) ) ;
#28676 = CARTESIAN_POINT ( 'NONE',  ( -5.560252395380252288, 7.580323442733986283, 1.443375672974058777 ) ) ;
#28675 = CARTESIAN_POINT ( 'NONE',  ( 5.924064563541377559, -1.897137492723115049, 0.2407653536913647030 ) ) ;
#28677 = CARTESIAN_POINT ( 'NONE',  ( -4.272227801637618505, 7.998366511970260717, 0.7216878364870338292 ) ) ;
#28678 = CARTESIAN_POINT ( 'NONE',  ( 6.282224075085741433, 8.422623735723785643, 1.599625672291268286 ) ) ;
#28679 = CARTESIAN_POINT ( 'NONE',  ( -6.200875153403786477, 8.327716660428123419, -1.599625672291271394 ) ) ;
#28680 = CARTESIAN_POINT ( 'NONE',  ( 1.137374441040917672, -0.04723908312853628000, 2.019287564836816262 ) ) ;
#28681 = FILL_AREA_STYLE ('',( #60105 ) ) ;
#28682 = CARTESIAN_POINT ( 'NONE',  ( 4.067613405475267285, 0.2862205578705340203, -2.289715105617713409 ) ) ;
#28683 = CARTESIAN_POINT ( 'NONE',  ( 6.039501783790233169, 1.813256598412491982, -0.7494862575098264479 ) ) ;
#28684 = CARTESIAN_POINT ( 'NONE',  ( 2.782025223480470544, -1.125517505138178942, -1.606590762409945583 ) ) ;
#28685 = CARTESIAN_POINT ( 'NONE',  ( 7.411503528164766763, 11.79850454950093841, 1.040834085586084257E-14 ) ) ;
#28686 = CARTESIAN_POINT ( 'NONE',  ( -9.568429106646000548, 14.89599861206369624, 7.242208005429680462 ) ) ;
#28687 = EDGE_LOOP ( 'NONE', ( #51695, #113319, #178825, #29932, #103092, #33792, #156090, #136382, #84750, #99321, #107421, #155337, #172513, #53558, #151860, #52043, #120980, #70054 ) ) ;
#28688 = CARTESIAN_POINT ( 'NONE',  ( 1.024788983299034451, 0.4191291695722613730, 2.075291419971446061 ) ) ;
#28690 = CARTESIAN_POINT ( 'NONE',  ( -8.355902744723985975, 8.642974711799791265, 1.040834085586084257E-14 ) ) ;
#28689 = CARTESIAN_POINT ( 'NONE',  ( -4.731959306369413198, 5.479372931307791461, -1.199719254218446718 ) ) ;
#28691 = CARTESIAN_POINT ( 'NONE',  ( 2.325889007780062023, 1.785771638016835361, 0.4476198290149570602 ) ) ;
#28692 = ORIENTED_EDGE ( 'NONE', *, *, #72060, .T. ) ;
#28693 = CARTESIAN_POINT ( 'NONE',  ( 11.57559917528478799, 8.195707862866003168, 2.997126751995791594 ) ) ;
#28694 = CARTESIAN_POINT ( 'NONE',  ( 2.724977724663907530, 1.532976055022855499, -1.465462182430438798 ) ) ;
#28695 = CARTESIAN_POINT ( 'NONE',  ( 0.7499999999999920064, 4.764583334016150751, 1.299038105676669330 ) ) ;
#28696 = CARTESIAN_POINT ( 'NONE',  ( 8.697719238366680372, 10.10609285197134533, 1.199719254218462483 ) ) ;
#28697 = CARTESIAN_POINT ( 'NONE',  ( -1.423205080756851260, 7.980384757729337863, 10.65537363484302524 ) ) ;
#28698 = CARTESIAN_POINT ( 'NONE',  ( 3.514965343742028736, 1.861552560010207191, 0.8843320499443955152 ) ) ;
#28699 = AXIS2_PLACEMENT_3D ( 'NONE', #206231, #76243, #42709 ) ;
#28701 = CARTESIAN_POINT ( 'NONE',  ( 0.2043192855987647494, 1.601443664334546213, 0.9084302959305108338 ) ) ;
#28700 = CARTESIAN_POINT ( 'NONE',  ( -8.701635661872465732, 9.046329781806354831, 1.040834085586084257E-14 ) ) ;
#28702 = CARTESIAN_POINT ( 'NONE',  ( -0.6823417656250212460, 3.801041667008085767, 1.181850606188767472 ) ) ;
#28703 = CARTESIAN_POINT ( 'NONE',  ( -0.02224634325196597762, 7.629137130509080045, -2.889100442546748582 ) ) ;
#28704 = CARTESIAN_POINT ( 'NONE',  ( 1.476571758179666016, 4.272627612153384824, 0.2774774824060997069 ) ) ;
#28705 = CARTESIAN_POINT ( 'NONE',  ( -3.741687207247254676, 7.309126141856352454, 1.040834085586084257E-14 ) ) ;
#28706 = CARTESIAN_POINT ( 'NONE',  ( 2.284789498180723744, -2.218439058979736700, -0.4430748376489759832 ) ) ;
#28707 = CARTESIAN_POINT ( 'NONE',  ( -7.998947442382709383, 12.27592974951444660, 0.7216878364870478180 ) ) ;
#28708 = CARTESIAN_POINT ( 'NONE',  ( 2.689504281738527514, 1.718874962283756691, -0.5722189708131807384 ) ) ;
#28709 = CARTESIAN_POINT ( 'NONE',  ( 2.817496537900533671, -1.290266535947793392, -1.416188432289398058 ) ) ;
#28710 = CARTESIAN_POINT ( 'NONE',  ( 4.176279081494421952, -1.061646348645030713, -1.777293304589353085 ) ) ;
#28711 = CARTESIAN_POINT ( 'NONE',  ( -1.201851678989727383E-14, 3.384375000341421469, 1.575800808251672791 ) ) ;
#28712 = CARTESIAN_POINT ( 'NONE',  ( 2.131653300961271924, -1.286245803994587877, -1.494167145092902160 ) ) ;
#28713 = CARTESIAN_POINT ( 'NONE',  ( 0.2879446430137333479, -0.9113367411649232475, 1.697199823463049428 ) ) ;
#28714 = CARTESIAN_POINT ( 'NONE',  ( 2.834663617355744680, 0.2272019944037397543, 1.856728029318695627 ) ) ;
#28716 = CARTESIAN_POINT ( 'NONE',  ( 4.636584873806110174, 8.438537862545894441, 0.4145994950837776916 ) ) ;
#28715 = CARTESIAN_POINT ( 'NONE',  ( 2.666999619196269045, -1.590435880060107499, 1.672335932400937253 ) ) ;
#28717 = CARTESIAN_POINT ( 'NONE',  ( 2.963170385688845609, 1.570644928931948181, 0.9979875196418576122 ) ) ;
#28718 = CARTESIAN_POINT ( 'NONE',  ( -1.201851678989727383E-14, 3.446875000341421469, -1.575800808251660134 ) ) ;
#28719 = CARTESIAN_POINT ( 'NONE',  ( 6.074688485276667826, 1.387953460639863801, -1.525998863508086778 ) ) ;
#28720 = STYLED_ITEM ( 'NONE', ( #73991 ), #81823 ) ;
#28721 = CARTESIAN_POINT ( 'NONE',  ( -5.063080299699540987, 7.994345218703034384, 1.199719254218464037 ) ) ;
#28722 = CARTESIAN_POINT ( 'NONE',  ( 6.425674737872927089, 9.584038729905381970, -1.199719254218440723 ) ) ;
#28723 = CARTESIAN_POINT ( 'NONE',  ( -1.464817136648365103, 3.470859643012771389, 0.3332976056707414592 ) ) ;
#28724 = CARTESIAN_POINT ( 'NONE',  ( 6.581095821095639842, -0.09928302661296910248, -2.103742297734310984 ) ) ;
#28725 = CARTESIAN_POINT ( 'NONE',  ( -1.364683531249997417, 3.821875000341416584, 1.214306433183764966E-14 ) ) ;
#28726 = CARTESIAN_POINT ( 'NONE',  ( 6.063787883973515314, 2.130759124531961923, -0.3628933549372145295 ) ) ;
#28727 = CARTESIAN_POINT ( 'NONE',  ( 6.270176981224262924, 2.014133449145325105, -0.1505704652167982327 ) ) ;
#28728 = CARTESIAN_POINT ( 'NONE',  ( 1.364683531249986537, -0.3447916663252443836, -0.7879004041258309554 ) ) ;
#28729 = CARTESIAN_POINT ( 'NONE',  ( -4.772106882330241717, 5.630174786549132726, -1.082531754730544860 ) ) ;
#28730 = VECTOR ( 'NONE', #194395, 1000.000000000000000 ) ;
#28733 = CARTESIAN_POINT ( 'NONE',  ( 4.446711195602238931, 6.210915699667823198, -1.443375672974051449 ) ) ;
#28732 = CARTESIAN_POINT ( 'NONE',  ( 6.825078400183572036, 7.053423702906556514, 2.353807037893948628 ) ) ;
#28731 = CARTESIAN_POINT ( 'NONE',  ( 6.875920180786008196, 8.050936961452347163, -1.199719254218452047 ) ) ;
#28734 = CARTESIAN_POINT ( 'NONE',  ( -5.764151584465413869, 6.753873599078290546, -1.199719254218453823 ) ) ;
#28735 = CARTESIAN_POINT ( 'NONE',  ( 4.997279897388729353, -0.2910847460899004258, 1.995267753224789997 ) ) ;
#28736 = CARTESIAN_POINT ( 'NONE',  ( -8.362681821530818738, 8.650883634741092010, -0.7998128361456291469 ) ) ;
#28738 = CARTESIAN_POINT ( 'NONE',  ( -5.912764388891193157, 9.912325863766124456, 0.000000000000000000 ) ) ;
#28737 = CARTESIAN_POINT ( 'NONE',  ( -9.680158490477310806, 10.39586578175276266, 0.7216878364870438212 ) ) ;
#28739 = CARTESIAN_POINT ( 'NONE',  ( -0.7500000000000215383, 4.941666666666684193, 1.299038105676671107 ) ) ;
#28741 = CARTESIAN_POINT ( 'NONE',  ( -0.6823417656250003738, 9.401041667008065872, 1.181850606188754593 ) ) ;
#28740 = CARTESIAN_POINT ( 'NONE',  ( 5.541917325712655717, 0.8799508658935292216, -1.974686638939105343 ) ) ;
#28742 = CARTESIAN_POINT ( 'NONE',  ( -11.80247861663003484, 13.79999999999998295, 1.695431928471866190 ) ) ;
#28743 = CARTESIAN_POINT ( 'NONE',  ( -11.68274454005080365, 7.296694540733708934, -2.750247670129647215 ) ) ;
#28745 = CARTESIAN_POINT ( 'NONE',  ( -0.05329673158829557195, -1.711387015114009369, -0.8607133870397830622 ) ) ;
#28744 = CARTESIAN_POINT ( 'NONE',  ( -5.707619481228814351, 9.602713794834864203, -0.7216878364870207285 ) ) ;
#28746 = CARTESIAN_POINT ( 'NONE',  ( 1.364683531249986537, -0.5739583329919174526, 0.7879004041258500513 ) ) ;
#28747 = CIRCLE ( 'NONE', #25328, 0.08000000000000040412 ) ;
#28748 = CARTESIAN_POINT ( 'NONE',  ( -1.500000000000001110, 8.520833333333337478, 0.8660254037844419273 ) ) ;
#28749 = CARTESIAN_POINT ( 'NONE',  ( 1.523609404914439969, -0.9557964113278711871, -1.435619824176268100 ) ) ;
#28750 = CARTESIAN_POINT ( 'NONE',  ( 7.180978637093494044, 8.406838493811077839, -1.199719254218452047 ) ) ;
#28751 = CARTESIAN_POINT ( 'NONE',  ( 5.773793314573267388, 7.829454515125894964, 1.599625672291268286 ) ) ;
#28752 = CARTESIAN_POINT ( 'NONE',  ( -11.40651083548348765, 7.885881328724557271, -3.736393980786399283 ) ) ;
#28753 = CARTESIAN_POINT ( 'NONE',  ( 1.176598488244801954, -0.03600270464337343435, -1.769546047349578100 ) ) ;
#28754 = CARTESIAN_POINT ( 'NONE',  ( 1.893228294049788207, -0.1010902060475794423, -2.010683160356161014 ) ) ;
#28755 = DIRECTION ( 'NONE',  ( 0.000000000000000000, 1.000000000000000000, 0.000000000000000000 ) ) ;
#28756 = CARTESIAN_POINT ( 'NONE',  ( 3.768774344222697970, -1.483932802477351487, 1.633493490917396151 ) ) ;
#28757 = CARTESIAN_POINT ( 'NONE',  ( 5.489208499878581726, 0.1525156608223678933, 2.165750181564994215 ) ) ;
#28758 = ORIENTED_EDGE ( 'NONE', *, *, #71694, .F. ) ;
#28759 = CARTESIAN_POINT ( 'NONE',  ( -1.402160292154681736E-14, -0.5374999999999753308, 1.732050807568877637 ) ) ;
#28760 = CARTESIAN_POINT ( 'NONE',  ( 7.090551149822722721, 11.21613407486112379, 0.7216878364870438212 ) ) ;
#28762 = CARTESIAN_POINT ( 'NONE',  ( 3.269157808572686896, 1.821735364950356484, -0.8647411805496332260 ) ) ;
#28761 = CARTESIAN_POINT ( 'NONE',  ( 3.299587915756982515, 1.916203934664402198, -0.9084051299479002362 ) ) ;
#28764 = EDGE_LOOP ( 'NONE', ( #199786, #68534, #184604, #14199 ) ) ;
#28763 = CARTESIAN_POINT ( 'NONE',  ( 3.076200346286896536, 0.8185659037078784062, 1.616202036402814901 ) ) ;
#28765 = CARTESIAN_POINT ( 'NONE',  ( 6.550524494058025837, 7.671308660269694712, -1.199719254218452047 ) ) ;
#28766 = ADVANCED_FACE ( 'NONE', ( #155327 ), #68833, .T. ) ;
#28767 = ORIENTED_EDGE ( 'NONE', *, *, #55350, .F. ) ;
#28768 = CARTESIAN_POINT ( 'NONE',  ( 0.4439547499465161251, 1.865322535695708606, 0.1421067652795371117 ) ) ;
#28769 = EDGE_CURVE ( 'NONE', #30840, #100761, #92494, .T. ) ;
#28770 = CARTESIAN_POINT ( 'NONE',  ( 6.823831386379729302, 6.855558127064808716, -0.7998128361456281477 ) ) ;
#28772 = CARTESIAN_POINT ( 'NONE',  ( 1.850665572125685721, -1.753200486404655090, -0.7725721188126480898 ) ) ;
#28771 = CARTESIAN_POINT ( 'NONE',  ( -3.418627288940168096, 7.140148937072163804, -0.7998128361456281477 ) ) ;
#28773 = CARTESIAN_POINT ( 'NONE',  ( 0.1745949693968694705, 0.009193469831055359198, -1.755468632744116242 ) ) ;
#28774 = DIRECTION ( 'NONE',  ( 3.330669073875479482E-16, -3.330669073875479482E-16, -1.000000000000000000 ) ) ;
#28775 = CARTESIAN_POINT ( 'NONE',  ( -1.201851678989727383E-14, 1.634375000341421025, 1.575800808251672791 ) ) ;
#28776 = CARTESIAN_POINT ( 'NONE',  ( 11.86145016429273191, 13.40000000000000036, -1.100000000000002087 ) ) ;
#28777 = CARTESIAN_POINT ( 'NONE',  ( -9.104463846776669200, 10.58062822844965645, -1.199719254218441611 ) ) ;
#28778 = CARTESIAN_POINT ( 'NONE',  ( 5.594645800149128156, -0.5210773734287167391, -2.097845705497362712 ) ) ;
#28779 = CARTESIAN_POINT ( 'NONE',  ( -4.475600106286965918, 8.235634200727838916, 0.7216878364870338292 ) ) ;
#28780 = CARTESIAN_POINT ( 'NONE',  ( -5.264308783856126439, 9.363720357799287797, -0.7998128361456362523 ) ) ;
#28781 = CARTESIAN_POINT ( 'NONE',  ( 3.041385797112206912, 0.05609166564453024750, 2.120036961950934273 ) ) ;
#28783 = CARTESIAN_POINT ( 'NONE',  ( -11.65676533170044138, 6.358709890710655621, 4.978123860300238235 ) ) ;
#28782 = DIRECTION ( 'NONE',  ( 0.000000000000000000, 1.000000000000000000, 0.000000000000000000 ) ) ;
#28784 = CARTESIAN_POINT ( 'NONE',  ( 4.921144022694462272, -0.09977086410491335655, 1.968969177566483042 ) ) ;
#28785 = B_SPLINE_CURVE_WITH_KNOTS ( 'NONE', 3,
 ( #56690, #57753, #140096, #136880, #123913, #120698, #40452, #54551, #206123, #152059 ),
 .UNSPECIFIED., .F., .F.,
 ( 4, 2, 2, 2, 4 ),
 ( 0.000000000000000000, 0.0003777850654088144890, 0.0007555701308176289779, 0.001133355196226443467, 0.001511140261635257956 ),
 .UNSPECIFIED. ) ;
#28786 = ORIENTED_EDGE ( 'NONE', *, *, #197101, .F. ) ;
#28787 = CARTESIAN_POINT ( 'NONE',  ( 5.559793223943660934, 1.263291928365728012, 1.699014672817029892 ) ) ;
#28788 = CARTESIAN_POINT ( 'NONE',  ( -2.075332711124689311, 1.720726420432414860, 11.62496126974821919 ) ) ;
#28789 = CARTESIAN_POINT ( 'NONE',  ( 6.883263157960362477, -0.001323150302089473379, 1.953658984494692330 ) ) ;
#28790 = CARTESIAN_POINT ( 'NONE',  ( 2.554547512858021729, -1.689694153139981392, -0.9569994400411386826 ) ) ;
#28791 = VERTEX_POINT ( 'NONE', #1063 ) ;
#28792 = CARTESIAN_POINT ( 'NONE',  ( 2.288037425052380058, 5.553570322680376314, 0.4296897185159433974 ) ) ;
#28793 = CARTESIAN_POINT ( 'NONE',  ( 5.905458427204159477, 9.047396044116986502, 1.199719254218452047 ) ) ;
#28795 = CARTESIAN_POINT ( 'NONE',  ( 6.388916700537700777, 8.476822122092563916, 1.599625672291281386 ) ) ;
#28794 = CARTESIAN_POINT ( 'NONE',  ( 2.660199397079235695, -1.441175001385604393, 1.514759066650630093 ) ) ;
#28796 = CARTESIAN_POINT ( 'NONE',  ( 8.025500584646550806, 8.327781868367935658, 0.000000000000000000 ) ) ;
#28798 = EDGE_LOOP ( 'NONE', ( #124667, #158765, #166217, #77754 ) ) ;
#28797 = CARTESIAN_POINT ( 'NONE',  ( -0.005635951793048382327, -1.756493610686832740, -0.4425278525194314971 ) ) ;
#28799 = CARTESIAN_POINT ( 'NONE',  ( 4.178501018151202118, -1.271701901513167421, 1.803451139310302986 ) ) ;
#28800 = CARTESIAN_POINT ( 'NONE',  ( 2.784424029790978139, -1.135345490304447091, 1.892179603154810819 ) ) ;
#28801 = CARTESIAN_POINT ( 'NONE',  ( 8.769426429940780920, 9.125419011219408461, 0.7998128361456462443 ) ) ;
#28802 = CARTESIAN_POINT ( 'NONE',  ( -11.80235830595197655, 12.29999999999998295, 1.696088231482817399 ) ) ;
#28803 = CARTESIAN_POINT ( 'NONE',  ( 1.418461073652961257, -0.6892283116659430053, -1.783923526276688154 ) ) ;
#28804 = CARTESIAN_POINT ( 'NONE',  ( 9.260382613333817403, 10.76253345609967660, -1.199719254218446718 ) ) ;
#28805 = CARTESIAN_POINT ( 'NONE',  ( 5.230950013807261989, -1.948248037745937022, -0.7008574099531189594 ) ) ;
#28806 = CIRCLE ( 'NONE', #180938, 0.07999999999999940492 ) ;
#28808 = CARTESIAN_POINT ( 'NONE',  ( 3.204151765443470357, -2.159293047372488950, 0.1044485798024074874 ) ) ;
#28807 = CARTESIAN_POINT ( 'NONE',  ( 0.3107038660269477726, -6.804704122739857475, 10.86205067566995552 ) ) ;
#28809 = CARTESIAN_POINT ( 'NONE',  ( 4.546525781634036534, -1.759932548463913671, 1.305750774140898685 ) ) ;
#28810 = ORIENTED_EDGE ( 'NONE', *, *, #120432, .F. ) ;
#28811 = CARTESIAN_POINT ( 'NONE',  ( -1.499999999999997780, 6.344000000000043826, -2.958666666666662337 ) ) ;
#28812 = CARTESIAN_POINT ( 'NONE',  ( 6.076298462418691315, 7.128931413452940014, -1.143247356662546732 ) ) ;
#28813 = CARTESIAN_POINT ( 'NONE',  ( -0.004619473214107579565, 7.151453204069600389, 1.999995854215794511 ) ) ;
#28814 = CARTESIAN_POINT ( 'NONE',  ( 5.631432701629774051, 7.663367133358481631, 1.599625672291269396 ) ) ;
#28815 = CARTESIAN_POINT ( 'NONE',  ( 1.642778471875000035, -2.763541666188709556, -2.845375778867859751 ) ) ;
#28816 = CARTESIAN_POINT ( 'NONE',  ( -4.329849954717889915, 6.144853928627882489, 1.599625672291270506 ) ) ;
#28817 = CARTESIAN_POINT ( 'NONE',  ( 0.7389079861009685279, 2.013985778099684154, -0.1017531103126300962 ) ) ;
#28818 = CARTESIAN_POINT ( 'NONE',  ( -9.829298180227631576, 10.56986208646148384, 1.040834085586084257E-14 ) ) ;
#28819 = CARTESIAN_POINT ( 'NONE',  ( 5.143339171537801846, 7.093924681584509173, 1.599625672291269396 ) ) ;
#28820 = CARTESIAN_POINT ( 'NONE',  ( 4.750872686184268723, -0.4484009487188305165, -2.020967519627144604 ) ) ;
#28821 = CARTESIAN_POINT ( 'NONE',  ( 2.824735624865559735, 1.814154213653540237, 0.6486305857245775464 ) ) ;
#28822 = CARTESIAN_POINT ( 'NONE',  ( 0.08751785467620704084, -0.5350655163729299835, 1.944078888069140865 ) ) ;
#28823 = CARTESIAN_POINT ( 'NONE',  ( 4.798696304233017074, 7.685897223992134819, -1.199719254218452047 ) ) ;
#28824 = CARTESIAN_POINT ( 'NONE',  ( 3.573067284968055812, 1.778583338327298646, 0.8461400097728142278 ) ) ;
#28825 = CARTESIAN_POINT ( 'NONE',  ( 0.2698121887318750689, 1.265274936352598134, 1.789097752032620114 ) ) ;
#28826 = CARTESIAN_POINT ( 'NONE',  ( 4.441915170580639227, 0.7783198120194650960, -1.651611053696280695 ) ) ;
#28827 = CARTESIAN_POINT ( 'NONE',  ( 6.455090533882185788, 8.624301270986276080, -1.443375672974078761 ) ) ;
#28829 = EDGE_CURVE ( 'NONE', #184758, #167216, #141483, .T. ) ;
#28828 = CARTESIAN_POINT ( 'NONE',  ( 4.053524740361575063, 4.791828954252362216, -1.082531754730543083 ) ) ;
#28830 = CARTESIAN_POINT ( 'NONE',  ( -4.959250327548641479, 9.007818825440551791, -0.7998128361456362523 ) ) ;
#28831 = CARTESIAN_POINT ( 'NONE',  ( 5.662465432362883355, 6.635239754958710989, 1.199719254218451159 ) ) ;
#28832 = ORIENTED_EDGE ( 'NONE', *, *, #186592, .T. ) ;
#28834 = CARTESIAN_POINT ( 'NONE',  ( 4.799092303436800933, -0.2508153390233992530, -1.997484173059483892 ) ) ;
#28833 = CARTESIAN_POINT ( 'NONE',  ( 1.241482983173985533, 1.839155304979672501, 0.08999620058360720265 ) ) ;
#28835 = CARTESIAN_POINT ( 'NONE',  ( 0.4569821463788895644, 1.705326812283548765, 1.541052590308614745 ) ) ;
#28836 = CARTESIAN_POINT ( 'NONE',  ( 4.979329090789969214, -0.1002203015587413149, 1.959344625532564610 ) ) ;
#28837 = CARTESIAN_POINT ( 'NONE',  ( -6.205881626753225966, 8.263281202677319470, 1.599625672291283607 ) ) ;
#28838 = CARTESIAN_POINT ( 'NONE',  ( -6.042630808230841359E-15, -1.968749999044084875, 3.474999999999999645 ) ) ;
#28839 = CARTESIAN_POINT ( 'NONE',  ( -2.300079615812729905, 5.835176651756807331, -0.7998128361456281477 ) ) ;
#28840 = DIRECTION ( 'NONE',  ( 1.000000000000000000, -0.000000000000000000, -0.000000000000000000 ) ) ;
#28841 = CARTESIAN_POINT ( 'NONE',  ( -5.957882158562513908, 5.915560371269843465, -0.7998128361456362523 ) ) ;
#28843 = CARTESIAN_POINT ( 'NONE',  ( 6.438360790777991838, 1.751285973423050368, 0.2548140705225035441 ) ) ;
#28842 = CARTESIAN_POINT ( 'NONE',  ( 1.347338520094189862, 0.6037249722931283813, -2.001697839036377324 ) ) ;
#28844 = CARTESIAN_POINT ( 'NONE',  ( 0.006800380015298257419, 7.009756401597622144, -1.999988438674496383 ) ) ;
#28845 = CARTESIAN_POINT ( 'NONE',  ( -0.1104750535120268828, 5.720715034752038797, -2.697548938405624597 ) ) ;
#28846 = CARTESIAN_POINT ( 'NONE',  ( 2.260927701655718103, 1.706565837815830822, -0.3407169315452397984 ) ) ;
#28847 = CARTESIAN_POINT ( 'NONE',  ( 6.449928391799196525, 8.548002428564306143, -1.599625672291262513 ) ) ;
#28849 = DIRECTION ( 'NONE',  ( 0.000000000000000000, 0.000000000000000000, 1.000000000000000000 ) ) ;
#28848 = DIRECTION ( 'NONE',  ( 0.000000000000000000, -1.000000000000000000, 0.000000000000000000 ) ) ;
#28850 = CARTESIAN_POINT ( 'NONE',  ( 1.892754278755165664, 1.501794282950255965, -0.8482797957840328973 ) ) ;
#28852 = ADVANCED_FACE ( 'NONE', ( #93550 ), #146312, .F. ) ;
#28851 = CARTESIAN_POINT ( 'NONE',  ( 1.558417602779540889, -1.546676288433556756, 1.552911753681482487 ) ) ;
#28853 = CARTESIAN_POINT ( 'NONE',  ( 4.196070124731249074, -0.8457972711899945928, 2.038567251995755836 ) ) ;
#28854 = FACE_OUTER_BOUND ( 'NONE', #111653, .T. ) ;
#28855 = CARTESIAN_POINT ( 'NONE',  ( 2.114367463569406080, 2.165448829365283157, -0.1565315255437193243 ) ) ;
#28856 = CARTESIAN_POINT ( 'NONE',  ( 0.5920835508136900183, -1.811502216344462735, -0.2265648652611390590 ) ) ;
#28857 = CARTESIAN_POINT ( 'NONE',  ( 3.345011933649364444, -1.869310496227539531, -0.9943253416123465360 ) ) ;
#28858 = CARTESIAN_POINT ( 'NONE',  ( 6.639320575229278099, 0.5905802482995252678, 1.949996947996739172 ) ) ;
#28859 = ORIENTED_EDGE ( 'NONE', *, *, #99914, .T. ) ;
#28861 = CARTESIAN_POINT ( 'NONE',  ( 0.6823417656249882723, -0.01145833299191073573, -1.181850606188749264 ) ) ;
#28860 = CARTESIAN_POINT ( 'NONE',  ( 3.948992478018618080, -1.906111675684089901, -1.273188117731700597 ) ) ;
#28862 = CARTESIAN_POINT ( 'NONE',  ( 1.874158809982156670, 3.299964346911599122, 0.3999999999999681033 ) ) ;
#28863 = CARTESIAN_POINT ( 'NONE',  ( 2.842405760359353106, 6.467890487061221272, -0.7998128361456291469 ) ) ;
#28864 = CARTESIAN_POINT ( 'NONE',  ( 5.988988838570013407, -2.108473666775429134, -0.6992015888120094447 ) ) ;
#28865 = CARTESIAN_POINT ( 'NONE',  ( -6.236387472606153892, 8.298871356172400127, -1.443375672974059665 ) ) ;
#28866 = CARTESIAN_POINT ( 'NONE',  ( 5.517805331081858888, 5.539787095791365523, 1.040834085586084257E-14 ) ) ;
#28867 = COLOUR_RGB ( '', 0.40784314, 0.44705882, 0.49803922) ;
#28868 = B_SPLINE_CURVE_WITH_KNOTS ( 'NONE', 3,
 ( #63901, #31416, #196051, #131103, #179797, #81219, #115907, #113794 ),
 .UNSPECIFIED., .F., .F.,
 ( 4, 2, 2, 4 ),
 ( 0.000000000000000000, 0.0004365159022973243174, 0.0006547738534459874790, 0.0008730318045946505864 ),
 .UNSPECIFIED. ) ;
#28869 = CARTESIAN_POINT ( 'NONE',  ( -7.415946836550729948, 9.675023947441092176, 1.443375672974090751 ) ) ;
#28870 = CARTESIAN_POINT ( 'NONE',  ( 5.424670859243587273, 5.501406555305196733, -0.7216878364870458196 ) ) ;
#28871 = ORIENTED_EDGE ( 'NONE', *, *, #97685, .T. ) ;
#28872 = CARTESIAN_POINT ( 'NONE',  ( 4.518204034511161815, -1.842447959940773705, 0.8197716922626956393 ) ) ;
#28874 = CARTESIAN_POINT ( 'NONE',  ( 2.079038939659454854, 1.922984332675440777, 0.7462749415493277194 ) ) ;
#28873 = CARTESIAN_POINT ( 'NONE',  ( 6.661133543015731462, 6.665743976473484267, -0.7998128361456281477 ) ) ;
#28875 = DIRECTION ( 'NONE',  ( -0.0006885664517736270196, 0.9962285034897218061, 0.08676574618402708994 ) ) ;
#28876 = CARTESIAN_POINT ( 'NONE',  ( 4.543390873910906791, 6.393985001019784953, 1.443375672974065660 ) ) ;
#28877 = AXIS2_PLACEMENT_3D ( 'NONE', #59612, #125768, #11921 ) ;
#28879 = EDGE_CURVE ( 'NONE', #56474, #79244, #1137, .T. ) ;
#28878 = CARTESIAN_POINT ( 'NONE',  ( -1.642778471875000035, -2.967708332855374831, -2.845375778867859751 ) ) ;
#28880 = CARTESIAN_POINT ( 'NONE',  ( -1.364683531250010295, 5.238541667008086655, -0.7879004041258300672 ) ) ;
#28881 = CARTESIAN_POINT ( 'NONE',  ( 5.419949545929089396, 1.307550890958172785, -1.758484179531449421 ) ) ;
#28882 = CARTESIAN_POINT ( 'NONE',  ( 2.813125141109920069, 1.117832431973438734, -1.678005364621336426 ) ) ;
#28883 = CARTESIAN_POINT ( 'NONE',  ( 2.436835438956724165, -1.365703447793526371, -1.235134912642745775 ) ) ;
#28884 = EDGE_CURVE ( 'NONE', #113279, #68165, #67128, .T. ) ;
#28885 = CARTESIAN_POINT ( 'NONE',  ( 5.472687561410540802, 9.536552588287639409, 0.7998128361456462443 ) ) ;
#28886 = CARTESIAN_POINT ( 'NONE',  ( 5.385714059857480862, 1.227405483141888132, 1.351559456777707835 ) ) ;
#28887 = VECTOR ( 'NONE', #23320, 999.9999999999998863 ) ;
#28888 = CARTESIAN_POINT ( 'NONE',  ( 6.065077313367789102, -1.076319894221990259, 1.704936797084610101 ) ) ;
#28889 = CARTESIAN_POINT ( 'NONE',  ( -6.852756576703439961, 10.08230087520760954, 1.199719254218453823 ) ) ;
#28891 = CARTESIAN_POINT ( 'NONE',  ( -5.387385936583832802, 7.378645907471495846, -1.599625672291271394 ) ) ;
#28890 = CARTESIAN_POINT ( 'NONE',  ( 6.034080775264698993, 1.121385855563570288, -1.965008656891243044 ) ) ;
#28892 = CARTESIAN_POINT ( 'NONE',  ( 0.4343773424168140274, 1.080651816385242547, -1.807535387385241776 ) ) ;
#28893 = CARTESIAN_POINT ( 'NONE',  ( -5.413448473606448985, 9.537716662508005427, 0.000000000000000000 ) ) ;
#28894 = CARTESIAN_POINT ( 'NONE',  ( 7.130698725783555680, 10.40656671580112658, 1.199719254218460707 ) ) ;
#28895 = CARTESIAN_POINT ( 'NONE',  ( 7.634649897826744080, 9.040084647953621655, 1.082531754730549078 ) ) ;
#28896 = DIRECTION ( 'NONE',  ( 1.000000000000000000, 0.000000000000000000, 0.000000000000000000 ) ) ;
#28897 = CARTESIAN_POINT ( 'NONE',  ( -8.202846631467911820, 9.528741477256060577, 1.199719254218462483 ) ) ;
#28898 = LINE ( 'NONE', #43037, #2493 ) ;
#28899 = CARTESIAN_POINT ( 'NONE',  ( 8.066738210006692000, 8.513542121203711233, 0.7216878364870458196 ) ) ;
#28900 = CARTESIAN_POINT ( 'NONE',  ( 4.046752668985390322, 7.764364035880440440, -0.4786816536347000550 ) ) ;
#28901 = CARTESIAN_POINT ( 'NONE',  ( -9.815740026613967828, 10.55404424057886636, -0.7216878364870267237 ) ) ;
#28903 = CARTESIAN_POINT ( 'NONE',  ( 2.865722905416301369, -1.818493784693291815, -1.275605581943892730 ) ) ;
#28902 = CARTESIAN_POINT ( 'NONE',  ( 1.600013431492643745, 1.466117565985028515, 1.532352819790145482 ) ) ;
#28904 = CARTESIAN_POINT ( 'NONE',  ( -0.3585786437627347389, 3.975028841772314969, 0.9637995837462216553 ) ) ;
#28905 = CARTESIAN_POINT ( 'NONE',  ( -5.906512197408906317, 6.919960980845699439, -1.199719254218453823 ) ) ;
#28906 = CARTESIAN_POINT ( 'NONE',  ( 5.286789834324991055, 8.255339675766103724, -1.199719254218452935 ) ) ;
#28907 = CARTESIAN_POINT ( 'NONE',  ( 3.877359892829432386, -0.1466975079335990917, 1.956454564409334296 ) ) ;
#28908 = CARTESIAN_POINT ( 'NONE',  ( 8.218213668177886788, 12.73966637951625813, 0.7998128361456462443 ) ) ;
#28909 = CARTESIAN_POINT ( 'NONE',  ( -4.525130642185515306, 7.025754810433701536, 1.158151338111103046 ) ) ;
#28910 = CARTESIAN_POINT ( 'NONE',  ( 3.551346171775753735, 6.230655402791975384, 1.199719254218462483 ) ) ;
#28911 = CARTESIAN_POINT ( 'NONE',  ( -3.662110889467009578, 7.286563447771212232, 0.7216878364870338292 ) ) ;
#28913 = EDGE_LOOP ( 'NONE', ( #3607, #6077, #149219, #136596, #24777 ) ) ;
#28912 = CARTESIAN_POINT ( 'NONE',  ( -6.317736394288148816, 8.393778431468064127, 1.443375672974078761 ) ) ;
#28914 = CARTESIAN_POINT ( 'NONE',  ( 3.498385214435925317, -1.041973313016024472, 1.846846941210858351 ) ) ;
#28915 = CARTESIAN_POINT ( 'NONE',  ( -6.283277845290492714, 6.295188672452495915, -0.7998128361456362523 ) ) ;
#28916 = CARTESIAN_POINT ( 'NONE',  ( 4.329101982860062314, 0.1031891237209987822, 2.159356164053369387 ) ) ;
#28917 = CARTESIAN_POINT ( 'NONE',  ( 3.438839575862782549, -1.396446551253815782, -1.200180114512699792 ) ) ;
#28918 = CARTESIAN_POINT ( 'NONE',  ( -4.322081814030608982, 7.236479734952984799, 0.9908985150933833363 ) ) ;
#28919 = CARTESIAN_POINT ( 'NONE',  ( 0.6823417656249882723, 0.7385416670080829915, -1.181850606188749264 ) ) ;
#28920 = CARTESIAN_POINT ( 'NONE',  ( 5.261534320672216936, 0.8623632012556389226, 1.511560460804670880 ) ) ;
#28921 = CARTESIAN_POINT ( 'NONE',  ( 0.4999999999999900080, 3.949999999999974420, 0.4999999999999640288 ) ) ;
#28922 = CARTESIAN_POINT ( 'NONE',  ( 3.714570900464269076, 7.277490450609545469, 0.7216878364870298324 ) ) ;
#28923 = CARTESIAN_POINT ( 'NONE',  ( 10.95308175811721085, 9.799999999999998934, -1.800000000000001155 ) ) ;
#28924 = CARTESIAN_POINT ( 'NONE',  ( 3.538091169922503276, 0.9737216987566952309, -1.930062384640649054 ) ) ;
#28925 = CARTESIAN_POINT ( 'NONE',  ( 6.186875009713125984, -1.117664052418202658, -1.677746505241828334 ) ) ;
#28926 = CARTESIAN_POINT ( 'NONE',  ( -8.148087131688679818, 12.44992605370473804, -0.7216878364870267237 ) ) ;
#28927 = CARTESIAN_POINT ( 'NONE',  ( 2.219795081190904629, -2.096929600374438429, 0.5247480557022954351 ) ) ;
#28928 =( BOUNDED_CURVE ( )  B_SPLINE_CURVE ( 2, ( #128943, #96387, #14014, #192771, #146204 ),
 .UNSPECIFIED., .F., .T. ) 
 B_SPLINE_CURVE_WITH_KNOTS ( ( 3, 2, 3 ),
 ( 0.04818853575335232259, 0.05000000000000000278, 0.05151109858792213281 ),
 .UNSPECIFIED. ) 
 CURVE ( )  GEOMETRIC_REPRESENTATION_ITEM ( )  RATIONAL_B_SPLINE_CURVE ( ( 0.9544155427547809101, 0.9708771770795741052, 1.000000000000000000, 0.9757061412209473428, 0.9602227822089841602 ) ) 
 REPRESENTATION_ITEM ( '' )  );
#28929 = CARTESIAN_POINT ( 'NONE',  ( 3.971915101536928283, 1.092440305464415840, 1.640793377567103528 ) ) ;
#28930 =( NAMED_UNIT ( * ) SI_UNIT ( $, .STERADIAN. ) SOLID_ANGLE_UNIT ( ) );
#28931 = CARTESIAN_POINT ( 'NONE',  ( 4.704598389810739079, 1.691404259434112767, 0.9541841752371772456 ) ) ;
#28934 = ORIENTED_EDGE ( 'NONE', *, *, #201067, .F. ) ;
#28933 = LINE ( 'NONE', #80880, #39327 ) ;
#28932 = CARTESIAN_POINT ( 'NONE',  ( -9.286972035236635392, 9.937148250638648150, -0.7216878364870267237 ) ) ;
#28935 = CARTESIAN_POINT ( 'NONE',  ( -7.293360289508603600, 7.473618190706972086, 0.000000000000000000 ) ) ;
#28936 = DIRECTION ( 'NONE',  ( 0.6507913734559658270, -0.7592566023652989049, 0.000000000000000000 ) ) ;
#28938 = ORIENTED_EDGE ( 'NONE', *, *, #40321, .T. ) ;
#28937 = CARTESIAN_POINT ( 'NONE',  ( -4.034433228518296666, 6.864533312316751790, -1.199719254218450271 ) ) ;
#28939 = CARTESIAN_POINT ( 'NONE',  ( -8.798878505144658746, 10.32807501316600884, -1.082531754730543083 ) ) ;
#28940 = CARTESIAN_POINT ( 'NONE',  ( 2.749284697512776710, -1.835294401387000285, 1.225074929180599792 ) ) ;
#28941 = CARTESIAN_POINT ( 'NONE',  ( -3.285556943750000070, -1.859374999522041882, 0.000000000000000000 ) ) ;
#28942 = CARTESIAN_POINT ( 'NONE',  ( 5.963715375765575644, -0.4800653121489819042, 1.901962685674676301 ) ) ;
#28943 = CARTESIAN_POINT ( 'NONE',  ( -1.364683531249997417, 5.821875000341418804, 1.214306433183764966E-14 ) ) ;
#28944 = CARTESIAN_POINT ( 'NONE',  ( 0.7499999999999902300, 3.764583334016149863, 1.299038105676669330 ) ) ;
#28945 = CARTESIAN_POINT ( 'NONE',  ( 4.912861335034773624, 6.872882102868723919, -1.423633489635463878 ) ) ;
#28946 = CARTESIAN_POINT ( 'NONE',  ( 0.07479286986305544449, 2.046156589154801253, -2.272744413733415403 ) ) ;
#28947 = CARTESIAN_POINT ( 'NONE',  ( 5.824118960990139371, 1.775556191179916699, 0.4867722729226392486 ) ) ;
#28948 = VERTEX_POINT ( 'NONE', #98605 ) ;
#28949 = CARTESIAN_POINT ( 'NONE',  ( -1.360316468750040642, -0.3802083329919277999, -0.7853790794159161148 ) ) ;
#28950 = CARTESIAN_POINT ( 'NONE',  ( -8.179646747746328828, 8.437342715325849341, -0.7998128361456291469 ) ) ;
#28951 = CARTESIAN_POINT ( 'NONE',  ( -1.499999999999997780, 6.280000000000042881, -2.499999999999995115 ) ) ;
#28952 = CARTESIAN_POINT ( 'NONE',  ( 6.099870585610251084, 1.463495690422533579, 1.534846084132005961 ) ) ;
#28953 = CARTESIAN_POINT ( 'NONE',  ( -2.370092853298476854, -0.1904551827020759536, -0.4476525039842733644 ) ) ;
#28954 = CARTESIAN_POINT ( 'NONE',  ( 4.660252114795294887, 6.460046772059735432, -1.599625672291256295 ) ) ;
#28955 = CARTESIAN_POINT ( 'NONE',  ( 6.555941810938458403, 2.055592219362284201, -0.1468124517445909549 ) ) ;
#28958 = CARTESIAN_POINT ( 'NONE',  ( 3.843160323004328305, 0.6166970922517557296, -1.735048075492843456 ) ) ;
#28957 = CARTESIAN_POINT ( 'NONE',  ( 1.750234856725553900, -1.851685525784763975, -0.1866200871585097509 ) ) ;
#28956 = CARTESIAN_POINT ( 'NONE',  ( -9.926723642588102692, -7.126685749119995528, 0.000000000000000000 ) ) ;
#28959 = CARTESIAN_POINT ( 'NONE',  ( 7.904567251967224095, 9.180748867838630645, 1.199719254218462483 ) ) ;
#28960 = CARTESIAN_POINT ( 'NONE',  ( 1.499999999999990896, 3.556250000682818602, 1.214306433183764966E-14 ) ) ;
#28961 =( GEOMETRIC_REPRESENTATION_CONTEXT ( 3 ) GLOBAL_UNCERTAINTY_ASSIGNED_CONTEXT ( ( #177832 ) ) GLOBAL_UNIT_ASSIGNED_CONTEXT ( ( #82587, #242, #184350 ) ) REPRESENTATION_CONTEXT ( 'NONE', 'WORKASPACE' ) );
#28962 = CARTESIAN_POINT ( 'NONE',  ( -5.596483547390937119, 9.751257581923240991, 0.000000000000000000 ) ) ;
#28964 = ORIENTED_EDGE ( 'NONE', *, *, #32928, .T. ) ;
#28963 = CARTESIAN_POINT ( 'NONE',  ( -1.500000000000001110, 10.52083333333333037, 0.8660254037844418162 ) ) ;
#28965 = CIRCLE ( 'NONE', #156990, 0.5000000000000006661 ) ;
#28966 = CARTESIAN_POINT ( 'NONE',  ( 3.580891165198408110, -2.126768340858419926, -0.5889919780145411732 ) ) ;
#28967 = CARTESIAN_POINT ( 'NONE',  ( 5.694667785318580755, -0.5416461603767928068, -2.196524604246933521 ) ) ;
#28968 = CARTESIAN_POINT ( 'NONE',  ( -7.076992996653451939, 7.358839372291564374, 0.7216878364870317197 ) ) ;
#28969 = CARTESIAN_POINT ( 'NONE',  ( 5.379120748016958053, -1.641329381114923658, -0.7670206631310432233 ) ) ;
#28970 = CARTESIAN_POINT ( 'NONE',  ( 6.192599819808762618, 1.414433556397393543, -1.292206900294754490 ) ) ;
#28971 = CARTESIAN_POINT ( 'NONE',  ( 0.4655551865852050608, -8.176568542494919711, 9.512045263456268884 ) ) ;
#28972 = CARTESIAN_POINT ( 'NONE',  ( 5.998880656844745474, 1.528293836345222312, -1.078463600801618405 ) ) ;
#28973 = CARTESIAN_POINT ( 'NONE',  ( 5.654919265238161685, 0.3773621422162172223, 1.874504418562010999 ) ) ;
#28974 = DIRECTION ( 'NONE',  ( 0.7592566023653005702, 0.6507913734559639396, 0.000000000000000000 ) ) ;
#28976 = AXIS2_PLACEMENT_3D ( 'NONE', #194619, #176258, #30002 ) ;
#28975 = CARTESIAN_POINT ( 'NONE',  ( 1.094370286708164386, -0.4508366001288487412, -1.815394955969009239 ) ) ;
#28977 = CARTESIAN_POINT ( 'NONE',  ( 1.745327705122714956, 0.3399549603602426417, -1.987498286102694411 ) ) ;
#28979 = CARTESIAN_POINT ( 'NONE',  ( 3.299542427861827498, 1.660325518240006071, 1.295591914420061830 ) ) ;
#28978 = CARTESIAN_POINT ( 'NONE',  ( -8.319899820280397762, 12.85830022363583147, -0.7998128361456281477 ) ) ;
#28980 = CARTESIAN_POINT ( 'NONE',  ( 8.666686507633574621, 11.13422023037111330, 1.599625672291281386 ) ) ;
#28982 = CARTESIAN_POINT ( 'NONE',  ( -7.669108446824431269, 12.09904362127053545, -0.7998128361456291469 ) ) ;
#28981 = CARTESIAN_POINT ( 'NONE',  ( -1.402160292154681736E-14, -0.03749999999998095135, 1.732050807568877637 ) ) ;
#28983 = CARTESIAN_POINT ( 'NONE',  ( -11.84668730067608777, 11.00634727754793651, 1.399999999999998579 ) ) ;
#28984 = CARTESIAN_POINT ( 'NONE',  ( 2.724872815078176913, 1.459976238909798996, -1.395942890215768895 ) ) ;
#28985 = CARTESIAN_POINT ( 'NONE',  ( -1.364683531250010295, 3.780208333674750953, 0.7879004041258379498 ) ) ;
#28986 = CARTESIAN_POINT ( 'NONE',  ( 10.38518247838791986, 11.21839376764850726, 0.7216878364870438212 ) ) ;
#28987 = CARTESIAN_POINT ( 'NONE',  ( 3.321700061091820366, -2.084211496276411779, 0.5730272365244913901 ) ) ;
#28988 = CARTESIAN_POINT ( 'NONE',  ( 6.339319342841494453, 9.553567112360518365, -1.199719254218452047 ) ) ;
#28989 = CARTESIAN_POINT ( 'NONE',  ( 1.499999999999987121, 4.545833333333352932, -0.8660254037844323793 ) ) ;
#28991 = FACE_OUTER_BOUND ( 'NONE', #206045, .T. ) ;
#28990 = CARTESIAN_POINT ( 'NONE',  ( 6.964048179274811012, 8.153752959689313684, 1.199719254218452047 ) ) ;
#28992 = CARTESIAN_POINT ( 'NONE',  ( 7.578644679914694926, 11.78557652663510424, 0.7216878364870438212 ) ) ;
#28994 = FACE_OUTER_BOUND ( 'NONE', #42507, .T. ) ;
#28993 = CARTESIAN_POINT ( 'NONE',  ( 0.3269468692386565678, -1.417551234153333395, 1.644607001386617418 ) ) ;
#28995 = CARTESIAN_POINT ( 'NONE',  ( -6.887178846062128379, 7.137389529935019183, -0.7216878364870278340 ) ) ;
#28996 = CARTESIAN_POINT ( 'NONE',  ( 1.364683531249986537, 0.6552083336747522857, -0.7879004041258239610 ) ) ;
#28997 = CARTESIAN_POINT ( 'NONE',  ( 1.681448347407452193, 1.514353137444489406, 1.584415833815432162 ) ) ;
#28998 = CARTESIAN_POINT ( 'NONE',  ( 6.460097816570166351, 6.783347224138203124, 0.3989550415292943408 ) ) ;
#28999 = CARTESIAN_POINT ( 'NONE',  ( 3.010884265427976825, 1.639692042162781194, -1.559206548184206564 ) ) ;
#29000 = CARTESIAN_POINT ( 'NONE',  ( -6.561256274009600986, 9.742217188731485678, -1.199719254218440723 ) ) ;
#29001 = CARTESIAN_POINT ( 'NONE',  ( -4.134873662043608178, 4.886736029548026217, 1.082531754730558626 ) ) ;
#29002 = CARTESIAN_POINT ( 'NONE',  ( 0.6823417656249899377, 4.738541667008086655, -1.181850606188754593 ) ) ;
#29003 = CARTESIAN_POINT ( 'NONE',  ( 6.244837129360077732, 6.910362811036335096, 0.8058565020967979331 ) ) ;
#29004 = CARTESIAN_POINT ( 'NONE',  ( -1.402160292154681736E-14, 12.81249999999999645, 1.732050807568881190 ) ) ;
#29005 = CARTESIAN_POINT ( 'NONE',  ( 7.024532985656136930, 8.328281583754568729, 1.082531754730549967 ) ) ;
#29006 = CARTESIAN_POINT ( 'NONE',  ( 4.534285406439878763, 1.735348426437629765, 0.3461848140887160974 ) ) ;
#29007 =( BOUNDED_CURVE ( )  B_SPLINE_CURVE ( 3, ( #19043, #637, #85122, #68850 ),
 .UNSPECIFIED., .F., .T. ) 
 B_SPLINE_CURVE_WITH_KNOTS ( ( 4, 4 ),
 ( 0.7261627075366219319, 1.570796326795131259 ),
 .UNSPECIFIED. ) 
 CURVE ( )  GEOMETRIC_REPRESENTATION_ITEM ( )  RATIONAL_B_SPLINE_CURVE ( ( 1.000000000000000000, 0.9414278581754867981, 0.9414278581754867981, 1.000000000000000000 ) ) 
 REPRESENTATION_ITEM ( '' )  );
#29008 = CARTESIAN_POINT ( 'NONE',  ( 9.531545685607134999, 11.07889037375188401, 1.199719254218450271 ) ) ;
#29009 = CARTESIAN_POINT ( 'NONE',  ( 0.8156195060344322290, -0.3088407994138153700, 2.083069475825300110 ) ) ;
#29010 = CARTESIAN_POINT ( 'NONE',  ( -1.364683531250010295, 9.880208333674728394, 0.7879004041258445001 ) ) ;
#29011 = CARTESIAN_POINT ( 'NONE',  ( -3.786470039966538970, 7.639575156594750283, 0.000000000000000000 ) ) ;
#29012 = CARTESIAN_POINT ( 'NONE',  ( -0.07118442604936793539, 7.078193277237627257, -2.121339347286375965 ) ) ;
#29014 = ORIENTED_EDGE ( 'NONE', *, *, #85316, .F. ) ;
#29013 = CARTESIAN_POINT ( 'NONE',  ( 5.027533431531807651, -0.2580777524966316738, 1.792966082415799800 ) ) ;
#29015 = EDGE_CURVE ( 'NONE', #24109, #113311, #23289, .T. ) ;
#29016 = CARTESIAN_POINT ( 'NONE',  ( 8.374132434735052755, 12.92157160716627295, -0.7998128361456352531 ) ) ;
#29017 = CARTESIAN_POINT ( 'NONE',  ( 3.221420234344949840, -1.803205065257794004, 0.4975683872451354683 ) ) ;
#29018 = CARTESIAN_POINT ( 'NONE',  ( 3.256751887857904926, -0.5965066610371800859, -1.982489643792232137 ) ) ;
#29019 = AXIS2_PLACEMENT_3D ( 'NONE', #11012, #106455, #90169 ) ;
#29020 = CARTESIAN_POINT ( 'NONE',  ( -6.305950843687521790, 7.489935751457798219, 1.082531754730548412 ) ) ;
#29021 = CARTESIAN_POINT ( 'NONE',  ( 1.355808955840422310E-16, -0.5000000000000004441, 2.024999999999999911 ) ) ;
#29022 = CARTESIAN_POINT ( 'NONE',  ( 7.567422294721922960, 11.98040977715095323, 0.7998128361456462443 ) ) ;
#29023 = CARTESIAN_POINT ( 'NONE',  ( -1.541006503187426269, 8.695732182938039401, 2.510084419394989386 ) ) ;
#29024 = CARTESIAN_POINT ( 'NONE',  ( 9.648753602328147494, 3.729558873908992211, 7.135166886579831669 ) ) ;
#29025 = CONICAL_SURFACE ( 'NONE', #184688, 1.219999999999999751, 0.7853981633974463916 ) ;
#29026 = CARTESIAN_POINT ( 'NONE',  ( 6.819229411136438657, -0.1619093195798972928, 2.126376854085454404 ) ) ;
#29027 = CARTESIAN_POINT ( 'NONE',  ( -1.602468905319636405E-14, -1.053124999658583638, -1.575800808251665908 ) ) ;
#29028 = CARTESIAN_POINT ( 'NONE',  ( 2.418345249890076154, 0.8361516037145629854, 1.774881043358336630 ) ) ;
#29029 = CARTESIAN_POINT ( 'NONE',  ( 1.405624810022429338, 0.3905361843517704545, 1.977748161624799161 ) ) ;
#29030 = ADVANCED_FACE ( 'NONE', ( #180907 ), #47746, .F. ) ;
#29031 = FACE_OUTER_BOUND ( 'NONE', #175719, .T. ) ;
#29033 = DIRECTION ( 'NONE',  ( 0.000000000000000000, 0.000000000000000000, 1.000000000000000000 ) ) ;
#29032 = CARTESIAN_POINT ( 'NONE',  ( 7.853197290813620945, 10.18514947741448573, 1.599625672291281386 ) ) ;
#29034 = CARTESIAN_POINT ( 'NONE',  ( 1.422894040683621464, -0.05142188859055819850, 1.870020055627517497 ) ) ;
#29035 = CARTESIAN_POINT ( 'NONE',  ( -0.6823417656250212460, 3.301041667008085323, 1.181850606188767472 ) ) ;
#29036 = CARTESIAN_POINT ( 'NONE',  ( 3.304942742240731590, -0.3968801077466362903, -1.973537420673168397 ) ) ;
#29038 = CARTESIAN_POINT ( 'NONE',  ( 2.671616206378808478, 1.499349897650571695, 1.495110359788552223 ) ) ;
#29037 = CARTESIAN_POINT ( 'NONE',  ( -6.887178846062123938, 8.097758744236356776, -1.082531754730544860 ) ) ;
#29039 = CARTESIAN_POINT ( 'NONE',  ( -6.628729601230480384, 6.698215721049152194, 0.3833203584966006217 ) ) ;
#29040 = CARTESIAN_POINT ( 'NONE',  ( 3.543477799061961253, 1.872898848466747479, -0.8826743078152868849 ) ) ;
#29041 = CARTESIAN_POINT ( 'NONE',  ( 6.535912570239620578, 9.782925877658371405, 1.199719254218452047 ) ) ;
#29043 = CARTESIAN_POINT ( 'NONE',  ( 11.84103413958623818, 13.61004478473146229, 1.443924719788817423 ) ) ;
#29042 = CARTESIAN_POINT ( 'NONE',  ( 6.421832395068366672, 1.204883778905677216, -1.708312069947721668 ) ) ;
#29045 = ORIENTED_EDGE ( 'NONE', *, *, #12956, .T. ) ;
#29044 = CARTESIAN_POINT ( 'NONE',  ( 5.315394819225006451, -0.2661953434012730435, 1.805952802178517613 ) ) ;
#29046 = CARTESIAN_POINT ( 'NONE',  ( 9.074484886248265880, 9.481320543578137361, 0.7998128361456462443 ) ) ;
#29047 = CARTESIAN_POINT ( 'NONE',  ( 5.738979324002048799, 5.917037536914529383, -2.440165351833862850 ) ) ;
#29048 = CARTESIAN_POINT ( 'NONE',  ( 9.780965096007749437, 12.99495041104594861, 8.039825270927440926 ) ) ;
#29049 = CARTESIAN_POINT ( 'NONE',  ( -10.19097401674926395, 4.476076320095182304, 5.708917106338025960 ) ) ;
#29050 = CARTESIAN_POINT ( 'NONE',  ( 1.364683531249997417, 11.79687500034139802, 2.602085213965210642E-15 ) ) ;
#29051 = CARTESIAN_POINT ( 'NONE',  ( 5.584596538761583240, -1.209766832763665034, 1.480987728393488245 ) ) ;
#29052 = CARTESIAN_POINT ( 'NONE',  ( -9.001723924469462901, 12.58942944760136484, -1.199719254218446718 ) ) ;
#29053 = CARTESIAN_POINT ( 'NONE',  ( 7.006866460164219212, 7.069099046480051385, -0.7998128361456281477 ) ) ;
#29054 = CARTESIAN_POINT ( 'NONE',  ( -11.92619526913699879, 10.90000000000000036, -1.328859060402686199 ) ) ;
#29055 = CARTESIAN_POINT ( 'NONE',  ( -5.599738924909661186, 5.745725798494749625, 0.2540040342395213369 ) ) ;
#29056 = CARTESIAN_POINT ( 'NONE',  ( 4.253507506385319381, 5.985511395581417204, 1.599625672291267398 ) ) ;
#29057 = ORIENTED_EDGE ( 'NONE', *, *, #178523, .F. ) ;
#29058 = CARTESIAN_POINT ( 'NONE',  ( -8.100070429521727178, 8.414780020722290033, 0.7998128361456341429 ) ) ;
#29059 = CARTESIAN_POINT ( 'NONE',  ( 4.903500725120335524, -0.5004011548357701900, 1.802273645872286334 ) ) ;
#29060 = CARTESIAN_POINT ( 'NONE',  ( -0.02319159430949970999, 2.891346550825595774, -2.299931007135449512 ) ) ;
#29061 = CARTESIAN_POINT ( 'NONE',  ( 5.505492895601038938, 8.580769590579979678, -1.199719254218452047 ) ) ;
#29062 = CARTESIAN_POINT ( 'NONE',  ( -6.378792857440260811, 6.837131066116997502, 0.5844455422965456615 ) ) ;
#29064 = CARTESIAN_POINT ( 'NONE',  ( -6.236387472606153892, 8.298871356172400127, -1.443375672974059665 ) ) ;
#29063 = VECTOR ( 'NONE', #81964, 1000.000000000000000 ) ;
#29065 = CARTESIAN_POINT ( 'NONE',  ( 3.388648328411762556, 6.040841252200647382, 1.199719254218462483 ) ) ;
#29066 = CARTESIAN_POINT ( 'NONE',  ( 1.041781249306489965, 1.318715992218882693, 1.462978117936466926 ) ) ;
#29067 = CARTESIAN_POINT ( 'NONE',  ( 3.110954007106698338, 0.05231540665236523308, 2.015913653835194719 ) ) ;
#29068 = CARTESIAN_POINT ( 'NONE',  ( -7.426115451983156923, 9.686887332112256388, -1.599625672291263179 ) ) ;
#29069 = CARTESIAN_POINT ( 'NONE',  ( 3.854260808034858155, 7.718664386007802136, -0.7998128361456362523 ) ) ;
#29070 = CARTESIAN_POINT ( 'NONE',  ( 6.727182134110203826, 2.399899341769623273, 2.668786705202597531 ) ) ;
#29071 = CARTESIAN_POINT ( 'NONE',  ( 3.433693710695666201, 0.9853049363134911420, -1.957518807868402044 ) ) ;
#29072 = DIRECTION ( 'NONE',  ( 8.638326563840814399E-31, 0.000000000000000000, 1.000000000000000000 ) ) ;
#29073 = CARTESIAN_POINT ( 'NONE',  ( 2.432535651424679646, 1.868085840533942221, 0.4698736581597633966 ) ) ;
#29074 = CARTESIAN_POINT ( 'NONE',  ( -7.974166903131914452, 12.45494515362926435, -0.7998128361456281477 ) ) ;
#29075 = SURFACE_SIDE_STYLE ('',( #156955 ) ) ;
#29076 = CARTESIAN_POINT ( 'NONE',  ( 0.1331565106231571705, 4.092041177288479048, -2.500854978060399691 ) ) ;
#29077 = CARTESIAN_POINT ( 'NONE',  ( 3.390947817193682656, 6.009837315817661008, -1.082531754730549967 ) ) ;
#29079 = ADVANCED_FACE ( 'NONE', ( #164666 ), #84469, .T. ) ;
#29078 = CARTESIAN_POINT ( 'NONE',  ( 6.448874621594486989, 10.67543749183559143, 0.7998128361456462443 ) ) ;
#29080 = CARTESIAN_POINT ( 'NONE',  ( 6.311484202361478779, 7.322151976631905868, -1.199719254218446718 ) ) ;
#29081 = CARTESIAN_POINT ( 'NONE',  ( 11.33772463945036790, 10.19999999999999929, -3.680000000000001048 ) ) ;
#29082 = CARTESIAN_POINT ( 'NONE',  ( 6.400857919427532572, 6.640291458853147866, -0.7216878364870458196 ) ) ;
#29083 = ORIENTED_EDGE ( 'NONE', *, *, #76301, .T. ) ;
#29085 = CARTESIAN_POINT ( 'NONE',  ( 2.174478567003877316, 0.8628565524405201748, 1.818940509527650295 ) ) ;
#29084 = CARTESIAN_POINT ( 'NONE',  ( 4.581507094455529838, -0.8636776874328588871, 1.626104626046148249 ) ) ;
#29086 = CARTESIAN_POINT ( 'NONE',  ( 4.464446571738351466, 1.842799458866357210, 1.373389552433499139 ) ) ;
#29088 = CARTESIAN_POINT ( 'NONE',  ( 2.025991663365491746, 0.9512761431412205537, 1.599265494891942030 ) ) ;
#29087 = CARTESIAN_POINT ( 'NONE',  ( -0.02900071798685524560, 2.860900941590225344, -2.661937258840251008 ) ) ;
#29089 = CARTESIAN_POINT ( 'NONE',  ( 0.000000000000000000, -2.646874999522040639, -3.793834371823813001 ) ) ;
#29090 = CARTESIAN_POINT ( 'NONE',  ( -4.138764970217294170, 3.930906674782672194, 0.2071306710573931620 ) ) ;
#29091 = CARTESIAN_POINT ( 'NONE',  ( 5.677967274442059953, 1.882970570262190835, -0.3333453579756898155 ) ) ;
#29092 = CARTESIAN_POINT ( 'NONE',  ( -8.667740277838301921, 9.006785167099828016, -0.7998128361456291469 ) ) ;
#29093 = CARTESIAN_POINT ( 'NONE',  ( -5.966997003790240228, 6.134120390609613338, -0.7216878364870338292 ) ) ;
#29095 = CARTESIAN_POINT ( 'NONE',  ( 3.028041890241763401, 1.040506211802554981, -1.554362669439563360 ) ) ;
#29094 = CARTESIAN_POINT ( 'NONE',  ( 5.337476071801405375, 0.8461711052811745626, -1.912038999733718825 ) ) ;
#29096 = CARTESIAN_POINT ( 'NONE',  ( 7.619319141200072920, 7.991553207595983643, 0.7216878364870317197 ) ) ;
#29097 = DIRECTION ( 'NONE',  ( 1.000000000000000000, -0.000000000000000000, -0.000000000000000000 ) ) ;
#29098 = CARTESIAN_POINT ( 'NONE',  ( -5.612712406377478480, 5.650512016969688744, 0.7216878364870735751 ) ) ;
#29099 = CARTESIAN_POINT ( 'NONE',  ( 5.514166437991733005, -0.7808720426115691726, -1.538077146617151669 ) ) ;
#29100 = CARTESIAN_POINT ( 'NONE',  ( -6.250472511100020334, 7.250971670160158311, 1.199719254218450271 ) ) ;
#29101 = CARTESIAN_POINT ( 'NONE',  ( 0.9317525018172129192, -1.365947654462830618, -1.068275208499162909 ) ) ;
#29102 = DIRECTION ( 'NONE',  ( 1.224646799147353207E-16, 1.000000000000000000, -1.301042606982605629E-17 ) ) ;
#29103 = CARTESIAN_POINT ( 'NONE',  ( 1.907692715643283243, 3.236394383240550621, 0.4609675857477184557 ) ) ;
#29104 = CARTESIAN_POINT ( 'NONE',  ( -1.484505139761352455, 7.334797934598009661, -4.257182005874962094 ) ) ;
#29105 = CARTESIAN_POINT ( 'NONE',  ( 6.034065736706932803, 1.286768452391522377, 1.748546487445822750 ) ) ;
#29106 = CARTESIAN_POINT ( 'NONE',  ( 3.914527900857078357, 1.289819402409349669, -1.292354223553587644 ) ) ;
#29107 = CARTESIAN_POINT ( 'NONE',  ( 2.764445781119912127, -0.7462812867886668977, -1.814464804917370166 ) ) ;
#29108 = CARTESIAN_POINT ( 'NONE',  ( 6.315624676198635434, -1.384492656466195681, -1.602007840318976584 ) ) ;
#29109 = DIRECTION ( 'NONE',  ( -0.06263215618080143765, 4.385051216238358438E-12, -0.9980366791917739677 ) ) ;
#29110 = CARTESIAN_POINT ( 'NONE',  ( 3.999470987966422086, 7.812499711282003823, 0.08775337862014347123 ) ) ;
#29111 = CARTESIAN_POINT ( 'NONE',  ( 8.589254009457354400, 9.979550084910457031, -1.199719254218446718 ) ) ;
#29112 = CARTESIAN_POINT ( 'NONE',  ( 2.614065066921432479, -0.6628553294307990562, 2.014303955012682223 ) ) ;
#29113 = CARTESIAN_POINT ( 'NONE',  ( -2.629918611371007575, 6.012062780000711371, 0.7216878364870317197 ) ) ;
#29114 = CARTESIAN_POINT ( 'NONE',  ( 5.573810548549551491, 6.635772073796838200, -1.082531754730548412 ) ) ;
#29115 = CARTESIAN_POINT ( 'NONE',  ( -5.486276195386677657, 6.266678140956847720, -0.9979454321464575894 ) ) ;
#29116 = CARTESIAN_POINT ( 'NONE',  ( 0.9013344411078340057, -1.777497804657724334, 1.061070337243313455 ) ) ;
#29117 = CARTESIAN_POINT ( 'NONE',  ( 1.500000000000001332, 14.40625000068279604, 0.000000000000000000 ) ) ;
#29119 = EDGE_LOOP ( 'NONE', ( #171994, #88858 ) ) ;
#29118 = CARTESIAN_POINT ( 'NONE',  ( 2.473529351063200377, -1.934054200746947227, -1.092377531094531173 ) ) ;
#29120 = CARTESIAN_POINT ( 'NONE',  ( 0.2824055751470951892, 1.906470811695348599, -1.284064767653005257 ) ) ;
#29122 = CARTESIAN_POINT ( 'NONE',  ( 5.893442400364165223, -1.866981718288396763, 0.8769185494091299438 ) ) ;
#29121 = CARTESIAN_POINT ( 'NONE',  ( 2.737856954955798727, 5.281584649835344258, 1.199719254218452047 ) ) ;
#29124 = CARTESIAN_POINT ( 'NONE',  ( 3.475000000000000533, -2.595833333333334103, -2.006292185433951047 ) ) ;
#29123 = CARTESIAN_POINT ( 'NONE',  ( 5.662465432362883355, 6.635239754958710989, 1.199719254218451159 ) ) ;
#29125 = EDGE_CURVE ( 'NONE', #44666, #172003, #180178, .T. ) ;
#29126 = CARTESIAN_POINT ( 'NONE',  ( -11.84668730067608600, 19.00000000000000000, -1.320000000000001616 ) ) ;
#29127 = CARTESIAN_POINT ( 'NONE',  ( 5.038538826285253514, -1.576363729006284187, 0.9512496309353533075 ) ) ;
#29128 = CARTESIAN_POINT ( 'NONE',  ( 4.162516854595432747, 4.815023404238158555, 1.199719254218464037 ) ) ;
#29129 = CARTESIAN_POINT ( 'NONE',  ( -0.2104748580754409182, 6.947232144882289795, -2.698723162346649662 ) ) ;
#29130 = CARTESIAN_POINT ( 'NONE',  ( 3.240908261985251837, -1.521742930289736728, 0.8118271961824756744 ) ) ;
#29131 = CARTESIAN_POINT ( 'NONE',  ( 0.7433754753295095385, 0.3886281223182270761, -1.978556061772406505 ) ) ;
#29132 = CARTESIAN_POINT ( 'NONE',  ( -1.364683531250012516, 3.342708333674756727, 0.7879004041258379498 ) ) ;
#29133 = CARTESIAN_POINT ( 'NONE',  ( 2.442968603456824095, 0.4936193734879111283, 2.207763252559187261 ) ) ;
#29134 = CARTESIAN_POINT ( 'NONE',  ( 3.686240278715931851, -1.037925599752804739, 1.832463683143903399 ) ) ;
#29135 = CARTESIAN_POINT ( 'NONE',  ( -5.496904935697871863, 5.377753611261092637, 0.7998128361456281477 ) ) ;
#29136 = CARTESIAN_POINT ( 'NONE',  ( 3.989309445023786704, 1.280397443517577782, 1.221928027103141634 ) ) ;
#29138 = EDGE_CURVE ( 'NONE', #8789, #46947, #97828, .T. ) ;
#29137 = CARTESIAN_POINT ( 'NONE',  ( 5.636439174979242850, 7.598931675607687453, -1.599625672291262513 ) ) ;
#29140 = CARTESIAN_POINT ( 'NONE',  ( 0.1645876019286318381, -1.492192613954560265, 1.740154187221523818 ) ) ;
#29139 = CARTESIAN_POINT ( 'NONE',  ( 3.567203813726949058, 7.175838526074521440, 0.7216878364870257245 ) ) ;
#29141 = CARTESIAN_POINT ( 'NONE',  ( 4.523293815724619193, -1.134750198001058585, -1.449786353205910538 ) ) ;
#29142 = CARTESIAN_POINT ( 'NONE',  ( -4.843287188579803448, 6.673587691474970107, -1.599625672291256295 ) ) ;
#29143 = CARTESIAN_POINT ( 'NONE',  ( 5.463572716182824252, 7.397254140345190798, 1.443375672974062551 ) ) ;
#29144 = CARTESIAN_POINT ( 'NONE',  ( -1.499999999999997780, 3.900000000000021672, 1.214306433183764966E-14 ) ) ;
#29145 = CARTESIAN_POINT ( 'NONE',  ( 4.242245924764226572, 0.5834501570099770440, 2.112278566661344392 ) ) ;
#29146 = CARTESIAN_POINT ( 'NONE',  ( -3.978428010606240850, 6.728917548094202949, -1.199719254218452047 ) ) ;
#29147 = CARTESIAN_POINT ( 'NONE',  ( -0.006768871532362320982, 8.210909518262125673, -2.038649385027043071 ) ) ;
#29148 = DIRECTION ( 'NONE',  ( 2.031254238220912814E-34, -1.000000000000000000, 1.301042606982605475E-17 ) ) ;
#29149 = CARTESIAN_POINT ( 'NONE',  ( -1.201851678989727383E-14, 3.946875000341423689, -1.575800808251660134 ) ) ;
#29150 = CARTESIAN_POINT ( 'NONE',  ( 3.053258290938072772, -1.575281680543440643, -1.108752609043755832 ) ) ;
#29151 = CARTESIAN_POINT ( 'NONE',  ( 1.364683531249996529, 8.963541667008067648, 0.7879004041258405033 ) ) ;
#29152 = CARTESIAN_POINT ( 'NONE',  ( -3.958617665510279160, 5.641473247893851628, -1.443375672974053447 ) ) ;
#29153 = CARTESIAN_POINT ( 'NONE',  ( 0.1588220795745398928, 2.216043539545629937, 0.1551192601621682043 ) ) ;
#29154 = CARTESIAN_POINT ( 'NONE',  ( -4.665414256878287702, 8.457084043084382330, -0.7216878364870338292 ) ) ;
#29155 = ORIENTED_EDGE ( 'NONE', *, *, #193063, .T. ) ;
#29156 = CARTESIAN_POINT ( 'NONE',  ( -4.746763178560296836, 6.631252689777363152, 1.443375672974058777 ) ) ;
#29157 = CARTESIAN_POINT ( 'NONE',  ( 3.517450787741589036, 6.191110788085444128, -1.199719254218446718 ) ) ;
#29158 = CARTESIAN_POINT ( 'NONE',  ( -2.474627113408586876, 0.3228523939998627079, -0.3300564308867506291 ) ) ;
#29159 = CARTESIAN_POINT ( 'NONE',  ( 0.5972946108512422470, 6.677937114322130441, -3.537249485762780310 ) ) ;
#29160 = CARTESIAN_POINT ( 'NONE',  ( 1.364683531249990311, 4.696875000341417916, 1.214306433183764966E-14 ) ) ;
#29161 = CARTESIAN_POINT ( 'NONE',  ( 2.682838027602444164, 1.232319236757819292, 1.229298679657732762 ) ) ;
#29162 = CARTESIAN_POINT ( 'NONE',  ( 3.823036129373602154, 6.443664003369091731, -1.082531754730548412 ) ) ;
#29163 = CARTESIAN_POINT ( 'NONE',  ( 11.84668730067608777, 12.59365272245202938, 1.399999999999998579 ) ) ;
#29164 = CARTESIAN_POINT ( 'NONE',  ( -1.402160292154681736E-14, 1.259375000341419248, -1.575800808251659024 ) ) ;
#29165 = ADVANCED_FACE ( 'NONE', ( #55700 ), #83396, .F. ) ;
#29166 = CARTESIAN_POINT ( 'NONE',  ( 5.858325616802108726, 0.8718737102157668728, 1.978260574764856283 ) ) ;
#29167 = PRESENTATION_LAYER_ASSIGNMENT (  '', '', ( #105266 ) ) ;
#29168 = CARTESIAN_POINT ( 'NONE',  ( -9.972185678051314284, 11.59297036493672017, 1.199719254218462483 ) ) ;
#29169 = EDGE_CURVE ( 'NONE', #71915, #192824, #118494, .T. ) ;
#29170 = CARTESIAN_POINT ( 'NONE',  ( -7.510853911846401942, 7.865010440016681592, 1.040834085586084257E-14 ) ) ;
#29171 = CARTESIAN_POINT ( 'NONE',  ( 5.787991602622606813, -0.9759734195362681497, 1.928925553883020338 ) ) ;
#29173 = VERTEX_POINT ( 'NONE', #121320 ) ;
#29172 = CARTESIAN_POINT ( 'NONE',  ( -0.2106725631050020975, 7.629137130509112907, -2.603678913577145426 ) ) ;
#29174 = CARTESIAN_POINT ( 'NONE',  ( 1.364683531249990311, 4.863541667008084879, 0.7879004041258500513 ) ) ;
#29175 = CARTESIAN_POINT ( 'NONE',  ( 6.749300054864300513, -1.582014061365591751, -1.175997427595596445 ) ) ;
#29176 = CARTESIAN_POINT ( 'NONE',  ( 6.608738931450677256, 0.6592670866186548517, -1.603827835538347291 ) ) ;
#29177 = MECHANICAL_DESIGN_GEOMETRIC_PRESENTATION_REPRESENTATION (  '', ( #133108 ), #50056 ) ;
#29179 = CARTESIAN_POINT ( 'NONE',  ( 3.597391730528697540, -0.6346259394694170330, 2.097678010650514402 ) ) ;
#29178 = CARTESIAN_POINT ( 'NONE',  ( 1.360316468749977581, 0.5364583336746844289, -0.7853790794159001276 ) ) ;
#29180 = CARTESIAN_POINT ( 'NONE',  ( 3.382123439733915493, 1.462175888237092547, 1.785228103979496384 ) ) ;
#29181 = CARTESIAN_POINT ( 'NONE',  ( 5.870404149471736943, -1.310866377807779593, 1.590078559457400287 ) ) ;
#29182 = CARTESIAN_POINT ( 'NONE',  ( 0.7088029311262042942, -0.2857661853880436031, 1.920690660100693226 ) ) ;
#29183 = CARTESIAN_POINT ( 'NONE',  ( -5.043269954159181445, 8.827639346586952485, 1.214306433183764966E-14 ) ) ;
#29184 = CARTESIAN_POINT ( 'NONE',  ( -0.3773006915670014116, -8.233136995002810821, -9.492905263954437345 ) ) ;
#29185 = DIRECTION ( 'NONE',  ( -1.276756478318932191E-15, 1.000000000000000000, -3.330669073875483426E-16 ) ) ;
#29186 = CARTESIAN_POINT ( 'NONE',  ( 4.500305224345508393, -0.9970752094022590217, 1.871535012320741265 ) ) ;
#29187 = CARTESIAN_POINT ( 'NONE',  ( -0.3870774458628380987, 0.9691415390508737460, 11.89165654491649349 ) ) ;
#29188 = CARTESIAN_POINT ( 'NONE',  ( 2.883435573726996548, -0.5880205015329244000, -1.928751729079546173 ) ) ;
#29189 = CARTESIAN_POINT ( 'NONE',  ( -5.544921637864833386, 7.492161215640853023, -1.443375672974051449 ) ) ;
#29190 = CARTESIAN_POINT ( 'NONE',  ( 5.403435775159438847, 1.801252639416499379, 1.274624607731331905 ) ) ;
#29191 = CARTESIAN_POINT ( 'NONE',  ( 6.750000000000007994, 7.629137130509070275, 2.600000000000001421 ) ) ;
#29193 =( BOUNDED_CURVE ( )  B_SPLINE_CURVE ( 2, ( #114272, #162961, #80637, #146729, #130526 ),
 .UNSPECIFIED., .F., .T. ) 
 B_SPLINE_CURVE_WITH_KNOTS ( ( 3, 2, 3 ),
 ( 0.1113702160535958580, 0.1125000000000000028, 0.1138193015819521647 ),
 .UNSPECIFIED. ) 
 CURVE ( )  GEOMETRIC_REPRESENTATION_ITEM ( )  RATIONAL_B_SPLINE_CURVE ( ( 0.9470460506485154362, 0.9636730364727235099, 1.000000000000000000, 0.9575793047851379747, 0.9420221409164253323 ) ) 
 REPRESENTATION_ITEM ( '' )  );
#29192 = CARTESIAN_POINT ( 'NONE',  ( -10.18461545817740088, 3.956598013261175772, 5.433575010662861082 ) ) ;
#29194 = CARTESIAN_POINT ( 'NONE',  ( 0.0004021782957080999310, 14.56829811979804923, 11.92774320584193859 ) ) ;
#29195 = CARTESIAN_POINT ( 'NONE',  ( -5.562588163356775972, 9.711712967216715953, 0.7998128361456291469 ) ) ;
#29197 = CARTESIAN_POINT ( 'NONE',  ( 0.000000000000000000, -9.900000000000005684, 0.000000000000000000 ) ) ;
#29196 = CARTESIAN_POINT ( 'NONE',  ( -4.622835856459495574, 8.451390222604121760, 0.3997878540293615113 ) ) ;
#29198 = CARTESIAN_POINT ( 'NONE',  ( -5.388983382465591276, 7.615141676677004590, 1.304926139240682348 ) ) ;
#29199 = ORIENTED_EDGE ( 'NONE', *, *, #81687, .F. ) ;
#29200 = CARTESIAN_POINT ( 'NONE',  ( 4.170816135027268778, -1.922254079802641069, -0.7435701193346122562 ) ) ;
#29201 = CARTESIAN_POINT ( 'NONE',  ( -7.607533590599451223, 9.008448956188397361, 1.082531754730549078 ) ) ;
#29202 = CARTESIAN_POINT ( 'NONE',  ( 0.2498445108307164875, 7.025621425018297117, -3.913348414359987704 ) ) ;
#29203 = CARTESIAN_POINT ( 'NONE',  ( -3.730464822054482710, 7.503959392372201442, 1.040834085586084257E-14 ) ) ;
#29204 = CARTESIAN_POINT ( 'NONE',  ( -4.842197138736131556, 5.678260079060780008, 1.199719254218452935 ) ) ;
#29205 = CARTESIAN_POINT ( 'NONE',  ( 3.879560801468981523, 0.2449043481074340001, -2.004685163654993385 ) ) ;
#29206 = CARTESIAN_POINT ( 'NONE',  ( 0.7499999999999885647, 1.316666666666688190, -1.299038105676652899 ) ) ;
#29208 = CARTESIAN_POINT ( 'NONE',  ( 8.595506201384004896, 12.01154575404795466, 1.082531754730546636 ) ) ;
#29207 = CARTESIAN_POINT ( 'NONE',  ( -4.468294144155606773, 7.370704380560280100, 1.199719254218452935 ) ) ;
#29209 = CARTESIAN_POINT ( 'NONE',  ( 5.933664784275179294, 10.07435934829639912, -0.7998128361456291469 ) ) ;
#29210 = CARTESIAN_POINT ( 'NONE',  ( 3.573166805712838734, 0.05218571934602388163, -2.060405206736420247 ) ) ;
#29211 = CARTESIAN_POINT ( 'NONE',  ( 2.725232599228684993, 2.001511357256777313, 0.2440295182731533341 ) ) ;
#29212 = EDGE_LOOP ( 'NONE', ( #53456, #56487, #144213, #37866 ) ) ;
#29213 = CARTESIAN_POINT ( 'NONE',  ( -0.1263102688159843667, 6.427441598446242743, 3.069922131261606513 ) ) ;
#29214 = CARTESIAN_POINT ( 'NONE',  ( 4.168242161197552420, 6.950367390450747251, -1.199719254218452047 ) ) ;
#29216 = ORIENTED_EDGE ( 'NONE', *, *, #101627, .F. ) ;
#29215 = CARTESIAN_POINT ( 'NONE',  ( -0.2638905955354677868, 7.233311467405415307, -1.984662505942582422 ) ) ;
#29217 = CARTESIAN_POINT ( 'NONE',  ( 3.198592129611950607, -1.351947076146834403, -1.495823048609262518 ) ) ;
#29218 = CARTESIAN_POINT ( 'NONE',  ( 2.624749632297512569, -1.717891791495285592, 0.6627527109525217508 ) ) ;
#29219 = CARTESIAN_POINT ( 'NONE',  ( 0.3116875490984937214, 2.011018277352360606, 1.131832386414432179 ) ) ;
#29220 = CARTESIAN_POINT ( 'NONE',  ( 5.224688093219824303, 7.188831756880171397, -1.599625672291283607 ) ) ;
#29221 = CARTESIAN_POINT ( 'NONE',  ( 2.935029080331118756, 0.2613785356864756770, 2.145644965459513109 ) ) ;
#29222 = CARTESIAN_POINT ( 'NONE',  ( -5.063080299699540987, 7.994345218703034384, 1.199719254218464037 ) ) ;
#29223 = CARTESIAN_POINT ( 'NONE',  ( 4.874263506423556436, -2.101702868649154343, -0.2561063476108938475 ) ) ;
#29224 = ORIENTED_EDGE ( 'NONE', *, *, #125699, .T. ) ;
#29225 = CARTESIAN_POINT ( 'NONE',  ( 5.946383829937739840, 4.757679660029577207, -2.499999999999690470 ) ) ;
#29226 = CARTESIAN_POINT ( 'NONE',  ( 1.621729638615863944, -1.036547396872866678, -1.557007864774778705 ) ) ;
#29227 = CARTESIAN_POINT ( 'NONE',  ( 6.174684870424203886, -1.871919000353940099, -0.6187097519457245287 ) ) ;
#29228 = MECHANICAL_DESIGN_GEOMETRIC_PRESENTATION_REPRESENTATION (  '', ( #87974 ), #63689 ) ;
#29230 = CARTESIAN_POINT ( 'NONE',  ( 7.402388682937041331, 11.57994453016116587, 1.040834085586084257E-14 ) ) ;
#29229 = CARTESIAN_POINT ( 'NONE',  ( 1.364683531249990311, 2.884375000341422801, 1.214306433183764966E-14 ) ) ;
#29232 = CARTESIAN_POINT ( 'NONE',  ( 0.1533209562146371774, -1.769702838771534559, 1.318327933512997152 ) ) ;
#29231 = CARTESIAN_POINT ( 'NONE',  ( -7.725448601688521322, 7.907444878258402809, 1.040834085586084257E-14 ) ) ;
#29233 = CARTESIAN_POINT ( 'NONE',  ( 6.004363041306050697, 2.067815565686380364, 0.1054426792976848049 ) ) ;
#29234 = CARTESIAN_POINT ( 'NONE',  ( 7.006866460164219212, 7.069099046480051385, -0.7998128361456281477 ) ) ;
#29235 = CARTESIAN_POINT ( 'NONE',  ( -5.819474248763749635, 7.812472595022922128, -1.599625672291256295 ) ) ;
#29236 = CARTESIAN_POINT ( 'NONE',  ( 6.639320575229256782, 4.691717626494606996, 2.665852771288126366 ) ) ;
#29237 = CARTESIAN_POINT ( 'NONE',  ( 5.119980909927547508, -1.054019455064346689, -1.665871061098343819 ) ) ;
#29238 = CARTESIAN_POINT ( 'NONE',  ( -0.08743476694611679312, -2.120266877281291595, -0.04547849331201780226 ) ) ;
#29239 = CARTESIAN_POINT ( 'NONE',  ( 1.499999999999987121, 0.7854166673494828999, 0.8660254037844524744 ) ) ;
#29240 = CARTESIAN_POINT ( 'NONE',  ( 4.459805605305016130, 0.5082999457236726526, -2.250878628046268037 ) ) ;
#29241 = AXIS2_PLACEMENT_3D ( 'NONE', #48246, #115416, #95932 ) ;
#29242 = CARTESIAN_POINT ( 'NONE',  ( 2.360284975695529752, -2.062195451902974597, 0.04632573159841534699 ) ) ;
#29243 = CARTESIAN_POINT ( 'NONE',  ( 7.619319141200070256, 8.951922421897323900, 1.082531754730558626 ) ) ;
#29244 = CARTESIAN_POINT ( 'NONE',  ( 4.355912491740495440, 8.303924683664389406, 0.000000000000000000 ) ) ;
#29245 = CARTESIAN_POINT ( 'NONE',  ( 5.032011289327418702, 5.899709921417326974, 1.199719254218452935 ) ) ;
#29246 = CARTESIAN_POINT ( 'NONE',  ( 1.364683531249988535, 1.926041667008086211, 0.7879004041258500513 ) ) ;
#29247 = CARTESIAN_POINT ( 'NONE',  ( 3.366167277942881064, 7.149221934233827014, -0.7998128361456362523 ) ) ;
#29248 = CARTESIAN_POINT ( 'NONE',  ( 5.951666246274803562, 7.006327377817825663, 1.082531754730558626 ) ) ;
#29249 = CARTESIAN_POINT ( 'NONE',  ( 4.422458135217792297, 1.019899284492602698, 1.916704820016806199 ) ) ;
#29251 = CARTESIAN_POINT ( 'NONE',  ( 3.755264181858387840, 1.826884192416846631, -0.2291247506851084581 ) ) ;
#29250 = CARTESIAN_POINT ( 'NONE',  ( -4.460269349215930212, 4.305995116947750390, 1.214306433183764966E-14 ) ) ;
#29253 = CARTESIAN_POINT ( 'NONE',  ( 6.720655732516669367, 7.629137130509068498, 2.426260288887295058 ) ) ;
#29252 = DIRECTION ( 'NONE',  ( 2.949029909160572061E-17, 1.000000000000000000, -8.673600428462391266E-15 ) ) ;
#29254 = CARTESIAN_POINT ( 'NONE',  ( 5.618738332679400038, -0.05485954975367920983, 2.191026952110195491 ) ) ;
#29255 = CARTESIAN_POINT ( 'NONE',  ( -11.01135777277262129, 10.90000000000000036, -1.400000000000001910 ) ) ;
#29256 = CARTESIAN_POINT ( 'NONE',  ( 6.403223674518304875, 1.876769595090790554, 1.263360297164903168 ) ) ;
#29257 = ORIENTED_EDGE ( 'NONE', *, *, #205822, .F. ) ;
#29258 = CARTESIAN_POINT ( 'NONE',  ( -3.976064435573588796, 7.848781721302746206, 0.05846302465613295585 ) ) ;
#29259 = CARTESIAN_POINT ( 'NONE',  ( 4.595450297557979624, 8.489593704440707711, 0.02661077391274621617 ) ) ;
#29260 = CARTESIAN_POINT ( 'NONE',  ( -4.272227801637618505, 7.998366511970260717, 0.7216878364870338292 ) ) ;
#29261 = CARTESIAN_POINT ( 'NONE',  ( 4.095971805104288599, 5.871996087412059140, 1.443375672974058777 ) ) ;
#29262 = CARTESIAN_POINT ( 'NONE',  ( 0.8129392405988710157, -0.2653805273100506290, 1.749707594005883937 ) ) ;
#29263 = CARTESIAN_POINT ( 'NONE',  ( 5.672526239869847053, 0.8180066501249063649, 1.839585422649665958 ) ) ;
#29264 = CARTESIAN_POINT ( 'NONE',  ( 5.849453209292126310, 8.911780279894442103, 1.199719254218462483 ) ) ;
#29265 = CARTESIAN_POINT ( 'NONE',  ( 4.260836881943074417, -1.562014524604074861, 1.412707936923715879 ) ) ;
#29266 = CARTESIAN_POINT ( 'NONE',  ( 2.161615495643732565, 1.180369796089770995, 1.508615382416353290 ) ) ;
#29267 = CARTESIAN_POINT ( 'NONE',  ( 4.090809663021327758, 5.795697244990093644, 1.599625672291267398 ) ) ;
#29268 = CARTESIAN_POINT ( 'NONE',  ( 2.752355523121536862, -1.964097686037095336, -0.1475717908260633926 ) ) ;
#29269 = CARTESIAN_POINT ( 'NONE',  ( 5.027605771429075610, -0.2921156310390393140, 1.998402611621821423 ) ) ;
#29270 = CARTESIAN_POINT ( 'NONE',  ( 1.305301652190330675, -0.4579020413679709689, 1.813615928118620380 ) ) ;
#29273 = ORIENTED_EDGE ( 'NONE', *, *, #3092, .F. ) ;
#29272 = CARTESIAN_POINT ( 'NONE',  ( 1.318461241437279607, -0.6911404020932455650, -1.783297644634279200 ) ) ;
#29271 = CARTESIAN_POINT ( 'NONE',  ( 5.180183349501196410, -0.9537450585986576579, 1.436990496349071833 ) ) ;
#29275 = CARTESIAN_POINT ( 'NONE',  ( 4.202664430556247055, 6.886563688082179446, 1.082531754730558626 ) ) ;
#29274 = CARTESIAN_POINT ( 'NONE',  ( 1.260703874955213744, 0.8971468365699288849, 2.016480257658866737 ) ) ;
#29276 = EDGE_CURVE ( 'NONE', #10766, #134057, #811, .T. ) ;
#29277 = CARTESIAN_POINT ( 'NONE',  ( 1.364683531249986537, 2.217708333674751398, -0.7879004041258239610 ) ) ;
#29278 = CARTESIAN_POINT ( 'NONE',  ( 7.377608144130607393, 11.75895993479440982, -0.7998128361456291469 ) ) ;
#29279 = CARTESIAN_POINT ( 'NONE',  ( -1.420000000000001039, 6.200000000000045475, -2.873333333333329520 ) ) ;
#29280 = CARTESIAN_POINT ( 'NONE',  ( -1.387778780781445676E-14, -5.907420853759282053, -10.91970695577495398 ) ) ;
#29281 = CARTESIAN_POINT ( 'NONE',  ( -2.449742653233043743, 3.949999999999981526, -0.4500000000000354272 ) ) ;
#29282 = CARTESIAN_POINT ( 'NONE',  ( 1.188034388246852480, -1.312013912954514971, -1.601590607232979524 ) ) ;
#29283 = CARTESIAN_POINT ( 'NONE',  ( -0.7500000000000215383, 1.691666666666688634, 1.299038105676659116 ) ) ;
#29284 = CARTESIAN_POINT ( 'NONE',  ( 5.931855901178834323, 6.879252291918818152, 1.199719254218462483 ) ) ;
#29285 = CARTESIAN_POINT ( 'NONE',  ( -5.865874016206865882, 9.995270118883347266, 0.000000000000000000 ) ) ;
#29286 = CARTESIAN_POINT ( 'NONE',  ( 4.878955176071345434, 6.785476686873604280, -1.599625672291269396 ) ) ;
#29287 = CARTESIAN_POINT ( 'NONE',  ( 5.250683377293950294, 2.089169806880130320, 0.3621421040747307973 ) ) ;
#29288 = CARTESIAN_POINT ( 'NONE',  ( 5.477130869796502211, 5.492333557625114437, 1.040834085586084257E-14 ) ) ;
#29289 = CARTESIAN_POINT ( 'NONE',  ( 1.364683531249986537, 2.155208333674751398, -0.7879004041258239610 ) ) ;
#29290 = ORIENTED_EDGE ( 'NONE', *, *, #186606, .F. ) ;
#29291 = CARTESIAN_POINT ( 'NONE',  ( 0.7499999999999885647, 3.316666666666689967, -1.299038105676658228 ) ) ;
#29293 = CARTESIAN_POINT ( 'NONE',  ( 3.063252641683779753, 5.661212951017999373, 1.199719254218450271 ) ) ;
#29292 = CARTESIAN_POINT ( 'NONE',  ( 6.812952578306354035, -1.517200236233799071, 1.243500037895750143 ) ) ;
#29294 = CARTESIAN_POINT ( 'NONE',  ( 4.182970119252515495, -1.034007530860373336, -1.730600854597413418 ) ) ;
#29295 = CARTESIAN_POINT ( 'NONE',  ( 4.698395719694191897, 1.316562313306284038, -1.391896452211606849 ) ) ;
#29296 = CARTESIAN_POINT ( 'NONE',  ( 2.700927432832851860, 1.852951201923001223, 1.169960570980829839 ) ) ;
#29297 = CARTESIAN_POINT ( 'NONE',  ( -3.449547071718236158, 5.499999999999998224, -2.024999999999992806 ) ) ;
#29298 = CARTESIAN_POINT ( 'NONE',  ( -1.500000000000013101, 0.4520833340161533598, 0.8660254037844403729 ) ) ;
#29299 = CARTESIAN_POINT ( 'NONE',  ( 4.886981372429439752, -1.897129443012405936, -0.6741400253723847102 ) ) ;
#29300 = CARTESIAN_POINT ( 'NONE',  ( -6.235860587281615075, 9.362588887548838557, -1.199719254218440723 ) ) ;
#29302 = CARTESIAN_POINT ( 'NONE',  ( 5.360994948850416719, -0.05292929278505505153, -2.116735950649220932 ) ) ;
#29301 = CARTESIAN_POINT ( 'NONE',  ( -3.253593677599670109, 5.779314476299451719, 1.082531754730560403 ) ) ;
#29303 = FILL_AREA_STYLE_COLOUR ( '', #670 ) ;
#29305 = CARTESIAN_POINT ( 'NONE',  ( -5.932574734431526942, 9.079031735882207244, 1.199719254218454489 ) ) ;
#29304 = CARTESIAN_POINT ( 'NONE',  ( 3.280887763456251882, 1.889169395226503401, -0.8960188238960642426 ) ) ;
#29307 = ORIENTED_EDGE ( 'NONE', *, *, #183234, .F. ) ;
#29306 = CARTESIAN_POINT ( 'NONE',  ( 1.412684849630441386, 1.518645404226389051, 0.8176530575639671117 ) ) ;
#29308 = CARTESIAN_POINT ( 'NONE',  ( 5.361630242575341931, -1.673063676233761621, -1.302930760576012092 ) ) ;
#29309 = CARTESIAN_POINT ( 'NONE',  ( 6.043183783389218355, 8.073467052085995022, 1.599625672291267398 ) ) ;
#29310 = CARTESIAN_POINT ( 'NONE',  ( 10.98546216864998826, 12.34258621008987866, 1.592236800091190396 ) ) ;
#29311 = CARTESIAN_POINT ( 'NONE',  ( 7.586197045692582464, -6.654700410849454961, 7.966449380362582211 ) ) ;
#29312 = CARTESIAN_POINT ( 'NONE',  ( -6.855650617048461903, -7.357813805523316653, -6.855650617048431705 ) ) ;
#29313 = CARTESIAN_POINT ( 'NONE',  ( 5.309989718046547402, 9.346738437696316737, 0.7998128361456462443 ) ) ;
#29314 = VERTEX_POINT ( 'NONE', #153743 ) ;
#29315 = CARTESIAN_POINT ( 'NONE',  ( -1.992711204631002198E-15, 2.999999999999989342, 1.224999999999989875 ) ) ;
#29317 = CARTESIAN_POINT ( 'NONE',  ( 1.506221797076849889, -1.802732806890252837, -0.1774259793663693907 ) ) ;
#29316 = CARTESIAN_POINT ( 'NONE',  ( 5.180097208873055692, 8.201141289397330780, -1.199719254218450271 ) ) ;
#29318 = CARTESIAN_POINT ( 'NONE',  ( -6.566226467720086113, 6.555019055295208119, 1.040834085586084257E-14 ) ) ;
#29319 = EDGE_LOOP ( 'NONE', ( #125613, #173002, #7337, #106352, #189033, #114658 ) ) ;
#29320 = CARTESIAN_POINT ( 'NONE',  ( 2.706824224222692088, 6.309712028235118453, 0.7998128361456362523 ) ) ;
#29321 = VERTEX_POINT ( 'NONE', #20521 ) ;
#29322 = CARTESIAN_POINT ( 'NONE',  ( 5.306037014901791693, 7.283738832175834510, 1.599625672291269396 ) ) ;
#29323 = CARTESIAN_POINT ( 'NONE',  ( 2.525776224529495906, -1.791516492901791713, 0.2672755921442840354 ) ) ;
#29324 = CARTESIAN_POINT ( 'NONE',  ( 6.639320575229253230, 6.038193673056963640, 2.491643636677738360 ) ) ;
#29325 = CARTESIAN_POINT ( 'NONE',  ( -10.98677171181893186, -7.666863022246093173, 0.5458515184425656308 ) ) ;
#29326 = CARTESIAN_POINT ( 'NONE',  ( 4.196871964084724738, 7.339766560697110975, 0.8424661700066529146 ) ) ;
#29327 = VERTEX_POINT ( 'NONE', #203521 ) ;
#29328 = CARTESIAN_POINT ( 'NONE',  ( 4.422197255734514165, 0.8761312318771010688, 1.641894029917531084 ) ) ;
#29329 = CARTESIAN_POINT ( 'NONE',  ( 1.950665421479770067, -1.752291233380006474, -0.7743663792006536539 ) ) ;
#29330 = CARTESIAN_POINT ( 'NONE',  ( 6.141620278036529434, -1.395723430145169752, -1.327979989909616521 ) ) ;
#29331 = AXIS2_PLACEMENT_3D ( 'NONE', #155910, #9640, #154842 ) ;
#29332 = CARTESIAN_POINT ( 'NONE',  ( 1.364417678870917472, 3.686064748296142390, 0.6242711042719444325 ) ) ;
#29333 = LINE ( 'NONE', #78071, #133470 ) ;
#29334 = CARTESIAN_POINT ( 'NONE',  ( 4.649081266440608928, 8.305916344280937835, -0.4560373724170601606 ) ) ;
#29335 = PRESENTATION_STYLE_ASSIGNMENT (( #49837 ) ) ;
#29336 = CARTESIAN_POINT ( 'NONE',  ( -4.105300466841341311, 3.978332001433686926, 0.4115170502265364516 ) ) ;
#29337 = MECHANICAL_DESIGN_GEOMETRIC_PRESENTATION_REPRESENTATION (  '', ( #198903 ), #192107 ) ;
#29338 = CARTESIAN_POINT ( 'NONE',  ( 6.629573927402440781, 10.67832731537079383, 1.040834085586084257E-14 ) ) ;
#29339 = CARTESIAN_POINT ( 'NONE',  ( 5.787944378201490103, -1.246615054290018065, -1.524717904608218877 ) ) ;
#29340 = CARTESIAN_POINT ( 'NONE',  ( -4.055860508782465068, 7.883587693554856557, 1.040834085586084257E-14 ) ) ;
#29341 = CARTESIAN_POINT ( 'NONE',  ( 6.938893903907228378E-15, 10.64264068711930733, 1.214306433183764966E-14 ) ) ;
#29342 = CARTESIAN_POINT ( 'NONE',  ( 0.1290073198303761104, -1.910558061381230521, 0.8492679875119947264 ) ) ;
#29343 = CARTESIAN_POINT ( 'NONE',  ( 5.346851039111009563, 6.199209027673978412, 1.092492203018504471 ) ) ;
#29344 = CARTESIAN_POINT ( 'NONE',  ( 5.719733624436385000, -1.879402930333987198, 0.4222299131634628111 ) ) ;
#29345 = CARTESIAN_POINT ( 'NONE',  ( -5.194745412330402878, 9.212286747694129474, 0.000000000000000000 ) ) ;
#29346 = CARTESIAN_POINT ( 'NONE',  ( 0.7623938366894518204, -1.325735992016435105, 1.255310662410371592 ) ) ;
#29347 = CARTESIAN_POINT ( 'NONE',  ( 1.823171247573553311, 2.059948494222668458, 0.7922594597074559264 ) ) ;
#29348 = DIRECTION ( 'NONE',  ( 0.000000000000000000, 0.000000000000000000, 1.000000000000000000 ) ) ;
#29349 = CARTESIAN_POINT ( 'NONE',  ( 0.03522015555855115276, -0.09184495783944729430, 1.910282976853895587 ) ) ;
#29350 = VERTEX_POINT ( 'NONE', #51984 ) ;
#29351 = CIRCLE ( 'NONE', #157227, 2.350000000000007194 ) ;
#29352 = CARTESIAN_POINT ( 'NONE',  ( 0.2737963954951051493, -1.932246063674218473, 0.3805649573235761474 ) ) ;
#29353 = CARTESIAN_POINT ( 'NONE',  ( 1.276788482218065734, 1.793752796627584578, -0.7448022267775021854 ) ) ;
#29354 = ORIENTED_EDGE ( 'NONE', *, *, #19442, .T. ) ;
#29355 = CARTESIAN_POINT ( 'NONE',  ( 0.5794536021234627521, 1.392335491182377316, -1.458330535474762213 ) ) ;
#29357 = CARTESIAN_POINT ( 'NONE',  ( 5.102340918953698790, 1.855823733615385551, 0.1392438295388219172 ) ) ;
#29356 = CARTESIAN_POINT ( 'NONE',  ( -6.791708605802965870, 6.888357893050385705, -0.7998128361456362523 ) ) ;
#29358 = CARTESIAN_POINT ( 'NONE',  ( 4.875038752565570732, 7.845239757038595663, -1.199719254218452047 ) ) ;
#29359 = CARTESIAN_POINT ( 'NONE',  ( 0.7500000000000006661, 11.41666666666666607, -1.299038105676657340 ) ) ;
#29360 = CARTESIAN_POINT ( 'NONE',  ( 6.509000000000037645, 2.054060622569788386, 2.307050226316338382 ) ) ;
#29361 = CARTESIAN_POINT ( 'NONE',  ( -6.227272627378437342, 6.159572908229946187, -0.7998128361456291469 ) ) ;
#29362 = CARTESIAN_POINT ( 'NONE',  ( -5.589704470584107909, 9.743348658981940247, -0.7998128361456362523 ) ) ;
#29363 = CARTESIAN_POINT ( 'NONE',  ( 1.945129482973105839, -1.762486321751283835, -1.302348873264857820 ) ) ;
#29364 = CARTESIAN_POINT ( 'NONE',  ( 2.711267533052988732, 6.106969855296372707, -0.7216878364870267237 ) ) ;
#29365 = CARTESIAN_POINT ( 'NONE',  ( 5.677832469072920496, 9.846164657218904992, 0.000000000000000000 ) ) ;
#29366 = CARTESIAN_POINT ( 'NONE',  ( -1.500000000000008216, 8.500000000000000000, 3.469446951953614189E-15 ) ) ;
#29367 = CARTESIAN_POINT ( 'NONE',  ( 3.088313589057069208, -1.798746773638896457, -0.3115406389907551810 ) ) ;
#29368 = FACE_OUTER_BOUND ( 'NONE', #145751, .T. ) ;
#29369 = CARTESIAN_POINT ( 'NONE',  ( -4.762992037102518950, 4.451245552908022596, -0.7998128361456221525 ) ) ;
#29370 = CARTESIAN_POINT ( 'NONE',  ( -6.481153920547079395, 6.846182452143763086, -0.6414432093310319383 ) ) ;
#29371 = CARTESIAN_POINT ( 'NONE',  ( -3.947104627881229622, 8.980740528189222971, 0.7749999999999996891 ) ) ;
#29372 = AXIS2_PLACEMENT_3D ( 'NONE', #91664, #40768, #58061 ) ;
#29373 = CARTESIAN_POINT ( 'NONE',  ( 9.728138913005292210, 11.30824913904973705, -1.199719254218440723 ) ) ;
#29374 = CARTESIAN_POINT ( 'NONE',  ( 1.084454569787800304, -1.879374161238209773, -0.4228483607967240543 ) ) ;
#29375 = CARTESIAN_POINT ( 'NONE',  ( 5.787936641206399280, -1.241742415844361291, -1.518776266119965745 ) ) ;
#29376 = CARTESIAN_POINT ( 'NONE',  ( -7.823218330285243383, 9.085841792542966644, -1.199719254218446718 ) ) ;
#29377 = CARTESIAN_POINT ( 'NONE',  ( 4.449046963578762615, 8.342305224150557308, -0.7998128361456231517 ) ) ;
#29378 = CARTESIAN_POINT ( 'NONE',  ( 5.196902890030515643, 1.791362914573800369, 1.262263373074036688 ) ) ;
#29379 = PRESENTATION_LAYER_ASSIGNMENT (  '', '', ( #91564 ) ) ;
#29380 = CARTESIAN_POINT ( 'NONE',  ( 4.053524740805938720, 3.831459740469437936, 1.214306433183764966E-14 ) ) ;
#29382 = ADVANCED_FACE ( 'NONE', ( #55175 ), #22644, .T. ) ;
#29381 = CARTESIAN_POINT ( 'NONE',  ( 3.924723049676182018, -1.394041313093749457, 1.530695986988837021 ) ) ;
#29384 = CARTESIAN_POINT ( 'NONE',  ( 1.364683531249986537, 0.7177083336747527298, -0.7879004041258239610 ) ) ;
#29383 = SURFACE_SIDE_STYLE ('',( #142097 ) ) ;
#29385 = EDGE_LOOP ( 'NONE', ( #1258, #38347, #171331, #6860 ) ) ;
#29386 = CARTESIAN_POINT ( 'NONE',  ( 4.324990310505356206, 0.9834070133523404866, -2.077815080336536280 ) ) ;
#29388 = ORIENTED_EDGE ( 'NONE', *, *, #103873, .F. ) ;
#29387 = CARTESIAN_POINT ( 'NONE',  ( 8.446366511633696561, 8.956441806435218922, 1.040834085586084257E-14 ) ) ;
#29390 = CARTESIAN_POINT ( 'NONE',  ( -3.285556943750000514, -1.188541666188710044, -1.896917185911906500 ) ) ;
#29389 = CARTESIAN_POINT ( 'NONE',  ( 7.038091139269835317, 7.383730215335837954, 0.000000000000000000 ) ) ;
#29391 = DIRECTION ( 'NONE',  ( 0.000000000000000000, 0.000000000000000000, -1.000000000000000000 ) ) ;
#29392 = DIRECTION ( 'NONE',  ( 1.000000000000000000, -7.771561172376097755E-16, -4.440892098500627148E-16 ) ) ;
#29393 = CARTESIAN_POINT ( 'NONE',  ( 3.644416830925560014, -1.587075459539259992, 1.118831915631451013 ) ) ;
#29394 = ORIENTED_EDGE ( 'NONE', *, *, #2690, .T. ) ;
#29396 = CARTESIAN_POINT ( 'NONE',  ( 3.701012746850603996, 7.261672604726938651, 1.040834085586084257E-14 ) ) ;
#29395 = AXIS2_PLACEMENT_3D ( 'NONE', #32284, #46412, #112528 ) ;
#29397 = ORIENTED_EDGE ( 'NONE', *, *, #125755, .F. ) ;
#29398 = CARTESIAN_POINT ( 'NONE',  ( 4.763870730211980487, 0.5944114921396548290, -1.817767169311027997 ) ) ;
#29399 = DIRECTION ( 'NONE',  ( -0.000000000000000000, -1.000000000000000000, -0.000000000000000000 ) ) ;
#29400 = CARTESIAN_POINT ( 'NONE',  ( 6.352575194690796678, 0.5466354793271388512, 1.635951794362877187 ) ) ;
#29401 = CARTESIAN_POINT ( 'NONE',  ( 4.241422899474024177, 0.4370803545316758743, -1.968444674787086734 ) ) ;
#29402 = LINE ( 'NONE', #81340, #191209 ) ;
#29403 = CARTESIAN_POINT ( 'NONE',  ( 2.385638622766753425, 2.017150886971270651, -0.8956362484653990208 ) ) ;
#29405 = CARTESIAN_POINT ( 'NONE',  ( 1.284279953904126748, 10.64264068711930733, 0.7750000000000013545 ) ) ;
#29404 = DIRECTION ( 'NONE',  ( 0.000000000000000000, 0.000000000000000000, 1.000000000000000000 ) ) ;
#29407 = CARTESIAN_POINT ( 'NONE',  ( 6.626229037604012717, 1.016508351997437165, -1.448449474740549858 ) ) ;
#29406 = CARTESIAN_POINT ( 'NONE',  ( 1.816468492311611893, 1.951142502984483107, 0.7513475392508098816 ) ) ;
#29408 = CARTESIAN_POINT ( 'NONE',  ( 5.977185442992979603, -2.006959616289708315, -0.1948445219252663840 ) ) ;
#29409 = EDGE_CURVE ( 'NONE', #179385, #194999, #169810, .T. ) ;
#29411 = CARTESIAN_POINT ( 'NONE',  ( 2.730776445121200435, 0.2818232878892740212, 2.274813446668845884 ) ) ;
#29410 = CARTESIAN_POINT ( 'NONE',  ( 6.249382461256315580, 6.255644057745969988, -0.7998128361456481317 ) ) ;
#29412 = CARTESIAN_POINT ( 'NONE',  ( 1.095196197045473774, -1.740516465796032586, -0.003461242977918776564 ) ) ;
#29413 = CARTESIAN_POINT ( 'NONE',  ( 0.2999999999999565237, 3.372708439410121439, 0.4999999999999553690 ) ) ;
#29414 = CARTESIAN_POINT ( 'NONE',  ( 1.211752002169782738, -1.362220228754877027, -1.072495211514002289 ) ) ;
#29415 = CARTESIAN_POINT ( 'NONE',  ( 0.6801582343749865700, 0.08854166700808518975, -1.178068619123869398 ) ) ;
#29416 = CARTESIAN_POINT ( 'NONE',  ( -11.41108574530292863, 12.34163144622367270, 3.405883542057530633 ) ) ;
#29417 = CARTESIAN_POINT ( 'NONE',  ( 1.768284035615394600, -2.154879749829127444, 0.2648707735025003229 ) ) ;
#29418 = CARTESIAN_POINT ( 'NONE',  ( 1.868375392651611122, -1.978555653031977446, -0.3886301775877995524 ) ) ;
#29419 = CARTESIAN_POINT ( 'NONE',  ( 4.687500000000003553, -1.451031289060926488, 1.451031289061301521 ) ) ;
#29420 = CARTESIAN_POINT ( 'NONE',  ( -0.7500000000000215383, 1.722916667349486008, 1.299038105676659116 ) ) ;
#29421 = CARTESIAN_POINT ( 'NONE',  ( 0.08292192553204823235, -0.1316706149618769306, -1.895886810074402185 ) ) ;
#29422 = CARTESIAN_POINT ( 'NONE',  ( -1.364683531250000748, 13.35937500034139980, 0.000000000000000000 ) ) ;
#29423 = CARTESIAN_POINT ( 'NONE',  ( 3.744553100839841608, 1.186064971860462114, -1.878093021827110354 ) ) ;
#29424 = VERTEX_POINT ( 'NONE', #122400 ) ;
#29425 = CARTESIAN_POINT ( 'NONE',  ( -9.579089671862764277, -9.990657512341117652, 0.1108584966531582228 ) ) ;
#29426 = DIRECTION ( 'NONE',  ( 0.000000000000000000, 0.000000000000000000, 1.000000000000000000 ) ) ;
#29427 = CARTESIAN_POINT ( 'NONE',  ( 8.751951852821344247, 10.16936423550178503, -1.199719254218446718 ) ) ;
#29428 = B_SPLINE_CURVE_WITH_KNOTS ( 'NONE', 3,
 ( #87366, #35394, #34330, #101471, #19141, #137197, #70009, #18065, #149153, #100405, #66798, #116711, #121018, #51673, #136125, #169673, #117794, #50588 ),
 .UNSPECIFIED., .F., .F.,
 ( 4, 2, 2, 2, 2, 2, 2, 2, 4 ),
 ( 0.8245435890462745609, 0.8388218094160719840, 0.8531000297858694070, 0.8673782501556668301, 0.8816564705254642531, 0.8959346908952616761, 0.9102129112650590992, 0.9244911316348565222, 0.9387693520046538342 ),
 .UNSPECIFIED. ) ;
#29429 = CARTESIAN_POINT ( 'NONE',  ( 5.513164599239865460, -1.696177307367072506, 0.3892859123911066588 ) ) ;
#29430 = CARTESIAN_POINT ( 'NONE',  ( 4.105873170248697690, 0.6631157982108953908, -1.846516426336957784 ) ) ;
#29432 = CARTESIAN_POINT ( 'NONE',  ( -5.694061328059534688, 8.626526735169329996, 1.082531754730548412 ) ) ;
#29431 = CARTESIAN_POINT ( 'NONE',  ( 3.277320446201373638, 4.846626492033466072, 1.599625672291267398 ) ) ;
#29433 = CARTESIAN_POINT ( 'NONE',  ( -1.399605654164548296, 4.349233160595044723, -0.07230550894161411057 ) ) ;
#29434 = CARTESIAN_POINT ( 'NONE',  ( 4.306154650063803935, -2.256721687276264099, 0.1609511959119753199 ) ) ;
#29435 = CARTESIAN_POINT ( 'NONE',  ( 2.119651477787509730, 0.3549358516394903740, -2.031769927719127455 ) ) ;
#29436 = CARTESIAN_POINT ( 'NONE',  ( -5.533699252672048985, 9.607732894759390518, -0.7998128361456231517 ) ) ;
#29437 = EDGE_CURVE ( 'NONE', #169582, #206352, #208541, .T. ) ;
#29438 = CARTESIAN_POINT ( 'NONE',  ( 2.817521562391828827, -0.2228243041610066255, 2.251526839675880520 ) ) ;
#29439 = ORIENTED_EDGE ( 'NONE', *, *, #139829, .F. ) ;
#29440 = CARTESIAN_POINT ( 'NONE',  ( 1.499999999999989120, 1.806250000682817269, 0.000000000000000000 ) ) ;
#29441 = CARTESIAN_POINT ( 'NONE',  ( 3.497188413392815498, 1.472618687456558773, 1.153256759092120554 ) ) ;
#29442 = CARTESIAN_POINT ( 'NONE',  ( 2.408496482339622879, -0.9999731500247920346, -1.416544738438466400 ) ) ;
#29443 = CARTESIAN_POINT ( 'NONE',  ( 6.040607902356621928, -1.852314659301615096, 1.170993205287726990 ) ) ;
#29444 = CARTESIAN_POINT ( 'NONE',  ( 6.827182134110238110, -0.009824402486291110986, 2.288967694407697984 ) ) ;
#29445 = CARTESIAN_POINT ( 'NONE',  ( 3.485389320157119997, 1.955090977548096687, -0.9225387301767663528 ) ) ;
#29446 = CARTESIAN_POINT ( 'NONE',  ( 4.910071578948462800, 1.337895470842176193, -1.407775065355970412 ) ) ;
#29447 = CARTESIAN_POINT ( 'NONE',  ( -10.49131193887636826, 11.13428543831092909, 1.040834085586084257E-14 ) ) ;
#29448 = CARTESIAN_POINT ( 'NONE',  ( 6.432864026670258362, 0.1834693771665257822, 1.861492386831371748 ) ) ;
#29449 = CARTESIAN_POINT ( 'NONE',  ( 4.525353972290461435, 6.990290696447242880, 1.167197606177571734 ) ) ;
#29450 = DIRECTION ( 'NONE',  ( 0.000000000000000000, 1.000000000000000000, 0.000000000000000000 ) ) ;
#29451 = CARTESIAN_POINT ( 'NONE',  ( 4.909461021924256485, 4.900328411765999981, 0.7216878364870338292 ) ) ;
#29452 = CARTESIAN_POINT ( 'NONE',  ( 0.6801582343749987825, 2.557291667008069869, -1.178068619123886718 ) ) ;
#29453 = CARTESIAN_POINT ( 'NONE',  ( 5.274064633610318076, 1.777012466945230962, -0.9530095070046653571 ) ) ;
#29454 = CARTESIAN_POINT ( 'NONE',  ( -10.49131193887636826, 11.13428543831092909, 1.040834085586084257E-14 ) ) ;
#29455 = CARTESIAN_POINT ( 'NONE',  ( 8.633844893804129228, 8.967240552393299424, -0.7998128361456211532 ) ) ;
#29456 = FACE_OUTER_BOUND ( 'NONE', #193940, .T. ) ;
#29457 = CARTESIAN_POINT ( 'NONE',  ( 3.158640206316553289, -1.382037546686708973, 1.193037399656725395 ) ) ;
#29458 = CARTESIAN_POINT ( 'NONE',  ( 2.116530880626496192, -1.040147864624408003, -1.946245422063937802 ) ) ;
#29459 = ORIENTED_EDGE ( 'NONE', *, *, #166273, .F. ) ;
#29460 = CARTESIAN_POINT ( 'NONE',  ( -6.102578539482539810, 6.292298848917299736, 0.000000000000000000 ) ) ;
#29461 = CARTESIAN_POINT ( 'NONE',  ( 0.000000000000000000, -3.784374999522044369, -3.793834371823813001 ) ) ;
#29462 = CARTESIAN_POINT ( 'NONE',  ( -7.320512876374914768, 10.62801655815766999, 1.199719254218453823 ) ) ;
#29463 = CARTESIAN_POINT ( 'NONE',  ( 1.230729765704338563, 1.353420925896263061, -1.499466043412321703 ) ) ;
#29464 = CARTESIAN_POINT ( 'NONE',  ( 1.313308151137903224, 1.731519532738003297, -1.223779428986125462 ) ) ;
#29465 = CARTESIAN_POINT ( 'NONE',  ( -6.473091995881817162, 6.516638514809040217, 0.7998128361456281477 ) ) ;
#29466 = CARTESIAN_POINT ( 'NONE',  ( 2.113880859634624354, 1.856391821545114951, -0.1307286092924550835 ) ) ;
#29467 = CARTESIAN_POINT ( 'NONE',  ( 5.678167406024951624, 5.518950149984223508, 0.7998128361456341429 ) ) ;
#29468 = CARTESIAN_POINT ( 'NONE',  ( 6.578986920187222864, -0.09832028258810160404, -2.058664976587327722 ) ) ;
#29469 = CARTESIAN_POINT ( 'NONE',  ( 6.047500043413473136, -1.423963828944514010, 1.427935028000301809 ) ) ;
#29470 = ORIENTED_EDGE ( 'NONE', *, *, #202242, .F. ) ;
#29471 = ORIENTED_EDGE ( 'NONE', *, *, #73420, .T. ) ;
#29472 = VERTEX_POINT ( 'NONE', #5311 ) ;
#29473 = CARTESIAN_POINT ( 'NONE',  ( -9.592557376868645846, 11.15007068022363157, -1.199719254218441611 ) ) ;
#29474 = CARTESIAN_POINT ( 'NONE',  ( 4.424309136736732206, 1.121156565774838354, -1.440799707636587712 ) ) ;
#29476 = CARTESIAN_POINT ( 'NONE',  ( -5.904496024515287544, 6.143719773163115683, -0.8530293227379917020 ) ) ;
#29475 = CARTESIAN_POINT ( 'NONE',  ( -3.955946960137363799, 7.837298230127379917, 0.7998128361456352531 ) ) ;
#29477 = CARTESIAN_POINT ( 'NONE',  ( 6.589288424369031283, 6.777081280454712697, 0.2339771526987007022 ) ) ;
#29478 = CARTESIAN_POINT ( 'NONE',  ( 6.520861224751243412, 2.010896128390584625, -0.1455136175190149816 ) ) ;
#29479 = CARTESIAN_POINT ( 'NONE',  ( 6.333933918656591722, 1.821832875601756774, 0.2651207078676054429 ) ) ;
#29480 = CARTESIAN_POINT ( 'NONE',  ( -10.99970480893081870, -5.907420853759282053, -0.08058608058607828750 ) ) ;
#29481 = CARTESIAN_POINT ( 'NONE',  ( 4.248838534556359292, 0.6131519058680062750, 2.224680453567278171 ) ) ;
#29482 = CARTESIAN_POINT ( 'NONE',  ( 6.554440917563797875, 6.611545590104705994, -0.7998128361456481317 ) ) ;
#29483 = CARTESIAN_POINT ( 'NONE',  ( 6.063787883973515314, 2.130759124531961923, -0.3628933549372145295 ) ) ;
#29484 = CARTESIAN_POINT ( 'NONE',  ( 0.8724827243445825165, -0.04916951280507049493, -1.941606035699546151 ) ) ;
#29485 = VERTEX_POINT ( 'NONE', #69259 ) ;
#29486 = CARTESIAN_POINT ( 'NONE',  ( 4.481968937923656249, 2.098976780363570604, 0.9367997793626892111 ) ) ;
#29487 = FACE_OUTER_BOUND ( 'NONE', #59958, .T. ) ;
#29489 = AXIS2_PLACEMENT_3D ( 'NONE', #167630, #169760, #101562 ) ;
#29488 = CARTESIAN_POINT ( 'NONE',  ( -4.167152111353897403, 5.955039778036558040, 1.599625672291270506 ) ) ;
#29490 = CARTESIAN_POINT ( 'NONE',  ( 4.996879044411707937, 1.554903924810165705, -1.039696167511289238 ) ) ;
#29491 = ORIENTED_EDGE ( 'NONE', *, *, #2591, .F. ) ;
#29494 = CARTESIAN_POINT ( 'NONE',  ( -4.098307573080856692, 8.003385611894792362, 0.7998128361456352531 ) ) ;
#29493 = CARTESIAN_POINT ( 'NONE',  ( -1.402160292154681736E-14, 0.1187500006828157706, -1.732050807568870754 ) ) ;
#29492 = CARTESIAN_POINT ( 'NONE',  ( 1.916128293556786044, -1.911906470838855343, 0.05044092668918254141 ) ) ;
#29495 = CARTESIAN_POINT ( 'NONE',  ( 4.283934280384479543, 1.440456688004333019, 1.672026782002330458 ) ) ;
#29496 = CARTESIAN_POINT ( 'NONE',  ( 6.883263157960401557, 3.701933627517115966, 2.360572570571787043 ) ) ;
#29497 = CARTESIAN_POINT ( 'NONE',  ( 0.000000000000000000, -0.5000000000000004441, 2.000000000000000000 ) ) ;
#29498 = CARTESIAN_POINT ( 'NONE',  ( 6.387299765369506055, 7.584842826753462219, -1.082531754730548412 ) ) ;
#29499 = CARTESIAN_POINT ( 'NONE',  ( -4.308793891044708779, 3.921347715840572956, 1.214306433183764966E-14 ) ) ;
#29500 = CARTESIAN_POINT ( 'NONE',  ( -7.241463443030476732, 7.620997903056574430, 0.000000000000000000 ) ) ;
#29501 = CARTESIAN_POINT ( 'NONE',  ( 1.141796867408477967, 0.8028701493673767731, -1.800646566474963572 ) ) ;
#29502 = CARTESIAN_POINT ( 'NONE',  ( 0.9390046912478089425, 2.274041295854188238, 0.3912414073941206105 ) ) ;
#29503 = CARTESIAN_POINT ( 'NONE',  ( 2.207404936347991065, -1.573848641742966459, -1.171066219227391070 ) ) ;
#29504 = CARTESIAN_POINT ( 'NONE',  ( 11.41381678389397614, 11.02879418241070830, 3.704697885617693753 ) ) ;
#29505 = CARTESIAN_POINT ( 'NONE',  ( 5.805554948619430000, -1.622591123950654746, -1.273203187973567241 ) ) ;
#29506 = CARTESIAN_POINT ( 'NONE',  ( 5.504247177468186258, 6.484338464210099851, 1.082531754730558626 ) ) ;
#29507 = CARTESIAN_POINT ( 'NONE',  ( 5.890091390494168522, 5.836471141856793388, 0.000000000000000000 ) ) ;
#29508 = ORIENTED_EDGE ( 'NONE', *, *, #53132, .T. ) ;
#29509 = DIRECTION ( 'NONE',  ( -1.000000000000000000, 5.578564026256504688E-16, 1.479114197289397135E-31 ) ) ;
#29510 = DIRECTION ( 'NONE',  ( 1.000000000000000000, -0.000000000000000000, -0.000000000000000000 ) ) ;
#29511 = CARTESIAN_POINT ( 'NONE',  ( 2.358755538653318773, 5.695705861830088423, 1.040834085586084257E-14 ) ) ;
#29512 = CARTESIAN_POINT ( 'NONE',  ( 0.6730172731169652423, 1.498246551899045098, -1.571433807820749706 ) ) ;
#29513 = CARTESIAN_POINT ( 'NONE',  ( 6.540882763950133238, 6.595727744222092959, 0.000000000000000000 ) ) ;
#29514 = CARTESIAN_POINT ( 'NONE',  ( 11.20845505065560666, 1.972237431423869314, -3.641847810296739762 ) ) ;
#29515 = CARTESIAN_POINT ( 'NONE',  ( -6.141084208779844289, 5.378569653125054195, -2.500000000000000888 ) ) ;
#29516 = CARTESIAN_POINT ( 'NONE',  ( 2.512791842090915218, 1.668957736969980621, 0.8448945032545759348 ) ) ;
#29517 = CARTESIAN_POINT ( 'NONE',  ( 0.3685255395303523307, -1.348100972195030334, 1.558720748697209224 ) ) ;
#29519 = CARTESIAN_POINT ( 'NONE',  ( 6.827182134110203471, 2.976138737189625516, 2.364467684523130497 ) ) ;
#29518 = CARTESIAN_POINT ( 'NONE',  ( -0.02224634325200240681, 0.6689394325187210111, -2.369055395299427769 ) ) ;
#29520 = CARTESIAN_POINT ( 'NONE',  ( -0.6823417656250246877, -0.4489583329919111243, 1.181850606188755259 ) ) ;
#29521 = CARTESIAN_POINT ( 'NONE',  ( 2.789602095257078584, 1.815147277589121533, -0.6018686165152677958 ) ) ;
#29522 = CARTESIAN_POINT ( 'NONE',  ( 4.065142161210800076, 0.2162087174472343276, -1.756520380257739822 ) ) ;
#29523 = STYLED_ITEM ( 'NONE', ( #171283 ), #94887 ) ;
#29524 = CARTESIAN_POINT ( 'NONE',  ( 2.209489775926488431, 1.479274643242427301, 1.211860329591994745 ) ) ;
#29525 = CARTESIAN_POINT ( 'NONE',  ( -3.744022975668147790, 7.519777238254810925, -0.7998128361456281477 ) ) ;
#29527 = CARTESIAN_POINT ( 'NONE',  ( 5.290618452874795707, 1.447395081947447704, -1.254909122497225971 ) ) ;
#29526 = LINE ( 'NONE', #26303, #177245 ) ;
#29528 = CARTESIAN_POINT ( 'NONE',  ( -1.402160292154681736E-14, -0.2874999999999741096, 1.732050807568877637 ) ) ;
#29529 = CARTESIAN_POINT ( 'NONE',  ( 6.514111218838506190, 1.964378047669375293, -0.1432920118879192073 ) ) ;
#29530 = CARTESIAN_POINT ( 'NONE',  ( -1.500000000000011324, 4.879166666666690411, -0.8660254037844313801 ) ) ;
#29531 = SURFACE_STYLE_USAGE ( .BOTH. , #77196 ) ;
#29532 = CARTESIAN_POINT ( 'NONE',  ( 4.944154083221365070, 1.865701114312174225, 0.1370711555178441010 ) ) ;
#29534 = ORIENTED_EDGE ( 'NONE', *, *, #176534, .F. ) ;
#29533 = CARTESIAN_POINT ( 'NONE',  ( 1.435882461153328515, 0.9014729512111450127, -1.587519582607027635 ) ) ;
#29536 = CARTESIAN_POINT ( 'NONE',  ( 4.612778539632031105, 8.351152097327862123, 0.2683542610703564812 ) ) ;
#29535 = CARTESIAN_POINT ( 'NONE',  ( 4.934293700819583073, 1.136511309699510308, -1.891595316245115788 ) ) ;
#29537 = EDGE_CURVE ( 'NONE', #45069, #194295, #200406, .T. ) ;
#29538 = CARTESIAN_POINT ( 'NONE',  ( -1.201851678989727383E-14, 5.759375000341417028, -1.575800808251660801 ) ) ;
#29539 = CARTESIAN_POINT ( 'NONE',  ( 1.750508186522087062, -2.052535545683041196, -0.2044793282457678107 ) ) ;
#29540 = CARTESIAN_POINT ( 'NONE',  ( 6.311484202361478779, 7.322151976631905868, -1.199719254218446718 ) ) ;
#29541 = CARTESIAN_POINT ( 'NONE',  ( -8.636707547105197946, 10.03491254549959777, -1.199719254218446718 ) ) ;
#29542 = CARTESIAN_POINT ( 'NONE',  ( 1.364564222265990390, 4.014448417934980640, -0.6239050962421918145 ) ) ;
#29543 = FACE_OUTER_BOUND ( 'NONE', #79119, .T. ) ;
#29544 = CARTESIAN_POINT ( 'NONE',  ( 6.261886844665240481, 8.398896966899865646, 1.599625672291268286 ) ) ;
#29545 = ORIENTED_EDGE ( 'NONE', *, *, #194119, .T. ) ;
#29546 = CARTESIAN_POINT ( 'NONE',  ( 4.984861949208964305, 1.980195279717174905, 0.6042863919064264122 ) ) ;
#29547 = CARTESIAN_POINT ( 'NONE',  ( -1.364683531250014514, -0.6572916663252459379, 0.7879004041258379498 ) ) ;
#29548 = CARTESIAN_POINT ( 'NONE',  ( 2.144033130777025065, 0.8294244109963678779, -1.996327601563187670 ) ) ;
#29549 = CARTESIAN_POINT ( 'NONE',  ( -4.606260857482554982, 8.381206713624141713, 0.1075878075270080697 ) ) ;
#29550 = CARTESIAN_POINT ( 'NONE',  ( 2.912765130361310018, -0.5885411476599323732, -1.932001019476004888 ) ) ;
#29551 = CARTESIAN_POINT ( 'NONE',  ( 6.720655732516624070, 2.949086357957014570, 2.625980845328681923 ) ) ;
#29552 = ORIENTED_EDGE ( 'NONE', *, *, #69670, .F. ) ;
#29553 = AXIS2_PLACEMENT_3D ( 'NONE', #122154, #24547, #23481 ) ;
#29554 = VERTEX_POINT ( 'NONE', #70324 ) ;
#29556 = CARTESIAN_POINT ( 'NONE',  ( 7.958272981541723468, 8.386999354661243800, 1.040834085586084257E-14 ) ) ;
#29555 = CARTESIAN_POINT ( 'NONE',  ( 1.001543065824772753E-15, -1.662500000000000533, 4.012584370867899430 ) ) ;
#29557 = CARTESIAN_POINT ( 'NONE',  ( -3.634994581795317536, 7.254927755487573293, 0.000000000000000000 ) ) ;
#29558 = CARTESIAN_POINT ( 'NONE',  ( 1.323454262349360144, -1.463929862531298198, -1.387097294446784090 ) ) ;
#29559 = CARTESIAN_POINT ( 'NONE',  ( 6.058177568126345669, -1.550975213528119623, 1.548612826651605712 ) ) ;
#29560 = CARTESIAN_POINT ( 'NONE',  ( 1.499999999999989120, 4.285416667349482900, 0.8660254037844524744 ) ) ;
#29561 = CARTESIAN_POINT ( 'NONE',  ( 4.834190613173367623, -1.027981871586785889, -1.612434056610718480 ) ) ;
#29562 = CARTESIAN_POINT ( 'NONE',  ( -3.415764635639130020, 6.072476943965863683, 1.199719254218462483 ) ) ;
#29563 = CARTESIAN_POINT ( 'NONE',  ( 6.060131475184119765, 9.053608573481392696, -1.082531754730537976 ) ) ;
#29565 = CARTESIAN_POINT ( 'NONE',  ( 2.003530013310977242, -1.955168117277843898, 0.4926643476272293820 ) ) ;
#29564 = CARTESIAN_POINT ( 'NONE',  ( -7.659993601596706725, 11.88048360193076647, -0.7216878364870267237 ) ) ;
#29566 = CARTESIAN_POINT ( 'NONE',  ( 1.364683531249997417, 13.29687500034139980, 2.602085213965210642E-15 ) ) ;
#29567 = CARTESIAN_POINT ( 'NONE',  ( -4.085803189671902480, 5.860132702740892263, -1.599625672291271394 ) ) ;
#29568 = CARTESIAN_POINT ( 'NONE',  ( 5.543893992536840010, 0.6953672157433439249, -1.578584939873737047 ) ) ;
#29569 = DIRECTION ( 'NONE',  ( 0.000000000000000000, 1.000000000000000000, 0.000000000000000000 ) ) ;
#29570 = CARTESIAN_POINT ( 'NONE',  ( 4.532503425670185493, 4.182342172903648070, 1.214306433183764966E-14 ) ) ;
#29571 = DIRECTION ( 'NONE',  ( 2.345077562848782505E-16, 0.000000000000000000, 1.000000000000000000 ) ) ;
#29572 = CARTESIAN_POINT ( 'NONE',  ( 3.018661757337009810, 6.673522483535157868, 0.000000000000000000 ) ) ;
#29573 = DIRECTION ( 'NONE',  ( 0.000000000000000000, 0.000000000000000000, -1.000000000000000000 ) ) ;
#29574 = ORIENTED_EDGE ( 'NONE', *, *, #92378, .T. ) ;
#29575 = CARTESIAN_POINT ( 'NONE',  ( 1.393514648303464387, -1.873246724434135313, 0.8816542684770899418 ) ) ;
#29576 = ORIENTED_EDGE ( 'NONE', *, *, #65507, .F. ) ;
#29577 = CARTESIAN_POINT ( 'NONE',  ( 4.688045340743730804, 1.047092163662701525, 1.477968688824328858 ) ) ;
#29578 = CARTESIAN_POINT ( 'NONE',  ( 6.201928923608456046, 6.200281597156833691, 0.7998128361456352531 ) ) ;
#29580 = EDGE_CURVE ( 'NONE', #14623, #126234, #4254, .T. ) ;
#29579 = DIRECTION ( 'NONE',  ( -0.6507913734559640506, -0.7592566023653004592, 0.000000000000000000 ) ) ;
#29581 = CARTESIAN_POINT ( 'NONE',  ( 6.393201686769759640, -0.09647555762395694512, -1.809044896826275783 ) ) ;
#29582 = CARTESIAN_POINT ( 'NONE',  ( 4.543390873910903238, 7.354354215321133204, 1.082531754730548412 ) ) ;
#29583 = CARTESIAN_POINT ( 'NONE',  ( -0.9486429539237212216, 3.288339070649073381, -1.028101543438966425 ) ) ;
#29584 = CARTESIAN_POINT ( 'NONE',  ( 3.451304434523004172, 0.5324976444292061073, -2.125649318046138880 ) ) ;
#29585 = VERTEX_POINT ( 'NONE', #201394 ) ;
#29587 = CARTESIAN_POINT ( 'NONE',  ( 9.915090410295563927, 10.46202698829998567, -0.7998128361456281477 ) ) ;
#29586 = CARTESIAN_POINT ( 'NONE',  ( 0.7659737006216191801, -1.952758744216346765, 0.1886366088557633325 ) ) ;
#29588 = VECTOR ( 'NONE', #186120, 1000.000000000000000 ) ;
#29589 = CARTESIAN_POINT ( 'NONE',  ( 5.009359837557266992, -1.817519814519794830, 0.6052834035694378834 ) ) ;
#29590 = DIRECTION ( 'NONE',  ( 0.000000000000000000, -1.000000000000000000, 0.000000000000000000 ) ) ;
#29591 = ADVANCED_FACE ( 'NONE', ( #172128 ), #67560, .F. ) ;
#29592 = CARTESIAN_POINT ( 'NONE',  ( -0.4019237886466966447, 12.05133545031537068, 1.500000000000003997 ) ) ;
#29593 = CARTESIAN_POINT ( 'NONE',  ( 1.364683531249986537, -0.3864583329919166199, 0.7879004041258500513 ) ) ;
#29595 = ORIENTED_EDGE ( 'NONE', *, *, #127031, .T. ) ;
#29594 = CARTESIAN_POINT ( 'NONE',  ( 4.799223189557548785, 7.582548906917042864, -1.082531754730549078 ) ) ;
#29596 = CARTESIAN_POINT ( 'NONE',  ( -8.514157279702020631, 11.91663867875229776, -1.082531754730543971 ) ) ;
#29597 = CARTESIAN_POINT ( 'NONE',  ( 2.377987466095924152, 1.329388817951412394, 1.704534938537699995 ) ) ;
#29598 = CARTESIAN_POINT ( 'NONE',  ( -3.298376509874564988, 7.070132704820777825, 0.000000000000000000 ) ) ;
#29599 = CARTESIAN_POINT ( 'NONE',  ( 5.391302360089590628, 6.318882837306503575, -1.199719254218452047 ) ) ;
#29600 = CARTESIAN_POINT ( 'NONE',  ( 1.465546361252961560, 1.799214786004127209, -0.3081908958329632742 ) ) ;
#29601 = CARTESIAN_POINT ( 'NONE',  ( -4.437596350374534815, 4.071617251725375475, -0.7998128361456221525 ) ) ;
#29602 = CARTESIAN_POINT ( 'NONE',  ( 4.278209411971904075, -1.050932907216840295, 1.492538610026641344 ) ) ;
#29603 = CARTESIAN_POINT ( 'NONE',  ( 9.241773570968582874, 13.11902652889326504, 9.006041125820061666 ) ) ;
#29604 = VERTEX_POINT ( 'NONE', #162273 ) ;
#29605 = CARTESIAN_POINT ( 'NONE',  ( 4.369560876907440772, -0.3388413995694672387, 1.940020671193002810 ) ) ;
#29606 = ORIENTED_EDGE ( 'NONE', *, *, #146212, .T. ) ;
#29608 = B_SPLINE_CURVE_WITH_KNOTS ( 'NONE', 3,
 ( #19639, #53217, #1239, #86783, #186402, #51089, #165905, #83576, #117213, #70499 ),
 .UNSPECIFIED., .F., .F.,
 ( 4, 2, 2, 2, 4 ),
 ( 0.000000000000000000, 0.0002021113321160284890, 0.0004042226642320569780, 0.0006063339963480854399, 0.0008084453284641139560 ),
 .UNSPECIFIED. ) ;
#29607 = CARTESIAN_POINT ( 'NONE',  ( 6.480031042553710208, -1.905489079494159910, -0.3742900760800580984 ) ) ;
#29609 = EDGE_LOOP ( 'NONE', ( #76178, #210081, #51408, #197019 ) ) ;
#29610 = CARTESIAN_POINT ( 'NONE',  ( -5.912237504011027767, 9.055304967058290799, 1.199719254218454489 ) ) ;
#29612 = CARTESIAN_POINT ( 'NONE',  ( 5.168275554957600271, 2.118074532352266282, -0.1063875075708180934 ) ) ;
#29611 = CARTESIAN_POINT ( 'NONE',  ( 5.505492895601038938, 8.580769590579979678, -1.199719254218452047 ) ) ;
#29613 = CARTESIAN_POINT ( 'NONE',  ( 6.658462837642791676, 8.861568958707010779, 1.443375672974063439 ) ) ;
#29614 = VERTEX_POINT ( 'NONE', #784 ) ;
#29615 = CARTESIAN_POINT ( 'NONE',  ( 5.285422529909848066, 6.578444217690160301, -1.363614577128515082 ) ) ;
#29616 = DIRECTION ( 'NONE',  ( -5.578564026256490882E-16, -1.000000000000000000, -9.066213480720158442E-32 ) ) ;
#29617 = ORIENTED_EDGE ( 'NONE', *, *, #139381, .F. ) ;
#29618 = CARTESIAN_POINT ( 'NONE',  ( 3.553118775233146120, 6.302999783484076524, -1.199719254218453823 ) ) ;
#29619 = PRODUCT_RELATED_PRODUCT_CATEGORY ( 'part', '', ( #14337 ) ) ;
#29620 = CARTESIAN_POINT ( 'NONE',  ( 5.654944829759325664, 0.3949471196958070918, 1.973809479704929704 ) ) ;
#29622 =( BOUNDED_CURVE ( )  B_SPLINE_CURVE ( 2, ( #80036, #146139, #212152, #114740, #129946, #98429, #144024, #210019, #47571 ),
 .UNSPECIFIED., .F., .T. ) 
 B_SPLINE_CURVE_WITH_KNOTS ( ( 3, 2, 2, 2, 3 ),
 ( 0.6160714285714286031, 0.6190476190476190688, 0.6250000000000000000, 0.6309523809523809312, 0.6339285714285713969 ),
 .UNSPECIFIED. ) 
 CURVE ( )  GEOMETRIC_REPRESENTATION_ITEM ( )  RATIONAL_B_SPLINE_CURVE ( ( 0.9330127018922194093, 0.9330127018922194093, 1.000000000000000000, 0.8660254037844387076, 1.000000000000000000, 0.8660254037844387076, 1.000000000000000000, 0.9330127018922194093, 0.9330127018922194093 ) ) 
 REPRESENTATION_ITEM ( '' )  );
#29621 = CARTESIAN_POINT ( 'NONE',  ( 0.09481041353608110622, -9.919511983836045488, 9.499526882191826616 ) ) ;
#29623 = CARTESIAN_POINT ( 'NONE',  ( 6.287720257080702702, 1.262826302610157381, 1.318732360701305062 ) ) ;
#29624 = CARTESIAN_POINT ( 'NONE',  ( 1.117730493923989599, 0.4056601665377961852, -2.030061024271647252 ) ) ;
#29625 = CARTESIAN_POINT ( 'NONE',  ( -7.917598520700757980, 9.299915031314755609, 1.082531754730558626 ) ) ;
#29626 = CARTESIAN_POINT ( 'NONE',  ( -5.495582220874787538, 7.482514367559947033, -1.250084184017367539 ) ) ;
#29627 = CARTESIAN_POINT ( 'NONE',  ( 2.207884333776653740E-15, 1.500000000682816914, -1.225000000000019851 ) ) ;
#29628 = CARTESIAN_POINT ( 'NONE',  ( -3.285556943749998737, -2.880208332855377584, 1.896917185911908721 ) ) ;
#29629 = CARTESIAN_POINT ( 'NONE',  ( 6.908042961362778733, 8.018137195466769285, 1.199719254218462483 ) ) ;
#29630 = PRESENTATION_STYLE_ASSIGNMENT (( #144482 ) ) ;
#29631 = CARTESIAN_POINT ( 'NONE',  ( -1.402160292154681736E-14, 11.23437500034139980, 1.575800808251682339 ) ) ;
#29632 = CARTESIAN_POINT ( 'NONE',  ( -4.599240423533815125, 6.388866465587984322, 1.599625672291267398 ) ) ;
#29634 = CARTESIAN_POINT ( 'NONE',  ( -4.977251789548269301, 4.979417640660637190, 0.7216878364870257245 ) ) ;
#29633 = FACE_OUTER_BOUND ( 'NONE', #152879, .T. ) ;
#29636 = CARTESIAN_POINT ( 'NONE',  ( 3.603937110245566178, -0.1228517400825197836, 1.729840182746833266 ) ) ;
#29635 = AXIS2_PLACEMENT_3D ( 'NONE', #106432, #135689, #169241 ) ;
#29637 = CARTESIAN_POINT ( 'NONE',  ( -3.405069135326500351, 7.124331091189553433, 1.040834085586084257E-14 ) ) ;
#29638 = CARTESIAN_POINT ( 'NONE',  ( 1.551716534671506498, 1.565040117424065347, 1.355267069636761912 ) ) ;
#29639 = CARTESIAN_POINT ( 'NONE',  ( 2.232168359954420200, 2.116822148135434567, 0.04868514642705767947 ) ) ;
#29640 = CARTESIAN_POINT ( 'NONE',  ( 4.273844736805816780, 6.009238164405336313, 1.599625672291267398 ) ) ;
#29641 = STYLED_ITEM ( 'NONE', ( #357 ), #192497 ) ;
#29642 = CARTESIAN_POINT ( 'NONE',  ( 9.250740883225924804, 9.686952540052077509, 1.040834085586084257E-14 ) ) ;
#29643 = LINE ( 'NONE', #28569, #111790 ) ;
#29644 = CARTESIAN_POINT ( 'NONE',  ( 0.8659821450925162534, -1.960479642884611629, 0.1873741036552133976 ) ) ;
#29645 = CARTESIAN_POINT ( 'NONE',  ( 4.093767505759832837, 7.703081727663242617, 0.6588811006658854552 ) ) ;
#29646 = CARTESIAN_POINT ( 'NONE',  ( 4.365362273920238678, 7.076377838673507448, 1.082531754730558626 ) ) ;
#29648 = DIRECTION ( 'NONE',  ( 0.000000000000000000, 1.000000000000000000, 0.000000000000000000 ) ) ;
#29647 = CARTESIAN_POINT ( 'NONE',  ( -1.737499999999997824, -0.9916666666666684726, 3.009438278150925683 ) ) ;
#29649 = CARTESIAN_POINT ( 'NONE',  ( 2.625266749315146253, -2.138330473123546405, 0.8262727722977771805 ) ) ;
#29650 = CARTESIAN_POINT ( 'NONE',  ( 0.5217476098421744979, -0.9739702522407606144, -1.544006022310390192 ) ) ;
#29651 = CARTESIAN_POINT ( 'NONE',  ( 3.550944491985886575, 0.2853618425060593378, 1.890879049853078087 ) ) ;
#29652 = CARTESIAN_POINT ( 'NONE',  ( 6.801350335910821165, 7.963938809097990124, 1.199719254218452047 ) ) ;
#29653 = CARTESIAN_POINT ( 'NONE',  ( 7.578644679914706472, 9.864838098032418401, 1.443375672974076540 ) ) ;
#29654 = CARTESIAN_POINT ( 'NONE',  ( 1.951433385020440836, -1.796364150513751312, 0.9090842167202308755 ) ) ;
#29655 = CARTESIAN_POINT ( 'NONE',  ( 2.149198318390078910, 1.709348667602617722, -0.9624241554767107854 ) ) ;
#29656 = CARTESIAN_POINT ( 'NONE',  ( -9.996439331977562404, 10.55693406359564790, 0.7998128361456462443 ) ) ;
#29657 = CARTESIAN_POINT ( 'NONE',  ( -6.958359152311683893, 9.141171649162195934, -1.599625672291263179 ) ) ;
#29658 = CARTESIAN_POINT ( 'NONE',  ( -10.84253909858433218, 4.919570308430900596, -5.035411995924089723 ) ) ;
#29660 = CARTESIAN_POINT ( 'NONE',  ( 3.678344558940789266, -1.705506331563589661, -0.4725282708486245875 ) ) ;
#29659 = CARTESIAN_POINT ( 'NONE',  ( 5.173812367756161379, -1.161941297927127525, 1.737786252440294055 ) ) ;
#29661 = CARTESIAN_POINT ( 'NONE',  ( -9.117697077659110860, 16.00000000000574829, 7.299999999990590460 ) ) ;
#29662 = EDGE_CURVE ( 'NONE', #101381, #74826, #134050, .T. ) ;
#29664 = CARTESIAN_POINT ( 'NONE',  ( 6.580031643469963498, -2.246689805010111396, -0.4540597329640746471 ) ) ;
#29663 = FACE_OUTER_BOUND ( 'NONE', #170730, .T. ) ;
#29665 = CARTESIAN_POINT ( 'NONE',  ( 4.118918040174416539, -1.664481161445837687, 0.5081549729096886958 ) ) ;
#29666 = CARTESIAN_POINT ( 'NONE',  ( 7.716561984472250835, 12.15440608185967086, 1.040834085586084257E-14 ) ) ;
#29667 = CARTESIAN_POINT ( 'NONE',  ( -0.1104750535120268828, 2.006893987364383403, -2.517811492722863864 ) ) ;
#29668 = CARTESIAN_POINT ( 'NONE',  ( 4.130049176863603400, 0.2125952495928511154, -1.720681531008328768 ) ) ;
#29669 = CARTESIAN_POINT ( 'NONE',  ( 5.213404077426219807, -1.831445439253748031, -1.165863444158367290 ) ) ;
#29670 = CARTESIAN_POINT ( 'NONE',  ( 2.361091307074211887, 5.906356958228550447, 0.7998128361456462443 ) ) ;
#29671 = CARTESIAN_POINT ( 'NONE',  ( 5.507046092540283766, -0.04465857163906890998, 2.016188657829049991 ) ) ;
#29672 = CARTESIAN_POINT ( 'NONE',  ( 5.343750000000003553, 1.895863743164196258, 0.7852924748297027691 ) ) ;
#29673 = CARTESIAN_POINT ( 'NONE',  ( -0.7500000000000215383, 5.222916667349482012, 1.299038105676671107 ) ) ;
#29674 = CARTESIAN_POINT ( 'NONE',  ( 2.748949809783503451, -1.602600522849004339, 1.068665135549841771 ) ) ;
#29675 = CARTESIAN_POINT ( 'NONE',  ( -1.500000000000015099, 10.51041666734946034, -0.8660254037844309360 ) ) ;
#29676 = CARTESIAN_POINT ( 'NONE',  ( 6.345936316318473658, -1.449877878406122145, -1.683046035897132420 ) ) ;
#29677 = ORIENTED_EDGE ( 'NONE', *, *, #190890, .F. ) ;
#29678 = CARTESIAN_POINT ( 'NONE',  ( 6.883263157960405998, 2.961743250487959056, 2.498998094365055600 ) ) ;
#29679 = CARTESIAN_POINT ( 'NONE',  ( 0.7499999999999902300, 2.483333333333351156, 1.299038105676669330 ) ) ;
#29680 = CARTESIAN_POINT ( 'NONE',  ( 5.636439174979242850, 7.598931675607687453, -1.599625672291262513 ) ) ;
#29681 = CARTESIAN_POINT ( 'NONE',  ( 2.596574818557799258, -1.139633321999042659, 1.906535983277869661 ) ) ;
#29682 = CARTESIAN_POINT ( 'NONE',  ( 0.000000000000000000, 11.29999999999998117, 0.000000000000000000 ) ) ;
#29683 = CARTESIAN_POINT ( 'NONE',  ( 7.212574532790092974, 9.437756259720353924, -1.443375672974057666 ) ) ;
#29684 = CARTESIAN_POINT ( 'NONE',  ( -10.15469386651127515, 11.90985960142705657, 1.082531754730558626 ) ) ;
#29685 = CARTESIAN_POINT ( 'NONE',  ( 3.715816618597135523, 6.492813934075403637, -1.199719254218453823 ) ) ;
#29686 = B_SPLINE_CURVE_WITH_KNOTS ( 'NONE', 3,
 ( #71579, #185339, #18574, #169098, #20696, #4434, #136619, #202645, #54294, #21750 ),
 .UNSPECIFIED., .F., .F.,
 ( 4, 2, 2, 2, 4 ),
 ( 0.000000000000000000, 0.0002299353307164169933, 0.0004598706614328339866, 0.0006898059921492511425, 0.0009197413228656684068 ),
 .UNSPECIFIED. ) ;
#29687 = CARTESIAN_POINT ( 'NONE',  ( 1.108046318188542489, -0.04667474159409169127, 2.016033875899234662 ) ) ;
#29689 = CARTESIAN_POINT ( 'NONE',  ( 5.600070422683368854, 0.8392489243487236683, -1.884408887491027196 ) ) ;
#29688 = CARTESIAN_POINT ( 'NONE',  ( 9.562578416340237197, 10.05076299535211781, 0.7998128361456462443 ) ) ;
#29690 = CARTESIAN_POINT ( 'NONE',  ( 4.879147978569815969, 4.879180288469956217, -0.1512534140984626019 ) ) ;
#29691 = CARTESIAN_POINT ( 'NONE',  ( -4.762992037102518950, 4.451245552908022596, -0.7998128361456221525 ) ) ;
#29692 = B_SPLINE_CURVE_WITH_KNOTS ( 'NONE', 3,
 ( #164537, #49715, #131040, #65930, #132079, #16123, #133137, #148300 ),
 .UNSPECIFIED., .F., .F.,
 ( 4, 2, 2, 4 ),
 ( 2.179219396325681589E-18, 0.0002925934901276173745, 0.0005851869802552325806, 0.001170373960510463426 ),
 .UNSPECIFIED. ) ;
#29693 = CARTESIAN_POINT ( 'NONE',  ( 1.499999999999989120, 5.077083334016151639, -0.8660254037844323793 ) ) ;
#29694 = CARTESIAN_POINT ( 'NONE',  ( 0.6823417656249899377, 1.092708333674752286, 1.181850606188755259 ) ) ;
#29695 = CARTESIAN_POINT ( 'NONE',  ( 6.714126539417144102, -0.8821443205445091973, -1.649434700640100226 ) ) ;
#29696 = CARTESIAN_POINT ( 'NONE',  ( 5.467320813769629417, -1.693630324315539726, -0.3718415804769247268 ) ) ;
#29697 = CARTESIAN_POINT ( 'NONE',  ( 5.899919523139840472, -0.6348737135929006792, -1.620717943835482844 ) ) ;
#29698 = CARTESIAN_POINT ( 'NONE',  ( 3.193229341380324549, 1.808410471145019960, 1.408695239656273301 ) ) ;
#29699 = CARTESIAN_POINT ( 'NONE',  ( -1.364683531250010295, 5.801041667008088432, -0.7879004041258300672 ) ) ;
#29700 = CARTESIAN_POINT ( 'NONE',  ( 0.9371597039556851527, 0.7481776565299683712, -1.682445429299509909 ) ) ;
#29701 = MECHANICAL_DESIGN_GEOMETRIC_PRESENTATION_REPRESENTATION (  '', ( #123175 ), #133479 ) ;
#29702 = CARTESIAN_POINT ( 'NONE',  ( 6.773376349083131132, -7.246166700180801001, 6.661184041420955992 ) ) ;
#29703 = CARTESIAN_POINT ( 'NONE',  ( -11.30167226555126980, 6.973387911292391550, 4.148494114740727490 ) ) ;
#29704 = CARTESIAN_POINT ( 'NONE',  ( 1.553431815599433108, 0.5335803070953272220, -1.745854899344486233 ) ) ;
#29705 = CARTESIAN_POINT ( 'NONE',  ( 2.795546247670523954, 1.458556481301529706, -1.392545902517070111 ) ) ;
#29706 = CARTESIAN_POINT ( 'NONE',  ( 0.8498829323080080433, 2.188760582993890313, -0.1110106097068005726 ) ) ;
#29707 = CARTESIAN_POINT ( 'NONE',  ( 8.541839355669758049, 15.38782976336730357, -7.875440542426230373 ) ) ;
#29708 = CARTESIAN_POINT ( 'NONE',  ( 4.840906100885360885, 0.3572417793257404717, 2.075268335340733739 ) ) ;
#29709 = CARTESIAN_POINT ( 'NONE',  ( -6.714312387265696458, 8.856450423275211037, 1.599625672291283607 ) ) ;
#29710 = CARTESIAN_POINT ( 'NONE',  ( 7.538246871973172780, 13.99683876731212884, 10.19897525888958789 ) ) ;
#29711 = CARTESIAN_POINT ( 'NONE',  ( 1.926316106172959230, 1.062450747350886848, 1.776810178100460824 ) ) ;
#29712 = CARTESIAN_POINT ( 'NONE',  ( 5.355634372598031767, 6.206993841907870291, -1.199719254218445830 ) ) ;
#29713 = CARTESIAN_POINT ( 'NONE',  ( -1.752700365193352367E-14, -0.3906249996585918205, -1.570758158831796258 ) ) ;
#29714 = CARTESIAN_POINT ( 'NONE',  ( 4.266349992362879817, 2.119992548681798095, -0.05317809935000831351 ) ) ;
#29715 = CARTESIAN_POINT ( 'NONE',  ( 6.604126001430527637, -1.825160783932573860, 0.05055279568313279792 ) ) ;
#29716 = ORIENTED_EDGE ( 'NONE', *, *, #87363, .F. ) ;
#29717 = CARTESIAN_POINT ( 'NONE',  ( -6.140917232347002042, 6.129101290685087911, -0.7998128361456362523 ) ) ;
#29718 = CARTESIAN_POINT ( 'NONE',  ( -11.35610322553117513, 11.11421628929174865, -3.553412924323506861 ) ) ;
#29719 = CARTESIAN_POINT ( 'NONE',  ( 5.031484404002867450, 8.884165881396448583, 0.7216878364870317197 ) ) ;
#29720 = CARTESIAN_POINT ( 'NONE',  ( 3.475000000000000533, -3.252083332377416092, -2.006292185433951047 ) ) ;
#29721 = CARTESIAN_POINT ( 'NONE',  ( -4.055860508782465068, 7.883587693554856557, 1.040834085586084257E-14 ) ) ;
#29722 = CARTESIAN_POINT ( 'NONE',  ( -0.2102771530458277249, -0.008943344768331040057, -2.203482896658352175 ) ) ;
#29723 = CARTESIAN_POINT ( 'NONE',  ( 1.114449138222296742, -0.9466070430152218051, -1.881282081674582995 ) ) ;
#29724 = CARTESIAN_POINT ( 'NONE',  ( -3.806807270387036368, 7.663301925418665839, 0.000000000000000000 ) ) ;
#29725 = CARTESIAN_POINT ( 'NONE',  ( 8.890396042259068210, 11.39521468743417998, -1.599625672291257406 ) ) ;
#29726 = CARTESIAN_POINT ( 'NONE',  ( 4.645250437676715194, 1.663689067502411412, -0.8338919413633429922 ) ) ;
#29727 = CARTESIAN_POINT ( 'NONE',  ( 7.404724451357931336, 11.79059562655963056, 0.7998128361456462443 ) ) ;
#29728 = CARTESIAN_POINT ( 'NONE',  ( -0.5723387408578866076, 4.245249788590611750, 0.3125093782470893533 ) ) ;
#29729 = CARTESIAN_POINT ( 'NONE',  ( -4.930325137224961907, 5.781076077297750970, -1.199719254218453823 ) ) ;
#29730 = CARTESIAN_POINT ( 'NONE',  ( -9.815740026613960723, 11.51441345488021106, -1.082531754730539753 ) ) ;
#29732 = CARTESIAN_POINT ( 'NONE',  ( 2.752341281506097470, -1.956419249932477955, -0.1471676765215298721 ) ) ;
#29731 = CARTESIAN_POINT ( 'NONE',  ( -5.669280788808708671, 9.765911353585494226, 0.7998128361456481317 ) ) ;
#29733 = CARTESIAN_POINT ( 'NONE',  ( 1.411231610350563992, 1.906656261001705488, 1.018656936289302539 ) ) ;
#29735 = CARTESIAN_POINT ( 'NONE',  ( -6.131331467106510225, 6.000095466447766590, 0.1540833971661673130 ) ) ;
#29734 = CARTESIAN_POINT ( 'NONE',  ( -6.445975688654487001, 6.485002823043819475, -0.7998128361456362523 ) ) ;
#29736 = CARTESIAN_POINT ( 'NONE',  ( -1.364683531250012516, 0.7802083336747528408, 0.7879004041258379498 ) ) ;
#29737 = CARTESIAN_POINT ( 'NONE',  ( 2.424751807388926039, 0.7370815838836901612, 1.569499502796549262 ) ) ;
#29738 = CARTESIAN_POINT ( 'NONE',  ( 2.765247366594007605, 0.9310170973755277357, 1.470147560556547273 ) ) ;
#29739 = CARTESIAN_POINT ( 'NONE',  ( 6.480434237652121787, 9.543961796360731498, 1.082531754730558626 ) ) ;
#29740 = CARTESIAN_POINT ( 'NONE',  ( -10.57232898948313604, 5.599354254162436817, 4.968808419985093039 ) ) ;
#29741 = CARTESIAN_POINT ( 'NONE',  ( 2.003267984693514858, 1.711604303819891593, 1.147383568780909302 ) ) ;
#29742 = EDGE_CURVE ( 'NONE', #108528, #45585, #32097, .T. ) ;
#29743 = CARTESIAN_POINT ( 'NONE',  ( 1.546249734355091388, 1.863884247081739609, -0.7690006294575402190 ) ) ;
#29744 = CARTESIAN_POINT ( 'NONE',  ( 6.825078400183551608, 4.689370880799383912, 2.706890346843467299 ) ) ;
#29745 = CARTESIAN_POINT ( 'NONE',  ( -5.309953438407606363, 6.223975762010839574, 1.199719254218452935 ) ) ;
#29746 = CARTESIAN_POINT ( 'NONE',  ( 1.059376886711576260, 0.3867523390363221125, -1.932997803022660666 ) ) ;
#29748 = CARTESIAN_POINT ( 'NONE',  ( -5.966997003790228682, 8.054858819212300958, -1.443375672974066548 ) ) ;
#29747 = CARTESIAN_POINT ( 'NONE',  ( 5.818603510220927255, -0.6945032022064903110, -1.782003016414166474 ) ) ;
#29749 = CARTESIAN_POINT ( 'NONE',  ( -5.926322542504860458, 9.928143709648733051, -0.7216878364870338292 ) ) ;
#29750 = CARTESIAN_POINT ( 'NONE',  ( 5.501576472095266901, 9.640532660744973725, -0.7998128361456481317 ) ) ;
#29751 = CARTESIAN_POINT ( 'NONE',  ( -7.795011973214244883, 8.058878488363559356, 0.7998128361456341429 ) ) ;
#29752 = CARTESIAN_POINT ( 'NONE',  ( 0.8385427299653764877, 1.201306043029852777, -1.623412603403198373 ) ) ;
#29753 = CARTESIAN_POINT ( 'NONE',  ( 0.4999999999999761302, 3.999999999999948042, -0.5000000000000299760 ) ) ;
#29754 = CARTESIAN_POINT ( 'NONE',  ( 4.454349891636342207, 2.307156057683857675, -0.05211387993751984832 ) ) ;
#29755 = CARTESIAN_POINT ( 'NONE',  ( 5.635196431686764207, -0.04651148872366302894, -1.961470878453225763 ) ) ;
#29756 = CARTESIAN_POINT ( 'NONE',  ( 2.026150138982992566, 1.004015975608811173, 1.685199498757394831 ) ) ;
#29757 = CARTESIAN_POINT ( 'NONE',  ( 10.07100917685271035, 10.64393221595000938, 0.7998128361456462443 ) ) ;
#29758 = CARTESIAN_POINT ( 'NONE',  ( -9.494457024078482021, 15.33445319465660717, 7.338830937051257663 ) ) ;
#29759 = ORIENTED_EDGE ( 'NONE', *, *, #51124, .T. ) ;
#29760 = CARTESIAN_POINT ( 'NONE',  ( 1.464221803445309167, -1.127774752583620366, 1.791820951956924812 ) ) ;
#29762 = CARTESIAN_POINT ( 'NONE',  ( -7.426115451983156923, 9.686887332112256388, -1.599625672291263179 ) ) ;
#29761 = CARTESIAN_POINT ( 'NONE',  ( -3.086452525405351643, 6.752611712948207057, 0.7998128361456341429 ) ) ;
#29763 = CARTESIAN_POINT ( 'NONE',  ( 0.6910384644343778859, -0.6650364481293036256, 1.717017257891314097 ) ) ;
#29764 = EDGE_LOOP ( 'NONE', ( #129103, #156266, #53842, #117131 ) ) ;
#29765 = CARTESIAN_POINT ( 'NONE',  ( 4.539989016966003099, 1.413352768409949389, 1.648148102320112329 ) ) ;
#29766 = CARTESIAN_POINT ( 'NONE',  ( 11.99956024306423785, 7.587643445255384478, 0.4561022673488305812 ) ) ;
#29767 = CARTESIAN_POINT ( 'NONE',  ( 3.041385797112206912, 0.05609166564453024750, 2.120036961950934273 ) ) ;
#29768 = CARTESIAN_POINT ( 'NONE',  ( 1.499999999999989120, 4.577083334016148974, -0.8660254037844323793 ) ) ;
#29769 = CARTESIAN_POINT ( 'NONE',  ( 9.426996880203592610, 9.892584536526015881, -0.7998128361456281477 ) ) ;
#29770 = SURFACE_STYLE_FILL_AREA ( #15617 ) ;
#29771 = VERTEX_POINT ( 'NONE', #79937 ) ;
#29772 = CARTESIAN_POINT ( 'NONE',  ( 3.479809507395460244, 1.304684485917747994, 1.595210877418812956 ) ) ;
#29774 = CARTESIAN_POINT ( 'NONE',  ( 0.09881949811249221560, -0.4921898920670075839, 1.774194203830472993 ) ) ;
#29773 = CARTESIAN_POINT ( 'NONE',  ( -7.557780564614042795, 10.90482886110335414, -1.199719254218446718 ) ) ;
#29775 = CARTESIAN_POINT ( 'NONE',  ( -1.364683531249997417, 3.259375000341423245, 1.214306433183764966E-14 ) ) ;
#29776 = CARTESIAN_POINT ( 'NONE',  ( -0.02224634325196857970, 4.078913133451218087, -2.843768138527980049 ) ) ;
#29777 = CARTESIAN_POINT ( 'NONE',  ( 1.367525579689990778, 4.283758018875697182, 0.2571629661623252572 ) ) ;
#29778 = CARTESIAN_POINT ( 'NONE',  ( -4.650083499362883011, 6.448183387388563226, 1.443375672974064550 ) ) ;
#29779 = CARTESIAN_POINT ( 'NONE',  ( 2.214515517796631805, -1.065126590517451843, -1.995962479041712534 ) ) ;
#29780 = CARTESIAN_POINT ( 'NONE',  ( -9.056483424248693126, 10.62861408545402675, 1.082531754730558626 ) ) ;
#29781 = CARTESIAN_POINT ( 'NONE',  ( 1.933590839544163664, -1.756428034162808904, 0.4429697619106263695 ) ) ;
#29782 = EDGE_CURVE ( 'NONE', #127758, #53890, #101193, .T. ) ;
#29783 = CARTESIAN_POINT ( 'NONE',  ( 2.219824929201766217, 0.8990433841352833966, -1.691613514901336490 ) ) ;
#29784 = CARTESIAN_POINT ( 'NONE',  ( 2.611853368047814872, 0.5545374748289233491, -1.994631108499920646 ) ) ;
#29785 = CARTESIAN_POINT ( 'NONE',  ( 1.364683531249988535, 2.926041667008082658, 0.7879004041258500513 ) ) ;
#29786 = CARTESIAN_POINT ( 'NONE',  ( 1.867985033921132798, 1.011920226373051346, 1.691812110196472041 ) ) ;
#29787 = CARTESIAN_POINT ( 'NONE',  ( 0.4285742275551830960, 1.842496385298073580, 0.5622912056609475906 ) ) ;
#29788 = CARTESIAN_POINT ( 'NONE',  ( 3.362029495745801899, 0.8400119854848131506, 1.671504782411597612 ) ) ;
#29790 = CARTESIAN_POINT ( 'NONE',  ( 4.985841187518467166, 7.931359929992748192, -1.059499378661461710 ) ) ;
#29789 = CARTESIAN_POINT ( 'NONE',  ( 1.682680061667326088, -1.231660274741898320, 1.951365989292063174 ) ) ;
#29791 = CARTESIAN_POINT ( 'NONE',  ( 2.576407586095734725, 1.218277932339612901, -1.406949740073556887 ) ) ;
#29792 = CARTESIAN_POINT ( 'NONE',  ( -1.364683531250012516, 2.530208333674753174, 0.7879004041258379498 ) ) ;
#29793 = AXIS2_PLACEMENT_3D ( 'NONE', #7118, #122051, #139297 ) ;
#29794 = CARTESIAN_POINT ( 'NONE',  ( 5.846154128119951388, -0.9308047640707247661, 1.840808156992862932 ) ) ;
#29795 = CARTESIAN_POINT ( 'NONE',  ( -5.870844209917351009, 6.808071985447069707, -1.199719254218446718 ) ) ;
#29796 = CARTESIAN_POINT ( 'NONE',  ( 7.100719765255169236, 9.307259030929609267, -1.599625672291262513 ) ) ;
#29797 = CARTESIAN_POINT ( 'NONE',  ( -1.355678468426067429, 3.935142031700837428, 0.6419787906858558379 ) ) ;
#29798 = CARTESIAN_POINT ( 'NONE',  ( 6.739294440770141392, -1.883009798889522024, 0.9431707147840006078 ) ) ;
#29799 = CARTESIAN_POINT ( 'NONE',  ( 1.364683531249990311, 3.196875000341416140, 1.214306433183764966E-14 ) ) ;
#29800 = CARTESIAN_POINT ( 'NONE',  ( 6.468072252983536607, 1.105043713804385153, 1.857642994352682653 ) ) ;
#29801 = CARTESIAN_POINT ( 'NONE',  ( 0.08815677907929740653, 1.166467155405017442, 1.648690671293622012 ) ) ;
#29802 = CARTESIAN_POINT ( 'NONE',  ( 0.6823417656249864960, -0.8239583329919114574, -1.181850606188749264 ) ) ;
#29803 = CARTESIAN_POINT ( 'NONE',  ( -4.419594888374909658, 8.100018436505289188, 0.7216878364870458196 ) ) ;
#29804 = EDGE_CURVE ( 'NONE', #140464, #188755, #170307, .T. ) ;
#29807 = CARTESIAN_POINT ( 'NONE',  ( 4.473827502829567315, 7.202920605734387749, -1.082531754730548412 ) ) ;
#29806 = CARTESIAN_POINT ( 'NONE',  ( -1.642778471875000035, -0.1677083328553742592, -2.845375778867859751 ) ) ;
#29805 = CARTESIAN_POINT ( 'NONE',  ( 4.877901405866606588, 8.912911750144889567, 0.7998128361456341429 ) ) ;
#29808 =( BOUNDED_SURFACE ( )  B_SPLINE_SURFACE ( 1, 2, ( 
 ( #42898, #175026, #29834, #13562, #45028, #92714, #10355, #111141, #210694, #9301, #75374, #177142, #142540, #94843, #160894, #62323, #163035, #14616, #146803, #179286, #30911, #195527, #80713, #47166, #212820, #113280, #129545, #96985, #186124, #22550, #138472, #73445, #156860, #8446, #137405, #40979, #172034, #107090, #106012, #173112, #140633, #104910, #202358, #87578, #203424, #169879, #24693, #121228, #54008, #21469, #6297, #139549, #55079, #170951, #168818, #90796, #120147, #7368, #20422, #187198, #74533, #119069, #153649, #155784, #206646, #38826, #88656, #23627, #154716, #205576, #86504, #185050, #71293, #36675, #72372, #152569, #4156, #37758, #102763, #89735, #70227, #204494, #136338, #57213, #122305, #103831, #5218, #56144, #188263, #39903, #123373, #189340, #147156, #79996, #195891, #212111, #211047, #96280, #97342, #182827, #146100, #116825, #114703, #47529, #196947, #181747, #83186, #66913, #162330, #180698, #113642, #148217, #149269, #13915, #64810, #165516, #63748, #129907, #82124, #46450, #214219, #30190, #112571, #65848, #98390, #178582, #179647, #17108, #133054, #32322, #31267, #163399, #14973, #115757, #848, #194814, #164454, #99459, #199055, #81070, #130957, #16041, #131997, #50701, #213181, #48587, #128832, #198006, #49633, #95212, #33378, #161261, #12848, #78922, #145045, #62673, #203325, #72263, #138371, #52832, #170853, #87480, #22443, #21372, #88554, #56044, #20321, #117903, #2991, #118969, #85335, #154615, #36574, #183896, #151417, #136235, #54977, #184947, #86407, #84267, #6194, #35508, #137309, #150352, #102660, #204389, #34442, #69058, #71192, #122200, #168718, #152474, #153546, #4054, #121130, #1923, #100516, #201193, #166591, #70124, #67981, #134124, #101585, #18180, #5115, #200133, #202258, #51786, #187093, #37655, #167653, #19254, #135178, #53909, #120044, #38727, #186018, #103732, #169783, #104808, #7262, #209733, #126456, #61377, #157824, #125386, #43017, #141602, #40878, #205476, #57108, #23522, #156759, #9420, #155680, #106983, #192420, #76546, #188162, #207609, #89628 ),
 ( #173008, #110193, #44074, #24589, #91768, #59228, #142657, #11546, #77616, #206543, #176203, #26730, #27804, #175144, #93902, #39795, #174086, #123277, #8346, #58173, #90696, #159941, #190291, #189239, #74431, #75491, #208667, #124331, #25659, #73339, #143739, #140531, #60298, #139441, #41948, #105902, #171926, #108061, #10472, #191352, #109131, #92832, #158876, #97097, #15793, #28876, #127534, #79745, #165259, #31022, #94961, #12604, #128597, #584, #180454, #161009, #63507, #45147, #98159, #130712, #16852, #194563, #177262, #82935, #46208, #114454, #145862, #111259, #78676, #193506, #144803, #149008, #65596, #210809, #163149, #64569, #196703, #80825, #112324, #62434, #178339, #29948, #96033, #14733, #162084, #99210, #13674, #212933, #211868, #32071, #181502, #129661, #146915, #197750, #195645, #47281, #164206, #113393, #81878, #179402, #48343, #147963, #213976, #131745, #49389, #115507, #33130, #152212, #67716, #17913, #200923, #87205, #137035, #166323, #86141, #120855, #69856, #203061, #18988, #199874, #50447, #37384, #154345, #116565, #83998, #118701, #51517, #167397, #183634, #182559, #133867, #68796, #66650, #117642, #88280, #3782, #85070, #168454, #153269, #54705, #132796, #102387, #35241, #186829, #198799, #4844, #38459, #101316, #104536, #134916, #52571, #184687, #151155, #70924, #22165, #20052, #36308, #135965, #201982, #170582, #1660, #150088, #119771, #53638, #185751, #34182, #2724, #100255, #103459, #169521, #21101, #96580, #139170, #10218, #108864, #5923, #25401, #121926, #206282, #155408, #107799, #91502, #56842, #30496, #138106, #8080, #173824, #171650, #79232, #204117, #62975, #125132, #9156, #187894, #74168, #157563, #156491, #124070, #23248, #75232, #145349, #141342, #73070, #190035, #123015, #41688, #207356, #211350, #140261, #58977, #39522, #92579, #71995, #106714, #90422, #195120, #40609, #57906, #55769, #174890, #191090, #42759, #105622, #24316, #26469, #129144, #158621, #46758, #188967, #112869, #178884, #89360, #6991, #205201, #172740, #133345, #72, #213466, #50997, #65090, #97636 ) ),
 .UNSPECIFIED., .F., .F., .T. ) 
 B_SPLINE_SURFACE_WITH_KNOTS ( ( 2, 2 ),
 ( 3, 2, 2, 2, 2, 2, 2, 2, 2, 2, 2, 2, 2, 2, 2, 2, 2, 2, 2, 2, 2, 2, 2, 2, 2, 2, 2, 2, 2, 2, 2, 2, 2, 2, 2, 2, 2, 2, 2, 2, 2, 2, 2, 2, 2, 2, 2, 2, 2, 2, 2, 2, 2, 2, 2, 2, 2, 2, 2, 2, 2, 2, 2, 2, 2, 2, 2, 2, 2, 2, 2, 2, 2, 2, 2, 2, 2, 2, 2, 2, 2, 2, 2, 2, 2, 2, 2, 2, 2, 2, 2, 2, 2, 2, 2, 2, 2, 2, 2, 2, 2, 2, 2, 2, 2, 2, 2, 2, 2, 2, 2, 2, 2, 2, 2, 2, 2, 2, 2, 2, 3 ),
 ( 0.000000000000000000, 1.000000000000000000 ),
 ( 0.000000000000000000, 0.008333333333333333218, 0.01666666666666666644, 0.02500000000000000139, 0.03333333333333333287, 0.04166666666666666435, 0.05000000000000000278, 0.05833333333333333426, 0.06666666666666666574, 0.07499999999999999722, 0.08333333333333332871, 0.09166666666666666019, 0.1000000000000000056, 0.1083333333333333370, 0.1166666666666666685, 0.1250000000000000000, 0.1333333333333333315, 0.1416666666666666630, 0.1499999999999999944, 0.1583333333333333259, 0.1666666666666666574, 0.1749999999999999889, 0.1833333333333333204, 0.1916666666666666796, 0.2000000000000000111, 0.2083333333333333426, 0.2166666666666666741, 0.2250000000000000056, 0.2333333333333333370, 0.2416666666666666685, 0.2500000000000000000, 0.2583333333333333592, 0.2666666666666666630, 0.2750000000000000222, 0.2833333333333333259, 0.2916666666666666852, 0.2999999999999999889, 0.3083333333333333481, 0.3166666666666666519, 0.3250000000000000111, 0.3333333333333333148, 0.3416666666666666741, 0.3499999999999999778, 0.3583333333333333370, 0.3666666666666666408, 0.3750000000000000000, 0.3833333333333333592, 0.3916666666666666630, 0.4000000000000000222, 0.4083333333333333259, 0.4166666666666666852, 0.4249999999999999889, 0.4333333333333333481, 0.4416666666666666519, 0.4500000000000000111, 0.4583333333333333148, 0.4666666666666666741, 0.4749999999999999778, 0.4833333333333333370, 0.4916666666666666408, 0.5000000000000000000, 0.5083333333333333037, 0.5166666666666667185, 0.5250000000000000222, 0.5333333333333333259, 0.5416666666666666297, 0.5500000000000000444, 0.5583333333333333481, 0.5666666666666666519, 0.5749999999999999556, 0.5833333333333333703, 0.5916666666666666741, 0.5999999999999999778, 0.6083333333333332815, 0.6166666666666666963, 0.6250000000000000000, 0.6333333333333333037, 0.6416666666666667185, 0.6500000000000000222, 0.6583333333333333259, 0.6666666666666666297, 0.6750000000000000444, 0.6833333333333333481, 0.6916666666666666519, 0.6999999999999999556, 0.7083333333333333703, 0.7166666666666666741, 0.7249999999999999778, 0.7333333333333332815, 0.7416666666666666963, 0.7500000000000000000, 0.7583333333333333037, 0.7666666666666667185, 0.7750000000000000222, 0.7833333333333333259, 0.7916666666666666297, 0.8000000000000000444, 0.8083333333333333481, 0.8166666666666666519, 0.8249999999999999556, 0.8333333333333333703, 0.8416666666666666741, 0.8499999999999999778, 0.8583333333333332815, 0.8666666666666666963, 0.8750000000000000000, 0.8833333333333333037, 0.8916666666666667185, 0.9000000000000000222, 0.9083333333333333259, 0.9166666666666666297, 0.9250000000000000444, 0.9333333333333333481, 0.9416666666666666519, 0.9499999999999999556, 0.9583333333333333703, 0.9666666666666666741, 0.9749999999999999778, 0.9833333333333332815, 0.9916666666666666963, 1.000000000000000000 ),
 .UNSPECIFIED. ) 
 GEOMETRIC_REPRESENTATION_ITEM ( )  RATIONAL_B_SPLINE_SURFACE ( (
 ( 1.000000000000000000, 0.8660254037844387076, 1.000000000000000000, 0.8660254037844387076, 1.000000000000000000, 0.8660254037844387076, 1.000000000000000000, 0.8660254037844387076, 1.000000000000000000, 0.8660254037844387076, 1.000000000000000000, 0.8660254037844387076, 1.000000000000000000, 0.8660254037844387076, 1.000000000000000000, 0.8660254037844387076, 1.000000000000000000, 0.8660254037844387076, 1.000000000000000000, 0.8660254037844387076, 1.000000000000000000, 0.8660254037844387076, 1.000000000000000000, 0.8660254037844387076, 1.000000000000000000, 0.8660254037844387076, 1.000000000000000000, 0.8660254037844387076, 1.000000000000000000, 0.8660254037844387076, 1.000000000000000000, 0.8660254037844387076, 1.000000000000000000, 0.8660254037844387076, 1.000000000000000000, 0.8660254037844387076, 1.000000000000000000, 0.8660254037844387076, 1.000000000000000000, 0.8660254037844387076, 1.000000000000000000, 0.8660254037844387076, 1.000000000000000000, 0.8660254037844387076, 1.000000000000000000, 0.8660254037844387076, 1.000000000000000000, 0.8660254037844387076, 1.000000000000000000, 0.8660254037844387076, 1.000000000000000000, 0.8660254037844387076, 1.000000000000000000, 0.8660254037844387076, 1.000000000000000000, 0.8660254037844387076, 1.000000000000000000, 0.8660254037844387076, 1.000000000000000000, 0.8660254037844387076, 1.000000000000000000, 0.8660254037844387076, 1.000000000000000000, 0.8660254037844387076, 1.000000000000000000, 0.8660254037844387076, 1.000000000000000000, 0.8660254037844387076, 1.000000000000000000, 0.8660254037844387076, 1.000000000000000000, 0.8660254037844387076, 1.000000000000000000, 0.8660254037844387076, 1.000000000000000000, 0.8660254037844387076, 1.000000000000000000, 0.8660254037844387076, 1.000000000000000000, 0.8660254037844387076, 1.000000000000000000, 0.8660254037844387076, 1.000000000000000000, 0.8660254037844387076, 1.000000000000000000, 0.8660254037844387076, 1.000000000000000000, 0.8660254037844387076, 1.000000000000000000, 0.8660254037844387076, 1.000000000000000000, 0.8660254037844387076, 1.000000000000000000, 0.8660254037844387076, 1.000000000000000000, 0.8660254037844387076, 1.000000000000000000, 0.8660254037844387076, 1.000000000000000000, 0.8660254037844387076, 1.000000000000000000, 0.8660254037844387076, 1.000000000000000000, 0.8660254037844387076, 1.000000000000000000, 0.8660254037844387076, 1.000000000000000000, 0.8660254037844387076, 1.000000000000000000, 0.8660254037844387076, 1.000000000000000000, 0.8660254037844387076, 1.000000000000000000, 0.8660254037844387076, 1.000000000000000000, 0.8660254037844387076, 1.000000000000000000, 0.8660254037844387076, 1.000000000000000000, 0.8660254037844387076, 1.000000000000000000, 0.8660254037844387076, 1.000000000000000000, 0.8660254037844387076, 1.000000000000000000, 0.8660254037844387076, 1.000000000000000000, 0.8660254037844387076, 1.000000000000000000, 0.8660254037844387076, 1.000000000000000000, 0.8660254037844387076, 1.000000000000000000, 0.8660254037844387076, 1.000000000000000000, 0.8660254037844387076, 1.000000000000000000, 0.8660254037844387076, 1.000000000000000000, 0.8660254037844387076, 1.000000000000000000, 0.8660254037844387076, 1.000000000000000000, 0.8660254037844387076, 1.000000000000000000, 0.8660254037844387076, 1.000000000000000000, 0.8660254037844387076, 1.000000000000000000, 0.8660254037844387076, 1.000000000000000000, 0.8660254037844387076, 1.000000000000000000, 0.8660254037844387076, 1.000000000000000000, 0.8660254037844387076, 1.000000000000000000, 0.8660254037844387076, 1.000000000000000000, 0.8660254037844387076, 1.000000000000000000, 0.8660254037844387076, 1.000000000000000000, 0.8660254037844387076, 1.000000000000000000, 0.8660254037844387076, 1.000000000000000000, 0.8660254037844387076, 1.000000000000000000, 0.8660254037844387076, 1.000000000000000000, 0.8660254037844387076, 1.000000000000000000, 0.8660254037844387076, 1.000000000000000000, 0.8660254037844387076, 1.000000000000000000, 0.8660254037844387076, 1.000000000000000000, 0.8660254037844387076, 1.000000000000000000, 0.8660254037844387076, 1.000000000000000000, 0.8660254037844387076, 1.000000000000000000, 0.8660254037844387076, 1.000000000000000000, 0.8660254037844387076, 1.000000000000000000, 0.8660254037844387076, 1.000000000000000000, 0.8660254037844387076, 1.000000000000000000, 0.8660254037844387076, 1.000000000000000000, 0.8660254037844387076, 1.000000000000000000, 0.8660254037844387076, 1.000000000000000000, 0.8660254037844387076, 1.000000000000000000, 0.8660254037844387076, 1.000000000000000000, 0.8660254037844387076, 1.000000000000000000, 0.8660254037844387076, 1.000000000000000000, 0.8660254037844387076, 1.000000000000000000, 0.8660254037844387076, 1.000000000000000000, 0.8660254037844387076, 1.000000000000000000, 0.8660254037844387076, 1.000000000000000000, 0.8660254037844387076, 1.000000000000000000, 0.8660254037844387076, 1.000000000000000000, 0.8660254037844387076, 1.000000000000000000, 0.8660254037844387076, 1.000000000000000000, 0.8660254037844387076, 1.000000000000000000, 0.8660254037844387076, 1.000000000000000000, 0.8660254037844387076, 1.000000000000000000, 0.8660254037844387076, 1.000000000000000000, 0.8660254037844387076, 1.000000000000000000, 0.8660254037844387076, 1.000000000000000000, 0.8660254037844387076, 1.000000000000000000, 0.8660254037844387076, 1.000000000000000000, 0.8660254037844387076, 1.000000000000000000),
 ( 1.000000000000000000, 0.8660254037844387076, 1.000000000000000000, 0.8660254037844387076, 1.000000000000000000, 0.8660254037844387076, 1.000000000000000000, 0.8660254037844387076, 1.000000000000000000, 0.8660254037844387076, 1.000000000000000000, 0.8660254037844387076, 1.000000000000000000, 0.8660254037844387076, 1.000000000000000000, 0.8660254037844387076, 1.000000000000000000, 0.8660254037844387076, 1.000000000000000000, 0.8660254037844387076, 1.000000000000000000, 0.8660254037844387076, 1.000000000000000000, 0.8660254037844387076, 1.000000000000000000, 0.8660254037844387076, 1.000000000000000000, 0.8660254037844387076, 1.000000000000000000, 0.8660254037844387076, 1.000000000000000000, 0.8660254037844387076, 1.000000000000000000, 0.8660254037844387076, 1.000000000000000000, 0.8660254037844387076, 1.000000000000000000, 0.8660254037844387076, 1.000000000000000000, 0.8660254037844387076, 1.000000000000000000, 0.8660254037844387076, 1.000000000000000000, 0.8660254037844387076, 1.000000000000000000, 0.8660254037844387076, 1.000000000000000000, 0.8660254037844387076, 1.000000000000000000, 0.8660254037844387076, 1.000000000000000000, 0.8660254037844387076, 1.000000000000000000, 0.8660254037844387076, 1.000000000000000000, 0.8660254037844387076, 1.000000000000000000, 0.8660254037844387076, 1.000000000000000000, 0.8660254037844387076, 1.000000000000000000, 0.8660254037844387076, 1.000000000000000000, 0.8660254037844387076, 1.000000000000000000, 0.8660254037844387076, 1.000000000000000000, 0.8660254037844387076, 1.000000000000000000, 0.8660254037844387076, 1.000000000000000000, 0.8660254037844387076, 1.000000000000000000, 0.8660254037844387076, 1.000000000000000000, 0.8660254037844387076, 1.000000000000000000, 0.8660254037844387076, 1.000000000000000000, 0.8660254037844387076, 1.000000000000000000, 0.8660254037844387076, 1.000000000000000000, 0.8660254037844387076, 1.000000000000000000, 0.8660254037844387076, 1.000000000000000000, 0.8660254037844387076, 1.000000000000000000, 0.8660254037844387076, 1.000000000000000000, 0.8660254037844387076, 1.000000000000000000, 0.8660254037844387076, 1.000000000000000000, 0.8660254037844387076, 1.000000000000000000, 0.8660254037844387076, 1.000000000000000000, 0.8660254037844387076, 1.000000000000000000, 0.8660254037844387076, 1.000000000000000000, 0.8660254037844387076, 1.000000000000000000, 0.8660254037844387076, 1.000000000000000000, 0.8660254037844387076, 1.000000000000000000, 0.8660254037844387076, 1.000000000000000000, 0.8660254037844387076, 1.000000000000000000, 0.8660254037844387076, 1.000000000000000000, 0.8660254037844387076, 1.000000000000000000, 0.8660254037844387076, 1.000000000000000000, 0.8660254037844387076, 1.000000000000000000, 0.8660254037844387076, 1.000000000000000000, 0.8660254037844387076, 1.000000000000000000, 0.8660254037844387076, 1.000000000000000000, 0.8660254037844387076, 1.000000000000000000, 0.8660254037844387076, 1.000000000000000000, 0.8660254037844387076, 1.000000000000000000, 0.8660254037844387076, 1.000000000000000000, 0.8660254037844387076, 1.000000000000000000, 0.8660254037844387076, 1.000000000000000000, 0.8660254037844387076, 1.000000000000000000, 0.8660254037844387076, 1.000000000000000000, 0.8660254037844387076, 1.000000000000000000, 0.8660254037844387076, 1.000000000000000000, 0.8660254037844387076, 1.000000000000000000, 0.8660254037844387076, 1.000000000000000000, 0.8660254037844387076, 1.000000000000000000, 0.8660254037844387076, 1.000000000000000000, 0.8660254037844387076, 1.000000000000000000, 0.8660254037844387076, 1.000000000000000000, 0.8660254037844387076, 1.000000000000000000, 0.8660254037844387076, 1.000000000000000000, 0.8660254037844387076, 1.000000000000000000, 0.8660254037844387076, 1.000000000000000000, 0.8660254037844387076, 1.000000000000000000, 0.8660254037844387076, 1.000000000000000000, 0.8660254037844387076, 1.000000000000000000, 0.8660254037844387076, 1.000000000000000000, 0.8660254037844387076, 1.000000000000000000, 0.8660254037844387076, 1.000000000000000000, 0.8660254037844387076, 1.000000000000000000, 0.8660254037844387076, 1.000000000000000000, 0.8660254037844387076, 1.000000000000000000, 0.8660254037844387076, 1.000000000000000000, 0.8660254037844387076, 1.000000000000000000, 0.8660254037844387076, 1.000000000000000000, 0.8660254037844387076, 1.000000000000000000, 0.8660254037844387076, 1.000000000000000000, 0.8660254037844387076, 1.000000000000000000, 0.8660254037844387076, 1.000000000000000000, 0.8660254037844387076, 1.000000000000000000, 0.8660254037844387076, 1.000000000000000000, 0.8660254037844387076, 1.000000000000000000, 0.8660254037844387076, 1.000000000000000000, 0.8660254037844387076, 1.000000000000000000, 0.8660254037844387076, 1.000000000000000000, 0.8660254037844387076, 1.000000000000000000, 0.8660254037844387076, 1.000000000000000000, 0.8660254037844387076, 1.000000000000000000, 0.8660254037844387076, 1.000000000000000000, 0.8660254037844387076, 1.000000000000000000, 0.8660254037844387076, 1.000000000000000000, 0.8660254037844387076, 1.000000000000000000, 0.8660254037844387076, 1.000000000000000000, 0.8660254037844387076, 1.000000000000000000, 0.8660254037844387076, 1.000000000000000000, 0.8660254037844387076, 1.000000000000000000, 0.8660254037844387076, 1.000000000000000000, 0.8660254037844387076, 1.000000000000000000, 0.8660254037844387076, 1.000000000000000000, 0.8660254037844387076, 1.000000000000000000) ) ) 
 REPRESENTATION_ITEM ( '' )  SURFACE ( )  );
#29809 = CARTESIAN_POINT ( 'NONE',  ( -4.118644803501354978, 8.027112380718707030, 0.7998128361456352531 ) ) ;
#29810 = CARTESIAN_POINT ( 'NONE',  ( 4.592982591267942283, 1.756852934926198317, 0.9896879400849432074 ) ) ;
#29811 = CARTESIAN_POINT ( 'NONE',  ( -7.877450944739929461, 9.149113176073413456, 1.199719254218462483 ) ) ;
#29813 = CARTESIAN_POINT ( 'NONE',  ( -7.282137903871469753, 8.628820655005750240, 1.082531754730549078 ) ) ;
#29812 = CARTESIAN_POINT ( 'NONE',  ( -10.16825202056928390, 10.96530823352674133, 0.7216878364870438212 ) ) ;
#29814 = APPLICATION_CONTEXT ( 'automotive_design' ) ;
#29815 = CARTESIAN_POINT ( 'NONE',  ( -0.6823417656250212460, 5.051041667008086655, 1.181850606188767472 ) ) ;
#29817 = CARTESIAN_POINT ( 'NONE',  ( 1.364683531249997417, 8.734375000341396245, 2.602085213965210642E-15 ) ) ;
#29816 = CARTESIAN_POINT ( 'NONE',  ( 6.403215362905616992, 1.794359850238020693, 1.205212418099836480 ) ) ;
#29818 = DIRECTION ( 'NONE',  ( 0.000000000000000000, 1.000000000000000000, 0.000000000000000000 ) ) ;
#29819 = CARTESIAN_POINT ( 'NONE',  ( -11.99966943091182259, 8.028188729005464097, 0.5386726004062643014 ) ) ;
#29821 = CARTESIAN_POINT ( 'NONE',  ( 6.327749939939702806, 0.7691082200134463642, -1.864175038933603146 ) ) ;
#29820 = CARTESIAN_POINT ( 'NONE',  ( -5.517805330637490790, 9.381263952478319013, 0.7216878364870458196 ) ) ;
#29822 = CARTESIAN_POINT ( 'NONE',  ( -0.6823417656250246877, -0.3864583329919110688, 1.181850606188755259 ) ) ;
#29823 = CARTESIAN_POINT ( 'NONE',  ( 6.639320575229294086, -0.003630812595115453199, 2.203388474976493594 ) ) ;
#29824 = CARTESIAN_POINT ( 'NONE',  ( 1.945521746005531627, 0.6619316864419527713, -1.593019548489343240 ) ) ;
#29825 = CARTESIAN_POINT ( 'NONE',  ( 5.422335090822693715, 5.290755458906732933, 0.000000000000000000 ) ) ;
#29826 = CARTESIAN_POINT ( 'NONE',  ( 5.006703865196457492, 9.063181286029688977, 0.000000000000000000 ) ) ;
#29827 = CARTESIAN_POINT ( 'NONE',  ( -12.00000782161162682, 9.022963770432253838, 0.3066704378487656868 ) ) ;
#29828 = CARTESIAN_POINT ( 'NONE',  ( 6.274654046616443992, -1.776150972019393093, -0.5868208112121618969 ) ) ;
#29829 = CARTESIAN_POINT ( 'NONE',  ( 1.154940503102233729, 0.3948395466160973255, 1.973830874585213113 ) ) ;
#29830 = CARTESIAN_POINT ( 'NONE',  ( 11.89942855770814312, 13.79999999999999893, -0.7000000000000009548 ) ) ;
#29831 = CARTESIAN_POINT ( 'NONE',  ( 3.294164632606086940, -0.8960083017303889230, 2.016869484631748310 ) ) ;
#29832 = CARTESIAN_POINT ( 'NONE',  ( 5.858309005574939832, -2.171239809575730817, -0.007779773244297875576 ) ) ;
#29833 = EDGE_LOOP ( 'NONE', ( #127743, #137722, #96028, #197817 ) ) ;
#29834 = CARTESIAN_POINT ( 'NONE',  ( 4.435452530326143616, 5.203724702582467998, -1.199719254218452047 ) ) ;
#29835 = CARTESIAN_POINT ( 'NONE',  ( 9.883530794237934458, 10.63313346947350269, -0.7216878364870257245 ) ) ;
#29837 = CARTESIAN_POINT ( 'NONE',  ( 2.847279977023515318, 0.2930488483154705670, -1.994874153863256172 ) ) ;
#29836 = CARTESIAN_POINT ( 'NONE',  ( 3.633539341399088407, -0.1543397204060332761, 2.114911865293423787 ) ) ;
#29839 = EDGE_LOOP ( 'NONE', ( #25548, #127192, #133783, #173581 ) ) ;
#29838 = CARTESIAN_POINT ( 'NONE',  ( 1.863241329703895888, -1.456548260382009685, -1.076974786960547048 ) ) ;
#29840 = CARTESIAN_POINT ( 'NONE',  ( 7.062871678076271920, 7.204714810702593120, -0.7998128361456341429 ) ) ;
#29841 = ORIENTED_EDGE ( 'NONE', *, *, #47045, .F. ) ;
#29842 = COLOUR_RGB ( '', 0.08235294, 0.09019608, 0.10196078) ;
#29843 = CARTESIAN_POINT ( 'NONE',  ( 6.796715079152391148, 6.823922435299587974, 0.7998128361456341429 ) ) ;
#29845 = CARTESIAN_POINT ( 'NONE',  ( 0.9892949506953198080, -0.4622125203353181222, 1.859009271263431184 ) ) ;
#29844 = CARTESIAN_POINT ( 'NONE',  ( -5.576481253922474401, 5.400316305864651056, -0.7998128361456221525 ) ) ;
#29846 = CARTESIAN_POINT ( 'NONE',  ( -11.94105721237523099, 10.19999999999999929, 1.187919463087248273 ) ) ;
#29847 = LINE ( 'NONE', #197650, #48712 ) ;
#29848 = EDGE_CURVE ( 'NONE', #93531, #135057, #7798, .T. ) ;
#29849 = CARTESIAN_POINT ( 'NONE',  ( 1.364683531249986537, 0.9260416670080896528, 0.7879004041258500513 ) ) ;
#29850 = CARTESIAN_POINT ( 'NONE',  ( 6.004977026901663351, 6.084690627017792508, 0.6157370554833795362 ) ) ;
#29851 = CARTESIAN_POINT ( 'NONE',  ( -10.08065090696061716, 11.71951313199760136, -1.199719254218441611 ) ) ;
#29852 = VECTOR ( 'NONE', #140530, 1000.000000000000000 ) ;
#29853 = CARTESIAN_POINT ( 'NONE',  ( 4.856408821558930278, 0.8241108818672329139, 1.998647875481096126 ) ) ;
#29854 = EDGE_CURVE ( 'NONE', #78193, #116248, #210753, .T. ) ;
#29855 = CARTESIAN_POINT ( 'NONE',  ( -4.340018570150309785, 7.117086527600392287, -1.082531754730551743 ) ) ;
#29856 = CARTESIAN_POINT ( 'NONE',  ( 4.828112100242277549, 6.726159765073026264, -1.443375672974068769 ) ) ;
#29857 = CARTESIAN_POINT ( 'NONE',  ( 2.566775492539817627, 0.7186216927172992541, 1.995234744298620910 ) ) ;
#29858 = CARTESIAN_POINT ( 'NONE',  ( -11.31901822352654641, 5.215070234333009758, -5.710337001866061968 ) ) ;
#29859 = CARTESIAN_POINT ( 'NONE',  ( 3.286357016390834218, -1.941589536447934972, -0.3404988550089679267 ) ) ;
#29860 = VERTEX_POINT ( 'NONE', #32266 ) ;
#29861 = CARTESIAN_POINT ( 'NONE',  ( -2.033424464989782354, 3.426985321572576737, 11.42673966862524537 ) ) ;
#29862 = CARTESIAN_POINT ( 'NONE',  ( 0.9419464005683108043, 1.389173191389100337, 1.535309223701806447 ) ) ;
#29863 = CARTESIAN_POINT ( 'NONE',  ( 2.941277052067638120, 0.6983745205926906729, -1.812199837690719129 ) ) ;
#29864 = ORIENTED_EDGE ( 'NONE', *, *, #58107, .F. ) ;
#29865 = CARTESIAN_POINT ( 'NONE',  ( -0.08000000000000714873, -9.999999999999994671, 10.91970695577494865 ) ) ;
#29867 = CARTESIAN_POINT ( 'NONE',  ( 1.886825320689258012, 2.480000000000016858, -2.459652456995881753 ) ) ;
#29866 = CARTESIAN_POINT ( 'NONE',  ( -5.316205630334251531, 9.216340645449683677, -0.7216878364870338292 ) ) ;
#29869 = CARTESIAN_POINT ( 'NONE',  ( 5.469824908109481854, 8.468880595181346393, -1.199719254218446718 ) ) ;
#29868 = CARTESIAN_POINT ( 'NONE',  ( 2.255913092623571092, 0.8947350874906587759, 1.889642235345281307 ) ) ;
#29870 = CARTESIAN_POINT ( 'NONE',  ( 6.556249800660121529, 9.806652646482286073, 1.199719254218452047 ) ) ;
#29872 = EDGE_LOOP ( 'NONE', ( #8787, #197268, #30381, #53624, #5851 ) ) ;
#29871 = CARTESIAN_POINT ( 'NONE',  ( -0.09351100681491937572, -0.3904691765420374439, -1.774915231904458990 ) ) ;
#29873 = CARTESIAN_POINT ( 'NONE',  ( 3.967548030458594610, 0.2710504330169677401, -2.190103208553782821 ) ) ;
#29874 = CARTESIAN_POINT ( 'NONE',  ( 3.241465689944766915, -1.947025830926933043, 1.038692105600529159 ) ) ;
#29875 = CARTESIAN_POINT ( 'NONE',  ( 8.015895134177609904, 10.37496362800581018, 1.599625672291281386 ) ) ;
#29876 = CARTESIAN_POINT ( 'NONE',  ( -3.094265954482870118, 2.800000000000024691, 2.490342512183699508 ) ) ;
#29877 = CARTESIAN_POINT ( 'NONE',  ( 1.365713085969634477, 0.5541664655046051324, -1.830235057661818487 ) ) ;
#29878 = CARTESIAN_POINT ( 'NONE',  ( 9.480175724453529185, 12.08329098332774265, 1.599625672291279388 ) ) ;
#29879 = CARTESIAN_POINT ( 'NONE',  ( 3.947765587739564097, 1.497496809916948779, 1.429883829622953462 ) ) ;
#29881 = CARTESIAN_POINT ( 'NONE',  ( 2.624079441566569582, -1.243859440641072123, -1.767801033134681843 ) ) ;
#29880 = CARTESIAN_POINT ( 'NONE',  ( -2.103486388414573138, 5.605817886458954291, 1.040834085586084257E-14 ) ) ;
#29882 = CARTESIAN_POINT ( 'NONE',  ( 4.757479570170550787, 2.167726397749652367, -0.3216086267831194112 ) ) ;
#29883 = CARTESIAN_POINT ( 'NONE',  ( -5.943394452344507251, 6.548109163587250592, 0.8056209499170760013 ) ) ;
#29884 = CARTESIAN_POINT ( 'NONE',  ( 3.987613135628201633, 7.732542241470636846, 0.05202909940443302406 ) ) ;
#29885 = CARTESIAN_POINT ( 'NONE',  ( -0.4229270055063389377, 8.019365653748030454, 1.955756443285257218 ) ) ;
#29886 = CARTESIAN_POINT ( 'NONE',  ( 4.199993725183334803, 8.122019456014369254, -0.7998128361456362523 ) ) ;
#29887 = CARTESIAN_POINT ( 'NONE',  ( -1.642778471875000035, -3.055208332855375630, -2.845375778867859751 ) ) ;
#29888 = CARTESIAN_POINT ( 'NONE',  ( -4.359828915246279024, 7.244161613499399799, -1.199719254218455378 ) ) ;
#29889 = CARTESIAN_POINT ( 'NONE',  ( 0.5631252389872200004, -1.117830369828230808, 1.678006741548984770 ) ) ;
#29890 = CARTESIAN_POINT ( 'NONE',  ( -7.510853912290736289, 11.70648729774046792, 0.7216878364870458196 ) ) ;
#29891 = CARTESIAN_POINT ( 'NONE',  ( 4.645415698524104187, 1.851598927129451955, -0.9261206523473937136 ) ) ;
#29892 = CARTESIAN_POINT ( 'NONE',  ( 3.211465258343335627, -0.3752234067680487728, 1.889445157240315254 ) ) ;
#29893 = CARTESIAN_POINT ( 'NONE',  ( 6.046512527486515687, -1.496967179435993778, 1.497493072882298382 ) ) ;
#29894 = CARTESIAN_POINT ( 'NONE',  ( 4.476163270806094552, 8.373940915915776273, 0.7998128361456462443 ) ) ;
#29895 = PLANE ( 'NONE',  #174057 ) ;
#29896 = CARTESIAN_POINT ( 'NONE',  ( 3.924621296410530480, -1.326038130087652922, 1.456277141313151224 ) ) ;
#29897 = CARTESIAN_POINT ( 'NONE',  ( 6.404234474585668302, 1.703059896339639057, -1.534467582428314270 ) ) ;
#29898 = CARTESIAN_POINT ( 'NONE',  ( 4.019992336727182369, -0.9402185374879183932, -1.564826772493657536 ) ) ;
#29899 = PRODUCT ( 'rubber for air flow regulation', 'rubber for air flow regulation', '', ( #17933 ) ) ;
#29900 = CARTESIAN_POINT ( 'NONE',  ( 6.292392690518195941, 8.434487120394948079, -1.443375672974078761 ) ) ;
#29901 = CARTESIAN_POINT ( 'NONE',  ( 4.487385655998873624, 7.218738451098584363, 1.082531754730558626 ) ) ;
#29902 = CARTESIAN_POINT ( 'NONE',  ( -5.661411662158206681, 8.762674818229999829, -1.199719254218452047 ) ) ;
#29903 = CARTESIAN_POINT ( 'NONE',  ( 5.692444392891300886, 7.734547439830227411, -1.599625672291281386 ) ) ;
#29904 = ORIENTED_EDGE ( 'NONE', *, *, #181023, .F. ) ;
#29906 = CARTESIAN_POINT ( 'NONE',  ( 5.326436552476821795, -0.9091558477445594866, -1.796327993944699219 ) ) ;
#29905 = CARTESIAN_POINT ( 'NONE',  ( 2.014959344526063845, -1.785600367564584179, 0.4486904387498573676 ) ) ;
#29907 = CARTESIAN_POINT ( 'NONE',  ( 6.311202115008078373, 1.327223183623595704, -1.876690649992603044 ) ) ;
#29908 = CARTESIAN_POINT ( 'NONE',  ( 5.998874280538830206, 0.3792253423284037139, 1.924579554046601970 ) ) ;
#29909 = CARTESIAN_POINT ( 'NONE',  ( -5.530836599371015794, 8.540060901653093950, 1.199719254218452047 ) ) ;
#29910 = AXIS2_PLACEMENT_3D ( 'NONE', #37276, #36196, #168347 ) ;
#29911 = B_SPLINE_CURVE_WITH_KNOTS ( 'NONE', 3,
 ( #64250, #130392, #196383, #48024, #180132, #117319 ),
 .UNSPECIFIED., .F., .F.,
 ( 4, 2, 4 ),
 ( 0.000000000000000000, 0.0003778774010236168619, 0.0007557548020472337237 ),
 .UNSPECIFIED. ) ;
#29912 = CARTESIAN_POINT ( 'NONE',  ( -5.461236948206312114, 5.265864615862458464, 0.7998128361456341429 ) ) ;
#29913 =( LENGTH_UNIT ( ) NAMED_UNIT ( * ) SI_UNIT ( .MILLI., .METRE. ) );
#29914 = CARTESIAN_POINT ( 'NONE',  ( -3.800028193580205382, 7.655393002477360653, -0.7998128361456481317 ) ) ;
#29916 = CARTESIAN_POINT ( 'NONE',  ( 6.455894400631252417, 1.764744506579400962, -0.1349141608881914423 ) ) ;
#29915 = CARTESIAN_POINT ( 'NONE',  ( 2.015285228526709549, -2.027172053905087701, 0.5110949307850811696 ) ) ;
#29917 = CARTESIAN_POINT ( 'NONE',  ( -8.024744567526244765, -5.166862915010145052, 7.523999700038795702 ) ) ;
#29918 = CARTESIAN_POINT ( 'NONE',  ( -0.1104750535120268828, 7.629137130509074716, -2.703481013110929254 ) ) ;
#29919 = CARTESIAN_POINT ( 'NONE',  ( 1.487455728203713745, -1.732000560005091616, -0.1708635279896036641 ) ) ;
#29920 = CARTESIAN_POINT ( 'NONE',  ( 6.287230548435207567, 8.358188277972981695, -1.599625672291262513 ) ) ;
#29922 = CARTESIAN_POINT ( 'NONE',  ( 0.4999999999999553690, -1.387778780781445676E-14, -0.5000000000000507372 ) ) ;
#29921 = DIRECTION ( 'NONE',  ( -1.000000000000000000, 0.000000000000000000, 5.421010862427519212E-16 ) ) ;
#29923 = CARTESIAN_POINT ( 'NONE',  ( 1.804884324593715839, 1.432779585713826576, 0.9600471282974596399 ) ) ;
#29924 = CARTESIAN_POINT ( 'NONE',  ( 2.015410700679621137, -2.124826835150806392, 0.5361769018528695918 ) ) ;
#29925 = CARTESIAN_POINT ( 'NONE',  ( -0.08779760418278770295, -1.063538860511966444, -1.369745729481768759 ) ) ;
#29926 = CARTESIAN_POINT ( 'NONE',  ( 3.932405576212230525, 1.181341412803040614, -1.863887651898883613 ) ) ;
#29927 = CARTESIAN_POINT ( 'NONE',  ( -10.44369633504468631, 5.112959841837462882, -5.232137017608346596 ) ) ;
#29928 = CARTESIAN_POINT ( 'NONE',  ( 1.551893958816989993, 1.642325835523240629, 1.420010234424383455 ) ) ;
#29929 = CARTESIAN_POINT ( 'NONE',  ( -0.02319159430949970999, 0.003959926571647092407, -1.810968101872318714 ) ) ;
#29930 = CARTESIAN_POINT ( 'NONE',  ( 3.362624215892480173, -2.041811681064845896, -0.5603701389207839112 ) ) ;
#29931 = CARTESIAN_POINT ( 'NONE',  ( 6.639320575229249677, 4.701313753536039641, 2.359456658813867236 ) ) ;
#29932 = ORIENTED_EDGE ( 'NONE', *, *, #37327, .T. ) ;
#29934 = CARTESIAN_POINT ( 'NONE',  ( 1.364683531249986537, 0.4677083336747514530, -0.7879004041258309554 ) ) ;
#29933 = CARTESIAN_POINT ( 'NONE',  ( 3.333774467322860868, 1.029290431845871989, -2.048349661755991313 ) ) ;
#29935 = PRESENTATION_STYLE_ASSIGNMENT (( #13661 ) ) ;
#29936 = CARTESIAN_POINT ( 'NONE',  ( 5.854423403002611437, 5.724582146458163656, 1.040834085586084257E-14 ) ) ;
#29937 = CARTESIAN_POINT ( 'NONE',  ( 5.690131909746282801, 1.321361375537116967, 1.785392519086197671 ) ) ;
#29938 = CARTESIAN_POINT ( 'NONE',  ( -5.748293942514172805, 8.689798118699771479, -1.082531754730538864 ) ) ;
#29939 = CARTESIAN_POINT ( 'NONE',  ( 5.856759171423504107, 5.935233242856626568, -0.7216878364870257245 ) ) ;
#29940 = CARTESIAN_POINT ( 'NONE',  ( -7.253248993186740989, 9.485209796849769504, 1.443375672974090751 ) ) ;
#29941 = CARTESIAN_POINT ( 'NONE',  ( 3.743459811148990291, 7.381470523066878009, -0.7216878364870338292 ) ) ;
#29943 = EDGE_LOOP ( 'NONE', ( #126753, #49101, #153179, #58864, #57822, #128190, #148822, #178631 ) ) ;
#29942 = AXIS2_PLACEMENT_3D ( 'NONE', #184411, #84790, #52296 ) ;
#29944 = CARTESIAN_POINT ( 'NONE',  ( 3.762342404062005041, 1.897698010425369786, -0.6819954029829021769 ) ) ;
#29946 = CARTESIAN_POINT ( 'NONE',  ( 2.746997431529357492, -0.3482204723163102034, -2.032804898803519222 ) ) ;
#29945 = CARTESIAN_POINT ( 'NONE',  ( 6.959412922516382771, 7.013736585890911535, 0.7998128361456341429 ) ) ;
#29947 = FACE_BOUND ( 'NONE', #103987, .T. ) ;
#29948 = CARTESIAN_POINT ( 'NONE',  ( 5.031484404002879884, 6.963427452793765404, 1.443375672974065660 ) ) ;
#29949 = CARTESIAN_POINT ( 'NONE',  ( 0.000000000000000000, -1.000000000000000888, 0.000000000000000000 ) ) ;
#29950 = CARTESIAN_POINT ( 'NONE',  ( -0.6823417656250212460, 4.551041667008086655, 1.181850606188767472 ) ) ;
#29951 = CARTESIAN_POINT ( 'NONE',  ( 4.945371362016417471, 0.6893947036107104243, -2.080263006054481334 ) ) ;
#29952 = CARTESIAN_POINT ( 'NONE',  ( 2.918592439375994552, -1.356299846568160827, -1.492255409411530120 ) ) ;
#29953 = CARTESIAN_POINT ( 'NONE',  ( 1.751249726499287673, 1.836263021919124050, -0.1365115386888632321 ) ) ;
#29954 = CARTESIAN_POINT ( 'NONE',  ( 8.229962938695207342, 9.560377169021284871, 1.199719254218462483 ) ) ;
#29955 = CARTESIAN_POINT ( 'NONE',  ( 5.491160184941096922, 1.609068807629027820, -0.8623064814072267659 ) ) ;
#29956 = CARTESIAN_POINT ( 'NONE',  ( 5.924453975591452703, -1.462443569488897754, -1.388487997949397368 ) ) ;
#29957 = CARTESIAN_POINT ( 'NONE',  ( -7.690499447449645309, 9.995335326823163058, 1.599625672291295375 ) ) ;
#29959 = CARTESIAN_POINT ( 'NONE',  ( -4.457598643843001973, 8.422558527783969851, 0.000000000000000000 ) ) ;
#29958 = CARTESIAN_POINT ( 'NONE',  ( 5.401357799220028788, 1.846321421614788516, 1.307461012187713933 ) ) ;
#29960 = CARTESIAN_POINT ( 'NONE',  ( 1.137491875146545039, -1.903277616399126293, 0.9019996372539202945 ) ) ;
#29961 = CARTESIAN_POINT ( 'NONE',  ( -7.774674742793745708, 8.035151719539642912, 0.7998128361456341429 ) ) ;
#29962 = CARTESIAN_POINT ( 'NONE',  ( 9.915090410295563927, 10.46202698829998567, -0.7998128361456281477 ) ) ;
#29963 = DIRECTION ( 'NONE',  ( 0.1393702726263792435, 0.3878236455354701073, 0.9111359651948915950 ) ) ;
#29964 = CARTESIAN_POINT ( 'NONE',  ( -6.503107236049161521, 10.73870887536603291, 0.7998128361456481317 ) ) ;
#29965 = UNCERTAINTY_MEASURE_WITH_UNIT (LENGTH_MEASURE( 1.000000000000000082E-05 ), #78184, 'distance_accuracy_value', 'NONE');
#29966 = CARTESIAN_POINT ( 'NONE',  ( -7.100579091573050228, -6.583980363594990948, 6.484567079770452658 ) ) ;
#29967 = CARTESIAN_POINT ( 'NONE',  ( 8.025500584646550806, 8.327781868367935658, 0.000000000000000000 ) ) ;
#29968 = CARTESIAN_POINT ( 'NONE',  ( 5.458613854904844409, 6.252117202148153474, -1.007154897844428687 ) ) ;
#29969 = CARTESIAN_POINT ( 'NONE',  ( -8.785320351975364872, 12.23299559640450518, 1.082531754730560403 ) ) ;
#29971 = CARTESIAN_POINT ( 'NONE',  ( 2.584490447655915624, 1.192291587189574065, 1.874175285706691341 ) ) ;
#29970 = CARTESIAN_POINT ( 'NONE',  ( 1.828540510153942922, -1.004066958311781832, -1.867862179375394005 ) ) ;
#29972 = DIRECTION ( 'NONE',  ( 1.224646799147353454E-16, 0.000000000000000000, -1.000000000000000000 ) ) ;
#29973 = CARTESIAN_POINT ( 'NONE',  ( -5.692444392891315097, 7.734547439830227411, -1.599625672291271394 ) ) ;
#29974 = CARTESIAN_POINT ( 'NONE',  ( 5.438792177376376991, 9.497007973581119700, 1.040834085586084257E-14 ) ) ;
#29975 = CARTESIAN_POINT ( 'NONE',  ( 3.455471728117681440, 1.544996161402897528, 1.208956721487665087 ) ) ;
#29976 = CARTESIAN_POINT ( 'NONE',  ( 4.788000803920411386, 8.737751371215816576, 1.040834085586084257E-14 ) ) ;
#29977 = CARTESIAN_POINT ( 'NONE',  ( -4.295139169456660078, 7.266651303919805294, 0.9588947021764819834 ) ) ;
#29978 = CARTESIAN_POINT ( 'NONE',  ( 3.011882680530176604, 6.665613560593854459, 0.7998128361456341429 ) ) ;
#29979 = CARTESIAN_POINT ( 'NONE',  ( -5.478903473698268023, 5.564677938835638216, -0.7216878364870338292 ) ) ;
#29981 = CARTESIAN_POINT ( 'NONE',  ( -7.375272376154096143, 8.667201196010339004, -1.082531754730544860 ) ) ;
#29980 = CIRCLE ( 'NONE', #185645, 0.08000000000000020983 ) ;
#29982 = CARTESIAN_POINT ( 'NONE',  ( 2.267978396857213585, 0.5610993688725562922, -2.044979925899123252 ) ) ;
#29983 = CARTESIAN_POINT ( 'NONE',  ( -4.447956913735107598, 7.346977611736363656, 1.199719254218452935 ) ) ;
#29984 = CARTESIAN_POINT ( 'NONE',  ( 3.977527890101069996, 2.036293384626610248, -0.7259696361804208742 ) ) ;
#29985 = CARTESIAN_POINT ( 'NONE',  ( 2.296224312773272658, 1.477747569344042500, -1.098160524033331642 ) ) ;
#29986 = CARTESIAN_POINT ( 'NONE',  ( -4.338815981289680934, 7.218015932674029855, 1.009429000442535918 ) ) ;
#29987 = CARTESIAN_POINT ( 'NONE',  ( 0.6823417656249899377, 0.6552083336747518416, 1.181850606188755259 ) ) ;
#29988 = CARTESIAN_POINT ( 'NONE',  ( 5.859256971114414014, 1.713395515214741538, -0.3040290152411839752 ) ) ;
#29989 = CARTESIAN_POINT ( 'NONE',  ( -1.992711204631002198E-15, 2.999999999999989342, 1.224999999999989875 ) ) ;
#29990 = CARTESIAN_POINT ( 'NONE',  ( 4.202664430556254160, 5.926194473780837413, 1.443375672974062551 ) ) ;
#29991 = VECTOR ( 'NONE', #207709, 1000.000000000000000 ) ;
#29992 = CARTESIAN_POINT ( 'NONE',  ( 2.852577672069932735, 0.7271573612388192442, 2.035869728763760378 ) ) ;
#29993 = ADVANCED_FACE ( 'NONE', ( #179588 ), #46394, .F. ) ;
#29994 = CARTESIAN_POINT ( 'NONE',  ( 4.376327261493318410, -0.3474131038204917310, 1.985796694155849362 ) ) ;
#29995 = CARTESIAN_POINT ( 'NONE',  ( -7.632877294369372123, 11.84884791016554573, 0.7216878364870458196 ) ) ;
#29996 = CARTESIAN_POINT ( 'NONE',  ( 2.325270847726228940, -0.0006328605136555342939, 2.161883445422786654 ) ) ;
#29997 = CARTESIAN_POINT ( 'NONE',  ( 2.565645918639497314, 1.934049084626581205, -0.3809019065194594877 ) ) ;
#29998 = CARTESIAN_POINT ( 'NONE',  ( 2.923064838257955156, -1.776166165677966591, 0.9548571111624851726 ) ) ;
#29999 = FACE_OUTER_BOUND ( 'NONE', #87328, .T. ) ;
#30000 = CARTESIAN_POINT ( 'NONE',  ( 4.511236532831874868, -1.903902423773628838, 0.3822933785788319438 ) ) ;
#30003 = VERTEX_POINT ( 'NONE', #81012 ) ;
#30002 = DIRECTION ( 'NONE',  ( 1.000000000000000000, 0.000000000000000000, 0.000000000000000000 ) ) ;
#30001 = CARTESIAN_POINT ( 'NONE',  ( -8.093854517234044366, 11.42628545587295186, 1.082531754730549967 ) ) ;
#30004 = CIRCLE ( 'NONE', #99271, 0.08000000000000014044 ) ;
#30005 = CARTESIAN_POINT ( 'NONE',  ( -3.160459205317013076, 6.701303149596211206, -0.7216878364870458196 ) ) ;
#30006 = CARTESIAN_POINT ( 'NONE',  ( 11.89844258446855285, 9.771473106700369726, 1.560502987793273233 ) ) ;
#30008 = ORIENTED_EDGE ( 'NONE', *, *, #158451, .T. ) ;
#30007 = CARTESIAN_POINT ( 'NONE',  ( -4.522526758610270647, 7.433975764090723359, -1.199719254218453823 ) ) ;
#30009 = CARTESIAN_POINT ( 'NONE',  ( -9.124274191872640216, 10.70770331434866485, -1.082531754730537976 ) ) ;
#30010 = CARTESIAN_POINT ( 'NONE',  ( 1.483733071427257411, 2.038639745401783721, -0.8453341458589253010 ) ) ;
#30011 = CARTESIAN_POINT ( 'NONE',  ( 3.285556943750000070, -1.684374999522043836, 0.000000000000000000 ) ) ;
#30012 = CARTESIAN_POINT ( 'NONE',  ( 5.735196368693616265, -0.04450293679344322767, -1.961403813732150780 ) ) ;
#30013 = CARTESIAN_POINT ( 'NONE',  ( -2.788906526875773208E-15, 8.937500000000001776, -1.499999999999998446 ) ) ;
#30014 = CARTESIAN_POINT ( 'NONE',  ( -0.7500000000000215383, 4.472916667349482012, 1.299038105676671107 ) ) ;
#30015 = CARTESIAN_POINT ( 'NONE',  ( 5.841900715481964212, 6.189949835993628469, -0.9061318016433889122 ) ) ;
#30016 = CARTESIAN_POINT ( 'NONE',  ( 3.820104440490858622, 1.748809976318686177, 0.5759312369505511509 ) ) ;
#30017 = ORIENTED_EDGE ( 'NONE', *, *, #12435, .T. ) ;
#30018 = CARTESIAN_POINT ( 'NONE',  ( 0.6801582343749744686, -0.7760416663252778235, 1.178068619123799898 ) ) ;
#30019 = CARTESIAN_POINT ( 'NONE',  ( -8.355902744723985975, 8.642974711799791265, 1.040834085586084257E-14 ) ) ;
#30020 = CARTESIAN_POINT ( 'NONE',  ( 8.002408263930250953, -6.836568542494980250, -7.346809171966436125 ) ) ;
#30021 = FACE_OUTER_BOUND ( 'NONE', #97888, .T. ) ;
#30022 = CARTESIAN_POINT ( 'NONE',  ( 4.625302960556422427, 8.547937220624488575, 1.040834085586084257E-14 ) ) ;
#30023 = CARTESIAN_POINT ( 'NONE',  ( 0.09275324736048547181, -0.4491109574935348014, -2.018345435551980316 ) ) ;
#30024 = ADVANCED_FACE ( 'NONE', ( #213124 ), #8122, .T. ) ;
#30027 = CARTESIAN_POINT ( 'NONE',  ( 3.350949008998193257, 0.4442310927498266948, -1.786741727165648497 ) ) ;
#30026 = CARTESIAN_POINT ( 'NONE',  ( 1.732617751151921404, -1.765751579927745007, -0.5880843478397956847 ) ) ;
#30025 = FACE_OUTER_BOUND ( 'NONE', #152812, .T. ) ;
#30028 = CARTESIAN_POINT ( 'NONE',  ( 7.771848369131631351, 10.09024240211882351, -1.599625672291262513 ) ) ;
#30029 = CYLINDRICAL_SURFACE ( 'NONE', #172710, 10.99999999999999112 ) ;
#30030 = CARTESIAN_POINT ( 'NONE',  ( -7.605197822622922210, 7.837428646007010613, -0.7998128361456362523 ) ) ;
#30031 = CARTESIAN_POINT ( 'NONE',  ( 3.834746474454188013E-15, 10.56250000000000178, 1.500000000000001554 ) ) ;
#30032 = CARTESIAN_POINT ( 'NONE',  ( 3.000804911251079510, -0.6410980074830170405, -2.111705341948390657 ) ) ;
#30033 = CARTESIAN_POINT ( 'NONE',  ( 6.450461099754450700, 0.7004171410973459855, 2.151357330220986963 ) ) ;
#30034 = CARTESIAN_POINT ( 'NONE',  ( -5.246642258808529746, 9.064907035344523578, 0.000000000000000000 ) ) ;
#30035 = CARTESIAN_POINT ( 'NONE',  ( 5.818593503215891971, -0.6604613111419742610, -1.687090931240011527 ) ) ;
#30036 = CARTESIAN_POINT ( 'NONE',  ( 6.227746030346171580, 0.7262518248569529433, -1.772935525165220128 ) ) ;
#30037 = CARTESIAN_POINT ( 'NONE',  ( -3.619250341048971809, 3.172667246362773863, -2.499999999999999556 ) ) ;
#30038 = CARTESIAN_POINT ( 'NONE',  ( 6.473518811298506925, 1.789458955665638618, -0.5451884755478533240 ) ) ;
#30039 = CARTESIAN_POINT ( 'NONE',  ( 6.373497979817693171, -0.2265250974912805249, 1.847160380126455559 ) ) ;
#30040 = CARTESIAN_POINT ( 'NONE',  ( 3.538314903486612817, 7.071858454135611538, 1.040834085586084257E-14 ) ) ;
#30041 = CARTESIAN_POINT ( 'NONE',  ( 6.280137008050575176, -0.9429096061123897199, 1.497559920798942512 ) ) ;
#30042 = CARTESIAN_POINT ( 'NONE',  ( 1.639861632979456418, 2.010800986640928656, -0.1531718788195315928 ) ) ;
#30044 = CARTESIAN_POINT ( 'NONE',  ( 2.543703448412675261, -1.561038821359970408, -1.413940773279374508 ) ) ;
#30043 = CARTESIAN_POINT ( 'NONE',  ( -10.32861409551237486, 10.94447128771960287, 1.040834085586084257E-14 ) ) ;
#30045 = CARTESIAN_POINT ( 'NONE',  ( 9.759171643738394408, 10.28012176064996197, 0.000000000000000000 ) ) ;
#30047 = CARTESIAN_POINT ( 'NONE',  ( -8.829384350997580455, 11.32403438096243775, 1.599625672291269396 ) ) ;
#30046 = CARTESIAN_POINT ( 'NONE',  ( -1.500000000000001332, -0.5999999999999755529, 0.000000000000000000 ) ) ;
#30048 = CARTESIAN_POINT ( 'NONE',  ( 6.983263157960366563, 7.629137130509066722, 2.653810918356712900 ) ) ;
#30049 = CARTESIAN_POINT ( 'NONE',  ( 2.443623115440888061, -1.883043647339300186, 0.7309814453849405869 ) ) ;
#30050 = CARTESIAN_POINT ( 'NONE',  ( -0.6823417656250003738, 2.967708333674754062, -1.181850606188749264 ) ) ;
#30051 = CARTESIAN_POINT ( 'NONE',  ( 8.595506201383999567, 12.97191496834930113, 0.7216878364870438212 ) ) ;
#30052 = ADVANCED_FACE ( 'NONE', ( #164399 ), #15982, .F. ) ;
#30053 = CARTESIAN_POINT ( 'NONE',  ( 3.813887338145681927, -2.130327034543195275, 0.3653767458386343314 ) ) ;
#30054 = CARTESIAN_POINT ( 'NONE',  ( 7.876360894896227371, 8.153785563659219804, -0.7998128361456341429 ) ) ;
#30056 = DIRECTION ( 'NONE',  ( -2.253752739989063359E-14, 4.419671232041788924E-16, 1.000000000000000000 ) ) ;
#30055 = CARTESIAN_POINT ( 'NONE',  ( 4.934241560730721510, 4.721313007132757811, 0.000000000000000000 ) ) ;
#30057 = CARTESIAN_POINT ( 'NONE',  ( 10.50720586046655391, 11.36075438007358507, 0.7216878364870438212 ) ) ;
#30059 = CARTESIAN_POINT ( 'NONE',  ( 0.000000000000000000, 1.899999999999999023, 0.000000000000000000 ) ) ;
#30058 = CARTESIAN_POINT ( 'NONE',  ( 1.135490968158389791, -0.05309211241652118246, -2.170675730929682246 ) ) ;
#30060 = CARTESIAN_POINT ( 'NONE',  ( -5.531363484695544841, 8.436712584578003771, 1.082531754730548412 ) ) ;
#30061 = VECTOR ( 'NONE', #153985, 1000.000000000000000 ) ;
#30062 = CARTESIAN_POINT ( 'NONE',  ( 1.364683531249986537, 1.113541667008082658, 0.7879004041258500513 ) ) ;
#30063 = CARTESIAN_POINT ( 'NONE',  ( 2.577880719133851084, -1.123996537731044354, 1.881222605751430521 ) ) ;
#30064 = CARTESIAN_POINT ( 'NONE',  ( -3.511198596259319960, 6.271927390929313617, 1.082471891955974153 ) ) ;
#30065 = CARTESIAN_POINT ( 'NONE',  ( 2.676973543053912330, -2.164909235287615807, -0.6573374913001366338 ) ) ;
#30066 = CARTESIAN_POINT ( 'NONE',  ( -6.821723845970312894, 11.11042825360738284, 0.000000000000000000 ) ) ;
#30067 = CARTESIAN_POINT ( 'NONE',  ( -3.917943204224928699, 4.633650495426258509, -1.082531754730548412 ) ) ;
#30068 = CARTESIAN_POINT ( 'NONE',  ( 0.6823417656249899377, 3.988541667008085767, -1.181850606188754593 ) ) ;
#30069 = CARTESIAN_POINT ( 'NONE',  ( 4.802738015080052492, 8.126035781178083894, 0.8349615142884360131 ) ) ;
#30070 = CARTESIAN_POINT ( 'NONE',  ( -1.402160292154681736E-14, 11.31249999999999822, 1.732050807568881190 ) ) ;
#30071 = CARTESIAN_POINT ( 'NONE',  ( 5.831415467653547680, 8.857049574687536619, -1.082531754730548412 ) ) ;
#30072 = ADVANCED_FACE ( 'NONE', ( #161205 ), #82067, .F. ) ;
#30073 = CARTESIAN_POINT ( 'NONE',  ( 2.758786678070863196, -1.537680025927037786, -0.8759604286991302668 ) ) ;
#30074 = CARTESIAN_POINT ( 'NONE',  ( 7.574201371528760163, 11.98831870009225931, 1.040834085586084257E-14 ) ) ;
#30075 = CARTESIAN_POINT ( 'NONE',  ( 6.053802686139254874, 0.6462426183462595120, -2.110027337871730690 ) ) ;
#30076 = CARTESIAN_POINT ( 'NONE',  ( -0.6823417656250039265, 9.317708333674733723, -1.181850606188755259 ) ) ;
#30077 = CARTESIAN_POINT ( 'NONE',  ( -3.800028193580205382, 7.655393002477360653, -0.7998128361456481317 ) ) ;
#30078 = CARTESIAN_POINT ( 'NONE',  ( -0.1400748609342543360, 7.098713645440452247, -2.115199198882514953 ) ) ;
#30079 = VERTEX_POINT ( 'NONE', #167598 ) ;
#30080 = CARTESIAN_POINT ( 'NONE',  ( 3.590566789841375339, -0.3639703897368729568, -1.834726254853453087 ) ) ;
#30081 = CARTESIAN_POINT ( 'NONE',  ( 3.678634981485491728, 1.317094234756083893, -1.597214816249421743 ) ) ;
#30082 = CARTESIAN_POINT ( 'NONE',  ( -5.763624699140874164, 8.777960344756069233, -1.082531754730549967 ) ) ;
#30083 = DIRECTION ( 'NONE',  ( -1.000000000000000000, 0.000000000000000000, 0.000000000000000000 ) ) ;
#30084 = PRESENTATION_LAYER_ASSIGNMENT (  '', '', ( #202924 ) ) ;
#30085 = CARTESIAN_POINT ( 'NONE',  ( -10.82855876678636520, 5.585670971531701667, -6.509986581443756748 ) ) ;
#30086 = SURFACE_SIDE_STYLE ('',( #46348 ) ) ;
#30087 = ADVANCED_FACE ( 'NONE', ( #36518 ), #197973, .T. ) ;
#30088 = CARTESIAN_POINT ( 'NONE',  ( -1.402160292154681736E-14, -0.9281249996585830830, 1.575800808251672791 ) ) ;
#30089 = CARTESIAN_POINT ( 'NONE',  ( 2.945700582358207864, 1.385421296276163838, 1.389331660621349274 ) ) ;
#30090 = EDGE_CURVE ( 'NONE', #135613, #80197, #150485, .T. ) ;
#30091 = CARTESIAN_POINT ( 'NONE',  ( 0.4036724312478366938, 0.3418800534340654118, 1.986742826083332858 ) ) ;
#30092 = CARTESIAN_POINT ( 'NONE',  ( -4.037141169473096980, 7.765219724388391143, 0.5542112752373774542 ) ) ;
#30093 = CARTESIAN_POINT ( 'NONE',  ( 8.097244055859613709, 10.46987070330147063, -1.599625672291262513 ) ) ;
#30094 = CARTESIAN_POINT ( 'NONE',  ( 0.9131076777311696313, -0.2804849920042574718, 1.849292663789033009 ) ) ;
#30095 = CARTESIAN_POINT ( 'NONE',  ( -1.364683531250012516, 3.238541667008084879, -0.7879004041258289570 ) ) ;
#30096 = CARTESIAN_POINT ( 'NONE',  ( 2.619392002094393490, 1.702953528017937090, 1.073460467912157101 ) ) ;
#30098 = CARTESIAN_POINT ( 'NONE',  ( 2.636446987817195886, 0.7160595562910974099, 1.992577970932450704 ) ) ;
#30097 = CARTESIAN_POINT ( 'NONE',  ( -7.863365906246074566, 8.276274433482971205, -0.7216878364870278340 ) ) ;
#30099 = CARTESIAN_POINT ( 'NONE',  ( 7.127284358736648784, 14.48154074412736669, -9.657187355191572564 ) ) ;
#30100 = CARTESIAN_POINT ( 'NONE',  ( 3.596198176508007105, 0.9334358170956689182, -1.848091447891623051 ) ) ;
#30101 = CARTESIAN_POINT ( 'NONE',  ( 7.180978637093494044, 8.406838493811077839, -1.199719254218452047 ) ) ;
#30103 = CARTESIAN_POINT ( 'NONE',  ( 4.241003122976366058, 3.842258486427521103, -0.7998128361456211532 ) ) ;
#30102 = CARTESIAN_POINT ( 'NONE',  ( 5.507793336809221785, -0.9391204764703815489, -1.867914344430561702 ) ) ;
#30105 = ORIENTED_EDGE ( 'NONE', *, *, #144093, .F. ) ;
#30104 = CARTESIAN_POINT ( 'NONE',  ( 4.418855976699648025, 1.669273799801282765, 0.7395231729718022562 ) ) ;
#30106 = CARTESIAN_POINT ( 'NONE',  ( 9.215791728987056786, 11.77484298861683598, -1.599625672291262513 ) ) ;
#30107 = CARTESIAN_POINT ( 'NONE',  ( 6.639320575229292309, -0.003630812595115444526, 2.203388474976493594 ) ) ;
#30108 = CARTESIAN_POINT ( 'NONE',  ( 11.49537292513043951, 8.930514822958286913, -3.071439876058613461 ) ) ;
#30109 = CARTESIAN_POINT ( 'NONE',  ( 6.510767885691055135, 1.639592601025055885, -1.477219212978691409 ) ) ;
#30110 = CARTESIAN_POINT ( 'NONE',  ( -0.6823417656250003738, 10.21354166700806587, 1.181850606188754593 ) ) ;
#30111 = CARTESIAN_POINT ( 'NONE',  ( 5.391234928627540945, -0.05113397888981999206, -1.911771334517261778 ) ) ;
#30113 = CARTESIAN_POINT ( 'NONE',  ( -9.755255220232635693, 11.33988483081495957, -1.199719254218441611 ) ) ;
#30112 = COLOUR_RGB ( '', 0.66274510, 0.83137255, 0.94901961) ;
#30114 = CARTESIAN_POINT ( 'NONE',  ( 7.969495366734495434, 8.192166104145387706, 1.040834085586084257E-14 ) ) ;
#30115 = CARTESIAN_POINT ( 'NONE',  ( -4.156403723172807449E-14, 1.859375000341410900, -1.570758158831802254 ) ) ;
#30116 = CARTESIAN_POINT ( 'NONE',  ( 4.812781342726870193, 4.717259109377208048, 0.7216878364870317197 ) ) ;
#30117 = FACE_OUTER_BOUND ( 'NONE', #223, .T. ) ;
#30118 = CARTESIAN_POINT ( 'NONE',  ( 0.7492455685023796663, 1.839184785914184994, -0.09005233288367914257 ) ) ;
#30119 = ORIENTED_EDGE ( 'NONE', *, *, #47376, .T. ) ;
#30120 = AXIS2_PLACEMENT_3D ( 'NONE', #112645, #25978, #74746 ) ;
#30121 = SURFACE_STYLE_FILL_AREA ( #46381 ) ;
#30122 = CARTESIAN_POINT ( 'NONE',  ( 4.587079231881330266, 1.671727914585485530, -0.8392916717318498199 ) ) ;
#30123 = CARTESIAN_POINT ( 'NONE',  ( -9.367496997608917297, 14.57669131241553728, -7.413898975919227752 ) ) ;
#30124 = CARTESIAN_POINT ( 'NONE',  ( 6.801350335910821165, 7.963938809097990124, 1.199719254218452047 ) ) ;
#30125 = CARTESIAN_POINT ( 'NONE',  ( -6.773846765317339980, -7.552951973956472997, -6.773846765317302676 ) ) ;
#30126 = CARTESIAN_POINT ( 'NONE',  ( -6.027110718723775129, 7.076430883291389584, 1.047497865993127553 ) ) ;
#30127 = CARTESIAN_POINT ( 'NONE',  ( -5.965224400332865606, 7.022145224218852455, 1.082531754730549967 ) ) ;
#30128 = CARTESIAN_POINT ( 'NONE',  ( 4.334856428067313416, 6.080418470877079429, -1.599625672291256295 ) ) ;
#30129 = CARTESIAN_POINT ( 'NONE',  ( 1.024188300031657617, 0.9657954515097492143, 1.716266578800438536 ) ) ;
#30130 = CARTESIAN_POINT ( 'NONE',  ( 3.462517696756307384, -1.944077823024586538, -0.5350690621670484148 ) ) ;
#30131 = CARTESIAN_POINT ( 'NONE',  ( -6.507023659554960204, 9.678945805201045971, 1.199719254218452047 ) ) ;
#30132 = CARTESIAN_POINT ( 'NONE',  ( 4.193214648376505593, 8.114110533073061404, 0.000000000000000000 ) ) ;
#30133 = DIRECTION ( 'NONE',  ( -1.000000000000000000, 0.000000000000000000, 0.000000000000000000 ) ) ;
#30134 = PRESENTATION_LAYER_ASSIGNMENT (  '', '', ( #168516 ) ) ;
#30135 = CARTESIAN_POINT ( 'NONE',  ( 4.171962795014371395, -1.262591954434747921, 1.790989659139609724 ) ) ;
#30136 =( LENGTH_UNIT ( ) NAMED_UNIT ( * ) SI_UNIT ( .MILLI., .METRE. ) );
#30137 = CARTESIAN_POINT ( 'NONE',  ( -9.429859533504656000, 10.96025652963230534, -1.199719254218441611 ) ) ;
#30138 = CARTESIAN_POINT ( 'NONE',  ( 4.934241560730721510, 4.721313007132757811, 0.000000000000000000 ) ) ;
#30139 = CARTESIAN_POINT ( 'NONE',  ( 0.2331563151865729544, 2.882199166944008795, -2.434502449063076224 ) ) ;
#30140 = CARTESIAN_POINT ( 'NONE',  ( 3.716343503921665459, 6.389465617000312569, -1.082531754730549967 ) ) ;
#30141 = CARTESIAN_POINT ( 'NONE',  ( 6.771407655021410399, 9.987393799911945536, -1.199719254218441611 ) ) ;
#30142 = CARTESIAN_POINT ( 'NONE',  ( -9.367496997608871112, 15.42330868759649043, 7.413898975919298806 ) ) ;
#30143 = CARTESIAN_POINT ( 'NONE',  ( 6.875393295905841917, 7.193916064744513506, 0.000000000000000000 ) ) ;
#30144 = ORIENTED_EDGE ( 'NONE', *, *, #183770, .T. ) ;
#30146 = CARTESIAN_POINT ( 'NONE',  ( 2.279941584743001126, 1.973825526184776580, -0.3948664393432794184 ) ) ;
#30145 = CARTESIAN_POINT ( 'NONE',  ( 4.458453498679889826, -1.646799808365447149, -0.8236825204945982248 ) ) ;
#30147 = CARTESIAN_POINT ( 'NONE',  ( 3.954713598875368774, 1.661701185475419118, 1.588069724787332992 ) ) ;
#30149 = CARTESIAN_POINT ( 'NONE',  ( 1.692022144237431469, 0.9228297918665344657, -1.615966242530289199 ) ) ;
#30148 = CARTESIAN_POINT ( 'NONE',  ( -0.1291982275798807533, 2.865258409039960430, -2.562285117308207294 ) ) ;
#30150 = CARTESIAN_POINT ( 'NONE',  ( -3.285556943750000514, -1.538541666188708357, -1.896917185911906500 ) ) ;
#30151 = LINE ( 'NONE', #95174, #77765 ) ;
#30152 = CARTESIAN_POINT ( 'NONE',  ( 6.099862406061942188, 1.323743610676546334, 1.380425988546908567 ) ) ;
#30153 = CARTESIAN_POINT ( 'NONE',  ( -8.646349277213090545, 11.11049346154719508, 1.599625672291269396 ) ) ;
#30154 = CARTESIAN_POINT ( 'NONE',  ( -5.234856708652269042, 7.200695141551334721, 1.443375672974058777 ) ) ;
#30156 = CARTESIAN_POINT ( 'NONE',  ( 2.922558825391399662, 1.760836971185793187, 0.6318509464167121337 ) ) ;
#30155 = CARTESIAN_POINT ( 'NONE',  ( 5.232010533483211212, 2.060019964192044917, 0.3561100859283144460 ) ) ;
#30157 = CARTESIAN_POINT ( 'NONE',  ( 5.829642864196157070, 8.784705193995428374, 1.082531754730558626 ) ) ;
#30158 = CARTESIAN_POINT ( 'NONE',  ( 6.427308110136687347, -1.208249125052461181, -1.389453836245766016 ) ) ;
#30159 = CARTESIAN_POINT ( 'NONE',  ( 4.142179624174931796, 4.791296635414242111, 1.199719254218464037 ) ) ;
#30160 = LINE ( 'NONE', #78892, #130930 ) ;
#30161 = CARTESIAN_POINT ( 'NONE',  ( 5.408750372623219782, 1.302234988713904640, -1.131221429639968745 ) ) ;
#30162 = CARTESIAN_POINT ( 'NONE',  ( -6.307567778855718288, 8.381915046796901692, -1.599625672291263179 ) ) ;
#30163 = CARTESIAN_POINT ( 'NONE',  ( 0.3692042219665427893, -0.2092721526018372635, -1.721406745681583583 ) ) ;
#30164 = CARTESIAN_POINT ( 'NONE',  ( -10.38614328979765489, 3.507114751586604129, -5.996442624206661520 ) ) ;
#30165 =( LENGTH_UNIT ( ) NAMED_UNIT ( * ) SI_UNIT ( .MILLI., .METRE. ) );
#30166 = CARTESIAN_POINT ( 'NONE',  ( 4.803694799390169301, -1.674174935400191799, -1.382237342716886586 ) ) ;
#30167 = CARTESIAN_POINT ( 'NONE',  ( 3.545350327189537687, -1.383302465072188792, -1.191577590537174158 ) ) ;
#30168 = CARTESIAN_POINT ( 'NONE',  ( 1.569116724355507975, 1.727593668635756918, 0.9295332132536607839 ) ) ;
#30169 = CARTESIAN_POINT ( 'NONE',  ( 0.3162073025194310771, 1.084344979787469354, -1.818339158833045976 ) ) ;
#30171 = CARTESIAN_POINT ( 'NONE',  ( 0.6823417656249899377, 4.238541667008085767, -1.181850606188754593 ) ) ;
#30170 = CARTESIAN_POINT ( 'NONE',  ( 0.6040055286682350921, -2.280654241543427663, 0.2304348961432670095 ) ) ;
#30172 = CARTESIAN_POINT ( 'NONE',  ( 9.920930332858631573, -7.768188185258914302, -0.4648879685169824416 ) ) ;
#30173 = CARTESIAN_POINT ( 'NONE',  ( 7.228468454380276853, 11.58496363008569574, 1.040834085586084257E-14 ) ) ;
#30174 = CARTESIAN_POINT ( 'NONE',  ( 3.106218681870171139, -0.8574772492565514437, 1.939554460742904274 ) ) ;
#30175 = CARTESIAN_POINT ( 'NONE',  ( -4.121315508874269007, 5.831287398485176077, -1.443375672974053447 ) ) ;
#30176 = CARTESIAN_POINT ( 'NONE',  ( 5.600441157405738224, 5.741305760636564059, 0.6425381723618078800 ) ) ;
#30177 = CARTESIAN_POINT ( 'NONE',  ( -4.622967192135580383, 5.456178481322002227, 1.082531754730558626 ) ) ;
#30178 =( BOUNDED_SURFACE ( )  B_SPLINE_SURFACE ( 3, 2, ( 
 ( #117386, #51261, #148760 ),
 ( #186582, #16594, #3538 ),
 ( #183382, #34988, #167147 ),
 ( #166072, #84817, #198546 ),
 ( #116312, #184440, #150906 ),
 ( #103209, #153024, #100007 ),
 ( #200675, #70673, #52324 ),
 ( #86957, #118453, #136783 ),
 ( #36057, #102138, #168206 ),
 ( #4599, #202812, #19805 ) ),
 .UNSPECIFIED., .F., .F., .T. ) 
 B_SPLINE_SURFACE_WITH_KNOTS ( ( 4, 2, 2, 2, 4 ),
 ( 3, 3 ),
 ( 0.001504965851240676507, 0.001881207314050846718, 0.002257448776861016929, 0.002633690239671187573, 0.003009931702481357784 ),
 ( 0.000000000000000000, 1.000000000000000000 ),
 .UNSPECIFIED. ) 
 GEOMETRIC_REPRESENTATION_ITEM ( )  RATIONAL_B_SPLINE_SURFACE ( (
 ( 1.000000000000000000, 0.7796377409682132553, 1.000000000000000000),
 ( 1.000000000000000000, 0.7901490482358394241, 1.000000000000000000),
 ( 1.000000000000000000, 0.7828211856522472312, 1.000000000000000000),
 ( 1.000000000000000000, 0.7482553577056408889, 1.000000000000000000),
 ( 1.000000000000000000, 0.7228574685501613084, 1.000000000000000000),
 ( 1.000000000000000000, 0.7019526649397319629, 1.000000000000000000),
 ( 1.000000000000000000, 0.7095376569258128319, 1.000000000000000000),
 ( 1.000000000000000000, 0.7455209376246204611, 1.000000000000000000),
 ( 1.000000000000000000, 0.7705606446023164358, 1.000000000000000000),
 ( 1.000000000000000000, 0.7796368470575135712, 1.000000000000000000) ) ) 
 REPRESENTATION_ITEM ( '' )  SURFACE ( )  );
#30179 = CARTESIAN_POINT ( 'NONE',  ( 0.7782871991188352601, -1.104406889285912907, -1.750870654829151274 ) ) ;
#30181 = CARTESIAN_POINT ( 'NONE',  ( -1.500000000000001110, 13.80208333401613352, 0.8660254037844419273 ) ) ;
#30180 = CARTESIAN_POINT ( 'NONE',  ( 6.883263157960421097, 0.5621630953002605402, 2.205140871664055702 ) ) ;
#30182 = VERTEX_POINT ( 'NONE', #51726 ) ;
#30184 = ORIENTED_EDGE ( 'NONE', *, *, #105724, .F. ) ;
#30183 = CARTESIAN_POINT ( 'NONE',  ( 2.368119171756615238, 0.5893650439614643854, -2.141638343492527685 ) ) ;
#30185 = CARTESIAN_POINT ( 'NONE',  ( 0.2121463357745425049, 2.202340261784305753, 0.6586529460593565366 ) ) ;
#30187 = CARTESIAN_POINT ( 'NONE',  ( 5.172745336439665387, 1.426162745032448109, -1.490257803364034128 ) ) ;
#30186 = CARTESIAN_POINT ( 'NONE',  ( 9.083599731475976213, 12.58098820582193689, 1.082531754730546636 ) ) ;
#30189 = CARTESIAN_POINT ( 'NONE',  ( 3.475000000000000533, -1.895833333333332815, -2.006292185433951047 ) ) ;
#30188 = CARTESIAN_POINT ( 'NONE',  ( 5.611095471209277541, 7.639640364534566075, 1.599625672291268286 ) ) ;
#30190 = CARTESIAN_POINT ( 'NONE',  ( 6.574778147984297938, 6.635272358928617997, -0.7998128361456481317 ) ) ;
#30191 = FACE_OUTER_BOUND ( 'NONE', #51033, .T. ) ;
#30192 = CARTESIAN_POINT ( 'NONE',  ( 5.724118993814841794, 1.776208094789998304, 0.4848738846057951135 ) ) ;
#30193 = EDGE_CURVE ( 'NONE', #4671, #59479, #119987, .T. ) ;
#30194 = CARTESIAN_POINT ( 'NONE',  ( 3.408985558832261731, 6.064568021024562938, 1.199719254218462483 ) ) ;
#30195 =( NAMED_UNIT ( * ) PLANE_ANGLE_UNIT ( ) SI_UNIT ( $, .RADIAN. ) );
#30196 = CARTESIAN_POINT ( 'NONE',  ( 2.397083457474056267, 1.331176160016230847, 1.096701253500545148 ) ) ;
#30197 = CARTESIAN_POINT ( 'NONE',  ( 1.341030165941111241, -1.731997234073547220, -1.032477317303444053 ) ) ;
#30198 = CARTESIAN_POINT ( 'NONE',  ( 1.829147786997789016, 0.8750025983248543859, -2.125820487401499204 ) ) ;
#30199 = CARTESIAN_POINT ( 'NONE',  ( -1.364683531249997417, 3.821875000341416584, 1.214306433183764966E-14 ) ) ;
#30200 =( BOUNDED_CURVE ( )  B_SPLINE_CURVE ( 2, ( #1095, #84499, #166830, #133292, #199298, #101819, #50943, #150589, #86635 ),
 .UNSPECIFIED., .F., .T. ) 
 B_SPLINE_CURVE_WITH_KNOTS ( ( 3, 2, 2, 2, 3 ),
 ( 0.04687499999999977796, 0.05208333333333333565, 0.06250000000000000000, 0.07291666666666667129, 0.07812500000000006939 ),
 .UNSPECIFIED. ) 
 CURVE ( )  GEOMETRIC_REPRESENTATION_ITEM ( )  RATIONAL_B_SPLINE_CURVE ( ( 0.9330127018922194093, 0.9330127018922165227, 1.000000000000000000, 0.8660254037844387076, 1.000000000000000000, 0.8660254037844387076, 1.000000000000000000, 0.9330127018922185211, 0.9330127018922194093 ) ) 
 REPRESENTATION_ITEM ( '' )  );
#30201 = CARTESIAN_POINT ( 'NONE',  ( 2.056323133375201007, 2.256402538945650349, -0.1652075827990733270 ) ) ;
#30202 = CARTESIAN_POINT ( 'NONE',  ( 4.248724916491292802, 0.5614479688690295900, 2.029775142636090379 ) ) ;
#30203 = CARTESIAN_POINT ( 'NONE',  ( -5.320648938720212051, 5.172121614787156929, 0.000000000000000000 ) ) ;
#30204 = CARTESIAN_POINT ( 'NONE',  ( 2.231405582217013794, -1.152036887248751862, -1.343533879150171861 ) ) ;
#30205 = VECTOR ( 'NONE', #48363, 999.9999999999998863 ) ;
#30206 = CARTESIAN_POINT ( 'NONE',  ( 5.286789834324991055, 8.255339675766103724, -1.199719254218452935 ) ) ;
#30208 = CARTESIAN_POINT ( 'NONE',  ( 5.267208303392540536, 2.209927380382335826, -0.6089511437187348220 ) ) ;
#30207 = CARTESIAN_POINT ( 'NONE',  ( 4.977251789548238214, 7.860525283564661514, -1.082531754730548412 ) ) ;
#30209 = CARTESIAN_POINT ( 'NONE',  ( -4.412288926243578935, 7.235088616337731260, 1.199719254218464037 ) ) ;
#30210 = UNCERTAINTY_MEASURE_WITH_UNIT (LENGTH_MEASURE( 1.000000000000000082E-05 ), #27032, 'distance_accuracy_value', 'NONE');
#30211 = CARTESIAN_POINT ( 'NONE',  ( -1.499999999999997780, 2.400000000000020339, 1.214306433183764966E-14 ) ) ;
#30212 = EDGE_CURVE ( 'NONE', #21772, #111149, #115036, .T. ) ;
#30213 = CARTESIAN_POINT ( 'NONE',  ( 4.787173061057010237, 1.622617466453496471, 1.473133629693437197 ) ) ;
#30214 = CARTESIAN_POINT ( 'NONE',  ( -5.298539104842322267, 5.076050465271134016, 0.7998128361456341429 ) ) ;
#30215 = CARTESIAN_POINT ( 'NONE',  ( 0.000000000000000000, 3.500000000000003109, 0.000000000000000000 ) ) ;
#30216 =( BOUNDED_SURFACE ( )  B_SPLINE_SURFACE ( 3, 2, ( 
 ( #165587, #99527, #4123 ),
 ( #133126, #202326, #182897 ),
 ( #198076, #135247, #69125 ),
 ( #17180, #50768, #149340 ),
 ( #65918, #33450, #166660 ),
 ( #117970, #85400, #19323 ),
 ( #101654, #185017, #199124 ),
 ( #87546, #132065, #102727 ) ),
 .UNSPECIFIED., .F., .F., .F. ) 
 B_SPLINE_SURFACE_WITH_KNOTS ( ( 4, 2, 2, 4 ),
 ( 3, 3 ),
 ( 0.000000000000000000, 0.003124175592871729877, 0.004686263389307594382, 0.006248351185743459754 ),
 ( 0.000000000000000000, 1.000000000000000000 ),
 .UNSPECIFIED. ) 
 GEOMETRIC_REPRESENTATION_ITEM ( )  RATIONAL_B_SPLINE_SURFACE ( (
 ( 1.000000000000000000, 0.7762074382822415908, 1.000000000000000000),
 ( 1.000000000000000000, 0.7833327836897199248, 1.000000000000000000),
 ( 1.000000000000000000, 0.7920843231447862731, 1.000000000000000000),
 ( 1.000000000000000000, 0.8126254522527567303, 1.000000000000000000),
 ( 1.000000000000000000, 0.8207499603065130378, 1.000000000000000000),
 ( 1.000000000000000000, 0.8408200424460848810, 1.000000000000000000),
 ( 1.000000000000000000, 0.8529123454023501694, 1.000000000000000000),
 ( 1.000000000000000000, 0.8665634049582059406, 1.000000000000000000) ) ) 
 REPRESENTATION_ITEM ( '' )  SURFACE ( )  );
#30217 = CARTESIAN_POINT ( 'NONE',  ( 11.89942855770814312, 9.799999999999998934, -0.7000000000000009548 ) ) ;
#30218 = CARTESIAN_POINT ( 'NONE',  ( 0.6823417656249899377, 5.176041667008086655, -1.181850606188754593 ) ) ;
#30219 = CARTESIAN_POINT ( 'NONE',  ( 2.789578772358902281, 1.362584191422511415, 1.362147869459982230 ) ) ;
#30220 = CARTESIAN_POINT ( 'NONE',  ( 0.6823417656249934904, 8.692708333674733723, 1.181850606188764807 ) ) ;
#30221 = CARTESIAN_POINT ( 'NONE',  ( -2.819732761962332024, 6.233512622357263666, -0.7216878364870267237 ) ) ;
#30222 = CARTESIAN_POINT ( 'NONE',  ( 5.220985865760717992, 1.604251394084664550, -1.386888226476624242 ) ) ;
#30223 = CARTESIAN_POINT ( 'NONE',  ( -6.129694847154222970, 7.284303755502281597, -1.082531754730549967 ) ) ;
#30224 = ORIENTED_EDGE ( 'NONE', *, *, #204793, .F. ) ;
#30226 = CARTESIAN_POINT ( 'NONE',  ( 0.000000000000000000, 0.4000000000000010214, 0.000000000000000000 ) ) ;
#30225 = CARTESIAN_POINT ( 'NONE',  ( -5.980555157403903976, 6.149938236492225485, 0.000000000000000000 ) ) ;
#30227 = CARTESIAN_POINT ( 'NONE',  ( 3.344057444064992168, 7.053150784717805877, 1.040834085586084257E-14 ) ) ;
#30228 = CARTESIAN_POINT ( 'NONE',  ( 5.724118993814841794, 1.776208094789998304, 0.4848738846057951135 ) ) ;
#30229 = CARTESIAN_POINT ( 'NONE',  ( 0.4131705840078804814, 6.915508634455322046, -3.854011512607138812 ) ) ;
#30230 = CARTESIAN_POINT ( 'NONE',  ( -1.364683531250010295, 4.592708333674755394, 0.7879004041258379498 ) ) ;
#30231 = CARTESIAN_POINT ( 'NONE',  ( 2.542201289624079319, -1.445942355291447434, 0.9683529963873671598 ) ) ;
#30232 = DIRECTION ( 'NONE',  ( 0.000000000000000000, 1.000000000000000000, 0.000000000000000000 ) ) ;
#30234 = EDGE_CURVE ( 'NONE', #146583, #36604, #76921, .T. ) ;
#30233 = CARTESIAN_POINT ( 'NONE',  ( 0.2034672893990868703, -1.513989045467616146, -1.247398002513319781 ) ) ;
#30235 = CARTESIAN_POINT ( 'NONE',  ( -1.364683531250000748, 0.07187500034142035865, 0.000000000000000000 ) ) ;
#30236 = LINE ( 'NONE', #129948, #52822 ) ;
#30237 = CARTESIAN_POINT ( 'NONE',  ( 5.875883356151954118, 1.283970044810868849, 1.738936680771227206 ) ) ;
#30238 = EDGE_CURVE ( 'NONE', #22926, #71404, #200077, .T. ) ;
#30239 = CARTESIAN_POINT ( 'NONE',  ( -10.32183501870554387, 10.93656236477829502, 0.7998128361456462443 ) ) ;
#30240 = CARTESIAN_POINT ( 'NONE',  ( -5.544921637864824504, 8.452530429942200385, -1.082531754730543971 ) ) ;
#30241 = CARTESIAN_POINT ( 'NONE',  ( 6.297764839082774735, -0.7330946318361495351, 2.033732118066629457 ) ) ;
#30243 = VERTEX_POINT ( 'NONE', #37596 ) ;
#30242 = CARTESIAN_POINT ( 'NONE',  ( -0.2726351642629555871, -5.197079954928571333, -10.99683038201373719 ) ) ;
#30244 = CARTESIAN_POINT ( 'NONE',  ( 0.6823417656249917140, 4.092708333674755394, 1.181850606188765695 ) ) ;
#30245 = CARTESIAN_POINT ( 'NONE',  ( 6.257099195183372764, -1.689481296825417811, -1.015638971094455556 ) ) ;
#30246 = CARTESIAN_POINT ( 'NONE',  ( 5.887993837006205489, -0.03927123031851989521, 1.733586367271770179 ) ) ;
#30248 = CARTESIAN_POINT ( 'NONE',  ( 2.823975127348025804, 1.215230906543849354, -1.823574674616668556 ) ) ;
#30247 = CARTESIAN_POINT ( 'NONE',  ( -3.956095110007852622E-14, 0.3281250003414356020, -1.570758158831788265 ) ) ;
#30249 = CARTESIAN_POINT ( 'NONE',  ( 3.716130297413534844, -2.273962828982917017, 0.3916390033968617512 ) ) ;
#30250 = CARTESIAN_POINT ( 'NONE',  ( 5.641890011675567251, 0.8391073529228080252, -1.882412581722334943 ) ) ;
#30251 = CARTESIAN_POINT ( 'NONE',  ( 1.499837725185527049, -0.6986378101729547874, -1.812093905146118233 ) ) ;
#30252 = CARTESIAN_POINT ( 'NONE',  ( -5.205967797523171292, 9.017453497178271604, 0.000000000000000000 ) ) ;
#30253 = CARTESIAN_POINT ( 'NONE',  ( -4.787964524281469458, 5.614988695530339413, -1.199719254218453823 ) ) ;
#30254 = CARTESIAN_POINT ( 'NONE',  ( -9.437721056244807727, 14.51368701454513221, 7.411487925289132583 ) ) ;
#30255 = CARTESIAN_POINT ( 'NONE',  ( 4.166350089634453191, 2.120059694336435374, -0.05518752902338577848 ) ) ;
#30256 = CARTESIAN_POINT ( 'NONE',  ( 2.303361484738715159, 1.314996338066702242, -1.528741580717301263 ) ) ;
#30257 = CARTESIAN_POINT ( 'NONE',  ( -6.358410854684796831, 6.520493539994793863, -0.7216878364870267237 ) ) ;
#30258 = CARTESIAN_POINT ( 'NONE',  ( 3.979664642534729513, 2.078844338038158934, -0.7408291028327750327 ) ) ;
#30259 = DIRECTION ( 'NONE',  ( 0.000000000000000000, -1.000000000000000000, 0.000000000000000000 ) ) ;
#30260 = CARTESIAN_POINT ( 'NONE',  ( -1.840780836846555912, -3.118471481109373666, -2.864343303366730265 ) ) ;
#30261 = CARTESIAN_POINT ( 'NONE',  ( 11.94105721237523277, 12.69999999999999929, -1.187919463087249827 ) ) ;
#30262 = CARTESIAN_POINT ( 'NONE',  ( -5.725286006720766707, 9.901527117808042178, 0.7998128361456291469 ) ) ;
#30264 = CARTESIAN_POINT ( 'NONE',  ( 6.825078400183518745, 0.5555073798480349989, 2.295529415773037929 ) ) ;
#30263 = CARTESIAN_POINT ( 'NONE',  ( -4.592595068035599581, 8.488991103336598343, 0.1827531742817755656 ) ) ;
#30265 = CARTESIAN_POINT ( 'NONE',  ( -5.233772384569284064, 7.755300245267345183, 1.265081041508690607 ) ) ;
#30266 = EDGE_LOOP ( 'NONE', ( #107547, #15169, #204639, #135350 ) ) ;
#30267 = CARTESIAN_POINT ( 'NONE',  ( 4.065347389730957772, 0.2539501645208458447, -2.045120066754711363 ) ) ;
#30268 = CARTESIAN_POINT ( 'NONE',  ( -1.360316468750006225, 2.640625000341401130, 3.469446951953614189E-15 ) ) ;
#30269 = CARTESIAN_POINT ( 'NONE',  ( 0.1796516426514959408, -8.073984524010706210, 9.498564853506346495 ) ) ;
#30270 = CARTESIAN_POINT ( 'NONE',  ( -4.660252114795309097, 6.460046772059735432, -1.599625672291256295 ) ) ;
#30272 = CARTESIAN_POINT ( 'NONE',  ( -3.644109427023046521, 7.473487774827342278, 0.000000000000000000 ) ) ;
#30271 = B_SPLINE_CURVE_WITH_KNOTS ( 'NONE', 3,
 ( #130584, #87079, #3660, #153149, #35115, #2602 ),
 .UNSPECIFIED., .F., .F.,
 ( 4, 2, 4 ),
 ( 0.000000000000000000, 0.0003157158648874029564, 0.0006314317297748059127 ),
 .UNSPECIFIED. ) ;
#30273 = CARTESIAN_POINT ( 'NONE',  ( 3.897132395768299951, -0.2000006916238558641, -2.009757592718981911 ) ) ;
#30274 = CARTESIAN_POINT ( 'NONE',  ( 0.7499999999999867883, 0.3166666666666873020, -1.299038105676652899 ) ) ;
#30276 = CARTESIAN_POINT ( 'NONE',  ( 2.683624340501134853, 5.218313266304903664, -1.199719254218446718 ) ) ;
#30275 = CARTESIAN_POINT ( 'NONE',  ( -5.503684012504701961, 5.385662534202396934, 0.000000000000000000 ) ) ;
#30277 = CARTESIAN_POINT ( 'NONE',  ( 7.470706336329915764, 8.674577799595093452, -1.199719254218441611 ) ) ;
#30278 = CARTESIAN_POINT ( 'NONE',  ( 2.834896919975951057, 0.2507222237850720847, 2.045500233692464587 ) ) ;
#30279 = CARTESIAN_POINT ( 'NONE',  ( 2.514296259408643319, -1.880434619097739013, 0.7283795345095490648 ) ) ;
#30280 = SPHERICAL_SURFACE ( 'NONE', #176783, 0.08000000000000000167 ) ;
#30281 = CARTESIAN_POINT ( 'NONE',  ( 5.301401758143367893, 6.143722458377430584, 1.199719254218462483 ) ) ;
#30282 = CIRCLE ( 'NONE', #161868, 0.07999999999999907185 ) ;
#30283 =( BOUNDED_CURVE ( )  B_SPLINE_CURVE ( 2, ( #63454, #62381, #33083, #179350, #97047, #131695, #115462, #98107, #144749, #128545, #165211, #212886, #82885, #64517, #130662, #48292, #148962, #114404, #164159, #534, #66601, #193454, #154298, #132747, #83947, #200877, #169472, #168409, #150038, #166272, #135916, #20006, #134870, #86090, #52522, #100206, #17864, #38408, #133812, #152166, #3735, #2676, #118654, #85021, #184640, #103411, #201934, #21057, #153225, #36258, #186782, #136988, #183582, #53591, #1609, #69810, #35189, #199826, #104490, #119725, #50397, #182507, #185704, #102337, #37338, #87154, #51467, #68748, #198750, #4795, #70874, #101265, #67668, #203015, #167349, #54657, #120805, #117591, #18936, #170533, #151110, #22118, #88230, #5873, #116517, #34137, #93590, #108817, #109886, #192109, #122962, #175899, #172690, #27490, #73025, #158570, #25352, #41637, #39472, #56793, #139123, #107751, #40559, #207305, #205150, #106665, #188921, #23196, #71946, #90373, #174841, #89312, #24268, #156442, #8026, #74116, #59993, #26418, #10169, #55721, #173777 ),
 .UNSPECIFIED., .F., .T. ) 
 B_SPLINE_CURVE_WITH_KNOTS ( ( 3, 2, 2, 2, 2, 2, 2, 2, 2, 2, 2, 2, 2, 2, 2, 2, 2, 2, 2, 2, 2, 2, 2, 2, 2, 2, 2, 2, 2, 2, 2, 2, 2, 2, 2, 2, 2, 2, 2, 2, 2, 2, 2, 2, 2, 2, 2, 2, 2, 2, 2, 2, 2, 2, 2, 2, 2, 2, 2, 2, 3 ),
 ( 0.000000000000000000, 0.005952380952380951183, 0.01190476190476190237, 0.01785714285714285615, 0.02380952380952380473, 0.02976190476190476025, 0.03571428571428571230, 0.04166666666666666435, 0.04761904761904760947, 0.05357142857142856845, 0.05952380952380952051, 0.06547619047619047949, 0.07142857142857142461, 0.07738095238095238360, 0.08333333333333332871, 0.08928571428571428770, 0.09523809523809521893, 0.1011904761904762057, 0.1071428571428571369, 0.1130952380952380959, 0.1190476190476190410, 0.1250000000000000000, 0.1309523809523809590, 0.1369047619047619180, 0.1428571428571428492, 0.1488095238095238082, 0.1547619047619047672, 0.1607142857142857262, 0.1666666666666666574, 0.1726190476190476164, 0.1785714285714285754, 0.1845238095238095621, 0.1904761904761904379, 0.1964285714285714246, 0.2023809523809524114, 0.2083333333333333426, 0.2142857142857142738, 0.2202380952380952328, 0.2261904761904761918, 0.2321428571428571508, 0.2380952380952380820, 0.2440476190476190133, 0.2500000000000000000, 0.2559523809523809312, 0.2619047619047619180, 0.2678571428571428492, 0.2738095238095238360, 0.2797619047619047672, 0.2857142857142856984, 0.2916666666666666852, 0.2976190476190476164, 0.3035714285714285476, 0.3095238095238095344, 0.3154761904761904656, 0.3214285714285714524, 0.3273809523809523836, 0.3333333333333333148, 0.3392857142857143016, 0.3452380952380952328, 0.3511904761904761640, 0.3537201901891439126 ),
 .UNSPECIFIED. ) 
 CURVE ( )  GEOMETRIC_REPRESENTATION_ITEM ( )  RATIONAL_B_SPLINE_CURVE ( ( 1.000000000000000000, 0.8660254037844387076, 1.000000000000000000, 0.8660254037844387076, 1.000000000000000000, 0.8660254037844387076, 1.000000000000000000, 0.8660254037844387076, 1.000000000000000000, 0.8660254037844387076, 1.000000000000000000, 0.8660254037844387076, 1.000000000000000000, 0.8660254037844387076, 1.000000000000000000, 0.8660254037844387076, 1.000000000000000000, 0.8660254037844387076, 1.000000000000000000, 0.8660254037844387076, 1.000000000000000000, 0.8660254037844387076, 1.000000000000000000, 0.8660254037844387076, 1.000000000000000000, 0.8660254037844387076, 1.000000000000000000, 0.8660254037844387076, 1.000000000000000000, 0.8660254037844387076, 1.000000000000000000, 0.8660254037844387076, 1.000000000000000000, 0.8660254037844387076, 1.000000000000000000, 0.8660254037844387076, 1.000000000000000000, 0.8660254037844387076, 1.000000000000000000, 0.8660254037844387076, 1.000000000000000000, 0.8660254037844387076, 1.000000000000000000, 0.8660254037844387076, 1.000000000000000000, 0.8660254037844387076, 1.000000000000000000, 0.8660254037844387076, 1.000000000000000000, 0.8660254037844387076, 1.000000000000000000, 0.8660254037844387076, 1.000000000000000000, 0.8660254037844387076, 1.000000000000000000, 0.8660254037844387076, 1.000000000000000000, 0.8660254037844387076, 1.000000000000000000, 0.8660254037844387076, 1.000000000000000000, 0.8660254037844387076, 1.000000000000000000, 0.8660254037844387076, 1.000000000000000000, 0.8660254037844387076, 1.000000000000000000, 0.8660254037844387076, 1.000000000000000000, 0.8660254037844387076, 1.000000000000000000, 0.8660254037844387076, 1.000000000000000000, 0.8660254037844387076, 1.000000000000000000, 0.8660254037844387076, 1.000000000000000000, 0.8660254037844387076, 1.000000000000000000, 0.8660254037844387076, 1.000000000000000000, 0.8660254037844387076, 1.000000000000000000, 0.8660254037844387076, 1.000000000000000000, 0.8660254037844387076, 1.000000000000000000, 0.8660254037844387076, 1.000000000000000000, 0.8660254037844387076, 1.000000000000000000, 0.8660254037844387076, 1.000000000000000000, 0.8660254037844387076, 1.000000000000000000, 0.8660254037844387076, 1.000000000000000000, 0.8660254037844387076, 1.000000000000000000, 0.8660254037844387076, 1.000000000000000000, 0.8660254037844387076, 1.000000000000000000, 0.8660254037844387076, 1.000000000000000000, 0.8660254037844387076, 1.000000000000000000, 0.8660254037844387076, 1.000000000000000000, 0.8660254037844387076, 1.000000000000000000, 0.8660254037844387076, 1.000000000000000000, 0.8660254037844387076, 1.000000000000000000, 0.8660254037844387076, 1.000000000000000000, 0.8660254037844387076, 1.000000000000000000, 0.9430618748659230777, 0.9345202395942615592 ) ) 
 REPRESENTATION_ITEM ( '' )  );
#30285 = ORIENTED_EDGE ( 'NONE', *, *, #63218, .F. ) ;
#30284 = CARTESIAN_POINT ( 'NONE',  ( -0.5029403714634873568, 7.727853499550840333, -1.993913793680506696 ) ) ;
#30286 = CARTESIAN_POINT ( 'NONE',  ( 1.253568445147245525, 0.7445567558202557112, 1.684058134371092752 ) ) ;
#30287 = CARTESIAN_POINT ( 'NONE',  ( 6.727182134110200273, -0.004969159814478123736, 2.189081792362323586 ) ) ;
#30288 = CARTESIAN_POINT ( 'NONE',  ( 4.224247379109608680, 7.085983154673295203, -1.199719254218452047 ) ) ;
#30289 = CARTESIAN_POINT ( 'NONE',  ( 3.128364550451453230, 1.203671540783244565, -1.795256801906938815 ) ) ;
#30290 = CARTESIAN_POINT ( 'NONE',  ( -2.467220768007014176, 5.822248629409386922, 0.7216878364870317197 ) ) ;
#30291 = CARTESIAN_POINT ( 'NONE',  ( 4.294233728257051297, -0.9087460953031538669, -1.912572187454407047 ) ) ;
#30292 = VECTOR ( 'NONE', #183455, 1000.000000000000000 ) ;
#30293 = CARTESIAN_POINT ( 'NONE',  ( 11.07790593930098311, 12.30000000000000071, -0.7000000000000009548 ) ) ;
#30294 = CARTESIAN_POINT ( 'NONE',  ( 0.6724591444495706671, -1.759989063064151038, -0.6342292696241008665 ) ) ;
#30295 = CARTESIAN_POINT ( 'NONE',  ( 4.944191625186433292, 1.966121618969366214, 0.1460544362237597982 ) ) ;
#30296 = CARTESIAN_POINT ( 'NONE',  ( 4.645720405014278853, 1.993893748393640086, -0.3006458143828410479 ) ) ;
#30298 = CARTESIAN_POINT ( 'NONE',  ( 10.03267048398825168, 10.80712977418221676, 0.000000000000000000 ) ) ;
#30297 = CARTESIAN_POINT ( 'NONE',  ( -0.6823417656249969321, 3.467708333674754506, -1.181850606188749264 ) ) ;
#30300 = CARTESIAN_POINT ( 'NONE',  ( 6.656868561830338038, -1.629224735911166233, 1.334343933791133141 ) ) ;
#30299 = CARTESIAN_POINT ( 'NONE',  ( -6.307567778855718288, 8.381915046796901692, -1.599625672291263179 ) ) ;
#30301 = CARTESIAN_POINT ( 'NONE',  ( 6.742638474511262636, -2.029596885996234334, -0.4079607620106340260 ) ) ;
#30302 = CARTESIAN_POINT ( 'NONE',  ( 6.331821432781979730, 7.345878745455822312, -1.199719254218445830 ) ) ;
#30303 = CARTESIAN_POINT ( 'NONE',  ( -7.063961727919978451, 8.200042423116789436, 1.199719254218450271 ) ) ;
#30304 = AXIS2_PLACEMENT_3D ( 'NONE', #74433, #39797, #121132 ) ;
#30305 = CARTESIAN_POINT ( 'NONE',  ( 6.639320575229291421, 7.052573552169272730, 2.601414154538615353 ) ) ;
#30306 = CARTESIAN_POINT ( 'NONE',  ( 4.698096894549816049, -1.971010956759836397, -0.04940921540304286930 ) ) ;
#30307 = CARTESIAN_POINT ( 'NONE',  ( 5.959241620951676310, -1.704104911329520800, 1.083944116985413819 ) ) ;
#30308 = CARTESIAN_POINT ( 'NONE',  ( 0.7499999999999867883, -0.1520833326505155458, -1.299038105676652899 ) ) ;
#30309 = CARTESIAN_POINT ( 'NONE',  ( 4.670747285963097184, -1.509779504925019999, 1.745381082733918676 ) ) ;
#30310 = CARTESIAN_POINT ( 'NONE',  ( 2.254800304804779110, -0.5458148477457210879, -1.989007103235032048 ) ) ;
#30311 = CARTESIAN_POINT ( 'NONE',  ( 8.595506201384020883, 9.130438111143927671, 0.7216878364870438212 ) ) ;
#30312 = EDGE_CURVE ( 'NONE', #172003, #121557, #94429, .T. ) ;
#30313 = CARTESIAN_POINT ( 'NONE',  ( 6.703580607314123085, 6.785541894813420072, 0.000000000000000000 ) ) ;
#30314 = CARTESIAN_POINT ( 'NONE',  ( 3.725458348705031231, 7.568394850123006279, -1.734723475976807094E-15 ) ) ;
#30315 = CARTESIAN_POINT ( 'NONE',  ( -1.402160292154681736E-14, 1.759375000341421469, -1.575800808251659024 ) ) ;
#30316 = CARTESIAN_POINT ( 'NONE',  ( 4.913904330310220558, 4.697586238308844919, 0.000000000000000000 ) ) ;
#30317 = CARTESIAN_POINT ( 'NONE',  ( 6.439759776366769550, 8.536139043893143707, 1.443375672974076540 ) ) ;
#30318 = CARTESIAN_POINT ( 'NONE',  ( 3.912682095371947444, 0.7780703539225676257, 2.027152283489948026 ) ) ;
#30319 = CARTESIAN_POINT ( 'NONE',  ( -3.256827568602408185, 6.415910372102921144, -0.7556650801423603347 ) ) ;
#30321 = CARTESIAN_POINT ( 'NONE',  ( 3.913478945735289205, -0.9499487412085620974, -1.577145280185827447 ) ) ;
#30320 = CARTESIAN_POINT ( 'NONE',  ( -4.622967192579922724, 4.495809267539077503, 1.214306433183764966E-14 ) ) ;
#30323 = CARTESIAN_POINT ( 'NONE',  ( 6.720655732516701342, 6.039000170257122768, 2.421169367564251385 ) ) ;
#30322 = CARTESIAN_POINT ( 'NONE',  ( -1.364683531250012516, 4.238541667008090208, -0.7879004041258300672 ) ) ;
#30325 = CARTESIAN_POINT ( 'NONE',  ( 5.706613541269077494, 1.932210019790636224, 1.034112652976440394 ) ) ;
#30324 = B_SPLINE_CURVE_WITH_KNOTS ( 'NONE', 3,
 ( #47517, #194802, #30176, #96266, #214206, #146087, #212099, #64798, #130942, #196935 ),
 .UNSPECIFIED., .F., .F.,
 ( 4, 3, 3, 4 ),
 ( 4.424023162370599995E-18, 3.125149536070166581E-05, 5.486596421586658484E-05, 7.848575944736516173E-05 ),
 .UNSPECIFIED. ) ;
#30326 = CARTESIAN_POINT ( 'NONE',  ( 0.4106005709051863128, 3.230891568747374265, 1.957863677979522654 ) ) ;
#30327 = CARTESIAN_POINT ( 'NONE',  ( 5.875896723904014962, 1.342229061679913071, 1.821250878268846352 ) ) ;
#30328 = ORIENTED_EDGE ( 'NONE', *, *, #162643, .T. ) ;
#30329 = CARTESIAN_POINT ( 'NONE',  ( -5.409091473909686698, 6.481950958801420803, -1.333638828535830045 ) ) ;
#30330 = CARTESIAN_POINT ( 'NONE',  ( 4.802592184731321545, 8.245026257381830703, 0.8702854636597904259 ) ) ;
#30331 = CARTESIAN_POINT ( 'NONE',  ( -5.817857313595549584, 6.920493299683823096, 1.082531754730549078 ) ) ;
#30332 = CARTESIAN_POINT ( 'NONE',  ( -7.235142258280603755, -6.594478602024295810, -7.235142258280561123 ) ) ;
#30333 = CARTESIAN_POINT ( 'NONE',  ( 0.4437791967034719343, 1.764639887404760188, 0.1366099650685937694 ) ) ;
#30334 = CARTESIAN_POINT ( 'NONE',  ( 4.248693477488805215, 1.974695210492120045, 0.3904942472512766827 ) ) ;
#30335 = CARTESIAN_POINT ( 'NONE',  ( 5.282873410819217241, 9.315102745931094219, -0.7998128361456281477 ) ) ;
#30336 = CARTESIAN_POINT ( 'NONE',  ( 2.960101939890079858, 2.095960298449873971, -0.2048252169620876917 ) ) ;
#30337 = CARTESIAN_POINT ( 'NONE',  ( 1.581495747622517323, -0.6437907056052544208, 1.804334155150161267 ) ) ;
#30338 = CARTESIAN_POINT ( 'NONE',  ( 3.011882680530176604, 6.665613560593854459, 0.7998128361456341429 ) ) ;
#30339 = CARTESIAN_POINT ( 'NONE',  ( 3.016014308207531247, 1.960325316701009735, -0.1901906172739661061 ) ) ;
#30340 = CARTESIAN_POINT ( 'NONE',  ( 6.082287225941254150, 1.041776932085249907, 1.730260143339139134 ) ) ;
#30341 = CARTESIAN_POINT ( 'NONE',  ( 1.867826558377215118, 0.9591755677602131769, 1.605880698980370225 ) ) ;
#30342 = CARTESIAN_POINT ( 'NONE',  ( 1.732786548908150870, -1.861864252656076912, -0.6185235971247133868 ) ) ;
#30345 = VERTEX_POINT ( 'NONE', #152419 ) ;
#30344 = CARTESIAN_POINT ( 'NONE',  ( 1.652457426684301955, 1.892030339952909035, 0.2773405859870237133 ) ) ;
#30343 = CARTESIAN_POINT ( 'NONE',  ( 3.808989599770518097, 1.480563749658039052, 0.8846867361136273589 ) ) ;
#30347 = CARTESIAN_POINT ( 'NONE',  ( 5.856759171423504107, 5.935233242856626568, -0.7216878364870257245 ) ) ;
#30346 = CARTESIAN_POINT ( 'NONE',  ( 1.137671262558290763, -1.993743905544292927, 0.9465009238469668240 ) ) ;
#30348 = CARTESIAN_POINT ( 'NONE',  ( 0.6823417656249899377, 2.405208333674753618, 1.181850606188767472 ) ) ;
#30349 = CARTESIAN_POINT ( 'NONE',  ( 9.562578416340237197, 10.05076299535211781, 0.7998128361456462443 ) ) ;
#30350 = CARTESIAN_POINT ( 'NONE',  ( 11.55950211276791251, 12.30000000000000071, -3.221476510067115662 ) ) ;
#30351 = CARTESIAN_POINT ( 'NONE',  ( -8.832353407160665526, 3.956598013261175772, -7.432338980325321920 ) ) ;
#30352 = CARTESIAN_POINT ( 'NONE',  ( -3.904308432943693230, 7.706776938409620747, -0.6575030929269864988 ) ) ;
#30353 = DIRECTION ( 'NONE',  ( -0.000000000000000000, -1.000000000000000000, -0.000000000000000000 ) ) ;
#30354 = CARTESIAN_POINT ( 'NONE',  ( 1.029834584532058672, 1.995790600324919506, -0.5504719462680053299 ) ) ;
#30355 = CARTESIAN_POINT ( 'NONE',  ( 1.499999999999987121, 2.045833333333356929, -0.8660254037844262731 ) ) ;
#30356 = CARTESIAN_POINT ( 'NONE',  ( 5.764187864104357573, 9.876636274763768597, 1.040834085586084257E-14 ) ) ;
#30357 = CARTESIAN_POINT ( 'NONE',  ( -9.027031348600448979, 9.425958082989001952, 1.040834085586084257E-14 ) ) ;
#30358 = CARTESIAN_POINT ( 'NONE',  ( 4.960304097753311936, 6.880383762169266504, 1.599625672291268286 ) ) ;
#30359 = CARTESIAN_POINT ( 'NONE',  ( 5.953796468794862129, -1.535729488331440074, -1.462440914314271811 ) ) ;
#30360 = CARTESIAN_POINT ( 'NONE',  ( 3.923105346307896202, 5.670318552149568703, -1.599625672291269396 ) ) ;
#30361 = EDGE_CURVE ( 'NONE', #11347, #185972, #49413, .T. ) ;
#30362 = CARTESIAN_POINT ( 'NONE',  ( 0.6823417656249899377, 2.842708333674753618, 1.181850606188765695 ) ) ;
#30363 = CARTESIAN_POINT ( 'NONE',  ( -1.500000000000013101, 4.129166666666687746, -0.8660254037844313801 ) ) ;
#30365 = CARTESIAN_POINT ( 'NONE',  ( 2.686486993802192913, 6.285985259411197568, 0.7998128361456362523 ) ) ;
#30364 = CARTESIAN_POINT ( 'NONE',  ( 5.670351692713981429, -0.8806477319739226539, -1.753155087565357428 ) ) ;
#30366 = CARTESIAN_POINT ( 'NONE',  ( 4.692732413458527319, -1.238132498367883860, -1.591073831703953445 ) ) ;
#30367 = CARTESIAN_POINT ( 'NONE',  ( 3.837047941109549054, -1.595840754823075303, -1.059516945425369450 ) ) ;
#30368 = DIRECTION ( 'NONE',  ( 0.7592566023653005702, 0.6507913734559639396, 0.000000000000000000 ) ) ;
#30369 = CARTESIAN_POINT ( 'NONE',  ( 1.329895901633147748, 1.076045675571284166, -1.909117696414885934 ) ) ;
#30370 = CARTESIAN_POINT ( 'NONE',  ( 0.1335669894368500255, -0.0009366757763962055587, -2.153671288142432250 ) ) ;
#30371 = CARTESIAN_POINT ( 'NONE',  ( -0.7500000000000006661, 1.139583334016154526, -1.299038105676652011 ) ) ;
#30372 = CARTESIAN_POINT ( 'NONE',  ( 5.467046525086633579, -1.584481552701553220, 1.241800460852604759 ) ) ;
#30373 = CARTESIAN_POINT ( 'NONE',  ( -6.856673000209188906, 9.022537805042615489, 1.599625672291283607 ) ) ;
#30374 = ADVANCED_FACE ( 'NONE', ( #3998 ), #121070, .F. ) ;
#30376 = CARTESIAN_POINT ( 'NONE',  ( 5.642236307234618664, 0.8587400236706268508, 1.935442681345787452 ) ) ;
#30375 = CARTESIAN_POINT ( 'NONE',  ( -3.633221978782290140, 6.222214161012547429, -1.082531754730549967 ) ) ;
#30377 = CARTESIAN_POINT ( 'NONE',  ( -1.364683531250000748, 8.671875000341403350, 0.000000000000000000 ) ) ;
#30379 = CARTESIAN_POINT ( 'NONE',  ( -6.071018923869249129, 10.30488218781460574, 0.7998128361456291469 ) ) ;
#30378 = CARTESIAN_POINT ( 'NONE',  ( 2.085595224044423102, -0.8910886986466991511, 1.891471387866516585 ) ) ;
#30381 = ORIENTED_EDGE ( 'NONE', *, *, #19259, .F. ) ;
#30380 = CARTESIAN_POINT ( 'NONE',  ( 1.623609269016149437, -0.9540678014761799774, -1.436642212298586907 ) ) ;
#30382 = CARTESIAN_POINT ( 'NONE',  ( 7.311924916471702396, 7.425000578838787391, -0.7998128361456281477 ) ) ;
#30383 = CARTESIAN_POINT ( 'NONE',  ( -1.397780926668899415, 13.25520333592606015, 0.5144292668303754867 ) ) ;
#30384 = CARTESIAN_POINT ( 'NONE',  ( 1.734723475976807094E-15, 15.00041888085534758, 12.17999951260719982 ) ) ;
#30385 = DIRECTION ( 'NONE',  ( -0.000000000000000000, -1.000000000000000000, -0.000000000000000000 ) ) ;
#30387 = CARTESIAN_POINT ( 'NONE',  ( 8.934460041281305109, 10.48625347199211966, -1.082531754730543083 ) ) ;
#30386 = CARTESIAN_POINT ( 'NONE',  ( 6.012151052656117933, 9.101594430485762999, 1.199719254218460707 ) ) ;
#30388 = ORIENTED_EDGE ( 'NONE', *, *, #91128, .F. ) ;
#30389 = CARTESIAN_POINT ( 'NONE',  ( 1.500000000000065503, 6.071532165918824830E-15, -10.99818166789400919 ) ) ;
#30391 = CARTESIAN_POINT ( 'NONE',  ( 2.103910407274149907, -0.7736040573625382333, 1.638098421638082947 ) ) ;
#30390 = CARTESIAN_POINT ( 'NONE',  ( 6.367489420273535039, 7.457767740854454708, -1.199719254218452047 ) ) ;
#30392 = CARTESIAN_POINT ( 'NONE',  ( -7.691553217654356622, 7.867900263551875994, -0.7998128361456291469 ) ) ;
#30394 = ORIENTED_EDGE ( 'NONE', *, *, #144483, .T. ) ;
#30393 = VECTOR ( 'NONE', #7755, 1000.000000000000000 ) ;
#30395 = CARTESIAN_POINT ( 'NONE',  ( 4.552840656090682891, 4.206068941727564514, 1.214306433183764966E-14 ) ) ;
#30396 = ORIENTED_EDGE ( 'NONE', *, *, #34941, .T. ) ;
#30397 = CARTESIAN_POINT ( 'NONE',  ( 6.170896192875352959, 7.228408975556602556, 1.199719254218453823 ) ) ;
#30398 = CARTESIAN_POINT ( 'NONE',  ( 2.244508708441519840, 1.757319924227723762, 0.4390839574351864671 ) ) ;
#30399 = CARTESIAN_POINT ( 'NONE',  ( 6.639320575229291421, 7.053415594291638335, 2.394893074302415936 ) ) ;
#30400 = CARTESIAN_POINT ( 'NONE',  ( 0.7500000000000006661, 9.083333333333332149, 1.299038105676657340 ) ) ;
#30401 = CARTESIAN_POINT ( 'NONE',  ( 4.307253300151457687, 7.213791655154011551, 0.9935852123437900474 ) ) ;
#30402 = CARTESIAN_POINT ( 'NONE',  ( 2.980726927023560346, 1.751358449955683350, 0.6298351686941299210 ) ) ;
#30403 = CARTESIAN_POINT ( 'NONE',  ( 0.4916157762205043413, -1.906313760269543911, 0.1885876022650559980 ) ) ;
#30404 = CARTESIAN_POINT ( 'NONE',  ( 0.3229203692996869823, -0.09522068211164493035, 1.823229820405058099 ) ) ;
#30405 = CARTESIAN_POINT ( 'NONE',  ( 1.378728738066221871, 4.086408449757453099, -0.5908528300941785494 ) ) ;
#30406 = EDGE_CURVE ( 'NONE', #79641, #131991, #208613, .T. ) ;
#30408 = AXIS2_PLACEMENT_3D ( 'NONE', #81106, #94187, #64849 ) ;
#30407 = CIRCLE ( 'NONE', #54513, 1.872309607372811158 ) ;
#30409 = CARTESIAN_POINT ( 'NONE',  ( 4.746850994788568201, 8.189453717816405742, 0.7312505120831546135 ) ) ;
#30410 = SURFACE_STYLE_USAGE ( .BOTH. , #179850 ) ;
#30411 = CARTESIAN_POINT ( 'NONE',  ( -2.657034918598345730, 5.083329257464595408, -1.082531754730543971 ) ) ;
#30412 = CARTESIAN_POINT ( 'NONE',  ( 6.466876084038451822, 10.48851316477946582, 1.040834085586084257E-14 ) ) ;
#30413 = CARTESIAN_POINT ( 'NONE',  ( 4.276189508915988036, -1.008629908464111269, -1.691384299763159182 ) ) ;
#30414 = CARTESIAN_POINT ( 'NONE',  ( -3.795392936821753604, 6.515376628678959392, -1.199719254218452047 ) ) ;
#30415 = CARTESIAN_POINT ( 'NONE',  ( -11.88237264505823987, 9.843229615316904102, -0.9087825512663008087 ) ) ;
#30416 = CARTESIAN_POINT ( 'NONE',  ( 6.632779825423476439, -1.959453823303359377, 0.9815127000676395763 ) ) ;
#30417 = CARTESIAN_POINT ( 'NONE',  ( 5.860362583224701716, 0.7811062513497173398, 1.761092865462327239 ) ) ;
#30418 = CARTESIAN_POINT ( 'NONE',  ( -6.880926654135487652, 7.986501503701545879, 1.199719254218450271 ) ) ;
#30419 = CARTESIAN_POINT ( 'NONE',  ( -0.2409995289980038091, -0.004801160710915519658, -2.000252362011435636 ) ) ;
#30420 = CARTESIAN_POINT ( 'NONE',  ( 2.473496279428960776, 0.1070396533628548558, -2.204406164007084445 ) ) ;
#30421 = CARTESIAN_POINT ( 'NONE',  ( -6.137446956630687289, 6.999240388318681561, 0.9466904651086446298 ) ) ;
#30422 = CARTESIAN_POINT ( 'NONE',  ( -0.1933232215488022709, -0.4202133615931051835, -1.872389726556406897 ) ) ;
#30423 = ORIENTED_EDGE ( 'NONE', *, *, #140820, .T. ) ;
#30424 = ORIENTED_EDGE ( 'NONE', *, *, #16302, .F. ) ;
#30425 = CARTESIAN_POINT ( 'NONE',  ( 0.6077773097897182231, 0.6213696771984353884, -1.869019927991413921 ) ) ;
#30426 = CARTESIAN_POINT ( 'NONE',  ( 1.153739077726954498, 0.7885942357991974072, 1.774928408438203098 ) ) ;
#30427 = CARTESIAN_POINT ( 'NONE',  ( 1.229842044428463010, -1.821462008879136896, -0.8645945014377558469 ) ) ;
#30429 = CARTESIAN_POINT ( 'NONE',  ( 4.979284885303652430, -0.09383206328643842187, 1.858730327737258436 ) ) ;
#30428 = CARTESIAN_POINT ( 'NONE',  ( -4.685224601974262271, 7.623789914682047808, -1.199719254218453823 ) ) ;
#30430 = CARTESIAN_POINT ( 'NONE',  ( 6.547661840756936691, 6.603636667163397256, 0.7998128361456352531 ) ) ;
#30431 = CARTESIAN_POINT ( 'NONE',  ( -3.599035817516879288, 3.565494897539134733, 2.500000000000000444 ) ) ;
#30432 = CARTESIAN_POINT ( 'NONE',  ( 9.579665964935223599, -7.246166700194470067, 5.204170427930421283E-15 ) ) ;
#30433 = CARTESIAN_POINT ( 'NONE',  ( -4.232116505760120440, 8.089219690028791376, -0.7998128361456281477 ) ) ;
#30434 = CARTESIAN_POINT ( 'NONE',  ( -7.425025402139490360, 8.691559719698066289, 1.199719254218452047 ) ) ;
#30435 = CARTESIAN_POINT ( 'NONE',  ( 1.769323484426460480, 2.095969018468134770, -0.6401429536977767398 ) ) ;
#30436 = CARTESIAN_POINT ( 'NONE',  ( 3.009546912553647147, 5.494593250412460606, -1.082531754730543083 ) ) ;
#30437 = ORIENTED_EDGE ( 'NONE', *, *, #63361, .F. ) ;
#30438 = CARTESIAN_POINT ( 'NONE',  ( 10.87712779691733544, -6.655928102867018303, -0.1480828224388737735 ) ) ;
#30439 = DIRECTION ( 'NONE',  ( -0.7592566023653004592, -0.6507913734559639396, 0.000000000000000000 ) ) ;
#30440 = CARTESIAN_POINT ( 'NONE',  ( 1.945663734523142230, 0.6997465788082489757, -1.686465609443507763 ) ) ;
#30441 = CARTESIAN_POINT ( 'NONE',  ( -4.135400547368138113, 4.783387712472935149, 1.199719254218462483 ) ) ;
#30442 = VECTOR ( 'NONE', #203391, 1000.000000000000000 ) ;
#30443 = CARTESIAN_POINT ( 'NONE',  ( -6.238615401616060652, 7.011456692927672485, -1.010807710288418981 ) ) ;
#30444 = CARTESIAN_POINT ( 'NONE',  ( 6.609000000000047947, 3.700659725723095761, 2.414405743007182359 ) ) ;
#30445 = CARTESIAN_POINT ( 'NONE',  ( 8.218213668177886788, 12.73966637951625813, 0.7998128361456462443 ) ) ;
#30446 = CARTESIAN_POINT ( 'NONE',  ( 0.6449897232218603227, -1.652859335204670543, 0.9894661712252955654 ) ) ;
#30447 = CARTESIAN_POINT ( 'NONE',  ( 4.223457129239616137, 0.2443821477370981265, -1.946437379933690481 ) ) ;
#30448 = VECTOR ( 'NONE', #196087, 1000.000000000000000 ) ;
#30449 = CARTESIAN_POINT ( 'NONE',  ( -7.503547950159405566, 10.84155747757291266, 1.199719254218453823 ) ) ;
#30450 = CARTESIAN_POINT ( 'NONE',  ( 4.299907273828439180, 8.168308919441841454, 1.040834085586084257E-14 ) ) ;
#30451 = CARTESIAN_POINT ( 'NONE',  ( 4.933237592207079025, -1.549687834843778811, -1.549900206446311657 ) ) ;
#30452 = CARTESIAN_POINT ( 'NONE',  ( 6.609000000000038177, 0.002801690667396730672, 2.000160786441218530 ) ) ;
#30453 = CARTESIAN_POINT ( 'NONE',  ( 4.135645376760338721, 1.951069878921590783, -0.6927527371542248069 ) ) ;
#30454 = CARTESIAN_POINT ( 'NONE',  ( -1.364683531250012516, 1.592708333674756727, 0.7879004041258379498 ) ) ;
#30455 = ORIENTED_EDGE ( 'NONE', *, *, #126255, .T. ) ;
#30456 = CARTESIAN_POINT ( 'NONE',  ( 4.307493173298723832, 1.414159744579394307, -1.812179591053430627 ) ) ;
#30458 = VERTEX_POINT ( 'NONE', #73281 ) ;
#30457 = CARTESIAN_POINT ( 'NONE',  ( 8.622622508611357262, 9.162073802909148412, -0.7216878364870197293 ) ) ;
#30460 = CARTESIAN_POINT ( 'NONE',  ( -1.642778471874998480, -1.101041666188708801, 2.845375778867863303 ) ) ;
#30459 = CARTESIAN_POINT ( 'NONE',  ( 5.722950238744200391, 7.770137593325314285, 1.443375672974065660 ) ) ;
#30461 = CARTESIAN_POINT ( 'NONE',  ( -7.717216217110848042, -5.600320323339640360, -7.761717428875279268 ) ) ;
#30462 = CARTESIAN_POINT ( 'NONE',  ( -10.06346916285073334, 4.651885711879500285, -6.538199818904806726 ) ) ;
#30463 = CARTESIAN_POINT ( 'NONE',  ( 4.224509699451983735, 0.09670237001900212903, 1.939662488567380993 ) ) ;
#30464 = ORIENTED_EDGE ( 'NONE', *, *, #173168, .F. ) ;
#30465 = CARTESIAN_POINT ( 'NONE',  ( -5.398914348987532641, 6.259949555863199677, -2.500000000000000444 ) ) ;
#30466 = CARTESIAN_POINT ( 'NONE',  ( 5.572493885891085519, 0.7809320506734825917, 1.745880147543739325 ) ) ;
#30467 = CARTESIAN_POINT ( 'NONE',  ( 0.000000000000000000, -9.900000000000005684, 0.000000000000000000 ) ) ;
#30468 = CARTESIAN_POINT ( 'NONE',  ( 5.280183324938524159, -0.9553487854751692154, 1.435786287184135368 ) ) ;
#30469 = CARTESIAN_POINT ( 'NONE',  ( 4.346888830327386266, -1.803415170841724979, -0.9023466997552240798 ) ) ;
#30470 =( BOUNDED_SURFACE ( )  B_SPLINE_SURFACE ( 3, 2, ( 
 ( #158301, #27207, #176671 ),
 ( #45621, #126942, #173498 ),
 ( #26142, #90102, #9892 ),
 ( #91176, #190767, #78095 ),
 ( #8830, #174566, #207023 ),
 ( #142072, #208086, #110671 ) ),
 .UNSPECIFIED., .F., .F., .F. ) 
 B_SPLINE_SURFACE_WITH_KNOTS ( ( 4, 2, 4 ),
 ( 3, 3 ),
 ( 0.000000000000000000, 0.0003831327362561331041, 0.0007662654725122662082 ),
 ( 0.000000000000000000, 1.000000000000000000 ),
 .UNSPECIFIED. ) 
 GEOMETRIC_REPRESENTATION_ITEM ( )  RATIONAL_B_SPLINE_SURFACE ( (
 ( 1.000000000000000000, 0.5879095031487548972, 1.000000000000000000),
 ( 1.000000000000000000, 0.5873691247577063068, 1.000000000000000000),
 ( 1.000000000000000000, 0.6054349545499626561, 1.000000000000000000),
 ( 1.000000000000000000, 0.6533334602764224730, 1.000000000000000000),
 ( 1.000000000000000000, 0.6828746263152883911, 1.000000000000000000),
 ( 1.000000000000000000, 0.7071067811865399122, 1.000000000000000000) ) ) 
 REPRESENTATION_ITEM ( '' )  SURFACE ( )  );
#30471 = CARTESIAN_POINT ( 'NONE',  ( 5.203857780826313117, 2.123009612837105209, 0.8817886472500915396 ) ) ;
#30472 = CARTESIAN_POINT ( 'NONE',  ( 0.5576012004645107822, -1.866542136390366036, -1.177153700605698461 ) ) ;
#30474 = CARTESIAN_POINT ( 'NONE',  ( -4.001064729808656573, 7.682009594836471500, 1.214306433183764966E-14 ) ) ;
#30473 = CARTESIAN_POINT ( 'NONE',  ( -8.306341666666730461, 12.84248237775322643, 1.040834085586084257E-14 ) ) ;
#30475 = CARTESIAN_POINT ( 'NONE',  ( 5.729715491186369469, -1.123817246201250786, -1.367138390065870457 ) ) ;
#30476 = CARTESIAN_POINT ( 'NONE',  ( 5.203750078570229753, 1.864167652161516031, 0.7691231355932278690 ) ) ;
#30478 = CARTESIAN_POINT ( 'NONE',  ( 2.484683925703546237, -0.3935552064166462083, -2.258081804418234473 ) ) ;
#30477 = CARTESIAN_POINT ( 'NONE',  ( 5.032011289327418702, 5.899709921417326974, 1.199719254218452935 ) ) ;
#30479 = CARTESIAN_POINT ( 'NONE',  ( 1.446757823190962577, 0.5079132294574678630, -1.664563843253030750 ) ) ;
#30480 = CIRCLE ( 'NONE', #58145, 0.08000000000000020983 ) ;
#30481 = CARTESIAN_POINT ( 'NONE',  ( 5.120175567455225618, 9.125288595339771547, -0.7998128361456281477 ) ) ;
#30482 = CARTESIAN_POINT ( 'NONE',  ( 1.194254265631944367, -1.094737682603286189, -1.344534739289292569 ) ) ;
#30483 = CARTESIAN_POINT ( 'NONE',  ( 0.6801582343749935644, 0.2552083336747196229, 1.178068619123780802 ) ) ;
#30484 = CARTESIAN_POINT ( 'NONE',  ( -11.97178994924802353, 13.87999993797205356, -0.8322011300497247355 ) ) ;
#30485 = CARTESIAN_POINT ( 'NONE',  ( 1.276089585440323138, -2.118389508516528519, 0.4752255978458518881 ) ) ;
#30486 = CARTESIAN_POINT ( 'NONE',  ( 2.342982756445275427, -1.756855002775299379, -0.9896843009072553432 ) ) ;
#30487 = CARTESIAN_POINT ( 'NONE',  ( 5.531250000000004441, -0.7852924748302730906, -1.895863743163958226 ) ) ;
#30488 = CARTESIAN_POINT ( 'NONE',  ( 1.499999999999989120, 2.056250000682817269, 1.214306433183764966E-14 ) ) ;
#30489 = CARTESIAN_POINT ( 'NONE',  ( 6.604134034941783860, -1.926004669841055339, 0.05029594667986003048 ) ) ;
#30490 = CARTESIAN_POINT ( 'NONE',  ( 1.364683531249997417, 13.23437500034139980, 2.602085213965210642E-15 ) ) ;
#30491 = CARTESIAN_POINT ( 'NONE',  ( 2.127449211838834398, 1.986592753075850037, 0.9941332784057993477 ) ) ;
#30492 = VERTEX_POINT ( 'NONE', #175090 ) ;
#30493 = CARTESIAN_POINT ( 'NONE',  ( 6.598949805828054238, -8.057948861126666529, 6.880414557363697448 ) ) ;
#30494 = CARTESIAN_POINT ( 'NONE',  ( -1.500000000000001332, -0.3499999999999753308, 0.000000000000000000 ) ) ;
#30495 = CARTESIAN_POINT ( 'NONE',  ( 7.995557903757111617, 10.35123685918189729, 1.599625672291281386 ) ) ;
#30496 = CARTESIAN_POINT ( 'NONE',  ( 6.414416072596830887, 8.576847732820027659, -1.443375672974078761 ) ) ;
#30497 =( NAMED_UNIT ( * ) SI_UNIT ( $, .STERADIAN. ) SOLID_ANGLE_UNIT ( ) );
#30498 = AXIS2_PLACEMENT_3D ( 'NONE', #44450, #178708, #110567 ) ;
#30499 = CARTESIAN_POINT ( 'NONE',  ( 5.319757424029775805, 1.030549729363830158, -1.402388650165889095 ) ) ;
#30501 = EDGE_CURVE ( 'NONE', #7055, #122390, #52955, .T. ) ;
#30500 = CARTESIAN_POINT ( 'NONE',  ( 3.367582429956605061, -0.3852447139683997657, 1.923494667983568718 ) ) ;
#30503 = CARTESIAN_POINT ( 'NONE',  ( -5.734735788900501952, 9.634349487118505806, 0.000000000000000000 ) ) ;
#30502 = CARTESIAN_POINT ( 'NONE',  ( 3.171717870593107058, 5.787755718078879674, -1.199719254218446718 ) ) ;
#30504 = DIRECTION ( 'NONE',  ( 0.000000000000000000, 0.000000000000000000, -1.000000000000000000 ) ) ;
#30505 = CARTESIAN_POINT ( 'NONE',  ( 4.727936083913598431, -1.386761530526101405, -1.787517356406182811 ) ) ;
#30506 = CARTESIAN_POINT ( 'NONE',  ( 1.592308366680051490, 1.018618965756763473, -1.793563681512408525 ) ) ;
#30507 = CARTESIAN_POINT ( 'NONE',  ( -5.859094939400033120, 9.987361195942037639, -0.7998128361456231517 ) ) ;
#30508 = CARTESIAN_POINT ( 'NONE',  ( 2.272703622300107362, -1.391801132404853147, 1.783687758696401504 ) ) ;
#30509 = VERTEX_POINT ( 'NONE', #140478 ) ;
#30510 = CARTESIAN_POINT ( 'NONE',  ( -0.7500000000000006661, 1.139583334016154526, -1.299038105676652011 ) ) ;
#30511 = CARTESIAN_POINT ( 'NONE',  ( 4.059713336928523653, 1.856696190431494475, -0.2264497139414511362 ) ) ;
#30512 = CARTESIAN_POINT ( 'NONE',  ( 1.986549370914699963, -1.733795460411426959, 0.04323319158786724514 ) ) ;
#30513 = CARTESIAN_POINT ( 'NONE',  ( 6.304242050522723240, 1.625252681175231029, -1.470355468214133543 ) ) ;
#30514 = CARTESIAN_POINT ( 'NONE',  ( 6.422925328166578574, 2.149888460833260684, 0.8388895797235284002 ) ) ;
#30515 = CARTESIAN_POINT ( 'NONE',  ( 3.643588467267334874, -1.635511012911139650, -1.413612897787956513 ) ) ;
#30516 = CARTESIAN_POINT ( 'NONE',  ( 4.382716955277085269, 1.733964400234957459, -0.8745241987923138005 ) ) ;
#30517 = CARTESIAN_POINT ( 'NONE',  ( -3.755245360860939297, 4.443836344834937613, -1.082531754730548412 ) ) ;
#30518 = CARTESIAN_POINT ( 'NONE',  ( 6.309813054293936574, -1.856383540575656799, 0.2289572138471432372 ) ) ;
#30519 = CARTESIAN_POINT ( 'NONE',  ( 4.307253300151457687, 7.213791655154011551, 0.9935852123437900474 ) ) ;
#30520 = CARTESIAN_POINT ( 'NONE',  ( -11.86145016429273191, 13.40000000000000036, 1.099999999999996758 ) ) ;
#30522 = EDGE_CURVE ( 'NONE', #61877, #96829, #123009, .T. ) ;
#30521 = CARTESIAN_POINT ( 'NONE',  ( 3.092668437693027794, 6.622213920701574885, -0.7216878364870338292 ) ) ;
#30523 = CARTESIAN_POINT ( 'NONE',  ( -1.360316468750052854, 2.661458333674782573, 0.7853790794158581612 ) ) ;
#30524 = CARTESIAN_POINT ( 'NONE',  ( 6.240861317752083970, 2.010826688392798101, -0.1511364921914087889 ) ) ;
#30525 = CARTESIAN_POINT ( 'NONE',  ( -8.306341666666730461, 12.84248237775322643, 1.040834085586084257E-14 ) ) ;
#30526 = CARTESIAN_POINT ( 'NONE',  ( 7.422199028477372451, 10.74665040227725044, -1.199719254218441611 ) ) ;
#30527 = DIRECTION ( 'NONE',  ( 5.578564026256490882E-16, 1.000000000000000000, 9.066213480720158442E-32 ) ) ;
#30529 = DIRECTION ( 'NONE',  ( 1.000000000000000000, -0.000000000000000000, -0.000000000000000000 ) ) ;
#30528 = CARTESIAN_POINT ( 'NONE',  ( 3.035583632137848653, -1.226507576337819483, -1.352503160878690380 ) ) ;
#30530 = CARTESIAN_POINT ( 'NONE',  ( 6.784185045882113130, -8.038658175288276198, -6.650326532587137685 ) ) ;
#30531 = ORIENTED_EDGE ( 'NONE', *, *, #125943, .T. ) ;
#30532 = CARTESIAN_POINT ( 'NONE',  ( -3.919715807682309094, 6.626733304721049933, 1.082531754730549967 ) ) ;
#30533 = CARTESIAN_POINT ( 'NONE',  ( 1.642778471875000035, -4.163541666188708135, -2.845375778867859751 ) ) ;
#30534 = CARTESIAN_POINT ( 'NONE',  ( -6.659026002606323047, 10.92061410301605662, 0.000000000000000000 ) ) ;
#30535 = CARTESIAN_POINT ( 'NONE',  ( 6.305333282589566934, 1.756257216537491450, -0.9971998561906397773 ) ) ;
#30536 = CARTESIAN_POINT ( 'NONE',  ( 1.207859650372544280, 1.608047128250057689, 1.382383069919224106 ) ) ;
#30537 = VERTEX_POINT ( 'NONE', #159886 ) ;
#30538 = CARTESIAN_POINT ( 'NONE',  ( -4.274563570058511175, 8.209017608368725405, 0.000000000000000000 ) ) ;
#30539 = CARTESIAN_POINT ( 'NONE',  ( 2.219380450391433168, 0.3239122733160957890, -1.832380290584040505 ) ) ;
#30540 = CARTESIAN_POINT ( 'NONE',  ( 4.704842999142070603, 5.447737239542574272, -1.199719254218452047 ) ) ;
#30541 = CARTESIAN_POINT ( 'NONE',  ( 6.069226122992825267, 0.1539936439061925788, -2.055202734049704105 ) ) ;
#30542 = CARTESIAN_POINT ( 'NONE',  ( 6.363907750917786821, -0.1017471579566435469, -2.013986097687201049 ) ) ;
#30543 = ORIENTED_EDGE ( 'NONE', *, *, #14538, .F. ) ;
#30544 = EDGE_LOOP ( 'NONE', ( #42490, #193144, #178946, #88016 ) ) ;
#30545 = CARTESIAN_POINT ( 'NONE',  ( -4.069418662396130593, 7.899405539437467816, -0.7998128361456281477 ) ) ;
#30546 = CARTESIAN_POINT ( 'NONE',  ( -8.109748439268576803, 12.61312361245537517, 0.7998128361456481317 ) ) ;
#30547 = DIRECTION ( 'NONE',  ( -1.000000000000000000, 0.000000000000000000, 0.000000000000000000 ) ) ;
#30549 = CARTESIAN_POINT ( 'NONE',  ( 0.07680821025396293578, 0.7488618828427398011, -1.895266105024134839 ) ) ;
#30548 = CARTESIAN_POINT ( 'NONE',  ( -4.630991987519598396, 7.560518531151607213, 1.199719254218452935 ) ) ;
#30550 = CARTESIAN_POINT ( 'NONE',  ( 6.177100234330334061, 7.056796855232915888, 1.058592334412721936 ) ) ;
#30551 = CARTESIAN_POINT ( 'NONE',  ( 5.905624997962407363, 0.3905408587613137805, 1.977747231101577352 ) ) ;
#30552 = CARTESIAN_POINT ( 'NONE',  ( 4.910013284106277354, 1.267360923890372693, -1.335742228452965863 ) ) ;
#30553 = CARTESIAN_POINT ( 'NONE',  ( 0.07700591528354748527, 7.629137130509112907, -2.510791685687420838 ) ) ;
#30554 = CARTESIAN_POINT ( 'NONE',  ( 3.282123524285113003, 1.463787882210180191, 1.784030387633539938 ) ) ;
#30555 = CARTESIAN_POINT ( 'NONE',  ( 5.397027666691686321, 8.454226823519094935, 1.199719254218451159 ) ) ;
#30556 = CARTESIAN_POINT ( 'NONE',  ( 6.380167732536218494, -1.162327630155314484, 1.822330041786710098 ) ) ;
#30557 = CARTESIAN_POINT ( 'NONE',  ( 6.825640269476072497, 10.05066518344239412, 1.199719254218460707 ) ) ;
#30558 = CARTESIAN_POINT ( 'NONE',  ( 0.7670095293261131042, 1.871311197688549699, -0.5191222856946677844 ) ) ;
#30559 = CARTESIAN_POINT ( 'NONE',  ( -3.653032323878261600, 6.349289246911547835, -1.199719254218452047 ) ) ;
#30560 = EDGE_LOOP ( 'NONE', ( #104714, #73690, #186209, #82054, #77047, #114590, #137810, #55593 ) ) ;
#30561 = CARTESIAN_POINT ( 'NONE',  ( 4.517165314107184138, 2.297965829929650372, -0.05084271438157876577 ) ) ;
#30562 = CARTESIAN_POINT ( 'NONE',  ( 5.630352418794719149, 6.139657267270441920, -0.8181431533968346326 ) ) ;
#30563 = CARTESIAN_POINT ( 'NONE',  ( -4.736594563127865420, 6.619389305106191834, -1.599625672291271394 ) ) ;
#30564 = CARTESIAN_POINT ( 'NONE',  ( 4.346470048663173102, 0.4987854378066917116, 1.802870001028591407 ) ) ;
#30565 = CIRCLE ( 'NONE', #85893, 0.08000000000000020983 ) ;
#30568 = CARTESIAN_POINT ( 'NONE',  ( -5.285699784481336927, 7.260012063351913625, 1.599625672291263179 ) ) ;
#30567 = CARTESIAN_POINT ( 'NONE',  ( 0.7499999999999885647, -0.2354166659838466402, 1.299038105676657340 ) ) ;
#30566 = CARTESIAN_POINT ( 'NONE',  ( 1.511816067030671729, -0.6413169068853613597, 1.801808535584384252 ) ) ;
#30569 = CARTESIAN_POINT ( 'NONE',  ( 2.930518499080053907, 1.225513248159842083, -1.835134156090315605 ) ) ;
#30570 = CARTESIAN_POINT ( 'NONE',  ( -0.1399997263889594112, -0.002789056014654289761, -2.000146600338557956 ) ) ;
#30571 = CARTESIAN_POINT ( 'NONE',  ( -3.765305043611756552, 7.354576300424669810, -0.6638232778202641793 ) ) ;
#30572 = CARTESIAN_POINT ( 'NONE',  ( 6.875393295461478260, 8.154285278527437342, -1.082531754730548412 ) ) ;
#30573 = CARTESIAN_POINT ( 'NONE',  ( -2.137381772448751605, 5.645362501165475777, -0.7998128361456281477 ) ) ;
#30574 = CARTESIAN_POINT ( 'NONE',  ( -6.794044373779495771, 8.059378203231773341, 1.082531754730549078 ) ) ;
#30575 = CARTESIAN_POINT ( 'NONE',  ( 1.475783946021753446, 1.170879755915053666, 1.585848323755238320 ) ) ;
#30576 = CARTESIAN_POINT ( 'NONE',  ( 1.712421914926518518, -2.289955115012487052, 0.2841115493098354539 ) ) ;
#30577 = CARTESIAN_POINT ( 'NONE',  ( 2.418345249890076154, 0.8361516037145629854, 1.774881043358336630 ) ) ;
#30578 = CARTESIAN_POINT ( 'NONE',  ( 5.735237406732953680, -0.04512126716067199617, -2.062225806692425945 ) ) ;
#30579 = CARTESIAN_POINT ( 'NONE',  ( 5.341549334104200852, 5.334155099317434257, 0.7216878364870317197 ) ) ;
#30580 = CARTESIAN_POINT ( 'NONE',  ( 5.123001941117305336, 7.070197912760590064, 1.599625672291268286 ) ) ;
#30581 = ORIENTED_EDGE ( 'NONE', *, *, #101820, .F. ) ;
#30582 = CARTESIAN_POINT ( 'NONE',  ( -1.364683531250010295, 5.592708333674750953, 0.7879004041258379498 ) ) ;
#30583 = DIRECTION ( 'NONE',  ( 5.578564026256490882E-16, 1.000000000000000000, 9.066213480720158442E-32 ) ) ;
#30584 = CARTESIAN_POINT ( 'NONE',  ( 4.189106276498237413, 3.989638198777126110, -0.7216878364870188411 ) ) ;
#30585 = CARTESIAN_POINT ( 'NONE',  ( 1.059715561420447205, 1.773747297294786307, 1.251667063311131312 ) ) ;
#30587 = DIRECTION ( 'NONE',  ( -0.7592566023652989049, 0.6507913734559658270, -1.175982368226367737E-15 ) ) ;
#30586 = DIRECTION ( 'NONE',  ( 0.000000000000000000, 0.000000000000000000, 1.000000000000000000 ) ) ;
#30588 = CARTESIAN_POINT ( 'NONE',  ( 11.19002393767583747, 0.9691415390508388850, -4.042856490848130591 ) ) ;
#30589 = CYLINDRICAL_SURFACE ( 'NONE', #146562, 0.09999999999999961697 ) ;
#30590 = CARTESIAN_POINT ( 'NONE',  ( 3.004993591039197831, 1.578202713744047303, 1.003818400984110681 ) ) ;
#30591 = CARTESIAN_POINT ( 'NONE',  ( 6.380167732536218494, -1.162327630155314484, 1.822330041786710098 ) ) ;
#30593 = CARTESIAN_POINT ( 'NONE',  ( 6.827182134110198142, 0.003888933837258023996, 1.810856214465889069 ) ) ;
#30592 = CARTESIAN_POINT ( 'NONE',  ( -0.02244404828157658613, 5.719765766439059540, -2.783169749654360814 ) ) ;
#30594 = CARTESIAN_POINT ( 'NONE',  ( -1.364683531250014514, -0.5114583329919092369, -0.7879004041258359514 ) ) ;
#30595 = CARTESIAN_POINT ( 'NONE',  ( 2.227084300891319035, 1.708885092217244051, 0.8583199515034346527 ) ) ;
#30596 = CARTESIAN_POINT ( 'NONE',  ( 3.660817930519409291, -1.560716028760079421, -0.8345783561882027524 ) ) ;
#30597 = CARTESIAN_POINT ( 'NONE',  ( 1.840342752298686380, 1.099902316243700939, -1.564109231055022864 ) ) ;
#30598 = CARTESIAN_POINT ( 'NONE',  ( -3.879604511804807032, 7.677955697080923514, 0.7998128361456341429 ) ) ;
#30600 = CARTESIAN_POINT ( 'NONE',  ( 5.062082326478217098, -1.060395474731326448, 1.595121111449711693 ) ) ;
#30599 = CARTESIAN_POINT ( 'NONE',  ( 0.3708575915560879954, -3.142560865293257510, -3.359854750545201885 ) ) ;
#30601 = CARTESIAN_POINT ( 'NONE',  ( 6.689911425329987615, -1.285551722473629477, -1.492250998650017202 ) ) ;
#30602 = CARTESIAN_POINT ( 'NONE',  ( -1.500000000000011324, 4.629166666666689522, -0.8660254037844313801 ) ) ;
#30604 = CARTESIAN_POINT ( 'NONE',  ( 1.846092968827160119, -1.388944967848893430, -1.602481653760478020 ) ) ;
#30603 = VECTOR ( 'NONE', #88207, 1000.000000000000000 ) ;
#30605 = CARTESIAN_POINT ( 'NONE',  ( 5.471519871388384360, 1.802534880541529994, -0.5000026934619330454 ) ) ;
#30607 = EDGE_LOOP ( 'NONE', ( #67891, #183800, #202705, #93886 ) ) ;
#30606 = CARTESIAN_POINT ( 'NONE',  ( 0.02954982209854748257, -1.120125052174587577, -1.442194003765177257 ) ) ;
#30609 = CARTESIAN_POINT ( 'NONE',  ( -1.999999999999988010, 2.428614679364265457E-14, 0.5999999999999969802 ) ) ;
#30608 = CARTESIAN_POINT ( 'NONE',  ( 4.723365791888975096, -0.1103408873950258995, 2.204240794804641190 ) ) ;
#30610 = CARTESIAN_POINT ( 'NONE',  ( 1.364683531249984538, -1.094791666325247936, -0.7879004041258309554 ) ) ;
#30611 = CARTESIAN_POINT ( 'NONE',  ( 2.436046450607622926, 1.266989887546982052, 1.627633791282004250 ) ) ;
#30612 = CARTESIAN_POINT ( 'NONE',  ( 6.908042961362778733, 8.018137195466769285, 1.199719254218462483 ) ) ;
#30613 = CARTESIAN_POINT ( 'NONE',  ( -9.176171038350775078, 9.599954387697719582, -0.7998128361456291469 ) ) ;
#30614 = CARTESIAN_POINT ( 'NONE',  ( 0.000000000000000000, 13.49999999999999822, -1.500000000000000222 ) ) ;
#30615 = CARTESIAN_POINT ( 'NONE',  ( 1.297623789354739987, 3.601497945116066468, -0.4387493294077405293 ) ) ;
#30616 = CARTESIAN_POINT ( 'NONE',  ( -0.9999999999999988898, 6.468705557303653819, -4.925226524755048629 ) ) ;
#30617 = CARTESIAN_POINT ( 'NONE',  ( 0.1753634416057497647, 0.2329791690731698173, -2.177930625204091086 ) ) ;
#30618 = ORIENTED_EDGE ( 'NONE', *, *, #122876, .T. ) ;
#30619 = CARTESIAN_POINT ( 'NONE',  ( 4.229010956685672618, -1.930657356216297860, -0.7480826485904977785 ) ) ;
#30620 = CARTESIAN_POINT ( 'NONE',  ( -0.7500000000000215383, 5.441666666666685082, 1.299038105676671107 ) ) ;
#30621 = CARTESIAN_POINT ( 'NONE',  ( 2.354944161360218224, -1.672559397656541824, 1.369352967626968898 ) ) ;
#30622 = CARTESIAN_POINT ( 'NONE',  ( -6.348239482750515528, 6.857177101084271698, -0.6483580952693357435 ) ) ;
#30623 = CARTESIAN_POINT ( 'NONE',  ( 2.455728411619819251, -1.498007593246965419, -1.354850333784217709 ) ) ;
#30624 = CARTESIAN_POINT ( 'NONE',  ( 4.465192238825641979, 7.096428296808035441, -1.166435484173217629 ) ) ;
#30625 = EDGE_CURVE ( 'NONE', #158833, #40807, #138669, .T. ) ;
#30626 = EDGE_LOOP ( 'NONE', ( #180949, #134007, #137222, #70638 ) ) ;
#30627 = ORIENTED_EDGE ( 'NONE', *, *, #27402, .T. ) ;
#30629 = CARTESIAN_POINT ( 'NONE',  ( 6.480434237652115570, 10.50433101066207442, 0.7216878364870438212 ) ) ;
#30628 = FACE_OUTER_BOUND ( 'NONE', #79279, .T. ) ;
#30630 = CARTESIAN_POINT ( 'NONE',  ( -4.462041952228954500, 6.299077925724123617, -1.443375672974066548 ) ) ;
#30631 = CARTESIAN_POINT ( 'NONE',  ( 0.005092704479254389627, -0.09411098085002241043, 2.014433268766747887 ) ) ;
#30632 = CARTESIAN_POINT ( 'NONE',  ( 5.179302069984247581, 1.471482994053765925, 1.624232740060495228 ) ) ;
#30633 = EDGE_CURVE ( 'NONE', #197667, #19630, #91025, .T. ) ;
#30634 = CARTESIAN_POINT ( 'NONE',  ( 0.7499999999999902300, 5.347916667349482012, -1.299038105676658228 ) ) ;
#30635 = CARTESIAN_POINT ( 'NONE',  ( 5.185773951807310489, 1.841398108398510480, -0.5159224025059681029 ) ) ;
#30636 = CARTESIAN_POINT ( 'NONE',  ( -3.090368948911150770, 5.692848642783215674, 1.199719254218462483 ) ) ;
#30637 = EDGE_CURVE ( 'NONE', #211395, #109852, #106246, .T. ) ;
#30638 = CARTESIAN_POINT ( 'NONE',  ( 5.246642258364164313, 8.104537820524768676, -1.082531754730549078 ) ) ;
#30640 = CARTESIAN_POINT ( 'NONE',  ( 2.583611426500437069, -0.6298568260672477992, 1.915607262459443794 ) ) ;
#30639 = CARTESIAN_POINT ( 'NONE',  ( -9.341204649691320583, 10.96078884847042545, 1.082531754730558626 ) ) ;
#30641 = CARTESIAN_POINT ( 'NONE',  ( -1.402160292154681736E-14, 12.73437500034139980, 1.575800808251682339 ) ) ;
#30642 = CARTESIAN_POINT ( 'NONE',  ( -3.467853430045390706, 7.267855778353407459, 0.7998128361456352531 ) ) ;
#30643 = CARTESIAN_POINT ( 'NONE',  ( 5.262619041473771020, -1.246969283750315460, 1.191858809209481285 ) ) ;
#30644 = CARTESIAN_POINT ( 'NONE',  ( 5.840530312436913007, 10.03597880781023299, 0.000000000000000000 ) ) ;
#30645 = CARTESIAN_POINT ( 'NONE',  ( 3.358669367883368118, 4.941533567329135401, -1.599625672291262513 ) ) ;
#30646 = DIRECTION ( 'NONE',  ( 3.070755325854836401E-18, 0.9998511425080263137, -0.01725377713413180428 ) ) ;
#30647 = DIRECTION ( 'NONE',  ( 0.000000000000000000, 1.000000000000000000, 0.000000000000000000 ) ) ;
#30648 = ORIENTED_EDGE ( 'NONE', *, *, #144753, .T. ) ;
#30649 = CARTESIAN_POINT ( 'NONE',  ( 0.7255434793691470929, 0.2065170452952343472, -2.059959488672699290 ) ) ;
#30650 = ORIENTED_EDGE ( 'NONE', *, *, #70571, .T. ) ;
#30651 = CARTESIAN_POINT ( 'NONE',  ( 4.529823624924778969, -1.775545877285337193, 0.3580350944670795399 ) ) ;
#30652 = CARTESIAN_POINT ( 'NONE',  ( 6.066347387471824781, 6.042103138330730872, -0.7998128361456481317 ) ) ;
#30653 = DIRECTION ( 'NONE',  ( 0.000000000000000000, -1.000000000000000000, 0.000000000000000000 ) ) ;
#30654 = CARTESIAN_POINT ( 'NONE',  ( 6.498695496729308907, -1.778006411731817060, -0.3456425897902185018 ) ) ;
#30655 = CARTESIAN_POINT ( 'NONE',  ( 6.495764994278809823, 6.751016379513001375, 0.7216878364870328300 ) ) ;
#30656 = COLOUR_RGB ( '', 0.40784314, 0.44705882, 0.49803922) ;
#30657 = CARTESIAN_POINT ( 'NONE',  ( 11.52676144591142915, 8.443953938884890320, 3.358931424421359502 ) ) ;
#30658 = CARTESIAN_POINT ( 'NONE',  ( 2.994263412949605296, -0.6367403190770392074, -2.096898073876966251 ) ) ;
#30659 = ORIENTED_EDGE ( 'NONE', *, *, #187807, .T. ) ;
#30661 = CARTESIAN_POINT ( 'NONE',  ( 8.751951852821344247, 10.16936423550178503, -1.199719254218446718 ) ) ;
#30660 = CARTESIAN_POINT ( 'NONE',  ( 0.5901948623465642640, 1.011764341257429978, -1.680720577067334354 ) ) ;
#30662 = CARTESIAN_POINT ( 'NONE',  ( 4.939036846723444008, -1.620647644904899654, -1.020970555301304206 ) ) ;
#30663 = DIRECTION ( 'NONE',  ( 0.000000000000000000, 1.000000000000000000, 0.000000000000000000 ) ) ;
#30664 = EDGE_CURVE ( 'NONE', #79740, #161718, #104776, .T. ) ;
#30665 =( LENGTH_UNIT ( ) NAMED_UNIT ( * ) SI_UNIT ( .MILLI., .METRE. ) );
#30666 = CARTESIAN_POINT ( 'NONE',  ( 1.364683531249986537, 0.1552083336747499542, -0.7879004041258309554 ) ) ;
#30667 = CARTESIAN_POINT ( 'NONE',  ( 4.772106882330221289, 6.590544000850479200, -1.443375672974051449 ) ) ;
#30668 = CARTESIAN_POINT ( 'NONE',  ( -9.164948653158003111, 9.794787638213568570, -0.7216878364870267237 ) ) ;
#30669 = CARTESIAN_POINT ( 'NONE',  ( 2.044033295145482043, 0.8276103948961744949, -1.997198329219296742 ) ) ;
#30670 = CARTESIAN_POINT ( 'NONE',  ( -4.285259070371116863, 7.157163461145040095, 1.199719254218452935 ) ) ;
#30671 = CARTESIAN_POINT ( 'NONE',  ( 3.881377115262159894, 7.750300077773022878, 0.7998128361456271485 ) ) ;
#30672 = CARTESIAN_POINT ( 'NONE',  ( 2.502731746374619259, 1.467688513602287470, -1.085450786651315225 ) ) ;
#30673 = CARTESIAN_POINT ( 'NONE',  ( -4.277761160311629673, 4.949475094240346706, 1.199719254218462483 ) ) ;
#30674 = CARTESIAN_POINT ( 'NONE',  ( 4.541915102786819425, 0.7800907816924649296, -1.650662693317282770 ) ) ;
#30675 = CARTESIAN_POINT ( 'NONE',  ( 9.231319260696198015, 13.16052827424349303, 9.015053781678833644 ) ) ;
#30676 = CARTESIAN_POINT ( 'NONE',  ( 2.636851627972558454, 1.802111047976437508, 0.6404684511054498097 ) ) ;
#30677 = ORIENTED_EDGE ( 'NONE', *, *, #33908, .F. ) ;
#30678 = CARTESIAN_POINT ( 'NONE',  ( 4.158625497742932886, -0.6157697831138170264, -1.870904811771924470 ) ) ;
#30679 = ORIENTED_EDGE ( 'NONE', *, *, #210461, .T. ) ;
#30680 = CARTESIAN_POINT ( 'NONE',  ( 4.669442277103274641, 1.121057080241712578, 1.585637770727834850 ) ) ;
#30681 = ORIENTED_EDGE ( 'NONE', *, *, #7830, .F. ) ;
#30682 = CARTESIAN_POINT ( 'NONE',  ( -6.074935347375019390, 9.245119117649618801, 1.199719254218452047 ) ) ;
#30684 = CARTESIAN_POINT ( 'NONE',  ( 5.678019686890188211, 2.088907387943875982, -0.3644037002746222664 ) ) ;
#30683 = CARTESIAN_POINT ( 'NONE',  ( 6.855582950365507244, 8.027210192628430718, -1.199719254218452047 ) ) ;
#30685 = CARTESIAN_POINT ( 'NONE',  ( -7.015401035077384329, 6.062865449010540253, -2.437084766375293476 ) ) ;
#30687 = ORIENTED_EDGE ( 'NONE', *, *, #40765, .T. ) ;
#30686 = CARTESIAN_POINT ( 'NONE',  ( 3.334525359879161766, 1.211162569113528598, -1.479845612687477496 ) ) ;
#30688 = B_SPLINE_CURVE_WITH_KNOTS ( 'NONE', 3,
 ( #91695, #107986, #123201, #27730 ),
 .UNSPECIFIED., .F., .F.,
 ( 4, 4 ),
 ( 0.0009695358052320346897, 0.001130783094531867799 ),
 .UNSPECIFIED. ) ;
#30689 = CARTESIAN_POINT ( 'NONE',  ( 5.178766244632133642, 6.659365504414815895, -1.397763381526682336 ) ) ;
#30690 = CARTESIAN_POINT ( 'NONE',  ( 6.983263157960362122, 3.696136926403908340, 2.460428995873820135 ) ) ;
#30691 = LINE ( 'NONE', #42685, #119560 ) ;
#30692 = CARTESIAN_POINT ( 'NONE',  ( 5.657830175604453338, 5.495223381160312393, 0.7998128361456341429 ) ) ;
#30693 = CARTESIAN_POINT ( 'NONE',  ( 5.356112940025661295, 0.8138243144468767509, -1.841424879227879119 ) ) ;
#30694 = CARTESIAN_POINT ( 'NONE',  ( 11.04536101718726293, 12.69999999999999929, -1.100000000000000311 ) ) ;
#30695 = CARTESIAN_POINT ( 'NONE',  ( 4.775911370473768791, 1.053640644303525331, 1.490772598166143048 ) ) ;
#30696 = CARTESIAN_POINT ( 'NONE',  ( 0.5903903138861701372, 1.065687334306382184, -1.774900233272216798 ) ) ;
#30697 = CARTESIAN_POINT ( 'NONE',  ( -8.690413276679693766, 9.241163032322203819, 1.040834085586084257E-14 ) ) ;
#30698 = STYLED_ITEM ( 'NONE', ( #197207 ), #213750 ) ;
#30699 = CARTESIAN_POINT ( 'NONE',  ( -6.477282242306868554, 6.848760321534919093, 0.6499626829332164624 ) ) ;
#30700 = CARTESIAN_POINT ( 'NONE',  ( -1.225000000000030065, 1.541666667349459230, -0.7072540797573017013 ) ) ;
#30701 = CARTESIAN_POINT ( 'NONE',  ( 5.735183426005796115, -1.690533149647139410, 0.8011652756413772947 ) ) ;
#30702 = CARTESIAN_POINT ( 'NONE',  ( 5.612185521052973414, 8.634967976948757951, -1.199719254218440723 ) ) ;
#30703 = CARTESIAN_POINT ( 'NONE',  ( 3.023105066167310895, 5.702484939155337607, -2.419999999999995044 ) ) ;
#30704 = CARTESIAN_POINT ( 'NONE',  ( 1.364683531250000303, 10.31770833367473195, -0.7879004041258355073 ) ) ;
#30705 = CARTESIAN_POINT ( 'NONE',  ( -6.600121851754250812, 6.594563670001734046, 0.7998128361456341429 ) ) ;
#30707 = CARTESIAN_POINT ( 'NONE',  ( -5.772739544368596043, 9.956889578397179363, -0.7998128361456362523 ) ) ;
#30706 = LINE ( 'NONE', #144486, #93436 ) ;
#30708 = CARTESIAN_POINT ( 'NONE',  ( -5.742041750587549842, 6.657802449562273850, 1.199719254218450271 ) ) ;
#30709 = AXIS2_PLACEMENT_3D ( 'NONE', #96625, #33719, #99796 ) ;
#30710 = CARTESIAN_POINT ( 'NONE',  ( 1.832961912758425349, -1.964510197511709189, -0.6532998099852762586 ) ) ;
#30711 = CARTESIAN_POINT ( 'NONE',  ( 2.302504360600155842, 1.380385731239835323, -1.605472654339132887 ) ) ;
#30712 = CARTESIAN_POINT ( 'NONE',  ( 6.401421083946654100, 10.62007503124645957, -0.7998128361456291469 ) ) ;
#30713 = CARTESIAN_POINT ( 'NONE',  ( 0.4041367621137377242, 3.038026290190030121, 0.4210133165199971828 ) ) ;
#30714 = CARTESIAN_POINT ( 'NONE',  ( 0.2507523796677147421, -0.4231762011769435450, -1.930160340004604569 ) ) ;
#30715 = CARTESIAN_POINT ( 'NONE',  ( 5.061713581663421557, 6.751138122384800155, 1.419579013000639378 ) ) ;
#30716 = CARTESIAN_POINT ( 'NONE',  ( 5.016153647376212277, 5.914896012436124728, 1.082531754730558626 ) ) ;
#30718 = DIRECTION ( 'NONE',  ( 0.000000000000000000, 1.000000000000000000, 0.000000000000000000 ) ) ;
#30717 = CARTESIAN_POINT ( 'NONE',  ( -1.737499999999997824, -3.791666666666665186, 3.009438278150925683 ) ) ;
#30719 = CARTESIAN_POINT ( 'NONE',  ( 2.836170770286027043, 2.275064633363361732, 0.2797384389828549978 ) ) ;
#30720 = CARTESIAN_POINT ( 'NONE',  ( 1.031563979315492485, -1.156294252604734396, -1.412831148817683680 ) ) ;
#30721 = CARTESIAN_POINT ( 'NONE',  ( 2.390748813209525814, -1.831196095803063528, -0.5514187292172747501 ) ) ;
#30723 = ORIENTED_EDGE ( 'NONE', *, *, #146061, .T. ) ;
#30722 = CARTESIAN_POINT ( 'NONE',  ( 6.530187263637528439, 7.647581891445782709, -1.199719254218452047 ) ) ;
#30724 = CARTESIAN_POINT ( 'NONE',  ( 7.415946836550722843, 8.714654733139752807, 1.082531754730558626 ) ) ;
#30725 = CARTESIAN_POINT ( 'NONE',  ( 1.582290772395946066, 1.038639357175192401, 1.724485448976780688 ) ) ;
#30726 = CARTESIAN_POINT ( 'NONE',  ( 0.6901946996495964548, 1.013433542811643440, -1.679602092450118489 ) ) ;
#30727 = CARTESIAN_POINT ( 'NONE',  ( -8.296699936558862731, 11.76690146170562201, 1.199719254218453823 ) ) ;
#30728 = CARTESIAN_POINT ( 'NONE',  ( -8.050844288416501016, 8.287073179441051707, 1.040834085586084257E-14 ) ) ;
#30729 = DIRECTION ( 'NONE',  ( 0.000000000000000000, 0.000000000000000000, 1.000000000000000000 ) ) ;
#30731 = CARTESIAN_POINT ( 'NONE',  ( 3.924454612484959082, 1.680539001619888229, 0.5552615287828834845 ) ) ;
#30730 = CARTESIAN_POINT ( 'NONE',  ( 4.259774723613071856, 0.9852665271268057356, 1.843911019796584450 ) ) ;
#30732 = CARTESIAN_POINT ( 'NONE',  ( -7.247736482492992849, 15.00000000000182077, 10.57961706324680584 ) ) ;
#30734 = CARTESIAN_POINT ( 'NONE',  ( 0.09403522832084068583, -2.191061582759439297, -0.04926842934906834615 ) ) ;
#30733 = CARTESIAN_POINT ( 'NONE',  ( 0.000000000000000000, -6.893137084989842123, 0.000000000000000000 ) ) ;
#30735 = CARTESIAN_POINT ( 'NONE',  ( 4.540767487494163035, -1.347652659646558115, -1.101159657664248170 ) ) ;
#30736 = CARTESIAN_POINT ( 'NONE',  ( 8.646349277213076334, 11.11049346154719508, 1.599625672291281386 ) ) ;
#30737 = MECHANICAL_DESIGN_GEOMETRIC_PRESENTATION_REPRESENTATION (  '', ( #23748 ), #120780 ) ;
#30738 = CARTESIAN_POINT ( 'NONE',  ( 0.000000000000000000, -4.000000000000005329, -4.899999999999999467 ) ) ;
#30739 = CARTESIAN_POINT ( 'NONE',  ( 4.973871655188280450, 1.509253006592145452, 0.8532917887605420137 ) ) ;
#30740 = CARTESIAN_POINT ( 'NONE',  ( 5.020078820186387070, 2.148262114505914866, -0.3138009609788168230 ) ) ;
#30741 = CARTESIAN_POINT ( 'NONE',  ( 4.871457266011829823, 4.577788319968905562, -0.7998128361456221525 ) ) ;
#30742 = CARTESIAN_POINT ( 'NONE',  ( 5.366422816783521732, -1.968444216653497003, -0.4370823996120917765 ) ) ;
#30743 = CARTESIAN_POINT ( 'NONE',  ( 6.187500000000010658, -1.451031289060719320, 1.451031289061361473 ) ) ;
#30744 = DIRECTION ( 'NONE',  ( 1.000000000000000000, 0.000000000000000000, 0.000000000000000000 ) ) ;
#30745 = CARTESIAN_POINT ( 'NONE',  ( 2.696214026845968448, -1.921097006559132625, -0.1437054574915888616 ) ) ;
#30746 = CARTESIAN_POINT ( 'NONE',  ( -1.500000000000001110, 9.802083334016129967, 0.8660254037844419273 ) ) ;
#30747 = CARTESIAN_POINT ( 'NONE',  ( 6.416288448142412726, -2.220950948806613034, 0.05311210701240512422 ) ) ;
#30748 = EDGE_LOOP ( 'NONE', ( #21644, #7939, #46642, #53862, #58105 ) ) ;
#30749 = CARTESIAN_POINT ( 'NONE',  ( 6.883263157960366918, 2.433703524355503411, 2.428201320676713237 ) ) ;
#30750 = CARTESIAN_POINT ( 'NONE',  ( -0.7500000000000215383, 2.941666666666689522, 1.299038105676671107 ) ) ;
#30751 = CARTESIAN_POINT ( 'NONE',  ( 4.123651276850781144, 7.962676922967908411, -0.7998128361456221525 ) ) ;
#30752 = CARTESIAN_POINT ( 'NONE',  ( 1.770501988737150922, 2.215049892327343173, -0.1675478377428234744 ) ) ;
#30754 = EDGE_CURVE ( 'NONE', #75032, #186231, #132482, .T. ) ;
#30753 = CARTESIAN_POINT ( 'NONE',  ( 6.549272904993657995, 1.707534169505098953, -0.9658701945045379267 ) ) ;
#30755 = CARTESIAN_POINT ( 'NONE',  ( 6.805829924380097040, 10.88395931184472154, 0.7216878364870438212 ) ) ;
#30756 = CIRCLE ( 'NONE', #65342, 10.24999999999999822 ) ;
#30757 = CARTESIAN_POINT ( 'NONE',  ( 0.4967775439448678942, 7.792564024146675372, 1.990974371293808165 ) ) ;
#30758 = CARTESIAN_POINT ( 'NONE',  ( 5.401997860402196316, 5.267028690082820930, 0.000000000000000000 ) ) ;
#30759 = CARTESIAN_POINT ( 'NONE',  ( -5.153507786970285665, 5.185049637652990207, -0.7216878364870338292 ) ) ;
#30761 = CARTESIAN_POINT ( 'NONE',  ( 5.055161771162819839, 1.716784339331741682, -1.143088790766825236 ) ) ;
#30760 = CARTESIAN_POINT ( 'NONE',  ( 9.622536337397022521, 12.24937836509514710, 1.599625672291281386 ) ) ;
#30762 = FACE_OUTER_BOUND ( 'NONE', #179004, .T. ) ;
#30763 = CARTESIAN_POINT ( 'NONE',  ( -3.255929445576174697, 6.950334786480840243, -0.7998128361456281477 ) ) ;
#30764 = CARTESIAN_POINT ( 'NONE',  ( -1.201851678989727383E-14, 5.118750000682815937, -1.732050807568863648 ) ) ;
#30765 = CARTESIAN_POINT ( 'NONE',  ( -1.364683531250014514, -0.5114583329919092369, -0.7879004041258359514 ) ) ;
#30766 = CARTESIAN_POINT ( 'NONE',  ( 6.626239551081194001, 1.076695052409048614, -1.529385127534782951 ) ) ;
#30767 = CARTESIAN_POINT ( 'NONE',  ( 5.432138663567621428, -1.371958567392589146, -1.060553414760868618 ) ) ;
#30768 = CARTESIAN_POINT ( 'NONE',  ( 4.493551464656197147, -1.740228352261258049, -0.03666429755099299970 ) ) ;
#30769 = CARTESIAN_POINT ( 'NONE',  ( 2.835626683552519012, 6.459981564119914310, 0.000000000000000000 ) ) ;
#30770 = B_SPLINE_CURVE_WITH_KNOTS ( 'NONE', 3,
 ( #100742, #81310, #150583, #179881, #66081, #198233, #147386, #49869 ),
 .UNSPECIFIED., .F., .F.,
 ( 4, 2, 2, 4 ),
 ( 0.000000000000000000, 0.002997375907120273901, 0.004496063860680410418, 0.005994751814240547802 ),
 .UNSPECIFIED. ) ;
#30771 = CARTESIAN_POINT ( 'NONE',  ( 2.912002956782848262, -1.132189443809348273, -1.993217883792548495 ) ) ;
#30772 = CARTESIAN_POINT ( 'NONE',  ( 1.364683531249990311, 5.196875000341417916, 1.214306433183764966E-14 ) ) ;
#30773 = CARTESIAN_POINT ( 'NONE',  ( 1.060217833243476182, -1.663605802054025418, -0.7890760572396152694 ) ) ;
#30774 = CARTESIAN_POINT ( 'NONE',  ( 3.998552503512865730, 7.829812139846150210, 0.1485553033222472286 ) ) ;
#30775 = CARTESIAN_POINT ( 'NONE',  ( -9.604686356149278126, 3.999999999999997335, -7.193747284969076894 ) ) ;
#30776 = CARTESIAN_POINT ( 'NONE',  ( 2.326929888710258965, -0.002694909042751796133, 1.825762228105472840 ) ) ;
#30777 = CARTESIAN_POINT ( 'NONE',  ( 3.111954093273407107, 0.05229746705895028935, 2.015912966248374349 ) ) ;
#30778 = CARTESIAN_POINT ( 'NONE',  ( 1.342011898504836820, 2.189069585219292957, 0.1046993245200772138 ) ) ;
#30779 = CARTESIAN_POINT ( 'NONE',  ( 9.573135803333604699, 13.80976963840737248, -8.295511852730781399 ) ) ;
#30780 = CARTESIAN_POINT ( 'NONE',  ( 4.383879424978657902, 1.373869114255725776, 1.596202613037283502 ) ) ;
#30781 = CARTESIAN_POINT ( 'NONE',  ( -6.527360889975461156, 9.702672574024962415, 1.199719254218452047 ) ) ;
#30782 = CARTESIAN_POINT ( 'NONE',  ( 8.745502095769714046, 13.65234029860456388, 7.751384471964883893 ) ) ;
#30783 = CARTESIAN_POINT ( 'NONE',  ( 1.469279758060073160, 1.824989553406907383, 0.9776941847434923449 ) ) ;
#30784 = CARTESIAN_POINT ( 'NONE',  ( 3.981290663907289140, 7.796589541200495965, -0.7998128361456221525 ) ) ;
#30785 = CARTESIAN_POINT ( 'NONE',  ( -1.360316468750024876, -1.057291666325259172, 0.7853790794158601596 ) ) ;
#30786 = CARTESIAN_POINT ( 'NONE',  ( 3.721430941620011534, 1.819509361161365524, 1.088713516244857571 ) ) ;
#30787 = CARTESIAN_POINT ( 'NONE',  ( 6.164658409365947556, -1.287482145768016339, 1.294691480910937775 ) ) ;
#30788 = ORIENTED_EDGE ( 'NONE', *, *, #2169, .F. ) ;
#30789 = CARTESIAN_POINT ( 'NONE',  ( -6.466312919074983512, 6.508729591867735031, -0.7998128361456362523 ) ) ;
#30790 = CARTESIAN_POINT ( 'NONE',  ( 10.01963921569910632, 11.64833282552586091, 1.199719254218450271 ) ) ;
#30791 = CARTESIAN_POINT ( 'NONE',  ( 4.868786560638878491, 8.694351730805124134, 0.7216878364870317197 ) ) ;
#30792 = CARTESIAN_POINT ( 'NONE',  ( 3.475000000000000533, -3.281249999044083765, 0.000000000000000000 ) ) ;
#30793 = CARTESIAN_POINT ( 'NONE',  ( -4.205000198532790279, 8.057583998263570635, 0.7998128361456341429 ) ) ;
#30794 = CARTESIAN_POINT ( 'NONE',  ( 3.111586589114573975, 1.594763109418888991, 1.239388640070989478 ) ) ;
#30795 = CARTESIAN_POINT ( 'NONE',  ( 0.7980485993467776318, -0.7579980429349441051, 1.964993406121709807 ) ) ;
#30796 = CARTESIAN_POINT ( 'NONE',  ( -3.983063267364693960, 7.868933921892603323, -0.7998128361456481317 ) ) ;
#30797 = CARTESIAN_POINT ( 'NONE',  ( 7.781490099239519509, 11.16582331816642260, 1.199719254218460707 ) ) ;
#30798 = CARTESIAN_POINT ( 'NONE',  ( 5.049569799528213387, 1.377159375265882391, 1.251766951177714526 ) ) ;
#30799 = CARTESIAN_POINT ( 'NONE',  ( 7.214910300766615769, 11.56914578420308715, -0.7998128361456291469 ) ) ;
#30800 = CARTESIAN_POINT ( 'NONE',  ( -0.6499431002536736335, 4.349926030312408542, 0.06915891592278980426 ) ) ;
#30801 = CARTESIAN_POINT ( 'NONE',  ( -5.957882158562513908, 5.915560371269843465, -0.7998128361456362523 ) ) ;
#30802 = CARTESIAN_POINT ( 'NONE',  ( -9.707274797704657843, 11.38787068781932987, 1.082531754730558626 ) ) ;
#30804 = CARTESIAN_POINT ( 'NONE',  ( 2.084357000244409175, 1.132115006494602394, -1.602057852124554316 ) ) ;
#30803 = CARTESIAN_POINT ( 'NONE',  ( -6.775324078527193983, 8.927630729746953264, -1.599625672291263179 ) ) ;
#30805 = CARTESIAN_POINT ( 'NONE',  ( 0.7784641540938314064, -1.199969256800371697, 1.797863220954009966 ) ) ;
#30807 = CARTESIAN_POINT ( 'NONE',  ( -5.867374215541069304, 6.167859493020809047, 0.9100554989533160555 ) ) ;
#30806 = CARTESIAN_POINT ( 'NONE',  ( -5.261446130555064826, 8.296048364692991228, 1.199719254218452935 ) ) ;
#30808 = CARTESIAN_POINT ( 'NONE',  ( 1.364683531249986537, 0.4052083336747511200, -0.7879004041258309554 ) ) ;
#30809 = CARTESIAN_POINT ( 'NONE',  ( 2.811537702714523856, -1.443443483380968173, 0.9601682615991720127 ) ) ;
#30810 = CARTESIAN_POINT ( 'NONE',  ( 1.921426573741076727, 1.003422016191083399, -1.421716384592019544 ) ) ;
#30811 = STYLED_ITEM ( 'NONE', ( #8520 ), #36249 ) ;
#30813 = CARTESIAN_POINT ( 'NONE',  ( 7.131225611108088280, 9.342849184424693476, 1.443375672974076540 ) ) ;
#30812 = CARTESIAN_POINT ( 'NONE',  ( 0.2359759974720798681, -2.107749471535870445, 0.9397143452993106383 ) ) ;
#30814 = CARTESIAN_POINT ( 'NONE',  ( -10.45142682343936791, 5.144546645612242841, 5.216777551074719632 ) ) ;
#30815 = CARTESIAN_POINT ( 'NONE',  ( 2.970052003254409545, 1.099468894914462647, 1.742775920482849905 ) ) ;
#30816 = CARTESIAN_POINT ( 'NONE',  ( 6.030679399980265920, 5.930214142932100252, -0.7998128361456281477 ) ) ;
#30817 = CARTESIAN_POINT ( 'NONE',  ( 1.124374798274978104, 0.3960433595797500095, -1.976652716225081097 ) ) ;
#30818 = CARTESIAN_POINT ( 'NONE',  ( 6.925078400183553029, 0.5745968962584145912, 2.096956839219825230 ) ) ;
#30819 = CARTESIAN_POINT ( 'NONE',  ( -3.135678666510573365, 6.880318554229450712, 0.000000000000000000 ) ) ;
#30820 = CARTESIAN_POINT ( 'NONE',  ( 1.639464495141579770, -1.426599704724445861, -1.360921036830293307 ) ) ;
#30821 = EDGE_CURVE ( 'NONE', #201912, #84679, #205772, .T. ) ;
#30823 = CARTESIAN_POINT ( 'NONE',  ( -6.970300371201519241, 7.304640985922785212, 0.7216878364870317197 ) ) ;
#30822 = CARTESIAN_POINT ( 'NONE',  ( 4.535362393419643645, -0.08824616237496611670, 1.910463848342447202 ) ) ;
#30824 = B_SPLINE_CURVE_WITH_KNOTS ( 'NONE', 3,
 ( #103868, #203460, #156892, #21503, #55114, #24727 ),
 .UNSPECIFIED., .F., .F.,
 ( 4, 2, 4 ),
 ( 0.001105973075985145371, 0.001142139074170123950, 0.001178305072355102529 ),
 .UNSPECIFIED. ) ;
#30825 = CARTESIAN_POINT ( 'NONE',  ( -7.404161286394468355, 7.810812053647902431, 0.000000000000000000 ) ) ;
#30826 = CARTESIAN_POINT ( 'NONE',  ( 6.013923656113508542, 9.173938811177871244, -1.199719254218452047 ) ) ;
#30827 = CARTESIAN_POINT ( 'NONE',  ( -7.279802135894939852, 7.457800344824362604, -0.7998128361456362523 ) ) ;
#30828 = CARTESIAN_POINT ( 'NONE',  ( 1.067063705314938771, -1.590654782179411031, 1.244411004956039291 ) ) ;
#30829 = DIRECTION ( 'NONE',  ( -1.276756478318932585E-15, 1.000000000000000000, -1.665334536937738262E-16 ) ) ;
#30830 = CARTESIAN_POINT ( 'NONE',  ( 4.542184868284099508, 0.9910628492805847456, -2.084066998532303483 ) ) ;
#30831 = CARTESIAN_POINT ( 'NONE',  ( 6.303176765056641706, -1.658072099422291057, 1.048360225930293321 ) ) ;
#30832 = CARTESIAN_POINT ( 'NONE',  ( 2.324987154519737143, -1.791562868964852395, -0.7996954790665599111 ) ) ;
#30833 = CARTESIAN_POINT ( 'NONE',  ( 8.062294901620731480, 12.55776115186623620, 1.040834085586084257E-14 ) ) ;
#30834 = CARTESIAN_POINT ( 'NONE',  ( 1.754679937794483280, 0.9610454613041006233, 1.302031786359980181 ) ) ;
#30835 = VERTEX_POINT ( 'NONE', #39736 ) ;
#30836 = CARTESIAN_POINT ( 'NONE',  ( 0.8841682305550628840, -2.117513412274423690, 0.006320426156874307463 ) ) ;
#30838 = CARTESIAN_POINT ( 'NONE',  ( -6.669721502918952716, 9.868759955792373972, 1.199719254218452047 ) ) ;
#30837 = CARTESIAN_POINT ( 'NONE',  ( -4.574986769607567894, 7.424902766929059261, 1.199719254218464037 ) ) ;
#30839 = CARTESIAN_POINT ( 'NONE',  ( 1.025062291269123405, -1.166378923895025510, -1.424538887614942739 ) ) ;
#30840 = VERTEX_POINT ( 'NONE', #105841 ) ;
#30841 = CARTESIAN_POINT ( 'NONE',  ( 4.575155497752975364, 1.982410897724752319, 0.8856408146403412784 ) ) ;
#30842 = CARTESIAN_POINT ( 'NONE',  ( 11.80883292463478185, 7.903546609398427236, -2.174370349999172891 ) ) ;
#30843 = CARTESIAN_POINT ( 'NONE',  ( 1.617596980227502756, 1.765956010477184535, 1.173731981927571555 ) ) ;
#30844 = CARTESIAN_POINT ( 'NONE',  ( 0.7499999999999885647, 3.347916667349487341, -1.299038105676658228 ) ) ;
#30845 = CARTESIAN_POINT ( 'NONE',  ( 7.618792255875527886, 10.97600916757510170, 1.199719254218460707 ) ) ;
#30846 = FILL_AREA_STYLE_COLOUR ( '', #91045 ) ;
#30847 = CARTESIAN_POINT ( 'NONE',  ( 3.022786435837477637, 1.939216523002813997, 0.6976457746366692136 ) ) ;
#30849 = CARTESIAN_POINT ( 'NONE',  ( 0.5910386730991653570, -0.6632029860377097741, 1.717849102829023922 ) ) ;
#30848 = CARTESIAN_POINT ( 'NONE',  ( -7.492852449846775897, 11.89341162479659531, 0.000000000000000000 ) ) ;
#30850 = CARTESIAN_POINT ( 'NONE',  ( -1.364683531249997417, 3.009375000341422801, 1.214306433183764966E-14 ) ) ;
#30851 = CARTESIAN_POINT ( 'NONE',  ( -0.02244404828160087226, 1.995160441984781041, -2.602654351998904492 ) ) ;
#30852 = CARTESIAN_POINT ( 'NONE',  ( 1.467608305004829194, 4.376302920305730204, -0.3199191423968851256 ) ) ;
#30853 =( GEOMETRIC_REPRESENTATION_CONTEXT ( 3 ) GLOBAL_UNCERTAINTY_ASSIGNED_CONTEXT ( ( #65884 ) ) GLOBAL_UNIT_ASSIGNED_CONTEXT ( ( #128836, #30195, #96284 ) ) REPRESENTATION_CONTEXT ( 'NONE', 'WORKASPACE' ) );
#30854 = CARTESIAN_POINT ( 'NONE',  ( 0.000000000000000000, 0.4999999999999998890, 10.24999999999999822 ) ) ;
#30855 = CARTESIAN_POINT ( 'NONE',  ( 1.827766392559232012, -2.130618655838847353, 0.7612957800654009954 ) ) ;
#30856 = CARTESIAN_POINT ( 'NONE',  ( -9.829298180227631576, 10.56986208646148384, 1.040834085586084257E-14 ) ) ;
#30857 = CARTESIAN_POINT ( 'NONE',  ( 3.005918303229858424, -0.7299923727487073188, 1.658169170237313583 ) ) ;
#30858 = CARTESIAN_POINT ( 'NONE',  ( 2.413182783470344983, -1.785834301256707723, 0.6938157933340273198 ) ) ;
#30859 = CARTESIAN_POINT ( 'NONE',  ( 3.596198176508007105, 0.9334358170956689182, -1.848091447891623051 ) ) ;
#30860 = CARTESIAN_POINT ( 'NONE',  ( -0.6823417656250212460, 1.113541667008083325, 1.181850606188755259 ) ) ;
#30861 = CARTESIAN_POINT ( 'NONE',  ( 1.832829291326312005, 0.1914625595707402927, 1.962137882790424559 ) ) ;
#30862 = CARTESIAN_POINT ( 'NONE',  ( 6.568979851886898480, -1.762530817088540758, -0.7781539781668064260 ) ) ;
#30863 = CARTESIAN_POINT ( 'NONE',  ( 2.922558825391399662, 1.760836971185793187, 0.6318509464167121337 ) ) ;
#30865 = CARTESIAN_POINT ( 'NONE',  ( 4.641000714467984345, 8.433135692799648808, 0.4354600853693716411 ) ) ;
#30864 = CARTESIAN_POINT ( 'NONE',  ( 0.8390048429645606820, 2.274487955075610301, 0.3892829850337137243 ) ) ;
#30866 = CARTESIAN_POINT ( 'NONE',  ( 2.295144308211858331, -1.664110045376477443, 0.8333370299275147941 ) ) ;
#30867 = CARTESIAN_POINT ( 'NONE',  ( -0.6823417656250212460, 3.551041667008085323, 1.181850606188767472 ) ) ;
#30868 = CARTESIAN_POINT ( 'NONE',  ( 5.617653825673187384, 0.4058615334493093085, -2.022196393678155957 ) ) ;
#30869 = CARTESIAN_POINT ( 'NONE',  ( -6.112028321662274166, 6.025121218227761588, 0.7998128361456341429 ) ) ;
#30870 = CARTESIAN_POINT ( 'NONE',  ( 6.479907352327590964, 9.647310113435821677, 1.199719254218462483 ) ) ;
#30871 = CARTESIAN_POINT ( 'NONE',  ( 10.85277107007934205, 3.956598013261175772, -3.932872935640606915 ) ) ;
#30872 = CARTESIAN_POINT ( 'NONE',  ( 6.510775453876758156, 1.563058401041140133, -1.411553977168745977 ) ) ;
#30873 = CARTESIAN_POINT ( 'NONE',  ( 1.364683531249988535, 2.967708333674755394, -0.7879004041258239610 ) ) ;
#30874 = CARTESIAN_POINT ( 'NONE',  ( 6.292270065666691892, -2.150519007954437622, -0.2187886337903441336 ) ) ;
#30875 = CARTESIAN_POINT ( 'NONE',  ( 0.6437974683802077935, 0.5340323341261629109, 1.762076181610471526 ) ) ;
#30876 = CARTESIAN_POINT ( 'NONE',  ( 5.320965550519270337, 1.527853097053995191, -1.320967980168601175 ) ) ;
#30877 = CARTESIAN_POINT ( 'NONE',  ( 1.364683531249988757, -0.3656249996585800299, 0.000000000000000000 ) ) ;
#30878 = CARTESIAN_POINT ( 'NONE',  ( -4.121315508874255684, 7.752025827087861920, -0.7216878364870267237 ) ) ;
#30881 = CARTESIAN_POINT ( 'NONE',  ( 4.609409038966229666, 6.400729850259146758, -1.443375672974051449 ) ) ;
#30880 = CARTESIAN_POINT ( 'NONE',  ( 3.285556943750000070, -0.6343749995220415716, 0.000000000000000000 ) ) ;
#30879 = CARTESIAN_POINT ( 'NONE',  ( 6.710359684120930091, 6.793450817754725257, 0.7998128361456352531 ) ) ;
#30882 = CARTESIAN_POINT ( 'NONE',  ( -4.197131071882288289, 7.054347462908075350, -1.199719254218455378 ) ) ;
#30883 = CARTESIAN_POINT ( 'NONE',  ( 4.979703994296570180, -0.7212954316567052881, 1.883311551353183511 ) ) ;
#30885 = B_SPLINE_CURVE_WITH_KNOTS ( 'NONE', 3,
 ( #17975, #3844, #50506, #82992 ),
 .UNSPECIFIED., .F., .F.,
 ( 4, 4 ),
 ( 5.198109377592358663E-17, 0.0001214485030784780796 ),
 .UNSPECIFIED. ) ;
#30884 = CARTESIAN_POINT ( 'NONE',  ( -7.985916173649233230, 9.275655943134292869, -1.199719254218446718 ) ) ;
#30887 = CARTESIAN_POINT ( 'NONE',  ( -6.061904078641520144, 10.08632216847484031, 0.7216878364870267237 ) ) ;
#30886 = CARTESIAN_POINT ( 'NONE',  ( -2.578021764892882040, 6.159442492350315490, 0.7998128361456341429 ) ) ;
#30888 = CARTESIAN_POINT ( 'NONE',  ( 1.364683531249990311, 5.363541667008086655, 0.7879004041258500513 ) ) ;
#30890 = CARTESIAN_POINT ( 'NONE',  ( -0.6823417656250003738, 9.651041667008065872, 1.181850606188754593 ) ) ;
#30889 = CARTESIAN_POINT ( 'NONE',  ( 5.489210439962995736, 1.908424935776025455, -1.015307555102950010 ) ) ;
#30891 = CARTESIAN_POINT ( 'NONE',  ( 5.346851039111033543, 6.199209027673978412, -1.009771797811720884 ) ) ;
#30892 = CARTESIAN_POINT ( 'NONE',  ( -11.77663116055808601, 7.701210053843842829, -2.069426955518140598 ) ) ;
#30893 = EDGE_CURVE ( 'NONE', #85328, #35153, #171868, .T. ) ;
#30895 = CARTESIAN_POINT ( 'NONE',  ( 5.976185453469534892, -2.006962702346287930, -0.1948244327795861652 ) ) ;
#30894 = CARTESIAN_POINT ( 'NONE',  ( -6.033015167956800262, 9.021972881716168402, -1.082531754730537976 ) ) ;
#30896 = CARTESIAN_POINT ( 'NONE',  ( 1.364683531249988757, -0.5531249996585801965, 0.000000000000000000 ) ) ;
#30897 = CARTESIAN_POINT ( 'NONE',  ( 2.191662871657253486, -0.7386692205221119245, 1.558845181661876467 ) ) ;
#30898 = CARTESIAN_POINT ( 'NONE',  ( 4.655245641445829641, 6.524482229810530498, 1.599625672291269396 ) ) ;
#30900 = CARTESIAN_POINT ( 'NONE',  ( 7.506374323821472849, 8.786466794993730289, -1.199719254218452047 ) ) ;
#30899 = CARTESIAN_POINT ( 'NONE',  ( 7.022760382198770301, 8.255937203062467589, -1.082531754730543083 ) ) ;
#30901 = CIRCLE ( 'NONE', #58555, 0.07999999999999998779 ) ;
#30902 = CARTESIAN_POINT ( 'NONE',  ( -11.81513045596701694, 8.669530242206672455, -2.119415056513991313 ) ) ;
#30903 = CARTESIAN_POINT ( 'NONE',  ( 6.919227945209173392, -0.1346273106918663420, 1.840389347376285345 ) ) ;
#30904 =( BOUNDED_SURFACE ( )  B_SPLINE_SURFACE ( 1, 2, ( 
 ( #137579, #207879, #205745, #125659, #204665, #190560, #203597, #124600, #71466, #188436, #23796, #7538, #191621, #90963, #43283, #174352, #107260, #22716, #171122, #109404, #6469, #8615, #58446, #40070, #187369, #92039, #108332, #75761, #55249, #139722, #25931, #56314, #72545, #88830, #57377, #155953, #73622, #9684, #153818, #74697, #123541, #121396, #106181, #138643, #172206, #89901, #189505, #38999, #41151, #173280, #24862, #140801, #206812, #141870, #208934, #146120, #192688, #96299, #160211, #210001, #45411, #77888, #176464, #126727, #63769, #212133, #193765, #147177, #145068, #213203, #144009, #129928, #76814, #195916, #10743, #61643, #177534, #161284, #64832, #30214, #130978, #113664, #46470, #28077, #44342, #196969, #11812, #162354, #47553, #127811, #110464, #31287, #179668, #14996, #142933, #78943, #97363, #111528, #29146, #94171, #211071, #95235, #12870, #163421, #48606, #13934, #62694, #180721, #128855, #194836, #112593, #178605, #80017, #60568, #81089, #114724, #93100, #159141, #132019, #136261, #148238, #85359, #198029, #35533, #99482, #149292, #199078, #17133, #115781, #65870, #3012, #151441, #133080, #32345, #164475, #200155, #19277, #69082, #53934, #66938, #181770, #86431, #1945, #135202, #49658, #4079, #152496, #50724, #34469, #201219, #873, #52860, #116849, #68007, #202281, #98411, #33403, #183921, #100540, #150375, #51809, #83209, #82146, #182850, #165540, #166615, #168742, #214240, #101609, #16062, #120070, #18205, #84289, #167676, #134147, #117927, #118993, #184972, #36597, #102684, #20345, #70150, #188185, #7285, #122225, #139468, #159696, #39820, #153571, #21396, #60058, #126213, #105928, #73362, #169807, #103758, #208424, #175962, #11295, #210569, #6219, #121153, #28635, #155704, #27557, #71216, #160765, #94722, #72288, #171952, #93653, #154638, #77374, #138396, #192175, #144559, #37681, #137333, #43836, #23541, #89650, #109952, #170877, #87507, #22469, #5140, #143489, #111013, #203349, #209486, #186046, #78439, #55002, #204414, #61127, #187118, #38750, #104832, #127287, #193258, #88580, #62203, #56068, #44905, #177018, #12360, #81639, #98971, #196467, #95790, #178091, #213741, #65364, #48109, #163977, #112090, #182324, #180220, #33953, #179157, #165023, #29709, #16617, #45969, #96860, #212693, #114221, #100028, #131511, #166091, #148779, #147724, #211626, #79511, #17679, #195406, #197514, #32893, #162908, #161847, #66422, #82698, #50215, #13435, #31842, #349, #30781, #47036, #145629, #97918, #130476, #15552, #132565, #83765, #49158, #115274, #1426, #14490, #113151, #80580, #146678, #64335, #63261, #181267, #129423, #198566, #116334, #149858, #128359, #194327, #120625, #167168, #54479, #55546, #118475, #52347, #171427, #70692, #68565, #136805, #67489, #18755, #84839, #23015, #202831, #134692, #186601, #133635, #150929, #2490, #71764, #170351, #137880, #200696, #36078, #184460, #69631, #151985, #102161, #38228, #168229, #104302, #185526, #19826, #199637, #21936, #39293, #155186, #89132, #51283, #85911, #135740, #169291, #88046, #3559, #201762, #117408, #183404, #154117, #35008, #53403, #5687, #203900, #121700, #187664, #105388, #101079, #119541, #86975, #37151, #103231, #20876, #153045, #4620, #124898, #6768, #75000, #91270, #7843, #11039, #140024, #58745, #206050, #90198, #60875, #159441, #73931, #191920, #41454, #190861, #141109, #175707, #176760, #110761, #57685, #27297, #42524, #107562, #108629, #123841, #93404, #174656, #77118, #143241, #72844, #28376, #209230, #127034, #172509, #207120, #56616, #44647, #26231, #8918, #92348, #208176, #189803, #173597, #24093, #25169, #204970, #157327, #158387, #142160, #9983, #76061, #59809, #125964, #94470, #43585, #138949, #109702, #122780, #192993, #188740, #40379, #106482, #156262, #46785, #82442, #61948, #78188, #164774, #33698, #144314, #210312, #213495, #147474, #148532, #211377, #145379, #16364, #113970, #64080, #160511, #14228, #30525, #161595, #99, #79262, #212438, #63003, #29454, #66165, #98715, #13184, #131273, #195151, #130223, #80323, #115021, #116076, #49957, #129174, #181018, #196217, #112899, #47858, #178910, #32638, #179967 ),
 ( #197261, #132310, #128107, #146424, #198317, #96605, #162657, #111837, #31589, #97664, #163722, #182066, #12114, #81390, #15302, #194065, #65117, #48901, #45718, #177840, #95544, #83509, #52091, #51026, #35827, #134442, #199379, #203639, #101905, #120363, #2234, #54225, #166913, #68311, #118218, #84586, #183151, #133374, #70436, #152786, #200445, #99775, #17426, #53153, #86717, #136552, #121440, #184204, #34754, #153862, #69376, #4366, #117147, #71510, #5431, #167970, #19576, #202573, #85649, #186338, #151736, #135484, #55290, #165840, #100828, #36891, #3306, #201506, #119282, #150673, #149592, #185268, #18507, #102973, #21678, #1176, #169031, #67240, #187409, #20628, #37973, #104046, #170092, #87788, #137622, #7580, #8659, #208975, #105125, #138688, #190600, #107300, #157070, #58487, #23835, #88872, #89942, #72587, #173324, #175450, #154926, #108371, #39040, #142974, #171165, #57420, #174394, #6511, #22754, #204705, #124643, #42258, #56355, #126770, #122518, #41193, #74738, #189545, #206855, #9726, #24902, #188481, #40111, #25972, #92078, #91008, #140843, #106222, #93142, #158135, #159179, #155993, #75801, #172248, #141909, #73665, #139764, #123582, #207921, #10780, #59541, #76855, #125702, #191661, #205790, #43325, #60611, #109443, #27034, #97406, #12911, #11851, #131020, #15041, #114765, #28116, #178646, #147219, #95279, #45452, #144049, #30257, #194878, #46514, #213244, #98454, #113708, #112637, #65913, #161327, #111568, #29189, #78991, #145107, #176504, #211113, #210045, #128897, #62737, #77929, #82188, #96343, #64874, #162398, #197012, #177576, #13974, #80061, #146162, #61684, #127853, #163461, #31329, #212177, #192728, #110504, #63812, #179712, #81133, #214280, #129972, #193803, #32389, #195959, #48648, #47593, #164519, #16104, #180762, #148281, #44382, #94210, #160250, #199118, #134182, #1981, #149334, #119028, #83249, #185010, #35567, #84328, #198070, #36637, #103794, #5179, #87539, #153608, #50761, #200191, #19318, #102721, #116891, #51844, #132060, #49698, #20383, #115826, #133119, #168778, #201254, #70185, #53969, #37716, #86467, #4116, #151480, #182890, #117963, #152531, #136297, #85394, #101648, #181813, #183957, #68045, #34507, #202319, #100580, #167715, #166653, #914, #186085, #120106, #18244, #169844, #150414, #3050, #69119, #21431, #33445, #99522, #135240, #165581, #52894, #17175, #66981, #56105, #25721, #107041, #75553, #9481, #71254, #92894, #91830, #141664, #22506, #139506, #121187, #109195, #40936, #73403, #205533, #58235, #122262, #188220, #88616, #39860, #55038, #138433, #204451, #206606, #155741, #140595, #74489, #105969, #26789, #171991, #175207, #23583, #158939, #108121, #137368, #191415, #89690, #203385, #7326, #207675, #187156, #38785, #59294, #104866, #170911, #154671, #124392, #190350, #125453, #57170, #123332, #6256, #42012, #72327, #174148, #189296, #173068, #24649, #43082, #157889, #90756, #156817, #8404, #194625, #45207, #62494, #209796, #179461, #46268, #14795, #163213, #10535, #32135, #31085, #80886, #176264, #78738, #60358, #48408, #112385, #12664, #144862, #211932, #61431, #127598, #27865, #193564, #208731, #77678, #143799, #145920, #95023, #79808, #13735, #111321, #180515, #177325, #114520, #28939, #98216, #47342, #76608, #130770, #161073, #142722, #210869, #146976, #126521, #192482, #212993, #44134, #110255, #93962, #63566, #129723, #64631, #128659, #178397, #160003, #195707, #11604, #113456, #30009, #96093, #162148, #196765, #97158, #168523, #165323, #132860, #16917, #166390, #34250, #181564, #151223, #115568, #2792, #67784, #116633, #15856, #68863, #136036, #37451, #119842, #185820, #82997, #17981, #51587, #134982, #149073, #84070, #164267, #81942, #52638, #148026, #650, #200992, #19058, #102457, #86207, #69924, #118766, #36379, #183702, #66716, #150159, #184751, #20121, #117711, #133934, #214036, #1727, #100323, #198864, #152278, #50511, #199939, #182628, #33192, #3851, #202049, #35310, #53709, #101387, #167462, #85136, #65661, #131809, #197818, #49449, #99275, #189038, #40676, #23318, #139237, #87274, #157624, #155477, #9221, #154413, #140327, #153342, #74234 ) ),
 .UNSPECIFIED., .F., .F., .T. ) 
 B_SPLINE_SURFACE_WITH_KNOTS ( ( 2, 2 ),
 ( 3, 2, 2, 2, 2, 2, 2, 2, 2, 2, 2, 2, 2, 2, 2, 2, 2, 2, 2, 2, 2, 2, 2, 2, 2, 2, 2, 2, 2, 2, 2, 2, 2, 2, 2, 2, 2, 2, 2, 2, 2, 2, 2, 2, 2, 2, 2, 2, 2, 2, 2, 2, 2, 2, 2, 2, 2, 2, 2, 2, 2, 2, 2, 2, 2, 2, 2, 2, 2, 2, 2, 2, 2, 2, 2, 2, 2, 2, 2, 2, 2, 2, 2, 2, 2, 2, 2, 2, 2, 2, 2, 2, 2, 2, 2, 2, 2, 2, 2, 2, 2, 2, 2, 2, 2, 2, 2, 2, 2, 2, 2, 2, 2, 2, 2, 2, 2, 2, 2, 2, 2, 2, 2, 2, 2, 2, 2, 2, 2, 2, 2, 2, 2, 2, 2, 2, 2, 2, 2, 2, 2, 2, 2, 2, 2, 2, 2, 2, 2, 2, 2, 2, 2, 2, 2, 2, 2, 2, 2, 2, 2, 2, 2, 2, 2, 2, 2, 2, 2, 2, 2, 2, 2, 2, 2, 2, 2, 2, 2, 2, 2, 2, 2, 2, 2, 2, 2, 2, 2, 2, 2, 2, 2, 2, 2, 2, 2, 2, 2, 2, 2, 2, 2, 2, 2, 2, 2, 2, 2, 2, 2, 2, 2, 2, 2, 2, 2, 2, 2, 2, 2, 2, 2, 2, 2, 2, 2, 2, 2, 2, 2, 2, 2, 2, 2, 2, 2, 2, 2, 2, 3 ),
 ( 0.000000000000000000, 1.000000000000000000 ),
 ( 0.000000000000000000, 0.004166666666666666609, 0.008333333333333333218, 0.01250000000000000069, 0.01666666666666666644, 0.02083333333333333218, 0.02500000000000000139, 0.02916666666666666713, 0.03333333333333333287, 0.03749999999999999861, 0.04166666666666666435, 0.04583333333333333010, 0.05000000000000000278, 0.05416666666666666852, 0.05833333333333333426, 0.06250000000000000000, 0.06666666666666666574, 0.07083333333333333148, 0.07499999999999999722, 0.07916666666666666297, 0.08333333333333332871, 0.08749999999999999445, 0.09166666666666666019, 0.09583333333333333981, 0.1000000000000000056, 0.1041666666666666713, 0.1083333333333333370, 0.1125000000000000028, 0.1166666666666666685, 0.1208333333333333343, 0.1250000000000000000, 0.1291666666666666796, 0.1333333333333333315, 0.1375000000000000111, 0.1416666666666666630, 0.1458333333333333426, 0.1499999999999999944, 0.1541666666666666741, 0.1583333333333333259, 0.1625000000000000056, 0.1666666666666666574, 0.1708333333333333370, 0.1749999999999999889, 0.1791666666666666685, 0.1833333333333333204, 0.1875000000000000000, 0.1916666666666666796, 0.1958333333333333315, 0.2000000000000000111, 0.2041666666666666630, 0.2083333333333333426, 0.2124999999999999944, 0.2166666666666666741, 0.2208333333333333259, 0.2250000000000000056, 0.2291666666666666574, 0.2333333333333333370, 0.2374999999999999889, 0.2416666666666666685, 0.2458333333333333204, 0.2500000000000000000, 0.2541666666666666519, 0.2583333333333333592, 0.2625000000000000111, 0.2666666666666666630, 0.2708333333333333148, 0.2750000000000000222, 0.2791666666666666741, 0.2833333333333333259, 0.2874999999999999778, 0.2916666666666666852, 0.2958333333333333370, 0.2999999999999999889, 0.3041666666666666408, 0.3083333333333333481, 0.3125000000000000000, 0.3166666666666666519, 0.3208333333333333592, 0.3250000000000000111, 0.3291666666666666630, 0.3333333333333333148, 0.3375000000000000222, 0.3416666666666666741, 0.3458333333333333259, 0.3499999999999999778, 0.3541666666666666852, 0.3583333333333333370, 0.3624999999999999889, 0.3666666666666666408, 0.3708333333333333481, 0.3750000000000000000, 0.3791666666666666519, 0.3833333333333333592, 0.3875000000000000111, 0.3916666666666666630, 0.3958333333333333148, 0.4000000000000000222, 0.4041666666666666741, 0.4083333333333333259, 0.4124999999999999778, 0.4166666666666666852, 0.4208333333333333370, 0.4249999999999999889, 0.4291666666666666408, 0.4333333333333333481, 0.4375000000000000000, 0.4416666666666666519, 0.4458333333333333592, 0.4500000000000000111, 0.4541666666666666630, 0.4583333333333333148, 0.4625000000000000222, 0.4666666666666666741, 0.4708333333333333259, 0.4749999999999999778, 0.4791666666666666852, 0.4833333333333333370, 0.4874999999999999889, 0.4916666666666666408, 0.4958333333333333481, 0.5000000000000000000, 0.5041666666666666519, 0.5083333333333333037, 0.5124999999999999556, 0.5166666666666667185, 0.5208333333333333703, 0.5250000000000000222, 0.5291666666666666741, 0.5333333333333333259, 0.5374999999999999778, 0.5416666666666666297, 0.5458333333333332815, 0.5500000000000000444, 0.5541666666666666963, 0.5583333333333333481, 0.5625000000000000000, 0.5666666666666666519, 0.5708333333333333037, 0.5749999999999999556, 0.5791666666666667185, 0.5833333333333333703, 0.5875000000000000222, 0.5916666666666666741, 0.5958333333333333259, 0.5999999999999999778, 0.6041666666666666297, 0.6083333333333332815, 0.6125000000000000444, 0.6166666666666666963, 0.6208333333333333481, 0.6250000000000000000, 0.6291666666666666519, 0.6333333333333333037, 0.6374999999999999556, 0.6416666666666667185, 0.6458333333333333703, 0.6500000000000000222, 0.6541666666666666741, 0.6583333333333333259, 0.6624999999999999778, 0.6666666666666666297, 0.6708333333333332815, 0.6750000000000000444, 0.6791666666666666963, 0.6833333333333333481, 0.6875000000000000000, 0.6916666666666666519, 0.6958333333333333037, 0.6999999999999999556, 0.7041666666666667185, 0.7083333333333333703, 0.7125000000000000222, 0.7166666666666666741, 0.7208333333333333259, 0.7249999999999999778, 0.7291666666666666297, 0.7333333333333332815, 0.7375000000000000444, 0.7416666666666666963, 0.7458333333333333481, 0.7500000000000000000, 0.7541666666666666519, 0.7583333333333333037, 0.7624999999999999556, 0.7666666666666667185, 0.7708333333333333703, 0.7750000000000000222, 0.7791666666666666741, 0.7833333333333333259, 0.7874999999999999778, 0.7916666666666666297, 0.7958333333333332815, 0.8000000000000000444, 0.8041666666666666963, 0.8083333333333333481, 0.8125000000000000000, 0.8166666666666666519, 0.8208333333333333037, 0.8249999999999999556, 0.8291666666666667185, 0.8333333333333333703, 0.8375000000000000222, 0.8416666666666666741, 0.8458333333333333259, 0.8499999999999999778, 0.8541666666666666297, 0.8583333333333332815, 0.8625000000000000444, 0.8666666666666666963, 0.8708333333333333481, 0.8750000000000000000, 0.8791666666666666519, 0.8833333333333333037, 0.8874999999999999556, 0.8916666666666667185, 0.8958333333333333703, 0.9000000000000000222, 0.9041666666666666741, 0.9083333333333333259, 0.9124999999999999778, 0.9166666666666666297, 0.9208333333333332815, 0.9250000000000000444, 0.9291666666666666963, 0.9333333333333333481, 0.9375000000000000000, 0.9416666666666666519, 0.9458333333333333037, 0.9499999999999999556, 0.9541666666666667185, 0.9583333333333333703, 0.9625000000000000222, 0.9666666666666666741, 0.9708333333333333259, 0.9749999999999999778, 0.9791666666666666297, 0.9833333333333332815, 0.9875000000000000444, 0.9916666666666666963, 0.9958333333333333481, 1.000000000000000000 ),
 .UNSPECIFIED. ) 
 GEOMETRIC_REPRESENTATION_ITEM ( )  RATIONAL_B_SPLINE_SURFACE ( (
 ( 1.000000000000000000, 0.8660254037844387076, 1.000000000000000000, 0.8660254037844387076, 1.000000000000000000, 0.8660254037844387076, 1.000000000000000000, 0.8660254037844387076, 1.000000000000000000, 0.8660254037844387076, 1.000000000000000000, 0.8660254037844387076, 1.000000000000000000, 0.8660254037844387076, 1.000000000000000000, 0.8660254037844387076, 1.000000000000000000, 0.8660254037844387076, 1.000000000000000000, 0.8660254037844387076, 1.000000000000000000, 0.8660254037844387076, 1.000000000000000000, 0.8660254037844387076, 1.000000000000000000, 0.8660254037844387076, 1.000000000000000000, 0.8660254037844387076, 1.000000000000000000, 0.8660254037844387076, 1.000000000000000000, 0.8660254037844387076, 1.000000000000000000, 0.8660254037844387076, 1.000000000000000000, 0.8660254037844387076, 1.000000000000000000, 0.8660254037844387076, 1.000000000000000000, 0.8660254037844387076, 1.000000000000000000, 0.8660254037844387076, 1.000000000000000000, 0.8660254037844387076, 1.000000000000000000, 0.8660254037844387076, 1.000000000000000000, 0.8660254037844387076, 1.000000000000000000, 0.8660254037844387076, 1.000000000000000000, 0.8660254037844387076, 1.000000000000000000, 0.8660254037844387076, 1.000000000000000000, 0.8660254037844387076, 1.000000000000000000, 0.8660254037844387076, 1.000000000000000000, 0.8660254037844387076, 1.000000000000000000, 0.8660254037844387076, 1.000000000000000000, 0.8660254037844387076, 1.000000000000000000, 0.8660254037844387076, 1.000000000000000000, 0.8660254037844387076, 1.000000000000000000, 0.8660254037844387076, 1.000000000000000000, 0.8660254037844387076, 1.000000000000000000, 0.8660254037844387076, 1.000000000000000000, 0.8660254037844387076, 1.000000000000000000, 0.8660254037844387076, 1.000000000000000000, 0.8660254037844387076, 1.000000000000000000, 0.8660254037844387076, 1.000000000000000000, 0.8660254037844387076, 1.000000000000000000, 0.8660254037844387076, 1.000000000000000000, 0.8660254037844387076, 1.000000000000000000, 0.8660254037844387076, 1.000000000000000000, 0.8660254037844387076, 1.000000000000000000, 0.8660254037844387076, 1.000000000000000000, 0.8660254037844387076, 1.000000000000000000, 0.8660254037844387076, 1.000000000000000000, 0.8660254037844387076, 1.000000000000000000, 0.8660254037844387076, 1.000000000000000000, 0.8660254037844387076, 1.000000000000000000, 0.8660254037844387076, 1.000000000000000000, 0.8660254037844387076, 1.000000000000000000, 0.8660254037844387076, 1.000000000000000000, 0.8660254037844387076, 1.000000000000000000, 0.8660254037844387076, 1.000000000000000000, 0.8660254037844387076, 1.000000000000000000, 0.8660254037844387076, 1.000000000000000000, 0.8660254037844387076, 1.000000000000000000, 0.8660254037844387076, 1.000000000000000000, 0.8660254037844387076, 1.000000000000000000, 0.8660254037844387076, 1.000000000000000000, 0.8660254037844387076, 1.000000000000000000, 0.8660254037844387076, 1.000000000000000000, 0.8660254037844387076, 1.000000000000000000, 0.8660254037844387076, 1.000000000000000000, 0.8660254037844387076, 1.000000000000000000, 0.8660254037844387076, 1.000000000000000000, 0.8660254037844387076, 1.000000000000000000, 0.8660254037844387076, 1.000000000000000000, 0.8660254037844387076, 1.000000000000000000, 0.8660254037844387076, 1.000000000000000000, 0.8660254037844387076, 1.000000000000000000, 0.8660254037844387076, 1.000000000000000000, 0.8660254037844387076, 1.000000000000000000, 0.8660254037844387076, 1.000000000000000000, 0.8660254037844387076, 1.000000000000000000, 0.8660254037844387076, 1.000000000000000000, 0.8660254037844387076, 1.000000000000000000, 0.8660254037844387076, 1.000000000000000000, 0.8660254037844387076, 1.000000000000000000, 0.8660254037844387076, 1.000000000000000000, 0.8660254037844387076, 1.000000000000000000, 0.8660254037844387076, 1.000000000000000000, 0.8660254037844387076, 1.000000000000000000, 0.8660254037844387076, 1.000000000000000000, 0.8660254037844387076, 1.000000000000000000, 0.8660254037844387076, 1.000000000000000000, 0.8660254037844387076, 1.000000000000000000, 0.8660254037844387076, 1.000000000000000000, 0.8660254037844387076, 1.000000000000000000, 0.8660254037844387076, 1.000000000000000000, 0.8660254037844387076, 1.000000000000000000, 0.8660254037844387076, 1.000000000000000000, 0.8660254037844387076, 1.000000000000000000, 0.8660254037844387076, 1.000000000000000000, 0.8660254037844387076, 1.000000000000000000, 0.8660254037844387076, 1.000000000000000000, 0.8660254037844387076, 1.000000000000000000, 0.8660254037844387076, 1.000000000000000000, 0.8660254037844387076, 1.000000000000000000, 0.8660254037844387076, 1.000000000000000000, 0.8660254037844387076, 1.000000000000000000, 0.8660254037844387076, 1.000000000000000000, 0.8660254037844387076, 1.000000000000000000, 0.8660254037844387076, 1.000000000000000000, 0.8660254037844387076, 1.000000000000000000, 0.8660254037844387076, 1.000000000000000000, 0.8660254037844387076, 1.000000000000000000, 0.8660254037844387076, 1.000000000000000000, 0.8660254037844387076, 1.000000000000000000, 0.8660254037844387076, 1.000000000000000000, 0.8660254037844387076, 1.000000000000000000, 0.8660254037844387076, 1.000000000000000000, 0.8660254037844387076, 1.000000000000000000, 0.8660254037844387076, 1.000000000000000000, 0.8660254037844387076, 1.000000000000000000, 0.8660254037844387076, 1.000000000000000000, 0.8660254037844387076, 1.000000000000000000, 0.8660254037844387076, 1.000000000000000000, 0.8660254037844387076, 1.000000000000000000, 0.8660254037844387076, 1.000000000000000000, 0.8660254037844387076, 1.000000000000000000, 0.8660254037844387076, 1.000000000000000000, 0.8660254037844387076, 1.000000000000000000, 0.8660254037844387076, 1.000000000000000000, 0.8660254037844387076, 1.000000000000000000, 0.8660254037844387076, 1.000000000000000000, 0.8660254037844387076, 1.000000000000000000, 0.8660254037844387076, 1.000000000000000000, 0.8660254037844387076, 1.000000000000000000, 0.8660254037844387076, 1.000000000000000000, 0.8660254037844387076, 1.000000000000000000, 0.8660254037844387076, 1.000000000000000000, 0.8660254037844387076, 1.000000000000000000, 0.8660254037844387076, 1.000000000000000000, 0.8660254037844387076, 1.000000000000000000, 0.8660254037844387076, 1.000000000000000000, 0.8660254037844387076, 1.000000000000000000, 0.8660254037844387076, 1.000000000000000000, 0.8660254037844387076, 1.000000000000000000, 0.8660254037844387076, 1.000000000000000000, 0.8660254037844387076, 1.000000000000000000, 0.8660254037844387076, 1.000000000000000000, 0.8660254037844387076, 1.000000000000000000, 0.8660254037844387076, 1.000000000000000000, 0.8660254037844387076, 1.000000000000000000, 0.8660254037844387076, 1.000000000000000000, 0.8660254037844387076, 1.000000000000000000, 0.8660254037844387076, 1.000000000000000000, 0.8660254037844387076, 1.000000000000000000, 0.8660254037844387076, 1.000000000000000000, 0.8660254037844387076, 1.000000000000000000, 0.8660254037844387076, 1.000000000000000000, 0.8660254037844387076, 1.000000000000000000, 0.8660254037844387076, 1.000000000000000000, 0.8660254037844387076, 1.000000000000000000, 0.8660254037844387076, 1.000000000000000000, 0.8660254037844387076, 1.000000000000000000, 0.8660254037844387076, 1.000000000000000000, 0.8660254037844387076, 1.000000000000000000, 0.8660254037844387076, 1.000000000000000000, 0.8660254037844387076, 1.000000000000000000, 0.8660254037844387076, 1.000000000000000000, 0.8660254037844387076, 1.000000000000000000, 0.8660254037844387076, 1.000000000000000000, 0.8660254037844387076, 1.000000000000000000, 0.8660254037844387076, 1.000000000000000000, 0.8660254037844387076, 1.000000000000000000, 0.8660254037844387076, 1.000000000000000000, 0.8660254037844387076, 1.000000000000000000, 0.8660254037844387076, 1.000000000000000000, 0.8660254037844387076, 1.000000000000000000, 0.8660254037844387076, 1.000000000000000000, 0.8660254037844387076, 1.000000000000000000, 0.8660254037844387076, 1.000000000000000000, 0.8660254037844387076, 1.000000000000000000, 0.8660254037844387076, 1.000000000000000000, 0.8660254037844387076, 1.000000000000000000, 0.8660254037844387076, 1.000000000000000000, 0.8660254037844387076, 1.000000000000000000, 0.8660254037844387076, 1.000000000000000000, 0.8660254037844387076, 1.000000000000000000, 0.8660254037844387076, 1.000000000000000000, 0.8660254037844387076, 1.000000000000000000, 0.8660254037844387076, 1.000000000000000000, 0.8660254037844387076, 1.000000000000000000, 0.8660254037844387076, 1.000000000000000000, 0.8660254037844387076, 1.000000000000000000, 0.8660254037844387076, 1.000000000000000000, 0.8660254037844387076, 1.000000000000000000, 0.8660254037844387076, 1.000000000000000000, 0.8660254037844387076, 1.000000000000000000, 0.8660254037844387076, 1.000000000000000000, 0.8660254037844387076, 1.000000000000000000, 0.8660254037844387076, 1.000000000000000000, 0.8660254037844387076, 1.000000000000000000, 0.8660254037844387076, 1.000000000000000000, 0.8660254037844387076, 1.000000000000000000, 0.8660254037844387076, 1.000000000000000000, 0.8660254037844387076, 1.000000000000000000, 0.8660254037844387076, 1.000000000000000000, 0.8660254037844387076, 1.000000000000000000, 0.8660254037844387076, 1.000000000000000000, 0.8660254037844387076, 1.000000000000000000, 0.8660254037844387076, 1.000000000000000000, 0.8660254037844387076, 1.000000000000000000, 0.8660254037844387076, 1.000000000000000000, 0.8660254037844387076, 1.000000000000000000, 0.8660254037844387076, 1.000000000000000000, 0.8660254037844387076, 1.000000000000000000, 0.8660254037844387076, 1.000000000000000000, 0.8660254037844387076, 1.000000000000000000, 0.8660254037844387076, 1.000000000000000000, 0.8660254037844387076, 1.000000000000000000, 0.8660254037844387076, 1.000000000000000000, 0.8660254037844387076, 1.000000000000000000, 0.8660254037844387076, 1.000000000000000000, 0.8660254037844387076, 1.000000000000000000, 0.8660254037844387076, 1.000000000000000000, 0.8660254037844387076, 1.000000000000000000, 0.8660254037844387076, 1.000000000000000000, 0.8660254037844387076, 1.000000000000000000, 0.8660254037844387076, 1.000000000000000000, 0.8660254037844387076, 1.000000000000000000, 0.8660254037844387076, 1.000000000000000000, 0.8660254037844387076, 1.000000000000000000, 0.8660254037844387076, 1.000000000000000000, 0.8660254037844387076, 1.000000000000000000, 0.8660254037844387076, 1.000000000000000000, 0.8660254037844387076, 1.000000000000000000, 0.8660254037844387076, 1.000000000000000000, 0.8660254037844387076, 1.000000000000000000, 0.8660254037844387076, 1.000000000000000000, 0.8660254037844387076, 1.000000000000000000, 0.8660254037844387076, 1.000000000000000000, 0.8660254037844387076, 1.000000000000000000, 0.8660254037844387076, 1.000000000000000000, 0.8660254037844387076, 1.000000000000000000),
 ( 1.000000000000000000, 0.8660254037844387076, 1.000000000000000000, 0.8660254037844387076, 1.000000000000000000, 0.8660254037844387076, 1.000000000000000000, 0.8660254037844387076, 1.000000000000000000, 0.8660254037844387076, 1.000000000000000000, 0.8660254037844387076, 1.000000000000000000, 0.8660254037844387076, 1.000000000000000000, 0.8660254037844387076, 1.000000000000000000, 0.8660254037844387076, 1.000000000000000000, 0.8660254037844387076, 1.000000000000000000, 0.8660254037844387076, 1.000000000000000000, 0.8660254037844387076, 1.000000000000000000, 0.8660254037844387076, 1.000000000000000000, 0.8660254037844387076, 1.000000000000000000, 0.8660254037844387076, 1.000000000000000000, 0.8660254037844387076, 1.000000000000000000, 0.8660254037844387076, 1.000000000000000000, 0.8660254037844387076, 1.000000000000000000, 0.8660254037844387076, 1.000000000000000000, 0.8660254037844387076, 1.000000000000000000, 0.8660254037844387076, 1.000000000000000000, 0.8660254037844387076, 1.000000000000000000, 0.8660254037844387076, 1.000000000000000000, 0.8660254037844387076, 1.000000000000000000, 0.8660254037844387076, 1.000000000000000000, 0.8660254037844387076, 1.000000000000000000, 0.8660254037844387076, 1.000000000000000000, 0.8660254037844387076, 1.000000000000000000, 0.8660254037844387076, 1.000000000000000000, 0.8660254037844387076, 1.000000000000000000, 0.8660254037844387076, 1.000000000000000000, 0.8660254037844387076, 1.000000000000000000, 0.8660254037844387076, 1.000000000000000000, 0.8660254037844387076, 1.000000000000000000, 0.8660254037844387076, 1.000000000000000000, 0.8660254037844387076, 1.000000000000000000, 0.8660254037844387076, 1.000000000000000000, 0.8660254037844387076, 1.000000000000000000, 0.8660254037844387076, 1.000000000000000000, 0.8660254037844387076, 1.000000000000000000, 0.8660254037844387076, 1.000000000000000000, 0.8660254037844387076, 1.000000000000000000, 0.8660254037844387076, 1.000000000000000000, 0.8660254037844387076, 1.000000000000000000, 0.8660254037844387076, 1.000000000000000000, 0.8660254037844387076, 1.000000000000000000, 0.8660254037844387076, 1.000000000000000000, 0.8660254037844387076, 1.000000000000000000, 0.8660254037844387076, 1.000000000000000000, 0.8660254037844387076, 1.000000000000000000, 0.8660254037844387076, 1.000000000000000000, 0.8660254037844387076, 1.000000000000000000, 0.8660254037844387076, 1.000000000000000000, 0.8660254037844387076, 1.000000000000000000, 0.8660254037844387076, 1.000000000000000000, 0.8660254037844387076, 1.000000000000000000, 0.8660254037844387076, 1.000000000000000000, 0.8660254037844387076, 1.000000000000000000, 0.8660254037844387076, 1.000000000000000000, 0.8660254037844387076, 1.000000000000000000, 0.8660254037844387076, 1.000000000000000000, 0.8660254037844387076, 1.000000000000000000, 0.8660254037844387076, 1.000000000000000000, 0.8660254037844387076, 1.000000000000000000, 0.8660254037844387076, 1.000000000000000000, 0.8660254037844387076, 1.000000000000000000, 0.8660254037844387076, 1.000000000000000000, 0.8660254037844387076, 1.000000000000000000, 0.8660254037844387076, 1.000000000000000000, 0.8660254037844387076, 1.000000000000000000, 0.8660254037844387076, 1.000000000000000000, 0.8660254037844387076, 1.000000000000000000, 0.8660254037844387076, 1.000000000000000000, 0.8660254037844387076, 1.000000000000000000, 0.8660254037844387076, 1.000000000000000000, 0.8660254037844387076, 1.000000000000000000, 0.8660254037844387076, 1.000000000000000000, 0.8660254037844387076, 1.000000000000000000, 0.8660254037844387076, 1.000000000000000000, 0.8660254037844387076, 1.000000000000000000, 0.8660254037844387076, 1.000000000000000000, 0.8660254037844387076, 1.000000000000000000, 0.8660254037844387076, 1.000000000000000000, 0.8660254037844387076, 1.000000000000000000, 0.8660254037844387076, 1.000000000000000000, 0.8660254037844387076, 1.000000000000000000, 0.8660254037844387076, 1.000000000000000000, 0.8660254037844387076, 1.000000000000000000, 0.8660254037844387076, 1.000000000000000000, 0.8660254037844387076, 1.000000000000000000, 0.8660254037844387076, 1.000000000000000000, 0.8660254037844387076, 1.000000000000000000, 0.8660254037844387076, 1.000000000000000000, 0.8660254037844387076, 1.000000000000000000, 0.8660254037844387076, 1.000000000000000000, 0.8660254037844387076, 1.000000000000000000, 0.8660254037844387076, 1.000000000000000000, 0.8660254037844387076, 1.000000000000000000, 0.8660254037844387076, 1.000000000000000000, 0.8660254037844387076, 1.000000000000000000, 0.8660254037844387076, 1.000000000000000000, 0.8660254037844387076, 1.000000000000000000, 0.8660254037844387076, 1.000000000000000000, 0.8660254037844387076, 1.000000000000000000, 0.8660254037844387076, 1.000000000000000000, 0.8660254037844387076, 1.000000000000000000, 0.8660254037844387076, 1.000000000000000000, 0.8660254037844387076, 1.000000000000000000, 0.8660254037844387076, 1.000000000000000000, 0.8660254037844387076, 1.000000000000000000, 0.8660254037844387076, 1.000000000000000000, 0.8660254037844387076, 1.000000000000000000, 0.8660254037844387076, 1.000000000000000000, 0.8660254037844387076, 1.000000000000000000, 0.8660254037844387076, 1.000000000000000000, 0.8660254037844387076, 1.000000000000000000, 0.8660254037844387076, 1.000000000000000000, 0.8660254037844387076, 1.000000000000000000, 0.8660254037844387076, 1.000000000000000000, 0.8660254037844387076, 1.000000000000000000, 0.8660254037844387076, 1.000000000000000000, 0.8660254037844387076, 1.000000000000000000, 0.8660254037844387076, 1.000000000000000000, 0.8660254037844387076, 1.000000000000000000, 0.8660254037844387076, 1.000000000000000000, 0.8660254037844387076, 1.000000000000000000, 0.8660254037844387076, 1.000000000000000000, 0.8660254037844387076, 1.000000000000000000, 0.8660254037844387076, 1.000000000000000000, 0.8660254037844387076, 1.000000000000000000, 0.8660254037844387076, 1.000000000000000000, 0.8660254037844387076, 1.000000000000000000, 0.8660254037844387076, 1.000000000000000000, 0.8660254037844387076, 1.000000000000000000, 0.8660254037844387076, 1.000000000000000000, 0.8660254037844387076, 1.000000000000000000, 0.8660254037844387076, 1.000000000000000000, 0.8660254037844387076, 1.000000000000000000, 0.8660254037844387076, 1.000000000000000000, 0.8660254037844387076, 1.000000000000000000, 0.8660254037844387076, 1.000000000000000000, 0.8660254037844387076, 1.000000000000000000, 0.8660254037844387076, 1.000000000000000000, 0.8660254037844387076, 1.000000000000000000, 0.8660254037844387076, 1.000000000000000000, 0.8660254037844387076, 1.000000000000000000, 0.8660254037844387076, 1.000000000000000000, 0.8660254037844387076, 1.000000000000000000, 0.8660254037844387076, 1.000000000000000000, 0.8660254037844387076, 1.000000000000000000, 0.8660254037844387076, 1.000000000000000000, 0.8660254037844387076, 1.000000000000000000, 0.8660254037844387076, 1.000000000000000000, 0.8660254037844387076, 1.000000000000000000, 0.8660254037844387076, 1.000000000000000000, 0.8660254037844387076, 1.000000000000000000, 0.8660254037844387076, 1.000000000000000000, 0.8660254037844387076, 1.000000000000000000, 0.8660254037844387076, 1.000000000000000000, 0.8660254037844387076, 1.000000000000000000, 0.8660254037844387076, 1.000000000000000000, 0.8660254037844387076, 1.000000000000000000, 0.8660254037844387076, 1.000000000000000000, 0.8660254037844387076, 1.000000000000000000, 0.8660254037844387076, 1.000000000000000000, 0.8660254037844387076, 1.000000000000000000, 0.8660254037844387076, 1.000000000000000000, 0.8660254037844387076, 1.000000000000000000, 0.8660254037844387076, 1.000000000000000000, 0.8660254037844387076, 1.000000000000000000, 0.8660254037844387076, 1.000000000000000000, 0.8660254037844387076, 1.000000000000000000, 0.8660254037844387076, 1.000000000000000000, 0.8660254037844387076, 1.000000000000000000, 0.8660254037844387076, 1.000000000000000000, 0.8660254037844387076, 1.000000000000000000, 0.8660254037844387076, 1.000000000000000000, 0.8660254037844387076, 1.000000000000000000, 0.8660254037844387076, 1.000000000000000000, 0.8660254037844387076, 1.000000000000000000, 0.8660254037844387076, 1.000000000000000000, 0.8660254037844387076, 1.000000000000000000, 0.8660254037844387076, 1.000000000000000000, 0.8660254037844387076, 1.000000000000000000, 0.8660254037844387076, 1.000000000000000000, 0.8660254037844387076, 1.000000000000000000, 0.8660254037844387076, 1.000000000000000000, 0.8660254037844387076, 1.000000000000000000, 0.8660254037844387076, 1.000000000000000000, 0.8660254037844387076, 1.000000000000000000, 0.8660254037844387076, 1.000000000000000000, 0.8660254037844387076, 1.000000000000000000, 0.8660254037844387076, 1.000000000000000000, 0.8660254037844387076, 1.000000000000000000, 0.8660254037844387076, 1.000000000000000000, 0.8660254037844387076, 1.000000000000000000, 0.8660254037844387076, 1.000000000000000000, 0.8660254037844387076, 1.000000000000000000, 0.8660254037844387076, 1.000000000000000000, 0.8660254037844387076, 1.000000000000000000, 0.8660254037844387076, 1.000000000000000000, 0.8660254037844387076, 1.000000000000000000, 0.8660254037844387076, 1.000000000000000000, 0.8660254037844387076, 1.000000000000000000, 0.8660254037844387076, 1.000000000000000000, 0.8660254037844387076, 1.000000000000000000, 0.8660254037844387076, 1.000000000000000000, 0.8660254037844387076, 1.000000000000000000, 0.8660254037844387076, 1.000000000000000000, 0.8660254037844387076, 1.000000000000000000, 0.8660254037844387076, 1.000000000000000000, 0.8660254037844387076, 1.000000000000000000, 0.8660254037844387076, 1.000000000000000000, 0.8660254037844387076, 1.000000000000000000, 0.8660254037844387076, 1.000000000000000000, 0.8660254037844387076, 1.000000000000000000, 0.8660254037844387076, 1.000000000000000000, 0.8660254037844387076, 1.000000000000000000, 0.8660254037844387076, 1.000000000000000000, 0.8660254037844387076, 1.000000000000000000, 0.8660254037844387076, 1.000000000000000000, 0.8660254037844387076, 1.000000000000000000, 0.8660254037844387076, 1.000000000000000000, 0.8660254037844387076, 1.000000000000000000, 0.8660254037844387076, 1.000000000000000000, 0.8660254037844387076, 1.000000000000000000, 0.8660254037844387076, 1.000000000000000000, 0.8660254037844387076, 1.000000000000000000, 0.8660254037844387076, 1.000000000000000000, 0.8660254037844387076, 1.000000000000000000, 0.8660254037844387076, 1.000000000000000000, 0.8660254037844387076, 1.000000000000000000, 0.8660254037844387076, 1.000000000000000000, 0.8660254037844387076, 1.000000000000000000, 0.8660254037844387076, 1.000000000000000000, 0.8660254037844387076, 1.000000000000000000, 0.8660254037844387076, 1.000000000000000000, 0.8660254037844387076, 1.000000000000000000, 0.8660254037844387076, 1.000000000000000000, 0.8660254037844387076, 1.000000000000000000) ) ) 
 REPRESENTATION_ITEM ( '' )  SURFACE ( )  );
#30905 = CARTESIAN_POINT ( 'NONE',  ( 1.383448652483735941, 0.1460618955802815977, -2.007835497447094664 ) ) ;
#30906 = DIRECTION ( 'NONE',  ( 0.000000000000000000, -0.000000000000000000, 1.000000000000000000 ) ) ;
#30907 = CARTESIAN_POINT ( 'NONE',  ( 2.802037382575186975, -0.6933082239683820980, 2.095089865402133267 ) ) ;
#30908 = B_SPLINE_CURVE_WITH_KNOTS ( 'NONE', 3,
 ( #171793, #122066, #185888, #105768, #90566, #156626 ),
 .UNSPECIFIED., .F., .F.,
 ( 4, 2, 4 ),
 ( 0.000000000000000000, 0.002403146417856977853, 0.004806292835713955706 ),
 .UNSPECIFIED. ) ;
#30909 = CARTESIAN_POINT ( 'NONE',  ( 4.979425714853139340, -0.1133551455631234828, 2.168255935233906584 ) ) ;
#30910 = EDGE_LOOP ( 'NONE', ( #50609, #100398, #203760, #160946, #3436, #102690 ) ) ;
#30911 = CARTESIAN_POINT ( 'NONE',  ( 3.627688620108284745, 6.389997935838436227, 1.199719254218452047 ) ) ;
#30913 = CARTESIAN_POINT ( 'NONE',  ( 1.458611474731505986, -1.915607644094442064, -0.6298556652749933704 ) ) ;
#30912 = CARTESIAN_POINT ( 'NONE',  ( 3.053504691927158898, -1.869126254513186591, 1.001442229663196182 ) ) ;
#30915 = VERTEX_POINT ( 'NONE', #174034 ) ;
#30914 = CARTESIAN_POINT ( 'NONE',  ( 2.126969254794884634, 1.619647995875729496, 0.8116002879420233240 ) ) ;
#30916 = CARTESIAN_POINT ( 'NONE',  ( 6.900173834712277632, 7.014900660111269559, -0.7998128361456341429 ) ) ;
#30917 = CARTESIAN_POINT ( 'NONE',  ( 5.099838337034727331, 9.101561826515851550, -0.7998128361456281477 ) ) ;
#30919 = CARTESIAN_POINT ( 'NONE',  ( 1.129944905810562839, 1.913687095308055808, 0.09034645858918381733 ) ) ;
#30918 = CARTESIAN_POINT ( 'NONE',  ( -2.916975605234527702, 6.554888639415577423, 1.040834085586084257E-14 ) ) ;
#30920 = CARTESIAN_POINT ( 'NONE',  ( 0.3870072406890456840, 1.529612873802629780, -11.82510647457160147 ) ) ;
#30921 = CARTESIAN_POINT ( 'NONE',  ( 9.597420367780058470, -7.030163990561723253, -0.01387835396682351140 ) ) ;
#30922 = CARTESIAN_POINT ( 'NONE',  ( 4.758548728272192108, 7.535095368750792666, -1.082531754730549078 ) ) ;
#30923 = CARTESIAN_POINT ( 'NONE',  ( 1.364683531249986537, -0.07395833299191513499, 0.7879004041258500513 ) ) ;
#30924 = CARTESIAN_POINT ( 'NONE',  ( -3.096514578442687515, 6.188910745953249304, -0.7944190528704382359 ) ) ;
#30925 = CARTESIAN_POINT ( 'NONE',  ( -7.974166903131914452, 12.45494515362926435, -0.7998128361456281477 ) ) ;
#30926 = CARTESIAN_POINT ( 'NONE',  ( 4.786082296487640164, -1.021991182799499409, 1.904868704497929333 ) ) ;
#30927 = CARTESIAN_POINT ( 'NONE',  ( -5.641601317062248988, 6.714861303728305586, -1.082531754730549967 ) ) ;
#30928 = CARTESIAN_POINT ( 'NONE',  ( 4.367134877377630175, 7.148722219365612141, -1.082531754730548412 ) ) ;
#30929 = CARTESIAN_POINT ( 'NONE',  ( 2.127334043950947606, 1.896359100603739911, 0.9491756072362851349 ) ) ;
#30931 = CARTESIAN_POINT ( 'NONE',  ( -12.00295043402534212, 5.507662538472692049, -4.496421502479775789 ) ) ;
#30930 = CARTESIAN_POINT ( 'NONE',  ( 0.000000000000000000, 7.849261790823902629, 0.000000000000000000 ) ) ;
#30932 = CARTESIAN_POINT ( 'NONE',  ( 3.620352162249322880, 1.253078330817010588, -1.521826374184510389 ) ) ;
#30933 = CARTESIAN_POINT ( 'NONE',  ( 5.308822938259078583, -0.4706598425541131947, -1.853433239416848455 ) ) ;
#30934 = EDGE_LOOP ( 'NONE', ( #179790, #143357, #27609, #78222 ) ) ;
#30935 = CARTESIAN_POINT ( 'NONE',  ( 1.530148271428825923, -1.292818251517693584, 1.500000000002693179 ) ) ;
#30936 = CARTESIAN_POINT ( 'NONE',  ( 0.7134375191242479097, -1.748147108003229810, -1.108949491591210146 ) ) ;
#30937 = CARTESIAN_POINT ( 'NONE',  ( 2.009616874778739071, -0.9155987108000520625, -1.712560621339030309 ) ) ;
#30938 = ORIENTED_EDGE ( 'NONE', *, *, #47755, .F. ) ;
#30939 = CARTESIAN_POINT ( 'NONE',  ( -4.229020061460118107, 7.343517960532633282, -0.8650006913940473385 ) ) ;
#30941 = CARTESIAN_POINT ( 'NONE',  ( 8.011942431032855083, 8.311964022485323511, 0.7998128361456291469 ) ) ;
#30940 = CARTESIAN_POINT ( 'NONE',  ( -7.756673280794142755, 8.222076047114187602, -0.7216878364870338292 ) ) ;
#30943 = CARTESIAN_POINT ( 'NONE',  ( 7.481401836642521452, 7.622723652371411696, 1.040834085586084257E-14 ) ) ;
#30942 = CARTESIAN_POINT ( 'NONE',  ( 2.484421436082083101, -0.3582009261528392163, -2.059553721446294894 ) ) ;
#30944 = CARTESIAN_POINT ( 'NONE',  ( 6.034787771414195312, 6.213209619504250547, -0.7216878364870458196 ) ) ;
#30946 = ORIENTED_EDGE ( 'NONE', *, *, #43574, .T. ) ;
#30945 = CARTESIAN_POINT ( 'NONE',  ( 5.760397938718036848, 1.910310778393434106, 0.08934430699411573251 ) ) ;
#30947 = CARTESIAN_POINT ( 'NONE',  ( 4.846401659255799466, 2.200796399388889935, 0.1645688927329121420 ) ) ;
#30948 = COLOUR_RGB ( '', 0.40784314, 0.44705882, 0.49803922) ;
#30949 = CARTESIAN_POINT ( 'NONE',  ( 2.643839551151895506, -1.634601560588926583, -1.482707865360691990 ) ) ;
#30950 = CARTESIAN_POINT ( 'NONE',  ( 8.959240580532112475, 9.346868853575953651, -0.7998128361456221525 ) ) ;
#30951 = DIRECTION ( 'NONE',  ( 0.1510067114093955887, 0.000000000000000000, -0.9885327375000383388 ) ) ;
#30952 = CARTESIAN_POINT ( 'NONE',  ( 1.541514448083292965, -1.800223203088219481, 0.6453159242577054533 ) ) ;
#30953 = CARTESIAN_POINT ( 'NONE',  ( 10.99943592164172657, -8.407420853759269619, -0.1113975120798811613 ) ) ;
#30954 = CARTESIAN_POINT ( 'NONE',  ( 10.42352117080803708, 11.05519620889787724, -0.7998128361456281477 ) ) ;
#30955 = CARTESIAN_POINT ( 'NONE',  ( 4.369627354678314646, -0.3570511267821044332, 2.039192500141631115 ) ) ;
#30957 = CARTESIAN_POINT ( 'NONE',  ( 1.358524781292804517, 0.8764843271744371389, 1.976213614152767750 ) ) ;
#30956 = CARTESIAN_POINT ( 'NONE',  ( 1.499999999999987121, 3.795833333333357373, -0.8660254037844263841 ) ) ;
#30958 = CARTESIAN_POINT ( 'NONE',  ( 3.210657068901449307, 1.982179491636561819, 0.9350799695589939731 ) ) ;
#30959 = AXIS2_PLACEMENT_3D ( 'NONE', #119293, #172259, #89954 ) ;
#30960 = CARTESIAN_POINT ( 'NONE',  ( -9.499668754385632852, 7.849261790823902629, -0.07933194154487524519 ) ) ;
#30961 = DIRECTION ( 'NONE',  ( 0.000000000000000000, 1.000000000000000000, 0.000000000000000000 ) ) ;
#30962 = CARTESIAN_POINT ( 'NONE',  ( -0.4996389044604229723, 7.815212647110488575, 1.937417588921823919 ) ) ;
#30963 = CARTESIAN_POINT ( 'NONE',  ( 6.561219994370630637, 6.619454513046008515, 0.000000000000000000 ) ) ;
#30964 = CARTESIAN_POINT ( 'NONE',  ( 1.364683531250000303, 13.81770833367473017, -0.7879004041258355073 ) ) ;
#30965 = CARTESIAN_POINT ( 'NONE',  ( -3.817502770699643388, 6.611447778194983194, 1.199719254218452935 ) ) ;
#30966 = CARTESIAN_POINT ( 'NONE',  ( -0.1341500063891595818, -0.1486117279969369209, -1.983907055413631992 ) ) ;
#30967 = CARTESIAN_POINT ( 'NONE',  ( -10.33094986393327197, 11.15512238411806578, 0.7216878364870438212 ) ) ;
#30968 = CARTESIAN_POINT ( 'NONE',  ( 4.592674910654532816, 2.029287475768901228, 0.4089837765668055680 ) ) ;
#30969 = CARTESIAN_POINT ( 'NONE',  ( 3.123571566491334384, -1.856553849623356234, 0.5141669907481066781 ) ) ;
#30970 = CARTESIAN_POINT ( 'NONE',  ( 6.222275945484236459, 2.094208529755392068, 0.3105017025616888526 ) ) ;
#30971 = CARTESIAN_POINT ( 'NONE',  ( 6.335737856287750880, 6.286115675290828264, -0.7998128361456281477 ) ) ;
#30972 = CARTESIAN_POINT ( 'NONE',  ( 4.796824973295459316, 8.251456047330133714, 0.8599625132450954279 ) ) ;
#30973 = CARTESIAN_POINT ( 'NONE',  ( 4.065260974683176265, 1.686948271169801616, 1.016115061114295504 ) ) ;
#30974 = CARTESIAN_POINT ( 'NONE',  ( 5.718756930148481743, -0.06150597819632765140, 2.291595365457484323 ) ) ;
#30975 = CARTESIAN_POINT ( 'NONE',  ( 4.107882937833263526, -1.820653182827164596, 0.1363937739093170898 ) ) ;
#30976 = CARTESIAN_POINT ( 'NONE',  ( 5.872089928494542477, 9.864872326636710653, 0.000000000000000000 ) ) ;
#30977 = CARTESIAN_POINT ( 'NONE',  ( 5.490689023410166847, 5.508151403507724808, -0.7216878364870207285 ) ) ;
#30978 = CARTESIAN_POINT ( 'NONE',  ( -7.293360289508603600, 7.473618190706972086, 0.000000000000000000 ) ) ;
#30979 = CARTESIAN_POINT ( 'NONE',  ( 4.667750024854814050, 8.667735138964429709, -0.7998128361456381397 ) ) ;
#30980 = EDGE_LOOP ( 'NONE', ( #52826, #137642, #9492, #213325 ) ) ;
#30982 = CARTESIAN_POINT ( 'NONE',  ( 5.027594669734884114, -0.2912581947275821315, 1.991892893239319617 ) ) ;
#30981 = CARTESIAN_POINT ( 'NONE',  ( 1.698526806778306586, 1.531337151408303621, 1.022036240780115346 ) ) ;
#30983 = CARTESIAN_POINT ( 'NONE',  ( 6.258407524398033495, 2.201109419358293628, -0.6625764064998507230 ) ) ;
#30984 = CARTESIAN_POINT ( 'NONE',  ( 5.594571816639393624, 1.932094781187740917, 0.3390067100078468232 ) ) ;
#30985 = CARTESIAN_POINT ( 'NONE',  ( -6.612626235163205024, 8.737816579155630592, -1.599625672291263179 ) ) ;
#30986 = CARTESIAN_POINT ( 'NONE',  ( -5.382750679825375251, 6.238629533673094585, -1.199719254218446718 ) ) ;
#30987 = CARTESIAN_POINT ( 'NONE',  ( -10.53927507717126666, 2.018041202053943994, -6.084853302868306280 ) ) ;
#30988 = CARTESIAN_POINT ( 'NONE',  ( -5.855142236255304944, 7.924361590421551860, -1.599625672291271394 ) ) ;
#30990 = CARTESIAN_POINT ( 'NONE',  ( 0.5845639792326964290, -0.2246964894469481722, -1.857040431621145959 ) ) ;
#30989 = CARTESIAN_POINT ( 'NONE',  ( 1.206708187092224716, 1.845608279032302512, 0.9822807542516975854 ) ) ;
#30991 = CARTESIAN_POINT ( 'NONE',  ( 0.5512317429218656084, 7.510131493957763915, -1.922545642343834738 ) ) ;
#30992 = CARTESIAN_POINT ( 'NONE',  ( 5.665949523032352886, -1.230194547739250854, 1.502597557546548446 ) ) ;
#30993 = CARTESIAN_POINT ( 'NONE',  ( -0.1102773484823937195, 1.994803768489497031, -2.617422746694163749 ) ) ;
#30994 = CARTESIAN_POINT ( 'NONE',  ( 1.452286687950472999, -1.492487064643189809, -0.8950295028009451759 ) ) ;
#30995 = CARTESIAN_POINT ( 'NONE',  ( 6.368579470117202490, 8.453095353268645695, 1.599625672291281386 ) ) ;
#30996 = CARTESIAN_POINT ( 'NONE',  ( 0.000000000000000000, 3.400000000000000355, 0.000000000000000000 ) ) ;
#30997 = CARTESIAN_POINT ( 'NONE',  ( 1.365380774817010368, 1.699871498885496379, -0.2916373863959387802 ) ) ;
#30998 = CARTESIAN_POINT ( 'NONE',  ( 1.892365914234435120, -0.5883382831698009685, -2.111031122750434808 ) ) ;
#30999 = CARTESIAN_POINT ( 'NONE',  ( 4.424592250794217030, 1.359014646446855767, -1.738718759629574118 ) ) ;
#31000 = CARTESIAN_POINT ( 'NONE',  ( -10.37923916842784422, 4.890109552615133026, -5.358306740738790097 ) ) ;
#31001 = MECHANICAL_DESIGN_GEOMETRIC_PRESENTATION_REPRESENTATION (  '', ( #121051 ), #93323 ) ;
#31002 = CARTESIAN_POINT ( 'NONE',  ( 1.253040875654364505, -0.5252153140962511069, -2.106489908942406952 ) ) ;
#31003 = CARTESIAN_POINT ( 'NONE',  ( 0.2932112110246976044, 1.350478442433366677, 1.228755397233910696 ) ) ;
#31004 = CARTESIAN_POINT ( 'NONE',  ( 2.536447107014605962, 0.7179835868570243473, 1.991995636484017673 ) ) ;
#31005 = FACE_OUTER_BOUND ( 'NONE', #18970, .T. ) ;
#31006 = ORIENTED_EDGE ( 'NONE', *, *, #141509, .F. ) ;
#31008 = CARTESIAN_POINT ( 'NONE',  ( -0.6823417656250246877, 0.3635416670080895973, 1.181850606188755259 ) ) ;
#31007 = CARTESIAN_POINT ( 'NONE',  ( 2.472590379642979563, -2.194723544211283350, -0.6619992606377905764 ) ) ;
#31009 = DIRECTION ( 'NONE',  ( 0.000000000000000000, 0.000000000000000000, 1.000000000000000000 ) ) ;
#31010 = CARTESIAN_POINT ( 'NONE',  ( 3.330499290451326200, 7.037332938835193730, -0.7998128361456291469 ) ) ;
#31011 = CARTESIAN_POINT ( 'NONE',  ( 4.494933454782477078, -2.154585855983886411, -0.5399016382821394400 ) ) ;
#31012 = CARTESIAN_POINT ( 'NONE',  ( -7.226132686403777150, 7.532835677000276675, 1.040834085586084257E-14 ) ) ;
#31013 = ADVANCED_FACE ( 'NONE', ( #25606 ), #135307, .T. ) ;
#31014 = CARTESIAN_POINT ( 'NONE',  ( 3.362058906508953449, 6.866226457661676719, -0.7216878364870267237 ) ) ;
#31015 = CARTESIAN_POINT ( 'NONE',  ( -8.500599125644013654, 9.019713189447241319, 0.7216878364870438212 ) ) ;
#31016 = CARTESIAN_POINT ( 'NONE',  ( 4.082413651490639062, 7.776916670132135501, 0.000000000000000000 ) ) ;
#31017 = EDGE_LOOP ( 'NONE', ( #116832, #45027, #165860, #134297, #63937 ) ) ;
#31018 = CARTESIAN_POINT ( 'NONE',  ( 2.461564753630896440, -1.930417925741171103, -0.5826551686555282439 ) ) ;
#31020 = CARTESIAN_POINT ( 'NONE',  ( 1.938405323705337135, -1.106995438288145950, 1.740174596247965555 ) ) ;
#31019 = CARTESIAN_POINT ( 'NONE',  ( 6.076025397218672630, 10.24044673006381245, -0.7998128361456291469 ) ) ;
#31021 = PLANE ( 'NONE',  #157884 ) ;
#31022 = CARTESIAN_POINT ( 'NONE',  ( 5.546694241322223107, 5.643767167730274537, -0.7216878364870458196 ) ) ;
#31023 = CARTESIAN_POINT ( 'NONE',  ( 0.4019237886466847653, 8.604914550367425363, 1.499999999999997113 ) ) ;
#31024 = CARTESIAN_POINT ( 'NONE',  ( 1.364683531249990311, 5.613541667008087543, 0.7879004041258500513 ) ) ;
#31025 = CARTESIAN_POINT ( 'NONE',  ( 5.578137875217415775, -2.137416510240647494, -0.4829537091169676666 ) ) ;
#31026 = CARTESIAN_POINT ( 'NONE',  ( 2.145157927413956944, 0.8647252629472859109, 1.821741647932619390 ) ) ;
#31027 = CARTESIAN_POINT ( 'NONE',  ( 1.645803748337611783, 0.5784278848013635344, 1.748079663633335334 ) ) ;
#31028 = EDGE_CURVE ( 'NONE', #22839, #9659, #133301, .T. ) ;
#31029 = CARTESIAN_POINT ( 'NONE',  ( 7.958799866421889746, 9.244020251369077457, -1.199719254218441611 ) ) ;
#31030 = FILL_AREA_STYLE ('',( #62441 ) ) ;
#31031 = CARTESIAN_POINT ( 'NONE',  ( 5.719710266082651096, -1.780569991979109590, 0.4021758204828808081 ) ) ;
#31032 = CARTESIAN_POINT ( 'NONE',  ( 5.520157785563180930, -1.821743191724470634, 0.8647220171385738841 ) ) ;
#31033 = CARTESIAN_POINT ( 'NONE',  ( -6.906989191158078079, 10.14557225873805812, -1.199719254218440723 ) ) ;
#31035 = CARTESIAN_POINT ( 'NONE',  ( -6.577640801285370209, 7.702944352034914566, -1.199719254218452047 ) ) ;
#31034 = CARTESIAN_POINT ( 'NONE',  ( 5.647450836711301214, -1.779752484188871886, -1.396855495411459147 ) ) ;
#31036 = CARTESIAN_POINT ( 'NONE',  ( 0.6453166446471610973, -1.805311040884694185, 1.084365637629558954 ) ) ;
#31037 = CARTESIAN_POINT ( 'NONE',  ( -6.291865805193673111, 9.498204651771386509, -1.199719254218452047 ) ) ;
#31038 = CARTESIAN_POINT ( 'NONE',  ( 4.281733463571851139, -1.982135700070002615, 0.5980053909793592304 ) ) ;
#31039 = CARTESIAN_POINT ( 'NONE',  ( 8.565000355531088516, 11.01558638625153286, -1.599625672291257406 ) ) ;
#31040 = DIRECTION ( 'NONE',  ( 1.000000000000000000, 0.000000000000000000, 0.000000000000000000 ) ) ;
#31041 = CARTESIAN_POINT ( 'NONE',  ( -9.016335848287868160, 10.47781223021269170, 1.199719254218462483 ) ) ;
#31042 = DIRECTION ( 'NONE',  ( 1.276756478318932585E-15, -1.000000000000000000, 1.665334536937738262E-16 ) ) ;
#31043 = CARTESIAN_POINT ( 'NONE',  ( 8.174640274396848483, 8.501778173076651512, 0.7998128361456291469 ) ) ;
#31044 = CARTESIAN_POINT ( 'NONE',  ( 5.808322585208748556, 6.028124808163927817, -0.4837759047566763670 ) ) ;
#31045 = CARTESIAN_POINT ( 'NONE',  ( -9.829298180227631576, 10.56986208646148384, 1.040834085586084257E-14 ) ) ;
#31047 = CARTESIAN_POINT ( 'NONE',  ( 3.322728300399055534, -0.9034660432867666069, -2.029577789741637162 ) ) ;
#31046 = CARTESIAN_POINT ( 'NONE',  ( 1.635180430577408028, 1.980530345366804834, 0.7584260845197098311 ) ) ;
#31048 = CYLINDRICAL_SURFACE ( 'NONE', #82018, 0.08000000000000020983 ) ;
#31049 = CARTESIAN_POINT ( 'NONE',  ( -7.096767062110449942, 7.244259425409119046, -0.7998128361456362523 ) ) ;
#31050 = CARTESIAN_POINT ( 'NONE',  ( 5.961834861707224320, 7.978559976790334574, -1.599625672291262513 ) ) ;
#31051 = CARTESIAN_POINT ( 'NONE',  ( 2.682025323810240280, -1.127217178123595565, -1.605522638798158264 ) ) ;
#31052 = CARTESIAN_POINT ( 'NONE',  ( 5.392392409933256303, 7.314210449720692786, 1.599625672291267398 ) ) ;
#31053 = CARTESIAN_POINT ( 'NONE',  ( -4.073306942994160629, 7.542743630792291043, -0.4897309385070089394 ) ) ;
#31054 = CARTESIAN_POINT ( 'NONE',  ( 2.659370686574860976, 6.254349567645977714, -0.7998128361456291469 ) ) ;
#31055 = CARTESIAN_POINT ( 'NONE',  ( -3.824808732831001201, 7.476377598362539345, 0.7216878364870338292 ) ) ;
#31056 = CARTESIAN_POINT ( 'NONE',  ( -7.429504990608782222, 8.730472579540773381, 1.082531754730549967 ) ) ;
#31057 = CARTESIAN_POINT ( 'NONE',  ( 1.881254504445781794, -1.940830296247602949, -0.8548571619346673200 ) ) ;
#31058 = CARTESIAN_POINT ( 'NONE',  ( -5.960744811863571968, 6.983232364376142698, 1.199719254218452935 ) ) ;
#31059 = CARTESIAN_POINT ( 'NONE',  ( 4.188458007013862172, -2.137797052781073237, -0.3198388112101158143 ) ) ;
#31060 = CARTESIAN_POINT ( 'NONE',  ( 3.386116603743833497, -0.3623624896987760469, -1.805063595765175499 ) ) ;
#31061 = CARTESIAN_POINT ( 'NONE',  ( -5.076477019373391464, 6.555905325687263030, 1.224675693024103174 ) ) ;
#31062 = ADVANCED_FACE ( 'NONE', ( #16801, #13624 ), #29895, .F. ) ;
#31063 = CARTESIAN_POINT ( 'NONE',  ( -1.364683531250000748, -0.1781249996585798634, 0.000000000000000000 ) ) ;
#31064 = CARTESIAN_POINT ( 'NONE',  ( 5.701030997009290502, -0.4167664840721523878, 1.689554919747728423 ) ) ;
#31065 = CARTESIAN_POINT ( 'NONE',  ( 6.727182134110193168, 4.701113012587437190, 2.373661997258198486 ) ) ;
#31066 = CARTESIAN_POINT ( 'NONE',  ( 4.202664430556247055, 6.886563688082179446, 1.082531754730558626 ) ) ;
#31067 = CARTESIAN_POINT ( 'NONE',  ( 2.588937169860201504, -0.3686131662095324946, -2.129881858774537395 ) ) ;
#31068 = AXIS2_PLACEMENT_3D ( 'NONE', #83764, #20875, #170350 ) ;
#31069 = CARTESIAN_POINT ( 'NONE',  ( 4.077499844852236599, 1.427718728413525318, -1.423743541103118737 ) ) ;
#31070 = CARTESIAN_POINT ( 'NONE',  ( -9.015808962963337336, 10.58116054728778366, 1.082531754730558626 ) ) ;
#31071 = CARTESIAN_POINT ( 'NONE',  ( 2.870174731959000525, 1.155358403710282866, 1.826860881501219280 ) ) ;
#31072 = CARTESIAN_POINT ( 'NONE',  ( 2.882053135459626159, -1.016639628983921684, 1.688880165396142718 ) ) ;
#31074 = EDGE_CURVE ( 'NONE', #95548, #90583, #108388, .T. ) ;
#31073 = CARTESIAN_POINT ( 'NONE',  ( 2.940638933469359895, -1.523795050681177710, 1.320827213682006285 ) ) ;
#31075 = CARTESIAN_POINT ( 'NONE',  ( 6.509000000000011887, 2.430396405248925529, 2.482145556523357222 ) ) ;
#31076 = CARTESIAN_POINT ( 'NONE',  ( 4.476081132534933893, -1.884639481945263872, -0.4683437986269470277 ) ) ;
#31079 = ORIENTED_EDGE ( 'NONE', *, *, #198311, .T. ) ;
#31078 = DIRECTION ( 'NONE',  ( -0.9055141421511233579, 0.4243160830846685050, -2.454401000341485681E-15 ) ) ;
#31077 = CARTESIAN_POINT ( 'NONE',  ( -9.802181872555943087, 10.53822639417784046, 0.7216878364870438212 ) ) ;
#31081 = EDGE_CURVE ( 'NONE', #136958, #93339, #30283, .T. ) ;
#31080 = CARTESIAN_POINT ( 'NONE',  ( -3.296040741453672318, 6.859481608422314025, 0.7216878364870338292 ) ) ;
#31082 = CARTESIAN_POINT ( 'NONE',  ( 4.004454267989866700, 5.765225627445230927, 1.599625672291262513 ) ) ;
#31084 = ORIENTED_EDGE ( 'NONE', *, *, #4355, .F. ) ;
#31083 = CARTESIAN_POINT ( 'NONE',  ( -4.606738333593328072, 8.596554832492683929, 0.7998128361456281477 ) ) ;
#31085 = CARTESIAN_POINT ( 'NONE',  ( -7.985389288324697965, 10.33937347451072775, -1.443375672974058777 ) ) ;
#31086 = CARTESIAN_POINT ( 'NONE',  ( 1.272829778695073299, -1.399090282553701270, 1.706552004499435560 ) ) ;
#31087 = CARTESIAN_POINT ( 'NONE',  ( -1.642778471875000035, -2.267708332855375541, -2.845375778867859751 ) ) ;
#31088 = CARTESIAN_POINT ( 'NONE',  ( 5.559412779221331924, 1.601624451964112739, 1.132529127964493121 ) ) ;
#31089 =( BOUNDED_SURFACE ( )  B_SPLINE_SURFACE ( 1, 2, ( 
 ( #48360, #114471, #128613, #146933, #100275, #15810, #162102, #210825, #62450, #195663, #194580, #213992, #131762, #96049, #197767, #115524, #145877, #119790, #37404, #68814, #39542, #150108, #20071, #117662, #101335, #5943, #55789, #85089, #67734, #187912, #151173, #72014, #152231, #199891, #120874, #84017, #51537, #105643, #170601, #17932, #201999, #169540, #87226, #133884, #183654, #1680, #86160, #35259, #200942, #53658, #167417, #69876, #19008, #121946, #138127, #3802, #135985, #185771, #134936, #88303, #52591, #118718, #4866, #2744, #184705, #103478, #21120, #203080, #153290, #36327, #102405, #154364, #168473, #70944, #137055, #54725, #186848, #38480, #204136, #104557, #22188, #175967, #27561, #126218, #158640, #75251, #58997, #159700, #173842, #107817, #205220, #174910, #172761, #93657, #24336, #26488, #188987, #77378, #192179, #92598, #10237, #11299, #139190, #190055, #143494, #76312, #209490, #91525, #140283, #142419, #23267, #41707, #108887, #57927, #7014, #56862, #157583, #125153, #89379, #191112, #43840, #25419, #9176, #141364, #155428, #206303, #109956, #73089, #207377, #127291, #171670, #124092, #208428, #61131, #42779, #60062, #123036, #44909, #193262, #40631, #106734, #90444, #156512, #8101, #74191, #210573, #112094, #144563, #32896, #97922, #96864, #28639, #81642, #114225, #65367, #165026, #180223, #98974, #63265, #29713, #94726, #147727, #129427, #198568, #16620, #196471, #95794, #211630, #13439, #12364, #178096, #113156, #111017, #161851, #62207, #78443, #79516, #131514, #197517, #82702, #177022, #146682, #213744, #128364, #45973, #145634, #31845, #115278, #64339, #160771, #179161, #30785, #195411 ),
 ( #49161, #163980, #194331, #47040, #148781, #351, #48113, #162912, #14494, #80584, #181270, #66424, #212698, #130481, #132567, #15555, #7570, #40100, #171154, #154917, #41183, #55280, #203628, #83767, #56346, #54214, #57407, #120352, #122508, #67492, #173312, #73655, #188468, #106212, #107290, #17681, #71501, #189535, #172238, #24891, #187398, #21669, #23826, #116336, #137612, #204696, #153851, #100031, #149860, #39030, #6501, #182326, #72576, #139755, #121428, #105114, #22744, #33955, #87777, #205779, #166093, #88862, #8648, #50217, #5422, #89931, #157060, #138677, #155982, #1428, #140832, #74727, #133637, #202562, #123573, #90997, #186329, #37963, #104036, #170082, #25962, #128887, #193793, #174384, #10771, #194868, #45442, #46502, #126758, #175439, #111556, #58477, #76845, #144036, #93132, #42247, #92067, #192718, #94200, #124632, #160240, #161315, #142964, #44372, #208967, #190590, #27024, #12899, #108360, #60599, #162387, #206845, #159171, #29178, #96331, #110495, #176494, #158125, #80048, #13964, #9716, #75792, #28105, #30247, #11840, #141900, #207910, #59531, #125691, #112625, #177565, #77917, #191650, #95267, #210033, #43315, #109433, #61673, #127841, #78979, #178635, #145098, #211102, #62726, #212167, #113697, #150403, #199106, #1970, #214269, #115815, #181802, #129959, #179701, #63801, #98444, #195947, #131009, #65902, #47583, #82176, #146151, #31317, #97394, #33435, #165569, #17164, #16092, #163450, #132048, #198058, #182879, #15030, #197001, #99512, #901, #18233, #116880, #32378, #164508, #81122, #147207, #34495, #148270, #49687, #83238, #213232, #64864, #149323, #100569, #48636, #114754, #180751 ) ),
 .UNSPECIFIED., .F., .F., .T. ) 
 B_SPLINE_SURFACE_WITH_KNOTS ( ( 2, 2 ),
 ( 3, 2, 2, 2, 2, 2, 2, 2, 2, 2, 2, 2, 2, 2, 2, 2, 2, 2, 2, 2, 2, 2, 2, 2, 2, 2, 2, 2, 2, 2, 2, 2, 2, 2, 2, 2, 2, 2, 2, 2, 2, 2, 2, 2, 2, 2, 2, 2, 2, 2, 2, 2, 2, 2, 2, 2, 2, 2, 2, 2, 2, 2, 2, 2, 2, 2, 2, 2, 2, 2, 2, 2, 2, 2, 2, 2, 2, 2, 2, 2, 2, 2, 2, 2, 2, 2, 2, 2, 2, 2, 2, 2, 2, 2, 2, 2, 3 ),
 ( 0.000000000000000000, 1.000000000000000000 ),
 ( 0.000000000000000000, 0.01041666666666666609, 0.02083333333333333218, 0.03125000000000000000, 0.04166666666666666435, 0.05208333333333333565, 0.06250000000000000000, 0.07291666666666667129, 0.08333333333333332871, 0.09375000000000000000, 0.1041666666666666713, 0.1145833333333333287, 0.1250000000000000000, 0.1354166666666666574, 0.1458333333333333426, 0.1562500000000000000, 0.1666666666666666574, 0.1770833333333333426, 0.1875000000000000000, 0.1979166666666666574, 0.2083333333333333426, 0.2187500000000000000, 0.2291666666666666574, 0.2395833333333333426, 0.2500000000000000000, 0.2604166666666666852, 0.2708333333333333148, 0.2812500000000000000, 0.2916666666666666852, 0.3020833333333333148, 0.3125000000000000000, 0.3229166666666666852, 0.3333333333333333148, 0.3437500000000000000, 0.3541666666666666852, 0.3645833333333333148, 0.3750000000000000000, 0.3854166666666666852, 0.3958333333333333148, 0.4062500000000000000, 0.4166666666666666852, 0.4270833333333333148, 0.4375000000000000000, 0.4479166666666666852, 0.4583333333333333148, 0.4687500000000000000, 0.4791666666666666852, 0.4895833333333333148, 0.5000000000000000000, 0.5104166666666666297, 0.5208333333333333703, 0.5312500000000000000, 0.5416666666666666297, 0.5520833333333333703, 0.5625000000000000000, 0.5729166666666666297, 0.5833333333333333703, 0.5937500000000000000, 0.6041666666666666297, 0.6145833333333333703, 0.6250000000000000000, 0.6354166666666666297, 0.6458333333333333703, 0.6562500000000000000, 0.6666666666666666297, 0.6770833333333333703, 0.6875000000000000000, 0.6979166666666666297, 0.7083333333333333703, 0.7187500000000000000, 0.7291666666666666297, 0.7395833333333333703, 0.7500000000000000000, 0.7604166666666666297, 0.7708333333333333703, 0.7812500000000000000, 0.7916666666666666297, 0.8020833333333333703, 0.8125000000000000000, 0.8229166666666666297, 0.8333333333333333703, 0.8437500000000000000, 0.8541666666666666297, 0.8645833333333333703, 0.8750000000000000000, 0.8854166666666666297, 0.8958333333333333703, 0.9062500000000000000, 0.9166666666666666297, 0.9270833333333333703, 0.9375000000000000000, 0.9479166666666666297, 0.9583333333333333703, 0.9687500000000000000, 0.9791666666666666297, 0.9895833333333333703, 1.000000000000000000 ),
 .UNSPECIFIED. ) 
 GEOMETRIC_REPRESENTATION_ITEM ( )  RATIONAL_B_SPLINE_SURFACE ( (
 ( 1.000000000000000000, 0.8660254037844387076, 1.000000000000000000, 0.8660254037844387076, 1.000000000000000000, 0.8660254037844387076, 1.000000000000000000, 0.8660254037844387076, 1.000000000000000000, 0.8660254037844387076, 1.000000000000000000, 0.8660254037844387076, 1.000000000000000000, 0.8660254037844387076, 1.000000000000000000, 0.8660254037844387076, 1.000000000000000000, 0.8660254037844387076, 1.000000000000000000, 0.8660254037844387076, 1.000000000000000000, 0.8660254037844387076, 1.000000000000000000, 0.8660254037844387076, 1.000000000000000000, 0.8660254037844387076, 1.000000000000000000, 0.8660254037844387076, 1.000000000000000000, 0.8660254037844387076, 1.000000000000000000, 0.8660254037844387076, 1.000000000000000000, 0.8660254037844387076, 1.000000000000000000, 0.8660254037844387076, 1.000000000000000000, 0.8660254037844387076, 1.000000000000000000, 0.8660254037844387076, 1.000000000000000000, 0.8660254037844387076, 1.000000000000000000, 0.8660254037844387076, 1.000000000000000000, 0.8660254037844387076, 1.000000000000000000, 0.8660254037844387076, 1.000000000000000000, 0.8660254037844387076, 1.000000000000000000, 0.8660254037844387076, 1.000000000000000000, 0.8660254037844387076, 1.000000000000000000, 0.8660254037844387076, 1.000000000000000000, 0.8660254037844387076, 1.000000000000000000, 0.8660254037844387076, 1.000000000000000000, 0.8660254037844387076, 1.000000000000000000, 0.8660254037844387076, 1.000000000000000000, 0.8660254037844387076, 1.000000000000000000, 0.8660254037844387076, 1.000000000000000000, 0.8660254037844387076, 1.000000000000000000, 0.8660254037844387076, 1.000000000000000000, 0.8660254037844387076, 1.000000000000000000, 0.8660254037844387076, 1.000000000000000000, 0.8660254037844387076, 1.000000000000000000, 0.8660254037844387076, 1.000000000000000000, 0.8660254037844387076, 1.000000000000000000, 0.8660254037844387076, 1.000000000000000000, 0.8660254037844387076, 1.000000000000000000, 0.8660254037844387076, 1.000000000000000000, 0.8660254037844387076, 1.000000000000000000, 0.8660254037844387076, 1.000000000000000000, 0.8660254037844387076, 1.000000000000000000, 0.8660254037844387076, 1.000000000000000000, 0.8660254037844387076, 1.000000000000000000, 0.8660254037844387076, 1.000000000000000000, 0.8660254037844387076, 1.000000000000000000, 0.8660254037844387076, 1.000000000000000000, 0.8660254037844387076, 1.000000000000000000, 0.8660254037844387076, 1.000000000000000000, 0.8660254037844387076, 1.000000000000000000, 0.8660254037844387076, 1.000000000000000000, 0.8660254037844387076, 1.000000000000000000, 0.8660254037844387076, 1.000000000000000000, 0.8660254037844387076, 1.000000000000000000, 0.8660254037844387076, 1.000000000000000000, 0.8660254037844387076, 1.000000000000000000, 0.8660254037844387076, 1.000000000000000000, 0.8660254037844387076, 1.000000000000000000, 0.8660254037844387076, 1.000000000000000000, 0.8660254037844387076, 1.000000000000000000, 0.8660254037844387076, 1.000000000000000000, 0.8660254037844387076, 1.000000000000000000, 0.8660254037844387076, 1.000000000000000000, 0.8660254037844387076, 1.000000000000000000, 0.8660254037844387076, 1.000000000000000000, 0.8660254037844387076, 1.000000000000000000, 0.8660254037844387076, 1.000000000000000000, 0.8660254037844387076, 1.000000000000000000, 0.8660254037844387076, 1.000000000000000000, 0.8660254037844387076, 1.000000000000000000, 0.8660254037844387076, 1.000000000000000000, 0.8660254037844387076, 1.000000000000000000, 0.8660254037844387076, 1.000000000000000000, 0.8660254037844387076, 1.000000000000000000, 0.8660254037844387076, 1.000000000000000000, 0.8660254037844387076, 1.000000000000000000, 0.8660254037844387076, 1.000000000000000000, 0.8660254037844387076, 1.000000000000000000, 0.8660254037844387076, 1.000000000000000000, 0.8660254037844387076, 1.000000000000000000, 0.8660254037844387076, 1.000000000000000000, 0.8660254037844387076, 1.000000000000000000, 0.8660254037844387076, 1.000000000000000000, 0.8660254037844387076, 1.000000000000000000, 0.8660254037844387076, 1.000000000000000000, 0.8660254037844387076, 1.000000000000000000, 0.8660254037844387076, 1.000000000000000000, 0.8660254037844387076, 1.000000000000000000, 0.8660254037844387076, 1.000000000000000000, 0.8660254037844387076, 1.000000000000000000, 0.8660254037844387076, 1.000000000000000000),
 ( 1.000000000000000000, 0.8660254037844387076, 1.000000000000000000, 0.8660254037844387076, 1.000000000000000000, 0.8660254037844387076, 1.000000000000000000, 0.8660254037844387076, 1.000000000000000000, 0.8660254037844387076, 1.000000000000000000, 0.8660254037844387076, 1.000000000000000000, 0.8660254037844387076, 1.000000000000000000, 0.8660254037844387076, 1.000000000000000000, 0.8660254037844387076, 1.000000000000000000, 0.8660254037844387076, 1.000000000000000000, 0.8660254037844387076, 1.000000000000000000, 0.8660254037844387076, 1.000000000000000000, 0.8660254037844387076, 1.000000000000000000, 0.8660254037844387076, 1.000000000000000000, 0.8660254037844387076, 1.000000000000000000, 0.8660254037844387076, 1.000000000000000000, 0.8660254037844387076, 1.000000000000000000, 0.8660254037844387076, 1.000000000000000000, 0.8660254037844387076, 1.000000000000000000, 0.8660254037844387076, 1.000000000000000000, 0.8660254037844387076, 1.000000000000000000, 0.8660254037844387076, 1.000000000000000000, 0.8660254037844387076, 1.000000000000000000, 0.8660254037844387076, 1.000000000000000000, 0.8660254037844387076, 1.000000000000000000, 0.8660254037844387076, 1.000000000000000000, 0.8660254037844387076, 1.000000000000000000, 0.8660254037844387076, 1.000000000000000000, 0.8660254037844387076, 1.000000000000000000, 0.8660254037844387076, 1.000000000000000000, 0.8660254037844387076, 1.000000000000000000, 0.8660254037844387076, 1.000000000000000000, 0.8660254037844387076, 1.000000000000000000, 0.8660254037844387076, 1.000000000000000000, 0.8660254037844387076, 1.000000000000000000, 0.8660254037844387076, 1.000000000000000000, 0.8660254037844387076, 1.000000000000000000, 0.8660254037844387076, 1.000000000000000000, 0.8660254037844387076, 1.000000000000000000, 0.8660254037844387076, 1.000000000000000000, 0.8660254037844387076, 1.000000000000000000, 0.8660254037844387076, 1.000000000000000000, 0.8660254037844387076, 1.000000000000000000, 0.8660254037844387076, 1.000000000000000000, 0.8660254037844387076, 1.000000000000000000, 0.8660254037844387076, 1.000000000000000000, 0.8660254037844387076, 1.000000000000000000, 0.8660254037844387076, 1.000000000000000000, 0.8660254037844387076, 1.000000000000000000, 0.8660254037844387076, 1.000000000000000000, 0.8660254037844387076, 1.000000000000000000, 0.8660254037844387076, 1.000000000000000000, 0.8660254037844387076, 1.000000000000000000, 0.8660254037844387076, 1.000000000000000000, 0.8660254037844387076, 1.000000000000000000, 0.8660254037844387076, 1.000000000000000000, 0.8660254037844387076, 1.000000000000000000, 0.8660254037844387076, 1.000000000000000000, 0.8660254037844387076, 1.000000000000000000, 0.8660254037844387076, 1.000000000000000000, 0.8660254037844387076, 1.000000000000000000, 0.8660254037844387076, 1.000000000000000000, 0.8660254037844387076, 1.000000000000000000, 0.8660254037844387076, 1.000000000000000000, 0.8660254037844387076, 1.000000000000000000, 0.8660254037844387076, 1.000000000000000000, 0.8660254037844387076, 1.000000000000000000, 0.8660254037844387076, 1.000000000000000000, 0.8660254037844387076, 1.000000000000000000, 0.8660254037844387076, 1.000000000000000000, 0.8660254037844387076, 1.000000000000000000, 0.8660254037844387076, 1.000000000000000000, 0.8660254037844387076, 1.000000000000000000, 0.8660254037844387076, 1.000000000000000000, 0.8660254037844387076, 1.000000000000000000, 0.8660254037844387076, 1.000000000000000000, 0.8660254037844387076, 1.000000000000000000, 0.8660254037844387076, 1.000000000000000000, 0.8660254037844387076, 1.000000000000000000, 0.8660254037844387076, 1.000000000000000000, 0.8660254037844387076, 1.000000000000000000, 0.8660254037844387076, 1.000000000000000000, 0.8660254037844387076, 1.000000000000000000, 0.8660254037844387076, 1.000000000000000000, 0.8660254037844387076, 1.000000000000000000, 0.8660254037844387076, 1.000000000000000000, 0.8660254037844387076, 1.000000000000000000, 0.8660254037844387076, 1.000000000000000000, 0.8660254037844387076, 1.000000000000000000, 0.8660254037844387076, 1.000000000000000000, 0.8660254037844387076, 1.000000000000000000, 0.8660254037844387076, 1.000000000000000000, 0.8660254037844387076, 1.000000000000000000, 0.8660254037844387076, 1.000000000000000000, 0.8660254037844387076, 1.000000000000000000, 0.8660254037844387076, 1.000000000000000000) ) ) 
 REPRESENTATION_ITEM ( '' )  SURFACE ( )  );
#31090 = CARTESIAN_POINT ( 'NONE',  ( -1.364683531250010295, 5.342708333674750953, 0.7879004041258379498 ) ) ;
#31091 = CARTESIAN_POINT ( 'NONE',  ( -1.500000000000013101, 2.702083334016155636, 0.8660254037844403729 ) ) ;
#31092 = CARTESIAN_POINT ( 'NONE',  ( 5.354985324346148268, 6.526937442883553153, -1.333766491515418817 ) ) ;
#31093 = CARTESIAN_POINT ( 'NONE',  ( 0.07499057489264349119, 0.2503043380940940810, -1.990932473338621778 ) ) ;
#31094 = CARTESIAN_POINT ( 'NONE',  ( 4.716662652015527257, -0.08744826293657045890, 1.839185557975311580 ) ) ;
#31095 = VERTEX_POINT ( 'NONE', #140212 ) ;
#31096 = CARTESIAN_POINT ( 'NONE',  ( -0.6125000000000279110, 2.520833334016120197, -1.060881119635969094 ) ) ;
#31097 = CARTESIAN_POINT ( 'NONE',  ( -6.886651960737580680, 10.12184548991413457, -1.199719254218440723 ) ) ;
#31098 = CARTESIAN_POINT ( 'NONE',  ( -1.225000000000005640, 1.387778780781445676E-14, -1.387778780781445676E-14 ) ) ;
#31099 = CARTESIAN_POINT ( 'NONE',  ( 4.992489932941452935, -1.175987964647656536, 1.764448611491518548 ) ) ;
#31100 = CARTESIAN_POINT ( 'NONE',  ( 6.484877546038077867, 6.460111979999551224, 1.040834085586084257E-14 ) ) ;
#31101 = ORIENTED_EDGE ( 'NONE', *, *, #101284, .T. ) ;
#31102 = CARTESIAN_POINT ( 'NONE',  ( 6.907514182033759553, -0.4531076517439984186, 2.017496682098403937 ) ) ;
#31105 = CARTESIAN_POINT ( 'NONE',  ( 3.263068207883256466, 1.795673413606920565, -0.4063787724192802209 ) ) ;
#31104 = CARTESIAN_POINT ( 'NONE',  ( 2.242426168690789368, -1.824373289281261634, -0.3667376154973446267 ) ) ;
#31103 = CARTESIAN_POINT ( 'NONE',  ( 5.451787166470912993, 6.493411461371761284, -1.082531754730548412 ) ) ;
#31106 = CARTESIAN_POINT ( 'NONE',  ( 8.471147050440139381, 8.777426401801974976, -0.7998128361456281477 ) ) ;
#31107 =( LENGTH_UNIT ( ) NAMED_UNIT ( * ) SI_UNIT ( .MILLI., .METRE. ) );
#31108 = CARTESIAN_POINT ( 'NONE',  ( -6.770317605177755382, 8.992066187497757213, 1.599625672291269396 ) ) ;
#31109 = CARTESIAN_POINT ( 'NONE',  ( -1.743066579297358008E-15, 2.250000000682787160, -1.225000000000020739 ) ) ;
#31110 = CARTESIAN_POINT ( 'NONE',  ( 3.211752199052122503, -0.4303563718574507369, 2.164345902561148005 ) ) ;
#31111 = CARTESIAN_POINT ( 'NONE',  ( 6.116559975520791781, 1.526041019664432508, -1.670398689176689544 ) ) ;
#31112 = CARTESIAN_POINT ( 'NONE',  ( -5.992340707560165569, 8.014150130285418783, 1.443375672974064550 ) ) ;
#31113 = CARTESIAN_POINT ( 'NONE',  ( 5.695527492674265169, 1.670499194714653468, -0.7014341174245084520 ) ) ;
#31114 = CARTESIAN_POINT ( 'NONE',  ( 5.190618481123168593, 1.446159319891277661, -1.256491027437984354 ) ) ;
#31115 = CARTESIAN_POINT ( 'NONE',  ( -1.364683531249997417, 5.321875000341417916, 1.214306433183764966E-14 ) ) ;
#31116 = CIRCLE ( 'NONE', #152157, 0.08000000000000020983 ) ;
#31117 = CARTESIAN_POINT ( 'NONE',  ( 6.069203928793593050, 0.1358119448514639727, -1.865795782587629681 ) ) ;
#31118 = CARTESIAN_POINT ( 'NONE',  ( 5.652756593210860103, -0.4525561148686143009, -1.805067620203390177 ) ) ;
#31119 = CARTESIAN_POINT ( 'NONE',  ( -5.426287360647527258, 6.306760859481674864, -1.047964138152550406 ) ) ;
#31120 = CARTESIAN_POINT ( 'NONE',  ( 6.684453129459355658, -1.736675761049325972, -0.3400495950729911510 ) ) ;
#31121 = CARTESIAN_POINT ( 'NONE',  ( 1.393767942625488532, -2.000731169080074423, 0.2516357431460446992 ) ) ;
#31123 = CARTESIAN_POINT ( 'NONE',  ( 2.877667905955140437, 1.999614821268459020, -0.6613089454029356107 ) ) ;
#31122 = CARTESIAN_POINT ( 'NONE',  ( -8.306341666666730461, 12.84248237775322643, 1.040834085586084257E-14 ) ) ;
#31124 = CARTESIAN_POINT ( 'NONE',  ( 7.639129486296027061, 10.99973593639901814, 1.199719254218460707 ) ) ;
#31126 = CARTESIAN_POINT ( 'NONE',  ( -8.479735010343349089, 11.98044238112085758, 1.199719254218453823 ) ) ;
#31125 = CARTESIAN_POINT ( 'NONE',  ( -1.734723475976807094E-14, 4.000000000000003553, -1.734723475976807094E-14 ) ) ;
#31127 = DIRECTION ( 'NONE',  ( -0.7592566023653005702, 0.6507913734559640506, 0.000000000000000000 ) ) ;
#31128 = CARTESIAN_POINT ( 'NONE',  ( 3.410420005539113841, -2.017668111602511694, -0.09479391224248739922 ) ) ;
#31129 = CARTESIAN_POINT ( 'NONE',  ( 1.364683531249990311, 4.134375000341417028, 1.214306433183764966E-14 ) ) ;
#31130 = CARTESIAN_POINT ( 'NONE',  ( 4.695201269034174452, 4.372156323494968966, 1.214306433183764966E-14 ) ) ;
#31131 = CARTESIAN_POINT ( 'NONE',  ( 3.110779230992101407, 1.568002374463087989, -1.488160049990403078 ) ) ;
#31132 = CARTESIAN_POINT ( 'NONE',  ( 6.610000000000011866, 2.967812824040619191, 2.453181572820534395 ) ) ;
#31134 =( NAMED_UNIT ( * ) SI_UNIT ( $, .STERADIAN. ) SOLID_ANGLE_UNIT ( ) );
#31133 = CARTESIAN_POINT ( 'NONE',  ( 7.367930134383754215, 7.560616343061329125, -0.7998128361456341429 ) ) ;
#31135 = CARTESIAN_POINT ( 'NONE',  ( 9.368320956918608999, 11.95279375453699622, 1.443375672974076540 ) ) ;
#31136 = CARTESIAN_POINT ( 'NONE',  ( 9.150980377513773689, 14.30259500125689698, -7.763699605349790644 ) ) ;
#31137 = CARTESIAN_POINT ( 'NONE',  ( -6.222829318992474157, 10.20379193889247382, 0.000000000000000000 ) ) ;
#31138 = CARTESIAN_POINT ( 'NONE',  ( -1.364683531250012516, 1.030208333674754062, 0.7879004041258379498 ) ) ;
#31139 = CARTESIAN_POINT ( 'NONE',  ( 1.751786407749492014, 2.185395279939935431, -0.1653414253460702699 ) ) ;
#31140 = DIRECTION ( 'NONE',  ( 1.000000000000000000, -0.000000000000000000, -0.000000000000000000 ) ) ;
#31141 = CARTESIAN_POINT ( 'NONE',  ( 2.325404209529509103, -2.741642530189327160E-05, 2.262689075223401236 ) ) ;
#31142 = CARTESIAN_POINT ( 'NONE',  ( -8.857554428429624593, 9.228235009456373206, 0.7998128361456462443 ) ) ;
#31143 = EDGE_CURVE ( 'NONE', #144257, #101488, #142832, .T. ) ;
#31144 = CARTESIAN_POINT ( 'NONE',  ( -3.809477975315625375, 4.507107728365378208, 1.082531754730558626 ) ) ;
#31145 = CARTESIAN_POINT ( 'NONE',  ( 0.6823417656249899377, 3.155208333674754062, 1.181850606188765695 ) ) ;
#31146 = CARTESIAN_POINT ( 'NONE',  ( 6.210774601750883583, 6.933448576277219111, 0.8519936491524527922 ) ) ;
#31147 = CARTESIAN_POINT ( 'NONE',  ( -1.500000000000008216, 11.24999999999999645, 3.469446951953614189E-15 ) ) ;
#31148 = CARTESIAN_POINT ( 'NONE',  ( 5.858531774880875176, 9.849054480754103835, -0.7216878364870458196 ) ) ;
#31149 = CARTESIAN_POINT ( 'NONE',  ( 3.338855477594515175, -1.562335520734370320, 0.8312421073871211208 ) ) ;
#31150 = COLOUR_RGB ( '', 0.31764706, 0.68627451, 0.89019608) ;
#31151 = CARTESIAN_POINT ( 'NONE',  ( 6.352570083819033542, 0.6862697483850827007, 2.097430819677794656 ) ) ;
#31152 = CARTESIAN_POINT ( 'NONE',  ( -0.6823417656250039265, 8.817708333674733723, -1.181850606188755259 ) ) ;
#31153 = CARTESIAN_POINT ( 'NONE',  ( -6.231907884136888676, 7.299589282028351001, -1.199719254218453823 ) ) ;
#31154 = CARTESIAN_POINT ( 'NONE',  ( 4.921500000981174239, -1.427949280599305482, -1.423951169029838315 ) ) ;
#31155 = ORIENTED_EDGE ( 'NONE', *, *, #194375, .F. ) ;
#31156 = CARTESIAN_POINT ( 'NONE',  ( 3.414787578387419309, 1.690673485743508619, 0.8009127983473337542 ) ) ;
#31157 = EDGE_CURVE ( 'NONE', #43349, #55688, #52417, .T. ) ;
#31158 = CARTESIAN_POINT ( 'NONE',  ( 3.414952709633051864, -1.570776679111930640, 1.348709175982481856 ) ) ;
#31159 = CARTESIAN_POINT ( 'NONE',  ( -6.658462837642833421, 8.861568958707010779, 1.443375672974064550 ) ) ;
#31160 = PLANE ( 'NONE',  #46701 ) ;
#31161 = CARTESIAN_POINT ( 'NONE',  ( -10.37923916842784422, 4.890109552615133026, -5.358306740738790097 ) ) ;
#31162 = CARTESIAN_POINT ( 'NONE',  ( -4.009374317532317100, 7.667071904143438310, 0.2036989888780231517 ) ) ;
#31163 = CARTESIAN_POINT ( 'NONE',  ( -1.364683531250012516, 4.551041667008082214, -0.7879004041258300672 ) ) ;
#31164 = CARTESIAN_POINT ( 'NONE',  ( 1.406358598101828283, -1.903450966454448334, -0.1843715739238485085 ) ) ;
#31165 = CARTESIAN_POINT ( 'NONE',  ( 2.365611650783586040, -0.4327418640146083462, 1.913375882425945917 ) ) ;
#31166 = CARTESIAN_POINT ( 'NONE',  ( 1.317732270343049183, -1.591076063098846527, 1.238129638497114549 ) ) ;
#31167 = CARTESIAN_POINT ( 'NONE',  ( -4.716257332707368910, 6.595662536282280719, -1.599625672291271394 ) ) ;
#31169 = CARTESIAN_POINT ( 'NONE',  ( 0.000000000000000000, 6.999999999999992006, 0.000000000000000000 ) ) ;
#31168 = CARTESIAN_POINT ( 'NONE',  ( 7.934546212495622086, 10.28005655271014795, -1.599625672291262513 ) ) ;
#31170 = CARTESIAN_POINT ( 'NONE',  ( 6.714144427970111906, -0.9273952116407166990, -1.739565242892411545 ) ) ;
#31171 = CARTESIAN_POINT ( 'NONE',  ( 1.364683531249986537, 2.655208333674754062, -0.7879004041258239610 ) ) ;
#31172 = CARTESIAN_POINT ( 'NONE',  ( 2.179941694947628683, 1.973542599225884153, -0.3968540688959447116 ) ) ;
#31174 = CARTESIAN_POINT ( 'NONE',  ( 2.513409721704229494, -1.974398269817168483, 0.7648893725459534609 ) ) ;
#31173 = CARTESIAN_POINT ( 'NONE',  ( -6.182154858151506893, 9.195969186943299789, 1.082531754730548412 ) ) ;
#31175 = CARTESIAN_POINT ( 'NONE',  ( 1.436838838544552299, 7.449283400311791148, 4.203727439823582657 ) ) ;
#31176 = CARTESIAN_POINT ( 'NONE',  ( 3.314952806421948672, -1.569539724514938950, 1.350292352848787569 ) ) ;
#31177 = CARTESIAN_POINT ( 'NONE',  ( 5.734172623936983904, 5.654565914206774124, 0.7998128361456352531 ) ) ;
#31179 = CARTESIAN_POINT ( 'NONE',  ( 2.530568227245037605, 6.104080031761181857, 0.000000000000000000 ) ) ;
#31178 = CARTESIAN_POINT ( 'NONE',  ( 5.753879374300719718, 0.8463200818398952663, 1.911864941374420201 ) ) ;
#31181 = ORIENTED_EDGE ( 'NONE', *, *, #159414, .T. ) ;
#31180 = CARTESIAN_POINT ( 'NONE',  ( 3.961776442328440506, 1.811803316853294765, -0.2231971713724384965 ) ) ;
#31182 = CARTESIAN_POINT ( 'NONE',  ( 9.378489572351044856, 11.96465713920816043, -1.599625672291262513 ) ) ;
#31183 = CARTESIAN_POINT ( 'NONE',  ( -1.499999999999993339, 10.64264068711930733, 1.232676135170975238E-14 ) ) ;
#31184 = CARTESIAN_POINT ( 'NONE',  ( 9.680359324772695118, 13.43752487939448947, 8.167046318416051776 ) ) ;
#31185 = CARTESIAN_POINT ( 'NONE',  ( 6.493228066955544442, 1.923254169853494178, -1.081975473724585912 ) ) ;
#31186 = CARTESIAN_POINT ( 'NONE',  ( 1.364683531250000748, 11.31770833367473728, -0.7879004041258355073 ) ) ;
#31187 = VERTEX_POINT ( 'NONE', #187846 ) ;
#31188 = CARTESIAN_POINT ( 'NONE',  ( 4.811142580195256535, 1.587781804131962682, -1.065416552848017284 ) ) ;
#31189 = CARTESIAN_POINT ( 'NONE',  ( -9.972185678051314284, 11.59297036493672017, 1.199719254218462483 ) ) ;
#31190 = CARTESIAN_POINT ( 'NONE',  ( 7.955937213120826357, 8.176348258262782664, 0.7998128361456481317 ) ) ;
#31191 = CARTESIAN_POINT ( 'NONE',  ( 0.6801582343749900117, 2.005208333674748822, 1.178068619123818994 ) ) ;
#31192 =( LENGTH_UNIT ( ) NAMED_UNIT ( * ) SI_UNIT ( .MILLI., .METRE. ) );
#31193 = CARTESIAN_POINT ( 'NONE',  ( 7.321368706613687216, 14.46581668038550994, -9.510808679899710683 ) ) ;
#31194 = CARTESIAN_POINT ( 'NONE',  ( 0.8195642880178370948, 1.096917009463085790, -1.478703137254427924 ) ) ;
#31195 = ORIENTED_EDGE ( 'NONE', *, *, #62276, .F. ) ;
#31196 = CARTESIAN_POINT ( 'NONE',  ( -6.668631453075260396, 8.873432343378178544, -1.599625672291271394 ) ) ;
#31198 = EDGE_CURVE ( 'NONE', #99015, #96867, #180973, .T. ) ;
#31197 = VECTOR ( 'NONE', #212434, 1000.000000000000000 ) ;
#31199 = CARTESIAN_POINT ( 'NONE',  ( 4.727732462671866642, -1.149354582003499159, -1.475719300151681512 ) ) ;
#31200 = CARTESIAN_POINT ( 'NONE',  ( -3.638309248663660345, 7.466720900074724554, 0.3421599456651515103 ) ) ;
#31201 = CARTESIAN_POINT ( 'NONE',  ( 0.4019237886466816012, 10.92633545031537068, -1.499999999999998668 ) ) ;
#31202 = CYLINDRICAL_SURFACE ( 'NONE', #213032, 1.500000000000000222 ) ;
#31203 = CARTESIAN_POINT ( 'NONE',  ( -5.116488771863230589, 7.819496687688390679, 1.149033069458482270 ) ) ;
#31204 = CARTESIAN_POINT ( 'NONE',  ( -6.887178846062128379, 7.137389529935019183, -0.7216878364870278340 ) ) ;
#31205 = CARTESIAN_POINT ( 'NONE',  ( 6.173040012923759257, 6.096301524699504704, -0.7998128361456281477 ) ) ;
#31206 = CARTESIAN_POINT ( 'NONE',  ( 1.199983893365302201, 0.8030756602186311932, -1.798478550607261583 ) ) ;
#31207 = CARTESIAN_POINT ( 'NONE',  ( 2.601185598297011570, -0.1948207814224910128, 2.006963067508853005 ) ) ;
#31208 = CARTESIAN_POINT ( 'NONE',  ( -8.025536864285518490, 11.45054454405341282, -1.199719254218446718 ) ) ;
#31209 = CARTESIAN_POINT ( 'NONE',  ( 4.342354338126830804, 8.288106837781779035, -0.7998128361456381397 ) ) ;
#31210 = CARTESIAN_POINT ( 'NONE',  ( -11.92619526913700057, 11.02781666661243243, -1.328859060402685976 ) ) ;
#31211 = CARTESIAN_POINT ( 'NONE',  ( 2.168174125648382411, -1.346884454587377711, 1.728604079486287137 ) ) ;
#31212 = CARTESIAN_POINT ( 'NONE',  ( -1.499999999999993339, 10.64264068711930733, 1.232676135170975238E-14 ) ) ;
#31213 = CARTESIAN_POINT ( 'NONE',  ( -10.47097470845587175, 11.11055866948701443, 1.040834085586084257E-14 ) ) ;
#31214 = CARTESIAN_POINT ( 'NONE',  ( 1.271070482942026292, 8.436788551174032591, 10.93994114196923029 ) ) ;
#31215 = CARTESIAN_POINT ( 'NONE',  ( -4.303094902415906198, 7.389312076987425648, -1.073240500945132236 ) ) ;
#31216 = CARTESIAN_POINT ( 'NONE',  ( 8.178592977541601527, 10.56477777859713463, 1.599625672291281386 ) ) ;
#31217 = CARTESIAN_POINT ( 'NONE',  ( -9.495441445486425991, 14.82923372934912365, 7.231220947886405348 ) ) ;
#31218 = CARTESIAN_POINT ( 'NONE',  ( 6.536439455564155843, 8.719208346281938304, 1.443375672974065660 ) ) ;
#31219 = VERTEX_POINT ( 'NONE', #9108 ) ;
#31221 = CARTESIAN_POINT ( 'NONE',  ( 1.998691314347844417, -1.974684511280549559, -0.3905480285893418446 ) ) ;
#31220 = CARTESIAN_POINT ( 'NONE',  ( 4.423293856316495187, -1.136390847421838490, -1.448631019334602144 ) ) ;
#31222 = CARTESIAN_POINT ( 'NONE',  ( 2.864987100074483539, -0.7226686165877260759, 2.181857903572166801 ) ) ;
#31224 = CARTESIAN_POINT ( 'NONE',  ( 1.744728380183872218, -0.2665191970635071295, -1.841615994452956873 ) ) ;
#31223 = CARTESIAN_POINT ( 'NONE',  ( -11.33772463945037146, 10.89999999999998259, 3.599999999999999201 ) ) ;
#31225 = CARTESIAN_POINT ( 'NONE',  ( 1.642778471875000035, -3.026041666188708401, -2.845375778867859751 ) ) ;
#31226 = CARTESIAN_POINT ( 'NONE',  ( -9.437721055127425984, 15.48631298644891352, -7.411487926712346130 ) ) ;
#31227 = CARTESIAN_POINT ( 'NONE',  ( 5.168181644781757456, 1.909928461159452251, -0.09994665148223277895 ) ) ;
#31228 = CARTESIAN_POINT ( 'NONE',  ( -9.158696461231359720, 10.64389961198009615, 1.199719254218462483 ) ) ;
#31229 = CARTESIAN_POINT ( 'NONE',  ( -5.397554552016258889, 7.390509292142662723, 1.443375672974058777 ) ) ;
#31231 = CARTESIAN_POINT ( 'NONE',  ( 3.203821283898714345, -1.868584281295191607, 0.09040415888627445495 ) ) ;
#31230 = CARTESIAN_POINT ( 'NONE',  ( 4.704676425016507402, 1.819892833079386651, 1.028999879293402531 ) ) ;
#31232 = CARTESIAN_POINT ( 'NONE',  ( 6.805829924380105034, 9.923590097543378619, 1.082531754730558626 ) ) ;
#31233 = EDGE_CURVE ( 'NONE', #162811, #21086, #89566, .T. ) ;
#31234 = CARTESIAN_POINT ( 'NONE',  ( 5.741722636381445533, 1.839460222191912964, 0.08393339073512617876 ) ) ;
#31235 = CARTESIAN_POINT ( 'NONE',  ( 3.979481780810941949, 4.601482484822914998, 1.199719254218464037 ) ) ;
#31236 = CARTESIAN_POINT ( 'NONE',  ( -2.905110965495596944E-15, 1.687500000000013101, -1.225000000000019851 ) ) ;
#31237 = CARTESIAN_POINT ( 'NONE',  ( 4.846200500028392533, 1.720618765505038006, 0.1221847348328516936 ) ) ;
#31238 = CARTESIAN_POINT ( 'NONE',  ( -6.901263884555985051, 8.010228272525461435, 1.199719254218450271 ) ) ;
#31239 =( NAMED_UNIT ( * ) SI_UNIT ( $, .STERADIAN. ) SOLID_ANGLE_UNIT ( ) );
#31240 = CARTESIAN_POINT ( 'NONE',  ( 1.911686719268508527, 3.274494700676894077, 0.4236673858377237312 ) ) ;
#31241 = SURFACE_SIDE_STYLE ('',( #95187 ) ) ;
#31242 = CARTESIAN_POINT ( 'NONE',  ( 4.504835797669192843, 0.5730007755406724135, 2.094059341655955198 ) ) ;
#31243 = CARTESIAN_POINT ( 'NONE',  ( 3.369579884941567016, 1.780956498284639533, -0.4009276245297774266 ) ) ;
#31244 = CARTESIAN_POINT ( 'NONE',  ( 1.252704021237858401, -0.4712815170893420724, -1.904206577484176321 ) ) ;
#31245 = CARTESIAN_POINT ( 'NONE',  ( 5.612555052430599822, 2.041346303960121400, 0.5620598648080311621 ) ) ;
#31246 = B_SPLINE_CURVE_WITH_KNOTS ( 'NONE', 3,
 ( #15493, #147664, #66362, #213681 ),
 .UNSPECIFIED., .F., .F.,
 ( 4, 4 ),
 ( 0.001636132410657741747, 0.002375893410536020125 ),
 .UNSPECIFIED. ) ;
#31247 = EDGE_CURVE ( 'NONE', #188712, #7055, #194259, .T. ) ;
#31249 = CARTESIAN_POINT ( 'NONE',  ( -0.6823417656249969321, 3.780208333674754506, -1.181850606188749264 ) ) ;
#31248 = CARTESIAN_POINT ( 'NONE',  ( 6.269073568569841548, 2.194993726949866719, -0.6609628413071825248 ) ) ;
#31250 = CARTESIAN_POINT ( 'NONE',  ( -10.44369227015510049, 5.112964020592959180, 5.232143560358710310 ) ) ;
#31251 = CARTESIAN_POINT ( 'NONE',  ( 8.320953590485093088, 10.73086516036454618, 1.599625672291281386 ) ) ;
#31252 = PRESENTATION_LAYER_ASSIGNMENT (  '', '', ( #131643 ) ) ;
#31253 = CARTESIAN_POINT ( 'NONE',  ( 2.051582899450168362, -1.892833867889589960, 0.9560217657286762538 ) ) ;
#31254 = CARTESIAN_POINT ( 'NONE',  ( -4.500943810056945438, 5.313817868896925312, 1.082531754730560403 ) ) ;
#31255 = SURFACE_STYLE_USAGE ( .BOTH. , #109370 ) ;
#31256 = CARTESIAN_POINT ( 'NONE',  ( -4.731432421044883263, 5.582721248382882528, -1.082531754730543971 ) ) ;
#31257 = CARTESIAN_POINT ( 'NONE',  ( 6.051681997923831879, 1.638823605779341053, 1.424080724270002873 ) ) ;
#31259 = CARTESIAN_POINT ( 'NONE',  ( 0.7500000000000006661, 13.86458333401613352, 1.299038105676657340 ) ) ;
#31258 = CARTESIAN_POINT ( 'NONE',  ( 6.883263157960358924, 4.692138088316172073, 2.616388454592593504 ) ) ;
#31261 = VERTEX_POINT ( 'NONE', #97850 ) ;
#31260 = CARTESIAN_POINT ( 'NONE',  ( 2.895431823567701457, -0.1657752626464791268, -2.215182847160178881 ) ) ;
#31262 = CARTESIAN_POINT ( 'NONE',  ( 6.574846728087075931, -0.8593996854794653251, 1.822268861383633531 ) ) ;
#31264 = CARTESIAN_POINT ( 'NONE',  ( 5.682507089483013196, 1.232960659210121879, -1.653321649057968967 ) ) ;
#31263 = CARTESIAN_POINT ( 'NONE',  ( 3.161022370280501814, 6.839609865302569425, 0.000000000000000000 ) ) ;
#31266 = CARTESIAN_POINT ( 'NONE',  ( 0.000000000000000000, -2.187499999999998668, -4.012584370867899430 ) ) ;
#31265 = CARTESIAN_POINT ( 'NONE',  ( 4.369470645354133431, 8.319742529546998000, 0.7998128361456271485 ) ) ;
#31267 = CARTESIAN_POINT ( 'NONE',  ( 6.170896192875352959, 7.228408975556602556, 1.199719254218453823 ) ) ;
#31268 = CARTESIAN_POINT ( 'NONE',  ( 3.285556943750000070, -0.2843749995220419269, 0.000000000000000000 ) ) ;
#31269 = CARTESIAN_POINT ( 'NONE',  ( 0.1333542156527321720, 1.344858830485482937, -2.298444861300387387 ) ) ;
#31270 = CARTESIAN_POINT ( 'NONE',  ( 5.583513413114173041, -0.8223277247318347971, 1.647484189299788682 ) ) ;
#31271 = EDGE_CURVE ( 'NONE', #43706, #30492, #74559, .T. ) ;
#31272 = CARTESIAN_POINT ( 'NONE',  ( 4.171104814498611368, 8.018039383557042044, 0.7998128361456321445 ) ) ;
#31273 = CARTESIAN_POINT ( 'NONE',  ( 1.518105509412637444, 1.162241833864360974, -1.274548180342775838 ) ) ;
#31274 = CARTESIAN_POINT ( 'NONE',  ( 1.323454262349359922, -1.463929862531297976, -1.387097294446783868 ) ) ;
#31275 = CARTESIAN_POINT ( 'NONE',  ( 1.530362799304554100, -1.938799508460651522, 1.234721073783265233 ) ) ;
#31276 = CARTESIAN_POINT ( 'NONE',  ( 0.6823417656249899377, 4.238541667008085767, -1.181850606188754593 ) ) ;
#31277 = CARTESIAN_POINT ( 'NONE',  ( 2.179354884421313088, -0.1095372306593382361, -2.259850278934079970 ) ) ;
#31278 = CARTESIAN_POINT ( 'NONE',  ( 4.195997148085639061, -0.8063668458072065226, 1.945788449171739876 ) ) ;
#31279 = CARTESIAN_POINT ( 'NONE',  ( -6.861835142292179057, 9.098836647464588978, 1.443375672974064550 ) ) ;
#31280 = CARTESIAN_POINT ( 'NONE',  ( 2.090717947541526289, 1.542569122296926221, -0.8672550169683733712 ) ) ;
#31281 = CARTESIAN_POINT ( 'NONE',  ( 6.986529229743720926, 7.045372277656132276, -0.7998128361456281477 ) ) ;
#31282 = CARTESIAN_POINT ( 'NONE',  ( 6.197485614778188712, 6.403023770095574108, -0.7216878364870458196 ) ) ;
#31283 = CARTESIAN_POINT ( 'NONE',  ( -4.355193658487827690, 6.104145239700998538, -1.599625672291256295 ) ) ;
#31284 = CARTESIAN_POINT ( 'NONE',  ( 0.7499999999999902300, 1.983333333333357817, 1.299038105676669330 ) ) ;
#31285 = CARTESIAN_POINT ( 'NONE',  ( 5.888988880356018640, -2.109219445749145994, -0.6973366327849057633 ) ) ;
#31286 = CARTESIAN_POINT ( 'NONE',  ( 3.574349206294104242, -2.111947977397998777, -0.5846811180381800144 ) ) ;
#31287 = CARTESIAN_POINT ( 'NONE',  ( -5.461236948206312114, 5.265864615862458464, 0.7998128361456341429 ) ) ;
#31288 = DIRECTION ( 'NONE',  ( 0.9982742078614211811, 0.000000000000000000, 0.05872483221476467591 ) ) ;
#31289 = EDGE_CURVE ( 'NONE', #8487, #201520, #73810, .T. ) ;
#31290 = CARTESIAN_POINT ( 'NONE',  ( 6.481110812017948142, -1.938455339442773706, -0.8599551062365147214 ) ) ;
#31291 = CARTESIAN_POINT ( 'NONE',  ( 1.364683531249988535, 2.613541667008089764, 0.7879004041258500513 ) ) ;
#31292 = CARTESIAN_POINT ( 'NONE',  ( -1.402160292154681736E-14, 9.421875000341398021, 1.575800808251682339 ) ) ;
#31293 = CARTESIAN_POINT ( 'NONE',  ( -4.948362879307902418, 4.875437568721725512, 1.214306433183764966E-14 ) ) ;
#31294 = CARTESIAN_POINT ( 'NONE',  ( 6.275647701495586261, 0.3610785225884837746, -2.089460823871174266 ) ) ;
#31295 = CARTESIAN_POINT ( 'NONE',  ( -5.478903473698247595, 8.445785581739666981, -1.082531754730549967 ) ) ;
#31296 = ORIENTED_EDGE ( 'NONE', *, *, #69557, .F. ) ;
#31298 = CARTESIAN_POINT ( 'NONE',  ( 0.000000000000000000, 11.37999999999998302, 0.000000000000000000 ) ) ;
#31297 = CARTESIAN_POINT ( 'NONE',  ( -5.641601317062259646, 5.754492089426966217, -0.7216878364870338292 ) ) ;
#31299 = CARTESIAN_POINT ( 'NONE',  ( 6.342516933094585418, 6.294024598232139667, 1.040834085586084257E-14 ) ) ;
#31300 = CARTESIAN_POINT ( 'NONE',  ( 6.462460624273299814, -1.686435539877573220, -0.7394478613861471539 ) ) ;
#31301 = CARTESIAN_POINT ( 'NONE',  ( -5.612892248198118494, 5.720998175752135317, -0.08478118863167052877 ) ) ;
#31302 = DIRECTION ( 'NONE',  ( -0.000000000000000000, -1.000000000000000000, -0.000000000000000000 ) ) ;
#31303 = CARTESIAN_POINT ( 'NONE',  ( -0.6823417656249969321, 4.530208333674755394, -1.181850606188749264 ) ) ;
#31304 = CARTESIAN_POINT ( 'NONE',  ( 2.137881509367345778, 0.3822841233627124469, 1.697745509426834332 ) ) ;
#31305 = CARTESIAN_POINT ( 'NONE',  ( -4.329838433221154581, 8.065578932188461891, -0.1632719438462266193 ) ) ;
#31306 = CARTESIAN_POINT ( 'NONE',  ( -1.402160292154681736E-14, 0.3843750003414230232, 1.575800808251672791 ) ) ;
#31307 = CARTESIAN_POINT ( 'NONE',  ( 6.438358464623771482, 2.137424745569570295, 0.3223339197731683869 ) ) ;
#31308 = CARTESIAN_POINT ( 'NONE',  ( -9.001723924469462901, 12.58942944760136484, -1.199719254218446718 ) ) ;
#31309 = CARTESIAN_POINT ( 'NONE',  ( -5.368665640887164692, 9.207267647769599606, 0.000000000000000000 ) ) ;
#31310 = CARTESIAN_POINT ( 'NONE',  ( 5.998930166150279852, 1.769978137569449883, -1.240765152474863520 ) ) ;
#31312 = VERTEX_POINT ( 'NONE', #131449 ) ;
#31311 = CARTESIAN_POINT ( 'NONE',  ( -1.403499169902660437, 7.376709478543006071, -4.304123474984413278 ) ) ;
#31313 = CARTESIAN_POINT ( 'NONE',  ( -1.364683531249997417, 4.009375000341424133, 1.214306433183764966E-14 ) ) ;
#31314 = CARTESIAN_POINT ( 'NONE',  ( 6.239525796224010712, -1.426203020326064275, -1.361167568813693718 ) ) ;
#31315 = CARTESIAN_POINT ( 'NONE',  ( 5.343005094570719038, -0.9615459055183853687, 1.442522970604209531 ) ) ;
#31316 = EDGE_CURVE ( 'NONE', #180001, #191870, #101347, .T. ) ;
#31318 = CARTESIAN_POINT ( 'NONE',  ( 2.191216702865448784, 1.696344223602393786, 1.387594652289561248 ) ) ;
#31317 = CARTESIAN_POINT ( 'NONE',  ( 1.360316468749978469, -0.4843749996586016460, -3.816391647148975608E-14 ) ) ;
#31319 = CARTESIAN_POINT ( 'NONE',  ( 3.522812192065057690, 1.465757825172078865, -1.782263946013421974 ) ) ;
#31320 = B_SPLINE_CURVE_WITH_KNOTS ( 'NONE', 3,
 ( #202898, #72911, #36143, #88115 ),
 .UNSPECIFIED., .F., .F.,
 ( 4, 4 ),
 ( 0.000000000000000000, 0.0002661342691797352611 ),
 .UNSPECIFIED. ) ;
#31321 = CARTESIAN_POINT ( 'NONE',  ( 6.028604891774052454, 1.984808026635048961, 0.5540661066990509864 ) ) ;
#31322 = CARTESIAN_POINT ( 'NONE',  ( 1.464679669172624488, 0.1433081720705318696, -1.936712990118959032 ) ) ;
#31323 = CARTESIAN_POINT ( 'NONE',  ( -5.327991180046197428, 8.199444895820425572, 1.082531754730548412 ) ) ;
#31325 = EDGE_CURVE ( 'NONE', #24517, #153088, #195337, .T. ) ;
#31324 = CARTESIAN_POINT ( 'NONE',  ( -4.034433228518296666, 6.864533312316751790, -1.199719254218450271 ) ) ;
#31326 = DIRECTION ( 'NONE',  ( -0.8583236685137333177, 0.5131086435338296781, -8.673617379884052827E-15 ) ) ;
#31327 = CARTESIAN_POINT ( 'NONE',  ( 4.183913158364858553, 2.056144659531285779, -0.5182805708664262045 ) ) ;
#31328 = CARTESIAN_POINT ( 'NONE',  ( 1.899064777474347654, -0.9530127170578571727, -1.777010740487514173 ) ) ;
#31329 = CARTESIAN_POINT ( 'NONE',  ( -4.880572110795192486, 8.637825195995631589, 1.214306433183764966E-14 ) ) ;
#31330 = CARTESIAN_POINT ( 'NONE',  ( 5.051906976816819217, 0.6964463896041681590, -2.094057263239030853 ) ) ;
#31331 = CARTESIAN_POINT ( 'NONE',  ( 1.001543065824772753E-15, -0.8093749995220410609, 3.793834371823811669 ) ) ;
#31332 = DIRECTION ( 'NONE',  ( 8.659560562354884787E-17, -0.7071067811865513475, 0.7071067811865435759 ) ) ;
#31333 = CARTESIAN_POINT ( 'NONE',  ( 0.02954982209854748257, -1.120125052174587577, -1.442194003765177257 ) ) ;
#31334 = CARTESIAN_POINT ( 'NONE',  ( -7.045397100956844127, 8.248660034984974132, -1.199719254218452047 ) ) ;
#31336 = CARTESIAN_POINT ( 'NONE',  ( -10.41114276008726058, -8.296408557650112314, 0.1817271728542615705 ) ) ;
#31335 = CARTESIAN_POINT ( 'NONE',  ( -5.569768141569340969, 7.516503378918355516, 1.348759926630802131 ) ) ;
#31337 = CARTESIAN_POINT ( 'NONE',  ( 0.6125000000000001554, 2.166666666666670960, -1.060881119635941339 ) ) ;
#31338 = ORIENTED_EDGE ( 'NONE', *, *, #166799, .F. ) ;
#31339 = CARTESIAN_POINT ( 'NONE',  ( 4.293860741714614626, -0.7905101867788848491, 1.903454510683154188 ) ) ;
#31340 = B_SPLINE_CURVE_WITH_KNOTS ( 'NONE', 3,
 ( #75644, #188310, #155831, #7415, #65740, #12743, #29024, #130847, #63649, #195784 ),
 .UNSPECIFIED., .F., .F.,
 ( 4, 2, 2, 2, 4 ),
 ( 0.000000000000000000, 0.0004096327454563874798, 0.0008192654909127749597, 0.001228898236369162494, 0.001638530981825549919 ),
 .UNSPECIFIED. ) ;
#31341 = PLANE ( 'NONE',  #12861 ) ;
#31342 = UNCERTAINTY_MEASURE_WITH_UNIT (LENGTH_MEASURE( 1.000000000000000082E-05 ), #63187, 'distance_accuracy_value', 'NONE');
#31343 = CARTESIAN_POINT ( 'NONE',  ( 0.08888683327021307257, 6.492044364012829583, -3.106763327641859362 ) ) ;
#31344 = CARTESIAN_POINT ( 'NONE',  ( -3.893162665418476109, 7.693773542963529444, 1.040834085586084257E-14 ) ) ;
#31345 = CARTESIAN_POINT ( 'NONE',  ( -4.034433228518296666, 6.864533312316751790, -1.199719254218450271 ) ) ;
#31346 = CARTESIAN_POINT ( 'NONE',  ( 3.246744516521868018, 1.970913372098213712, 0.4403762775553735631 ) ) ;
#31347 = CARTESIAN_POINT ( 'NONE',  ( -1.402160292154681736E-14, 1.337500000000025446, -1.732050807568863648 ) ) ;
#31348 = CARTESIAN_POINT ( 'NONE',  ( 9.246297574839974942, 11.81043314211192019, 1.443375672974076540 ) ) ;
#31349 = CARTESIAN_POINT ( 'NONE',  ( 6.877010230629674759, 9.046264573866535486, 1.599625672291281386 ) ) ;
#31350 = CARTESIAN_POINT ( 'NONE',  ( 3.608323775901512764, -0.8336323056173270407, -1.884943839506166174 ) ) ;
#31351 = CARTESIAN_POINT ( 'NONE',  ( 6.727182134110200273, 0.5640974741700152117, 2.241195997201197443 ) ) ;
#31352 = CARTESIAN_POINT ( 'NONE',  ( 4.924636110261782385, 6.768494766770632332, 1.599625672291267398 ) ) ;
#31353 = CARTESIAN_POINT ( 'NONE',  ( -0.2408018239684096284, 1.329574536483958846, -2.350731018214331947 ) ) ;
#31354 = CARTESIAN_POINT ( 'NONE',  ( 1.148114065366242498, -1.452583890646602205, 1.131155481815901753 ) ) ;
#31355 = CARTESIAN_POINT ( 'NONE',  ( 0.3468381721418262731, 2.301974930567828537, 0.1634500305177730706 ) ) ;
#31356 = CARTESIAN_POINT ( 'NONE',  ( 6.384963997392946844, 6.413822516572072807, 0.7998128361456352531 ) ) ;
#31357 = CARTESIAN_POINT ( 'NONE',  ( 3.022914066069124051, 2.034213141994867247, 0.7313807043239917149 ) ) ;
#31358 = CARTESIAN_POINT ( 'NONE',  ( -2.955314298098991266, 6.391691081183366485, 0.7216878364870317197 ) ) ;
#31359 = CARTESIAN_POINT ( 'NONE',  ( 1.428923106112218067, -1.700960256238340573, 1.082842518468102089 ) ) ;
#31360 = CARTESIAN_POINT ( 'NONE',  ( 2.495865491978021211, 2.229134443137513966, 0.5594839687708874632 ) ) ;
#31361 = CARTESIAN_POINT ( 'NONE',  ( 4.222669843016465308, 3.519858668466394835, -2.499999999999995115 ) ) ;
#31362 = CARTESIAN_POINT ( 'NONE',  ( -0.3833105440376022299, 6.967102400362891856, 3.825703835310487300 ) ) ;
#31363 = CARTESIAN_POINT ( 'NONE',  ( 4.399269495383588691, 1.582840427583383613, 1.175083439883710890 ) ) ;
#31364 = CARTESIAN_POINT ( 'NONE',  ( 5.085172837459294826, 1.651341431264556014, 1.157102043685846793 ) ) ;
#31366 = CARTESIAN_POINT ( 'NONE',  ( 10.04622863760192963, 10.82294762006482713, -0.7216878364870257245 ) ) ;
#31365 = CARTESIAN_POINT ( 'NONE',  ( -1.201851678989727383E-14, 2.696875000341417916, -1.575800808251660134 ) ) ;
#31368 = CARTESIAN_POINT ( 'NONE',  ( 6.533818191484063398, -1.374270492279753286, -1.595981979862278077 ) ) ;
#31367 = CARTESIAN_POINT ( 'NONE',  ( -5.540478329478883524, 9.615641817700700145, 0.000000000000000000 ) ) ;
#31369 = CARTESIAN_POINT ( 'NONE',  ( 6.268043187460373922, -2.055199631210803624, 0.2494731385529954104 ) ) ;
#31370 = CARTESIAN_POINT ( 'NONE',  ( 5.819474248763732760, 7.812472595022922128, -1.599625672291262513 ) ) ;
#31371 = CARTESIAN_POINT ( 'NONE',  ( -7.223796917982883592, 7.322184580601816428, -0.7998128361456291469 ) ) ;
#31372 = CARTESIAN_POINT ( 'NONE',  ( 1.981527703613512825, 3.480048614628221681, -0.4617793045968336396 ) ) ;
#31373 = CARTESIAN_POINT ( 'NONE',  ( 3.907068546088189986, 1.690197745946390162, 1.014639218175046764 ) ) ;
#31374 = CARTESIAN_POINT ( 'NONE',  ( 6.082287225941254150, 1.041776932085249907, 1.730260143339139134 ) ) ;
#31375 = CARTESIAN_POINT ( 'NONE',  ( 1.499999999999987121, 0.5354166673494816786, 0.8660254037844524744 ) ) ;
#31376 = CARTESIAN_POINT ( 'NONE',  ( 4.389522222404328211, 2.062498103173298514, -1.035318202965694434 ) ) ;
#31377 = CARTESIAN_POINT ( 'NONE',  ( 2.184505357994303232, 1.191016756910455943, -1.683754781088636632 ) ) ;
#31378 = CARTESIAN_POINT ( 'NONE',  ( 8.459924665247367415, 8.972259652317825740, -0.7216878364870267237 ) ) ;
#31379 = CARTESIAN_POINT ( 'NONE',  ( 5.554000203453580475, 6.508696987897830688, -1.199719254218452047 ) ) ;
#31380 = CARTESIAN_POINT ( 'NONE',  ( 4.411198876399872404, 6.239761003923544713, -1.599625672291273171 ) ) ;
#31381 = CARTESIAN_POINT ( 'NONE',  ( 0.6823417656249882723, 0.2385416670080825474, -1.181850606188749264 ) ) ;
#31382 = CARTESIAN_POINT ( 'NONE',  ( 3.203469434578891661, 6.959407783642502565, -0.7998128361456362523 ) ) ;
#31383 = CARTESIAN_POINT ( 'NONE',  ( 7.605760987142057061, 7.975735361194951523, -0.7216878364870267237 ) ) ;
#31384 = CARTESIAN_POINT ( 'NONE',  ( 4.475155579853315579, 1.983319414854123552, 0.8838481202026007288 ) ) ;
#31385 = CYLINDRICAL_SURFACE ( 'NONE', #96269, 1.250000000000000000 ) ;
#31387 = CARTESIAN_POINT ( 'NONE',  ( 2.841158510722852970, 0.6603703904487292498, -1.718939526767604420 ) ) ;
#31386 = CARTESIAN_POINT ( 'NONE',  ( -4.785665035943912571, 4.685623418130398399, 1.214306433183764966E-14 ) ) ;
#31388 = CARTESIAN_POINT ( 'NONE',  ( 0.6823417656249899377, 4.426041667008086655, -1.181850606188754593 ) ) ;
#31389 = CARTESIAN_POINT ( 'NONE',  ( 6.040607902356621928, -1.852314659301615096, 1.170993205287726990 ) ) ;
#31390 = CARTESIAN_POINT ( 'NONE',  ( 8.362811809344231406, 14.02572535640353735, 8.606655576677448849 ) ) ;
#31391 = CARTESIAN_POINT ( 'NONE',  ( 6.245044592044297183, -1.915350782734099200, 1.204081839623271311 ) ) ;
#31392 = CARTESIAN_POINT ( 'NONE',  ( -5.338497050760650176, 6.533440992188984886, -1.368045069562271010 ) ) ;
#31393 = CARTESIAN_POINT ( 'NONE',  ( 4.684384365712907616, 8.380862967975740929, 0.5977175665230231028 ) ) ;
#31394 = VECTOR ( 'NONE', #110129, 1000.000000000000000 ) ;
#31395 = CARTESIAN_POINT ( 'NONE',  ( -6.265276382846530545, 6.482112999508623297, 0.000000000000000000 ) ) ;
#31396 = CARTESIAN_POINT ( 'NONE',  ( 2.943528747942701695, 6.448217615992859919, 0.000000000000000000 ) ) ;
#31397 = CARTESIAN_POINT ( 'NONE',  ( 6.327411112729964593, -1.665570200489007169, 0.5986406977509810545 ) ) ;
#31398 = CARTESIAN_POINT ( 'NONE',  ( 0.6823417656249934904, 12.44270833367473017, 1.181850606188764807 ) ) ;
#31399 = CARTESIAN_POINT ( 'NONE',  ( 4.617841973404108735, -0.5345865524139911118, 1.940763608534997520 ) ) ;
#31400 = B_SPLINE_CURVE_WITH_KNOTS ( 'NONE', 3,
 ( #76121, #205032, #40440, #174718, #43648, #8983, #26291, #58805, #89193, #190921, #41510, #59869 ),
 .UNSPECIFIED., .F., .F.,
 ( 4, 2, 2, 2, 2, 4 ),
 ( 0.002160919429045905869, 0.002539139494017131175, 0.002917359558988356916, 0.003673799688930807529, 0.004430239818873258142, 0.005186679948815707888 ),
 .UNSPECIFIED. ) ;
#31401 = CARTESIAN_POINT ( 'NONE',  ( 7.657657833620182153, 7.828355648845348291, -0.7998128361456281477 ) ) ;
#31402 = CARTESIAN_POINT ( 'NONE',  ( 2.520660759794272732, 1.376564137786383091, -1.593852158419235332 ) ) ;
#31403 = CARTESIAN_POINT ( 'NONE',  ( 2.653800294728881681, 1.026947457930127872, 1.616878242289141676 ) ) ;
#31404 = CARTESIAN_POINT ( 'NONE',  ( 5.034155109375821446, 4.767602470560229122, -0.7998128361456221525 ) ) ;
#31405 = CARTESIAN_POINT ( 'NONE',  ( 3.350016042381760872, -0.8005406348832925234, 1.799716665148870964 ) ) ;
#31406 = CARTESIAN_POINT ( 'NONE',  ( 1.533845512228737551, 0.9248708299973290581, -1.625957014461040906 ) ) ;
#31407 = CARTESIAN_POINT ( 'NONE',  ( 1.557006721180295150, 1.605793932651664813, -1.126831546849601740 ) ) ;
#31410 = ORIENTED_EDGE ( 'NONE', *, *, #43730, .F. ) ;
#31409 = CARTESIAN_POINT ( 'NONE',  ( -0.1581436608063293003, -1.178060542814472367, -1.506996232563104776 ) ) ;
#31408 = CARTESIAN_POINT ( 'NONE',  ( 4.406709194360526993, 1.330975820509268104, -1.097133727364963729 ) ) ;
#31412 = CARTESIAN_POINT ( 'NONE',  ( 4.663641653420880218, 8.384739662392275861, -0.7216878364870207285 ) ) ;
#31411 = CARTESIAN_POINT ( 'NONE',  ( 1.664966938652842954, -1.558911317520403239, 1.562347339584921002 ) ) ;
#31413 = CARTESIAN_POINT ( 'NONE',  ( 1.364683531249986537, 0.4677083336747514530, -0.7879004041258309554 ) ) ;
#31414 = CARTESIAN_POINT ( 'NONE',  ( 11.84668730067608600, 10.89999999999998259, 1.399999999999998357 ) ) ;
#31415 = CARTESIAN_POINT ( 'NONE',  ( -1.299038105676657340, 6.499999999999999112, 0.7500000000000006661 ) ) ;
#31416 = CARTESIAN_POINT ( 'NONE',  ( 6.673079560224744355, -7.008190897455786939, -6.761669295867157814 ) ) ;
#31417 = CARTESIAN_POINT ( 'NONE',  ( 6.420769920452011448, -1.468259139554881409, 1.459777494992514857 ) ) ;
#31418 = CARTESIAN_POINT ( 'NONE',  ( 0.6607010325807397555, -0.6960017893198193750, -1.950014918625786020 ) ) ;
#31419 = CARTESIAN_POINT ( 'NONE',  ( -1.499999999999997780, 1.650000000000019451, 0.000000000000000000 ) ) ;
#31420 = CARTESIAN_POINT ( 'NONE',  ( 5.937581207780954884, 9.014596278131406848, -1.199719254218440723 ) ) ;
#31421 = CARTESIAN_POINT ( 'NONE',  ( -7.690499447449645309, 9.995335326823163058, 1.599625672291295375 ) ) ;
#31422 = CARTESIAN_POINT ( 'NONE',  ( 5.740951700743842423, 5.662474837148078421, -0.7998128361456481317 ) ) ;
#31423 = CARTESIAN_POINT ( 'NONE',  ( 5.549516566986255839, -1.916978305411633166, 0.9067721062034905799 ) ) ;
#31424 = CARTESIAN_POINT ( 'NONE',  ( 4.706615602599436343, 5.520081620234675412, 1.199719254218452935 ) ) ;
#31425 = CARTESIAN_POINT ( 'NONE',  ( -0.6823417656250003738, 1.217708333674752286, -1.181850606188749264 ) ) ;
#31426 = ORIENTED_EDGE ( 'NONE', *, *, #203130, .T. ) ;
#31427 = CARTESIAN_POINT ( 'NONE',  ( -1.402160292154681736E-14, 2.337500000000022560, -1.732050807568863648 ) ) ;
#31429 = CARTESIAN_POINT ( 'NONE',  ( 4.359110081993588182, 5.044382169536003602, -1.199719254218452047 ) ) ;
#31428 = CARTESIAN_POINT ( 'NONE',  ( 6.619590441841329387, 0.3365870006281460047, -1.932621868259084330 ) ) ;
#31430 = CARTESIAN_POINT ( 'NONE',  ( 4.235703761680151835, -1.880146911114020325, -0.7282675588539261335 ) ) ;
#31431 = CARTESIAN_POINT ( 'NONE',  ( 3.573361294032686430, 1.391295603808204051, 1.317194196901736669 ) ) ;
#31432 = CARTESIAN_POINT ( 'NONE',  ( -1.896367326442726542, 3.293421909012321347, -0.4056650308922968851 ) ) ;
#31433 = CARTESIAN_POINT ( 'NONE',  ( 1.505704256594592838, -2.174480876681058827, 0.2726767719730335826 ) ) ;
#31434 = CARTESIAN_POINT ( 'NONE',  ( 0.1333692844072802142, 0.2389375359408679178, -2.087895146362698906 ) ) ;
#31435 = CARTESIAN_POINT ( 'NONE',  ( 2.846779338809723559, -1.557328454271855955, 1.035869100625155470 ) ) ;
#31436 = CARTESIAN_POINT ( 'NONE',  ( -1.402160292154681736E-14, 1.118750000682820378, -1.732050807568863648 ) ) ;
#31437 = CARTESIAN_POINT ( 'NONE',  ( -6.398558430645608475, 9.552403038140164782, -1.199719254218440723 ) ) ;
#31439 = CARTESIAN_POINT ( 'NONE',  ( 5.308266703545434062, 1.260341450243172678, -1.701113402177101053 ) ) ;
#31438 = CARTESIAN_POINT ( 'NONE',  ( -5.260200412422220140, 5.239248024021764039, -0.7216878364870207285 ) ) ;
#31440 = CARTESIAN_POINT ( 'NONE',  ( -1.402160292154681736E-14, 8.484375000341403350, 1.575800808251682339 ) ) ;
#31442 = CARTESIAN_POINT ( 'NONE',  ( -6.903036488013351679, 8.082572653217566128, -1.199719254218452047 ) ) ;
#31441 = CARTESIAN_POINT ( 'NONE',  ( 2.630511997247253486, 0.2585083551314356631, 2.074647729848762889 ) ) ;
#31444 = ORIENTED_EDGE ( 'NONE', *, *, #186498, .T. ) ;
#31443 = CARTESIAN_POINT ( 'NONE',  ( 1.342334339533798104, 0.3310447913058271463, 1.692513552724637771 ) ) ;
#31445 = CARTESIAN_POINT ( 'NONE',  ( 5.099838337034727331, 9.101561826515851550, -0.7998128361456281477 ) ) ;
#31446 = EDGE_CURVE ( 'NONE', #89957, #121080, #87603, .T. ) ;
#31447 = CARTESIAN_POINT ( 'NONE',  ( -1.101813147103377633, 13.26515898734009369, 0.9875499716500963920 ) ) ;
#31448 = CARTESIAN_POINT ( 'NONE',  ( 0.000000000000000000, -9.911192057434348612, 9.579665964948883783 ) ) ;
#31449 = CARTESIAN_POINT ( 'NONE',  ( -9.367496997601190145, 14.57669131240758276, 7.413898975931879853 ) ) ;
#31451 = CARTESIAN_POINT ( 'NONE',  ( 7.714226216051361718, 11.94375498546120795, -0.7216878364870267237 ) ) ;
#31450 = CARTESIAN_POINT ( 'NONE',  ( 6.714312387265682247, 8.856450423275211037, 1.599625672291281386 ) ) ;
#31452 = VERTEX_POINT ( 'NONE', #113085 ) ;
#31453 = LINE ( 'NONE', #30389, #30448 ) ;
#31454 = MECHANICAL_DESIGN_GEOMETRIC_PRESENTATION_REPRESENTATION (  '', ( #145589 ), #58955 ) ;
#31456 = CARTESIAN_POINT ( 'NONE',  ( 1.488595082971344352, -1.720062743487455581, -0.5684112265044569678 ) ) ;
#31455 = CARTESIAN_POINT ( 'NONE',  ( 6.475954649182838807, 7.584310507915338562, 1.199719254218452047 ) ) ;
#31457 = CARTESIAN_POINT ( 'NONE',  ( -7.369020184227459858, 8.555943955475521889, 1.199719254218450271 ) ) ;
#31458 = CARTESIAN_POINT ( 'NONE',  ( 3.832150974156964818, 7.622593236491780999, 1.040834085586084257E-14 ) ) ;
#31459 = CARTESIAN_POINT ( 'NONE',  ( 6.873057527484919937, 6.983264968346048818, 0.7998128361456352531 ) ) ;
#31460 = CARTESIAN_POINT ( 'NONE',  ( 6.639320575229255006, 7.629137130509086262, 2.396737603865983779 ) ) ;
#31461 = CIRCLE ( 'NONE', #48776, 0.2000000000000000389 ) ;
#31462 = DIRECTION ( 'NONE',  ( 1.207943261119674327E-30, 2.168404344971008079E-15, -1.000000000000000000 ) ) ;
#31463 = CARTESIAN_POINT ( 'NONE',  ( 4.067670533747345551, 7.502496534258641603, 0.5382987142239087364 ) ) ;
#31464 = CARTESIAN_POINT ( 'NONE',  ( 7.944714827928033962, 12.21265836598400689, 0.7216878364870438212 ) ) ;
#31465 = EDGE_LOOP ( 'NONE', ( #155483, #128240, #20598, #120185 ) ) ;
#31466 = EDGE_CURVE ( 'NONE', #108115, #76056, #29643, .T. ) ;
#31467 = CARTESIAN_POINT ( 'NONE',  ( 2.875287963320713569, -0.1852811808005799254, 1.851819283609082323 ) ) ;
#31468 = EDGE_CURVE ( 'NONE', #73686, #10457, #156727, .T. ) ;
#31469 = CARTESIAN_POINT ( 'NONE',  ( -0.07089544441234334193, -1.481030113823898375, -1.214736957437832832 ) ) ;
#31470 = CARTESIAN_POINT ( 'NONE',  ( 6.545928648987922038, 0.7364953880720639390, -1.780233924599901929 ) ) ;
#31471 = CARTESIAN_POINT ( 'NONE',  ( 1.220146605508150803E-14, 11.68749999999999822, -1.499999999999998446 ) ) ;
#31472 = CARTESIAN_POINT ( 'NONE',  ( 0.000000000000000000, 6.999999999999999112, 0.000000000000000000 ) ) ;
#31473 = CARTESIAN_POINT ( 'NONE',  ( 4.713861384769566953, 8.227931952640012980, -0.6562286284988675389 ) ) ;
#31474 = CARTESIAN_POINT ( 'NONE',  ( -2.494337075234348777, 5.853884321174607663, -0.7216878364870267237 ) ) ;
#31475 = CARTESIAN_POINT ( 'NONE',  ( 8.649738815838679429, 10.15407870897571563, -1.082531754730543083 ) ) ;
#31476 = CARTESIAN_POINT ( 'NONE',  ( 4.223468175789964363, 0.2452432568937177593, -1.954070501097299850 ) ) ;
#31477 = CARTESIAN_POINT ( 'NONE',  ( 1.700013272279196963, 1.464590769506744161, 1.533662747278791816 ) ) ;
#31478 = CARTESIAN_POINT ( 'NONE',  ( -4.367698041896780126, 8.247398148854895084, 0.7998128361456481317 ) ) ;
#31479 = CARTESIAN_POINT ( 'NONE',  ( -5.083944415000194894, 5.033616027029421680, 0.7216878364870371598 ) ) ;
#31480 = CARTESIAN_POINT ( 'NONE',  ( 9.474246188248169886, -6.532648833121171172, -0.3333842132581051887 ) ) ;
#31481 = CARTESIAN_POINT ( 'NONE',  ( 5.507841377412062478, -0.9828142975771281264, -1.958786091674463714 ) ) ;
#31482 = CARTESIAN_POINT ( 'NONE',  ( -1.500000000000001110, 10.05208333401613174, 0.8660254037844418162 ) ) ;
#31483 = CARTESIAN_POINT ( 'NONE',  ( 4.629859910813647339, -1.184627732843917647, -1.519026826222178661 ) ) ;
#31484 = CARTESIAN_POINT ( 'NONE',  ( -5.693534442735004752, 8.729875052244421951, 1.199719254218452047 ) ) ;
#31485 = CARTESIAN_POINT ( 'NONE',  ( 0.1647065507319189492, -1.628042339203483957, -0.8261295386280396169 ) ) ;
#31486 = CARTESIAN_POINT ( 'NONE',  ( 0.6806489137391663613, -1.222764829241920426, 1.836970590647703849 ) ) ;
#31487 = CARTESIAN_POINT ( 'NONE',  ( 6.925078400183550364, -0.007619068086212391067, 2.144148427808051594 ) ) ;
#31488 = DIRECTION ( 'NONE',  ( 1.000000000000000000, -0.000000000000000000, -0.000000000000000000 ) ) ;
#31489 = ORIENTED_EDGE ( 'NONE', *, *, #67112, .T. ) ;
#31491 =( BOUNDED_CURVE ( )  B_SPLINE_CURVE ( 2, ( #81099, #113674, #213213, #64842, #114733, #32356, #77898 ),
 .UNSPECIFIED., .F., .T. ) 
 B_SPLINE_CURVE_WITH_KNOTS ( ( 3, 2, 2, 3 ),
 ( 0.1874999999999999722, 0.1916666666666666796, 0.1958333333333333870, 0.2000000000000000944 ),
 .UNSPECIFIED. ) 
 CURVE ( )  GEOMETRIC_REPRESENTATION_ITEM ( )  RATIONAL_B_SPLINE_CURVE ( ( 1.000000000000000888, 0.8660254037844378194, 1.000000000000000000, 0.8660254037844387076, 1.000000000000000000, 0.8660254037844360431, 1.000000000000002665 ) ) 
 REPRESENTATION_ITEM ( '' )  );
#31490 = CARTESIAN_POINT ( 'NONE',  ( 3.106226591306694651, 6.638031766584184368, 0.000000000000000000 ) ) ;
#31492 = ORIENTED_EDGE ( 'NONE', *, *, #166617, .F. ) ;
#31493 = CARTESIAN_POINT ( 'NONE',  ( 6.297704708030454235, -1.423956832742166112, -1.360762174370538258 ) ) ;
#31494 = CARTESIAN_POINT ( 'NONE',  ( 1.751409898207861415, 1.936723520591139058, -0.1449614948935191994 ) ) ;
#31495 = CARTESIAN_POINT ( 'NONE',  ( 6.696599425470320277, -1.493074370650529392, -1.747488531831635550 ) ) ;
#31497 = CARTESIAN_POINT ( 'NONE',  ( 5.700015841690603935, 0.7557596558054953118, -1.700775360669419145 ) ) ;
#31496 = CARTESIAN_POINT ( 'NONE',  ( -6.119526231721793330, 8.232809585132461194, 1.599625672291263179 ) ) ;
#31498 = CARTESIAN_POINT ( 'NONE',  ( 5.875479466675786355, 7.948088359245467416, -1.599625672291283607 ) ) ;
#31499 = CARTESIAN_POINT ( 'NONE',  ( 1.499999999999996891, 11.39583333333333393, -0.8660254037844378194 ) ) ;
#31500 = CARTESIAN_POINT ( 'NONE',  ( -11.78331023100045627, 11.37999999999999901, -1.800000000000001155 ) ) ;
#31501 = CARTESIAN_POINT ( 'NONE',  ( -6.043183783389232566, 8.073467052085995022, 1.599625672291269396 ) ) ;
#31502 = CARTESIAN_POINT ( 'NONE',  ( -7.937372586157736443, 8.224965870130965584, 0.7998128361456341429 ) ) ;
#31503 = CARTESIAN_POINT ( 'NONE',  ( 1.540847765565691585, -1.849059859674206496, 1.176127931831471907 ) ) ;
#31504 = CARTESIAN_POINT ( 'NONE',  ( 3.985733972737593778, 6.633478153960411738, -1.082531754730548412 ) ) ;
#31505 = CARTESIAN_POINT ( 'NONE',  ( 0.3999999999999896416, 3.999999999999973799, -0.8338124244296082344 ) ) ;
#31506 =( BOUNDED_CURVE ( )  B_SPLINE_CURVE ( 2, ( #120740, #100140, #202949, #54593, #186714, #16734, #82820 ),
 .UNSPECIFIED., .F., .T. ) 
 B_SPLINE_CURVE_WITH_KNOTS ( ( 3, 2, 2, 3 ),
 ( 0.1625000000000001443, 0.1666666666666666852, 0.1708333333333332260, 0.1749999999999997669 ),
 .UNSPECIFIED. ) 
 CURVE ( )  GEOMETRIC_REPRESENTATION_ITEM ( )  RATIONAL_B_SPLINE_CURVE ( ( 0.9999999999999955591, 0.8660254037844431485, 1.000000000000000000, 0.8660254037844387076, 1.000000000000000000, 0.8660254037844458130, 0.9999999999999928946 ) ) 
 REPRESENTATION_ITEM ( '' )  );
#31507 = CARTESIAN_POINT ( 'NONE',  ( 1.963248404482214049, 0.3131683437365209710, -1.798463397695612809 ) ) ;
#31508 = CARTESIAN_POINT ( 'NONE',  ( -3.755772246185468788, 4.340488027759846545, -1.199719254218452047 ) ) ;
#31509 = CARTESIAN_POINT ( 'NONE',  ( -0.3407659764052391460, 3.347064181880099021, -1.971699800770186695 ) ) ;
#31510 = CARTESIAN_POINT ( 'NONE',  ( 3.673896439623286714, 4.156855427197417185, -7.499999999999997335 ) ) ;
#31511 = CARTESIAN_POINT ( 'NONE',  ( 8.757677159423465696, 12.30470822171437284, 1.199719254218450271 ) ) ;
#31512 = CARTESIAN_POINT ( 'NONE',  ( 6.287720257080702702, 1.262826302610157381, 1.318732360701305062 ) ) ;
#31513 = CARTESIAN_POINT ( 'NONE',  ( 4.311346321947408633, -1.628642355029306987, -1.093319670275281652 ) ) ;
#31514 = CARTESIAN_POINT ( 'NONE',  ( -9.352427035328430449, 9.805586384171650849, 1.040834085586084257E-14 ) ) ;
#31515 = CARTESIAN_POINT ( 'NONE',  ( 5.799137018343234473, 7.788745826199009237, -1.599625672291262513 ) ) ;
#31516 = CARTESIAN_POINT ( 'NONE',  ( 4.107102485094754840, -0.3736803571842538529, 2.159302612355806339 ) ) ;
#31517 = AXIS2_PLACEMENT_3D ( 'NONE', #132563, #102159, #168227 ) ;
#31518 = CARTESIAN_POINT ( 'NONE',  ( 3.499976210622149253, 7.235056012367826028, 0.7998128361456321445 ) ) ;
#31519 = CARTESIAN_POINT ( 'NONE',  ( 3.836834752522141567, -1.993853832596056197, -0.5568897355931883286 ) ) ;
#31521 = CARTESIAN_POINT ( 'NONE',  ( 1.364683531249988535, 1.926041667008086211, 0.7879004041258500513 ) ) ;
#31520 = CARTESIAN_POINT ( 'NONE',  ( 6.137203345855459347, 5.375636887024366928, 2.500000000000000888 ) ) ;
#31522 = ORIENTED_EDGE ( 'NONE', *, *, #190238, .T. ) ;
#31523 = CARTESIAN_POINT ( 'NONE',  ( 3.657115705757322477, 1.277955821227232613, 1.910552683106376382 ) ) ;
#31524 = CARTESIAN_POINT ( 'NONE',  ( 6.629573927402440781, 10.67832731537079383, 1.040834085586084257E-14 ) ) ;
#31526 = CARTESIAN_POINT ( 'NONE',  ( 0.000000000000000000, 4.099999999999999645, 0.000000000000000000 ) ) ;
#31525 = CARTESIAN_POINT ( 'NONE',  ( 4.733205024946604667, 8.536173272497439513, 0.000000000000000000 ) ) ;
#31527 = CARTESIAN_POINT ( 'NONE',  ( -1.500000000000001110, 8.302083334016129967, 0.8660254037844418162 ) ) ;
#31528 = CARTESIAN_POINT ( 'NONE',  ( 1.772826578343066117, 3.950000000000009059, 0.4499999999999590994 ) ) ;
#31529 = CARTESIAN_POINT ( 'NONE',  ( 3.503789773231671845, -0.7878879028691202491, -1.775113385239434072 ) ) ;
#31530 = VERTEX_POINT ( 'NONE', #163913 ) ;
#31531 = CARTESIAN_POINT ( 'NONE',  ( 8.880227426826630577, 12.34372051706435869, 1.082531754730546636 ) ) ;
#31532 = EDGE_CURVE ( 'NONE', #17367, #55688, #107650, .T. ) ;
#31533 = CARTESIAN_POINT ( 'NONE',  ( 4.166199421025416960, 1.911861072351704882, -0.05224187775455800542 ) ) ;
#31534 = CARTESIAN_POINT ( 'NONE',  ( -3.929058411375401683, 5.499999999999998224, -0.7500000000000006661 ) ) ;
#31535 = CARTESIAN_POINT ( 'NONE',  ( 5.403229623239121260, 1.412049869051584361, 0.9901104176405839397 ) ) ;
#31536 = CARTESIAN_POINT ( 'NONE',  ( 5.050017674172561755, 0.9981218692422781924, 1.752141108012375437 ) ) ;
#31537 = CARTESIAN_POINT ( 'NONE',  ( 5.397245865906225681, -1.031513598091776673, -2.054350403923683732 ) ) ;
#31538 = CARTESIAN_POINT ( 'NONE',  ( 1.225528936851564721, -0.05108506852482053856, 2.206457870188942572 ) ) ;
#31540 = CARTESIAN_POINT ( 'NONE',  ( -5.370438244788932280, 6.398504386076097283, 1.082531754730549078 ) ) ;
#31539 = CARTESIAN_POINT ( 'NONE',  ( -9.775592450653132204, 11.36361159963886891, -1.199719254218441611 ) ) ;
#31541 = CARTESIAN_POINT ( 'NONE',  ( 6.098865926757823352, 1.445600302716108843, -1.020594415802724919 ) ) ;
#31543 = CARTESIAN_POINT ( 'NONE',  ( 1.570720025219290328, -2.177795595024238473, -0.7155201368211090429 ) ) ;
#31542 = CARTESIAN_POINT ( 'NONE',  ( 4.877901405866606588, 8.912911750144889567, 0.7998128361456341429 ) ) ;
#31544 = CARTESIAN_POINT ( 'NONE',  ( 1.534671620441448558, -1.258764033546970529, -1.202027791382529909 ) ) ;
#31545 = AXIS2_PLACEMENT_3D ( 'NONE', #36469, #152365, #100407 ) ;
#31546 = CARTESIAN_POINT ( 'NONE',  ( -4.510196435976065565, 7.040407170307378060, -1.149263043085164915 ) ) ;
#31547 = CARTESIAN_POINT ( 'NONE',  ( 0.6668559383766320403, -0.5766704339003425606, -1.635293367498649397 ) ) ;
#31548 = CARTESIAN_POINT ( 'NONE',  ( -0.6801582343750316451, 0.8802083336747270614, -1.178068619123876282 ) ) ;
#31549 = CARTESIAN_POINT ( 'NONE',  ( 0.000000000000000000, 3.799999999999998046, 0.000000000000000000 ) ) ;
#31550 = CARTESIAN_POINT ( 'NONE',  ( 1.697964449562241018, -1.571978469985369831, -1.497844480664213052 ) ) ;
#31551 = CARTESIAN_POINT ( 'NONE',  ( 2.659388954101277847, 1.913261587491304150, -0.6371546050257800298 ) ) ;
#31552 =( BOUNDED_CURVE ( )  B_SPLINE_CURVE ( 2, ( #214253, #115796, #102699, #181784, #20360, #150388, #149305, #84303, #86444 ),
 .UNSPECIFIED., .F., .T. ) 
 B_SPLINE_CURVE_WITH_KNOTS ( ( 3, 2, 2, 2, 3 ),
 ( 0.4531250000000002220, 0.4583333333333333148, 0.4687500000000000000, 0.4791666666666666852, 0.4843749999999997780 ),
 .UNSPECIFIED. ) 
 CURVE ( )  GEOMETRIC_REPRESENTATION_ITEM ( )  RATIONAL_B_SPLINE_CURVE ( ( 0.9330127018922194093, 0.9330127018922221849, 1.000000000000000000, 0.8660254037844387076, 1.000000000000000000, 0.8660254037844387076, 1.000000000000000000, 0.9330127018922221849, 0.9330127018922194093 ) ) 
 REPRESENTATION_ITEM ( '' )  );
#31553 = CARTESIAN_POINT ( 'NONE',  ( -0.7500000000000215383, 0.7229166673494852313, 1.299038105676659116 ) ) ;
#31554 = CARTESIAN_POINT ( 'NONE',  ( 6.006463946069247939, -0.6956954824784820079, -1.796673741800159707 ) ) ;
#31555 = CARTESIAN_POINT ( 'NONE',  ( -1.364683531250000748, 13.10937500034139980, 0.000000000000000000 ) ) ;
#31556 = CARTESIAN_POINT ( 'NONE',  ( 2.795431959603801086, -0.1677860356435970368, -2.215157990583861203 ) ) ;
#31557 = EDGE_LOOP ( 'NONE', ( #142828, #98739, #11709, #186001, #62870, #89820 ) ) ;
#31558 = CARTESIAN_POINT ( 'NONE',  ( -9.579592329540000506, -9.999999999999994671, 0.07839159645131747733 ) ) ;
#31559 = SURFACE_SIDE_STYLE ('',( #27270 ) ) ;
#31560 = CARTESIAN_POINT ( 'NONE',  ( 7.914208982075123799, 10.25632978388623684, -1.599625672291262513 ) ) ;
#31561 = FACE_OUTER_BOUND ( 'NONE', #74634, .T. ) ;
#31562 = CARTESIAN_POINT ( 'NONE',  ( 1.364683531249984538, -1.094791666325247936, -0.7879004041258309554 ) ) ;
#31563 = CARTESIAN_POINT ( 'NONE',  ( 5.354937190278808323, 0.3318421670873850648, -1.708331137930273913 ) ) ;
#31564 = CARTESIAN_POINT ( 'NONE',  ( 3.332423539472821439, -1.170687260143790320, 1.574129132985650825 ) ) ;
#31566 = CARTESIAN_POINT ( 'NONE',  ( -6.073689629242158716, 9.069426419882418600, -1.082531754730538864 ) ) ;
#31565 = CARTESIAN_POINT ( 'NONE',  ( 9.083599731475976213, 12.58098820582193689, 1.082531754730546636 ) ) ;
#31567 = CARTESIAN_POINT ( 'NONE',  ( -1.352846302990983851, 4.252095575701212660, 0.3040853380226599678 ) ) ;
#31568 = CARTESIAN_POINT ( 'NONE',  ( 4.903763976872734354, -0.6097993234682648200, 2.178603239016148052 ) ) ;
#31569 = CARTESIAN_POINT ( 'NONE',  ( 1.205618545266523567, -1.624909386276121692, -1.270427818644123796 ) ) ;
#31570 = CARTESIAN_POINT ( 'NONE',  ( -5.747767057189642870, 8.793146435774861658, -1.199719254218440723 ) ) ;
#31571 = CARTESIAN_POINT ( 'NONE',  ( 2.430887666589570451, 2.194555640652501527, 0.5498776597147712053 ) ) ;
#31572 = EDGE_LOOP ( 'NONE', ( #72075, #180227, #89538, #7713 ) ) ;
#31573 = CARTESIAN_POINT ( 'NONE',  ( -0.7500000000000006661, 0.8895833340161543035, -1.299038105676652011 ) ) ;
#31574 = CARTESIAN_POINT ( 'NONE',  ( 2.020564968092851021, 1.743606242109306148, 0.6777753874912318954 ) ) ;
#31575 = CARTESIAN_POINT ( 'NONE',  ( 1.687715598229572844, 1.441817134274174794, 0.9631580532376384784 ) ) ;
#31576 = EDGE_CURVE ( 'NONE', #53708, #134461, #96734, .T. ) ;
#31577 = CARTESIAN_POINT ( 'NONE',  ( 5.038714576072483631, -1.879839391954684746, 1.126354835186346603 ) ) ;
#31578 = CARTESIAN_POINT ( 'NONE',  ( 0.3412290553763823175, 0.3797058362894655814, 2.173699509851903855 ) ) ;
#31579 = CARTESIAN_POINT ( 'NONE',  ( 4.434552454296070145, 2.119417814153037316, 0.4246342833542292028 ) ) ;
#31580 = CARTESIAN_POINT ( 'NONE',  ( 5.103436805131417842, -1.932407887632971555, 0.1922973783335303055 ) ) ;
#31581 = CARTESIAN_POINT ( 'NONE',  ( -4.419594887930571758, 4.258541578781506409, 1.214306433183764966E-14 ) ) ;
#31582 = CARTESIAN_POINT ( 'NONE',  ( 6.784453417974287248, -1.834524189944960471, -0.3643881242741816018 ) ) ;
#31583 = CARTESIAN_POINT ( 'NONE',  ( 2.062500000000001776, -1.451031289061204266, -1.451031289061035956 ) ) ;
#31584 = EDGE_CURVE ( 'NONE', #138847, #162407, #139411, .T. ) ;
#31585 = CARTESIAN_POINT ( 'NONE',  ( 4.159596813995052322, 7.384974941181836172, -0.7733407813514819873 ) ) ;
#31586 = DIRECTION ( 'NONE',  ( 0.000000000000000000, 0.000000000000000000, 1.000000000000000000 ) ) ;
#31587 = FACE_OUTER_BOUND ( 'NONE', #26054, .T. ) ;
#31588 = CARTESIAN_POINT ( 'NONE',  ( 5.379529795981254914, -0.4926393568372189335, -1.955173248319847845 ) ) ;
#31589 = CARTESIAN_POINT ( 'NONE',  ( -3.809477975315625375, 4.507107728365378208, 1.082531754730558626 ) ) ;
#31590 = CARTESIAN_POINT ( 'NONE',  ( 8.294891053462476904, 8.571794405328034827, 1.040834085586084257E-14 ) ) ;
#31591 = CARTESIAN_POINT ( 'NONE',  ( 4.927462483923885195, 4.713404084191450849, -0.7998128361456481317 ) ) ;
#31592 = CARTESIAN_POINT ( 'NONE',  ( 3.809063337113669068, 1.566667275063510445, 0.9371452329686791316 ) ) ;
#31593 = DIRECTION ( 'NONE',  ( 0.000000000000000000, 1.000000000000000000, 0.000000000000000000 ) ) ;
#31594 = ORIENTED_EDGE ( 'NONE', *, *, #64213, .T. ) ;
#31595 = CARTESIAN_POINT ( 'NONE',  ( -5.194182247366913252, 7.153241603385088965, 1.443375672974058777 ) ) ;
#31596 = CYLINDRICAL_SURFACE ( 'NONE', #25081, 0.7500000000000006661 ) ;
#31597 = CARTESIAN_POINT ( 'NONE',  ( -8.513630394377489807, 12.01998699582738972, -1.199719254218446718 ) ) ;
#31598 = CARTESIAN_POINT ( 'NONE',  ( 0.3342475891858322501, -1.084071894752016041, -1.704023929676929727 ) ) ;
#31599 = CARTESIAN_POINT ( 'NONE',  ( 1.155114678095255254, 0.4172207117813032662, 2.078868179971034902 ) ) ;
#31600 = ORIENTED_EDGE ( 'NONE', *, *, #169914, .T. ) ;
#31601 = CARTESIAN_POINT ( 'NONE',  ( -4.423703259808839938, 8.383013913077441259, 0.7998128361456352531 ) ) ;
#31602 = CARTESIAN_POINT ( 'NONE',  ( 2.869522067586683711, 6.499526178826442013, 0.7998128361456362523 ) ) ;
#31603 = CARTESIAN_POINT ( 'NONE',  ( 6.596562995212404523, -0.5471746534140635720, -1.986858483302299083 ) ) ;
#31604 = CARTESIAN_POINT ( 'NONE',  ( 6.346327303948391396, 0.3419391630616851474, -1.987045965717588958 ) ) ;
#31605 = EDGE_LOOP ( 'NONE', ( #101538, #82930, #73485, #181055 ) ) ;
#31606 = ORIENTED_EDGE ( 'NONE', *, *, #51124, .F. ) ;
#31607 = CARTESIAN_POINT ( 'NONE',  ( 4.084924167595121780, -0.1881231333150361895, -1.917172266129524294 ) ) ;
#31608 = CARTESIAN_POINT ( 'NONE',  ( -10.45741655484220267, 11.09474082360439873, -0.7998128361456221525 ) ) ;
#31609 = CARTESIAN_POINT ( 'NONE',  ( 0.9311234436981512541, -1.109380368602566946, -3.475000000000000977 ) ) ;
#31610 = CIRCLE ( 'NONE', #100851, 1.000000000000000000 ) ;
#31613 = ORIENTED_EDGE ( 'NONE', *, *, #198798, .T. ) ;
#31612 = CARTESIAN_POINT ( 'NONE',  ( 6.883263157960391787, -0.001104538646235289417, 1.946037152736757925 ) ) ;
#31611 = CARTESIAN_POINT ( 'NONE',  ( -5.306037014901836990, 7.283738832175834510, 1.599625672291263179 ) ) ;
#31614 = CARTESIAN_POINT ( 'NONE',  ( 5.403926048761924505, 7.658933883257522446, 1.327442161737320436 ) ) ;
#31615 = CARTESIAN_POINT ( 'NONE',  ( 5.712267477471262289, -1.587595409608580255, -1.242535230690837489 ) ) ;
#31616 = CARTESIAN_POINT ( 'NONE',  ( 4.874869531740305462, 1.716800804850382223, -0.6655867697097294089 ) ) ;
#31617 = CIRCLE ( 'NONE', #145753, 0.08000000000000020983 ) ;
#31618 = CARTESIAN_POINT ( 'NONE',  ( 0.07700591528354487625, 0.7269319812311864082, -1.993543990282041767 ) ) ;
#31619 = CARTESIAN_POINT ( 'NONE',  ( 2.913035970020665388, 1.671030660360285802, -1.591803581779531074 ) ) ;
#31620 = CARTESIAN_POINT ( 'NONE',  ( 6.530187263637528439, 7.647581891445782709, -1.199719254218452047 ) ) ;
#31621 = CARTESIAN_POINT ( 'NONE',  ( 5.870447946289019114, -1.376328297836002301, 1.666777564274177781 ) ) ;
#31622 = CARTESIAN_POINT ( 'NONE',  ( 6.662942426112080874, 9.860851032851066122, 1.199719254218460707 ) ) ;
#31623 = CARTESIAN_POINT ( 'NONE',  ( 1.101004982060274751, -0.4702163980460572490, 1.884172457509038834 ) ) ;
#31624 = CARTESIAN_POINT ( 'NONE',  ( -4.959585264500673496, 4.680604318205876524, 1.214306433183764966E-14 ) ) ;
#31625 = ORIENTED_EDGE ( 'NONE', *, *, #187512, .T. ) ;
#31626 = CARTESIAN_POINT ( 'NONE',  ( 5.516820392445955790, 6.318161192665863624, -1.127043001766608432 ) ) ;
#31627 = CARTESIAN_POINT ( 'NONE',  ( -3.332271893908731464, 7.109677319527304640, -0.7998128361456481317 ) ) ;
#31628 = CARTESIAN_POINT ( 'NONE',  ( 4.838664814796108438, 0.3202261158844340594, 1.842872994462002367 ) ) ;
#31631 = CARTESIAN_POINT ( 'NONE',  ( -5.611095471209320174, 7.639640364534566075, 1.599625672291263179 ) ) ;
#31630 = CARTESIAN_POINT ( 'NONE',  ( 0.7499999999999885647, 0.7645833340161543035, 1.299038105676657340 ) ) ;
#31629 = CARTESIAN_POINT ( 'NONE',  ( 0.9492982845318720386, -1.727743609841876360, 0.8201845251225792222 ) ) ;
#31632 = CARTESIAN_POINT ( 'NONE',  ( 3.369938178094655346, 2.153121441420174698, -0.4834393813165636100 ) ) ;
#31633 = CARTESIAN_POINT ( 'NONE',  ( -1.458525620005792334, 8.740196138359387135, -2.548959422809881747 ) ) ;
#31634 = FACE_OUTER_BOUND ( 'NONE', #172255, .T. ) ;
#31635 = CARTESIAN_POINT ( 'NONE',  ( 5.506019780481205217, 9.437790487287811558, 0.000000000000000000 ) ) ;
#31636 = CARTESIAN_POINT ( 'NONE',  ( -3.297657676621885692, 4.870353260857385180, 1.599625672291267398 ) ) ;
#31637 = CARTESIAN_POINT ( 'NONE',  ( -6.902509602688821744, 8.185920970292658083, -1.082531754730549967 ) ) ;
#31638 = CARTESIAN_POINT ( 'NONE',  ( 2.126188665331921079, 1.138154612934966670, -1.609425365540081865 ) ) ;
#31639 = CARTESIAN_POINT ( 'NONE',  ( 0.7984239956072606281, -0.8271026589724904676, 2.154427444091823851 ) ) ;
#31640 = CARTESIAN_POINT ( 'NONE',  ( 1.890992312513404716, 0.1891058464698439912, 1.952711869325058691 ) ) ;
#31641 = CARTESIAN_POINT ( 'NONE',  ( 5.313357764218651802, -1.739529159241906875, -1.108013508251452395 ) ) ;
#31642 = CARTESIAN_POINT ( 'NONE',  ( 5.517805331081858888, 5.539787095791365523, 1.040834085586084257E-14 ) ) ;
#31643 = CARTESIAN_POINT ( 'NONE',  ( 5.337069745634900997, 6.255611453776062980, 1.199719254218452047 ) ) ;
#31644 = VERTEX_POINT ( 'NONE', #213676 ) ;
#31645 = CARTESIAN_POINT ( 'NONE',  ( 1.364683531249992088, 5.446875000341417916, 1.214306433183764966E-14 ) ) ;
#31646 = CARTESIAN_POINT ( 'NONE',  ( 10.91339599544321892, -6.211932585243247651, 5.201946966443877167E-15 ) ) ;
#31647 = CARTESIAN_POINT ( 'NONE',  ( 4.216222583725566686, 4.981643104843690217, -1.082531754730548412 ) ) ;
#31648 = CARTESIAN_POINT ( 'NONE',  ( 1.235490768065301337, -0.05108008202716606688, -2.170608684345101125 ) ) ;
#31650 = CARTESIAN_POINT ( 'NONE',  ( 6.339398910184078417, 0.6979989802004606947, -1.704029730133400866 ) ) ;
#31649 = CARTESIAN_POINT ( 'NONE',  ( -0.09999999999989878097, -10.00000000000009592, -10.91954211494242877 ) ) ;
#31651 = ADVANCED_FACE ( 'NONE', ( #210502 ), #141026, .T. ) ;
#31652 = CARTESIAN_POINT ( 'NONE',  ( 6.609253696060806149, -8.104785249476799791, 6.824425546749157689 ) ) ;
#31653 = DIRECTION ( 'NONE',  ( 0.000000000000000000, 1.000000000000000000, 0.000000000000000000 ) ) ;
#31654 = CARTESIAN_POINT ( 'NONE',  ( 1.633845377418343237, 0.9265681688636999702, -1.624882239709434018 ) ) ;
#31655 = CARTESIAN_POINT ( 'NONE',  ( 5.589210384452774960, 1.909260796540311000, -1.013481389624170115 ) ) ;
#31656 = CARTESIAN_POINT ( 'NONE',  ( -6.082092046053040768, 6.030765914320626919, 0.4329532585971782033 ) ) ;
#31657 = CARTESIAN_POINT ( 'NONE',  ( -0.02244404828160086532, 2.859736408857795009, -2.677210243787793598 ) ) ;
#31658 = CARTESIAN_POINT ( 'NONE',  ( 1.364683531249984538, -1.094791666325247936, -0.7879004041258309554 ) ) ;
#31659 = CARTESIAN_POINT ( 'NONE',  ( 1.893074787327468700, -0.09523556418119562272, -1.910042277862213034 ) ) ;
#31661 = ADVANCED_FACE ( 'NONE', ( #198502 ), #163128, .T. ) ;
#31660 = CARTESIAN_POINT ( 'NONE',  ( 2.852158073610413513, 0.5945245674133512459, 1.667141438756434058 ) ) ;
#31662 = CARTESIAN_POINT ( 'NONE',  ( 0.9262460828363194842, -0.8603794558708977025, -1.707882697979688391 ) ) ;
#31664 = CARTESIAN_POINT ( 'NONE',  ( 5.009359837557266992, -1.817519814519794830, 0.6052834035694378834 ) ) ;
#31663 = CARTESIAN_POINT ( 'NONE',  ( 7.806764249273698830, -6.480061791515699277, 7.750016138724927117 ) ) ;
#31665 = CARTESIAN_POINT ( 'NONE',  ( 6.742638201966631328, -1.931250359857048515, -0.3855633916233728309 ) ) ;
#31666 = CARTESIAN_POINT ( 'NONE',  ( -0.7500000000000215383, 5.191666666666685082, 1.299038105676671107 ) ) ;
#31667 = CARTESIAN_POINT ( 'NONE',  ( 0.5629301599625028407, 0.6213668382478373386, 2.027498709647377773 ) ) ;
#31668 = SURFACE_STYLE_FILL_AREA ( #106829 ) ;
#31669 = CARTESIAN_POINT ( 'NONE',  ( 4.539837415608827698, 0.7997722286730184482, -1.691214532891088362 ) ) ;
#31671 = ORIENTED_EDGE ( 'NONE', *, *, #168035, .T. ) ;
#31670 = CARTESIAN_POINT ( 'NONE',  ( 1.031563979315492485, -1.156294252604734396, -1.412831148817683680 ) ) ;
#31673 = CARTESIAN_POINT ( 'NONE',  ( 4.871809496981259535, 8.050285353323946680, -0.9368363805376724862 ) ) ;
#31672 = CARTESIAN_POINT ( 'NONE',  ( 4.266400587755204477, 1.039063272370500668, 1.946970035688735390 ) ) ;
#31674 = CARTESIAN_POINT ( 'NONE',  ( -1.364683531249997417, 4.821875000341417916, 1.214306433183764966E-14 ) ) ;
#31675 = CARTESIAN_POINT ( 'NONE',  ( 1.504421023514388889, 2.060217768730878696, 0.1034037034779722308 ) ) ;
#31676 = CARTESIAN_POINT ( 'NONE',  ( 5.774883364416965037, 8.824782127540085952, -1.199719254218440723 ) ) ;
#31677 = CARTESIAN_POINT ( 'NONE',  ( -6.692921386640485082, 10.96015871772258521, -0.7998128361456291469 ) ) ;
#31678 = DIRECTION ( 'NONE',  ( -0.8079921913640178976, 0.000000000000000000, -0.5891931930146276919 ) ) ;
#31679 = CARTESIAN_POINT ( 'NONE',  ( -3.423144538496482259, -0.02155739199629116976, -0.4187269634647496352 ) ) ;
#31680 = VECTOR ( 'NONE', #29510, 1000.000000000000000 ) ;
#31681 = CARTESIAN_POINT ( 'NONE',  ( 5.151735183068521629, 5.112705256442466428, 1.040834085586084257E-14 ) ) ;
#31682 = CARTESIAN_POINT ( 'NONE',  ( 5.806634928402749196, 9.996434193103704402, -0.7998128361456481317 ) ) ;
#31683 = ORIENTED_EDGE ( 'NONE', *, *, #203502, .T. ) ;
#31684 = CARTESIAN_POINT ( 'NONE',  ( 4.562978833902987752, 1.602482145440896399, -1.310924660355553106 ) ) ;
#31685 = CARTESIAN_POINT ( 'NONE',  ( -1.364683531250014514, -1.157291666325248158, 0.7879004041258379498 ) ) ;
#31686 = CARTESIAN_POINT ( 'NONE',  ( 1.036653925908154639, 2.129443126370239803, 0.3705773954724435604 ) ) ;
#31687 = CARTESIAN_POINT ( 'NONE',  ( -5.310352258326699548, 7.640991054048470232, -1.228972953101372223 ) ) ;
#31688 = CARTESIAN_POINT ( 'NONE',  ( 1.945969044768879552, -1.321035068824018222, -1.527795347589502972 ) ) ;
#31689 = DIRECTION ( 'NONE',  ( -5.578564026256490882E-16, -1.000000000000000000, -9.066213480720158442E-32 ) ) ;
#31690 = PRODUCT ( 'drip tip', 'drip tip', '', ( #82954 ) ) ;
#31691 = VERTEX_POINT ( 'NONE', #182260 ) ;
#31693 = CARTESIAN_POINT ( 'NONE',  ( 6.480434237652121787, 9.543961796360731498, 1.082531754730558626 ) ) ;
#31692 = CARTESIAN_POINT ( 'NONE',  ( -3.475000000000000533, -2.479166666666667851, -2.006292185433948827 ) ) ;
#31694 = CARTESIAN_POINT ( 'NONE',  ( 0.08011315927822239280, 14.48238172885137587, 11.99973258290723699 ) ) ;
#31695 = CARTESIAN_POINT ( 'NONE',  ( 0.7257964430846426396, 0.8128130212789463904, -1.845628942776005088 ) ) ;
#31696 = CARTESIAN_POINT ( 'NONE',  ( 4.652002595327206613, 0.8389548150543740812, 2.024815518666116088 ) ) ;
#31697 = CARTESIAN_POINT ( 'NONE',  ( -1.500000000000011324, 4.452083334016148086, 0.8660254037844403729 ) ) ;
#31698 = CARTESIAN_POINT ( 'NONE',  ( 4.711142613322857109, 1.586760866459841379, -1.067142987418716604 ) ) ;
#31699 = CARTESIAN_POINT ( 'NONE',  ( -2.754277761870538299, 6.365074488824250309, 1.040834085586084257E-14 ) ) ;
#31700 = CARTESIAN_POINT ( 'NONE',  ( 5.111060722227499298, 8.906728576000002562, -0.7216878364870267237 ) ) ;
#31702 = CARTESIAN_POINT ( 'NONE',  ( 2.214470461757975794, 1.956567829827577931, 0.4871813834786202224 ) ) ;
#31701 = DIRECTION ( 'NONE',  ( 1.000000000000000000, -0.000000000000000000, -0.000000000000000000 ) ) ;
#31703 = CARTESIAN_POINT ( 'NONE',  ( 0.6823417656249934904, 12.25520833367473017, 1.181850606188764807 ) ) ;
#31705 = CARTESIAN_POINT ( 'NONE',  ( -3.546339698426324460, 6.295090860542775779, -1.199719254218450271 ) ) ;
#31704 = CARTESIAN_POINT ( 'NONE',  ( -0.005774900045998726007, -2.292045413227526751, -0.04753075064714216980 ) ) ;
#31706 = CARTESIAN_POINT ( 'NONE',  ( 4.067213672036010585, 0.2104045600922407611, -1.711820660605578137 ) ) ;
#31707 = CARTESIAN_POINT ( 'NONE',  ( 0.000000000000000000, -1.099999999999982991, -2.499999999999995115 ) ) ;
#31708 = CARTESIAN_POINT ( 'NONE',  ( 2.523789150438203510, 6.096171108819874007, 0.7998128361456462443 ) ) ;
#31709 = AXIS2_PLACEMENT_3D ( 'NONE', #44141, #175214, #163220 ) ;
#31710 = LINE ( 'NONE', #159561, #119708 ) ;
#31711 = CARTESIAN_POINT ( 'NONE',  ( 11.97181073603049306, 9.719999999999998863, -0.8318477717169578955 ) ) ;
#31712 = EDGE_LOOP ( 'NONE', ( #39299, #105251, #95140, #159344 ) ) ;
#31713 = SURFACE_SIDE_STYLE ('',( #184330 ) ) ;
#31714 = ORIENTED_EDGE ( 'NONE', *, *, #150811, .F. ) ;
#31715 = CARTESIAN_POINT ( 'NONE',  ( 5.180233172056982305, 0.8977705535664436409, 1.573279850597033347 ) ) ;
#31716 = ORIENTED_EDGE ( 'NONE', *, *, #121204, .T. ) ;
#31717 = CARTESIAN_POINT ( 'NONE',  ( 4.342354338126830804, 8.288106837781779035, -0.7998128361456381397 ) ) ;
#31718 = CARTESIAN_POINT ( 'NONE',  ( 0.000000000000000000, 4.999999999999997335, 0.000000000000000000 ) ) ;
#31719 = CARTESIAN_POINT ( 'NONE',  ( 6.252603509501785339, 1.792834410666717337, 0.2582872775454737591 ) ) ;
#31720 = CARTESIAN_POINT ( 'NONE',  ( 6.495764994278809823, 7.711385593814346073, 1.082531754730549967 ) ) ;
#31721 = CARTESIAN_POINT ( 'NONE',  ( 2.280077068888842540, 5.600296667721481825, -0.6021448391562183033 ) ) ;
#31722 = CARTESIAN_POINT ( 'NONE',  ( 2.871223686158608679, 2.080653275041044026, -0.6881803712485771163 ) ) ;
#31723 = VERTEX_POINT ( 'NONE', #200631 ) ;
#31725 = EDGE_CURVE ( 'NONE', #102537, #168291, #185226, .T. ) ;
#31724 = CIRCLE ( 'NONE', #107848, 10.92874649719719571 ) ;
#31727 = CARTESIAN_POINT ( 'NONE',  ( 9.887974103068218668, 10.43039129653476493, 0.7998128361456462443 ) ) ;
#31726 = CARTESIAN_POINT ( 'NONE',  ( 6.443805748662878585, 1.284351271648530357, 1.347085863211768819 ) ) ;
#31728 = CARTESIAN_POINT ( 'NONE',  ( 3.638217106272136903, 0.6927189700525613336, 1.786146362908203944 ) ) ;
#31729 = DIRECTION ( 'NONE',  ( 0.000000000000000000, -0.7071067811865469066, -0.7071067811865482389 ) ) ;
#31730 = CARTESIAN_POINT ( 'NONE',  ( -15.75000000000000000, 13.40000000000000036, 1.099999999999996758 ) ) ;
#31731 = CARTESIAN_POINT ( 'NONE',  ( -1.364683531250014514, 0.03020833367475737191, 0.7879004041258379498 ) ) ;
#31732 = CARTESIAN_POINT ( 'NONE',  ( 5.829642864196171281, 5.903597551091405826, 0.7216878364870317197 ) ) ;
#31733 = CARTESIAN_POINT ( 'NONE',  ( -7.971831135155409420, 11.28392484344787405, 1.082531754730549967 ) ) ;
#31734 = CARTESIAN_POINT ( 'NONE',  ( 0.2687375195599971400, -1.410744835756465365, 1.637978619736128127 ) ) ;
#31735 = CARTESIAN_POINT ( 'NONE',  ( -6.069210040772897052, 7.109775131437022999, -1.199719254218453823 ) ) ;
#31736 = CARTESIAN_POINT ( 'NONE',  ( 3.203469434578891661, 6.959407783642502565, -0.7998128361456362523 ) ) ;
#31737 = CARTESIAN_POINT ( 'NONE',  ( 2.010518257881420023, 1.354885872097401078, -1.223726681998098087 ) ) ;
#31738 = CARTESIAN_POINT ( 'NONE',  ( -3.093231602212184850, 6.760520635889515795, -0.7998128361456281477 ) ) ;
#31739 = CARTESIAN_POINT ( 'NONE',  ( 3.434410497111122673, 1.780829521046650932, 0.4009754434649847044 ) ) ;
#31740 = ADVANCED_FACE ( 'NONE', ( #168161 ), #25283, .T. ) ;
#31741 = CARTESIAN_POINT ( 'NONE',  ( 9.687436728043250511, 13.40831512142563042, -8.157569025435085663 ) ) ;
#31742 = ORIENTED_EDGE ( 'NONE', *, *, #66878, .T. ) ;
#31743 = CARTESIAN_POINT ( 'NONE',  ( 2.787508051956408384, -1.838732291863707236, 0.7063352763673010903 ) ) ;
#31744 = ORIENTED_EDGE ( 'NONE', *, *, #68712, .F. ) ;
#31745 = CARTESIAN_POINT ( 'NONE',  ( 5.214377421777850685, 1.795891487756570815, 0.7396389662707256729 ) ) ;
#31746 = ORIENTED_EDGE ( 'NONE', *, *, #196609, .T. ) ;
#31747 = CARTESIAN_POINT ( 'NONE',  ( -6.424584688029276514, 8.588711117491191871, 1.599625672291269396 ) ) ;
#31749 = CARTESIAN_POINT ( 'NONE',  ( 5.695592476053609410, 1.958610405324921588, -0.8133567297157192622 ) ) ;
#31748 = CARTESIAN_POINT ( 'NONE',  ( 5.155843554946782703, 9.237177590738404831, -0.7998128361456481317 ) ) ;
#31750 = B_SPLINE_CURVE_WITH_KNOTS ( 'NONE', 3,
 ( #86868, #203788, #185420, #23985, #122669, #91161 ),
 .UNSPECIFIED., .F., .F.,
 ( 4, 2, 4 ),
 ( 0.000000000000000000, 0.0003155923098472861849, 0.0006311846196945723698 ),
 .UNSPECIFIED. ) ;
#31751 = DIRECTION ( 'NONE',  ( 0.000000000000000000, 0.000000000000000000, -1.000000000000000000 ) ) ;
#31752 = CARTESIAN_POINT ( 'NONE',  ( 2.561071438676546741, -1.588783617390630898, 1.063917234122884858 ) ) ;
#31753 = CARTESIAN_POINT ( 'NONE',  ( 4.860569815253008130, 6.917139861862701800, -1.418536646215622365 ) ) ;
#31754 = CARTESIAN_POINT ( 'NONE',  ( -1.833030277982346634, 0.000000000000000000, -2.499999999999998668 ) ) ;
#31755 = ORIENTED_EDGE ( 'NONE', *, *, #52269, .T. ) ;
#31756 = CARTESIAN_POINT ( 'NONE',  ( 5.401997860402196316, 5.267028690082820930, 0.000000000000000000 ) ) ;
#31757 = CARTESIAN_POINT ( 'NONE',  ( 3.714044015139744914, 6.420469553383295391, 1.199719254218462483 ) ) ;
#31758 = CARTESIAN_POINT ( 'NONE',  ( 4.389318492827157137, -0.002256833108382152835, -2.013265972533995640 ) ) ;
#31759 = CARTESIAN_POINT ( 'NONE',  ( 0.09916492693110359746, -9.919999999999998153, 9.499482423651659957 ) ) ;
#31760 = CARTESIAN_POINT ( 'NONE',  ( 5.531824841778981927, -1.161409778037244100, -1.408645805323349487 ) ) ;
#31761 = CARTESIAN_POINT ( 'NONE',  ( 0.2915762745691782287, -1.893489616766583117, 0.8377075429084477332 ) ) ;
#31762 = CARTESIAN_POINT ( 'NONE',  ( -9.029367117021344313, 9.636609179387466639, 0.7216878364870438212 ) ) ;
#31763 = CIRCLE ( 'NONE', #473, 11.00000000000000000 ) ;
#31764 = CARTESIAN_POINT ( 'NONE',  ( -6.601093878019091754, 6.767222581227101408, 0.2246719935465150975 ) ) ;
#31765 = DIRECTION ( 'NONE',  ( 0.000000000000000000, 0.000000000000000000, 1.000000000000000000 ) ) ;
#31766 = CARTESIAN_POINT ( 'NONE',  ( 5.295714669793899709, -0.6724083694377264164, 1.745798414713333413 ) ) ;
#31767 = CARTESIAN_POINT ( 'NONE',  ( 6.775324078527185989, 8.927630729746953264, -1.599625672291262513 ) ) ;
#31768 = FACE_OUTER_BOUND ( 'NONE', #56104, .T. ) ;
#31769 = CARTESIAN_POINT ( 'NONE',  ( -0.6823417656250039265, 10.38020833367472839, -1.181850606188755259 ) ) ;
#31770 = CARTESIAN_POINT ( 'NONE',  ( -3.899941742225307539, 7.701682465904834629, 0.7998128361456341429 ) ) ;
#31772 = CARTESIAN_POINT ( 'NONE',  ( -2.997761361953021009, 6.511488999004883205, -0.7216878364870458196 ) ) ;
#31771 = CARTESIAN_POINT ( 'NONE',  ( 3.521367211247359741, 5.131347717920458962, -1.599625672291262513 ) ) ;
#31773 = CARTESIAN_POINT ( 'NONE',  ( -3.296040741453672318, 6.859481608422314025, 0.7216878364870338292 ) ) ;
#31774 = CARTESIAN_POINT ( 'NONE',  ( -6.254388934605767503, 6.191208599995166040, 0.7998128361456341429 ) ) ;
#31775 = CARTESIAN_POINT ( 'NONE',  ( 0.7958623839904412911, -1.461433461687311253, -1.466603172318406090 ) ) ;
#31776 = CARTESIAN_POINT ( 'NONE',  ( 1.845463042662376818, 0.3584012047737962781, -2.086523245552903472 ) ) ;
#31777 = CARTESIAN_POINT ( 'NONE',  ( 9.402743226277308963, 10.92862083786708816, -1.199719254218446718 ) ) ;
#31778 = CARTESIAN_POINT ( 'NONE',  ( -1.499999999999997780, 3.431250000682818602, 1.214306433183764966E-14 ) ) ;
#31779 = CARTESIAN_POINT ( 'NONE',  ( 0.8835773814684219074, -1.871821877138898582, 0.6126781507047509567 ) ) ;
#31780 = CARTESIAN_POINT ( 'NONE',  ( 4.291011075107065587, 7.468133931351726318, 1.062205608224401576 ) ) ;
#31781 = CARTESIAN_POINT ( 'NONE',  ( 5.233084105194869551, 6.167981546557892436, -1.082531754730548412 ) ) ;
#31783 = DIRECTION ( 'NONE',  ( 1.000000000000000000, 3.451266460341926649E-31, 8.638326563840809144E-31 ) ) ;
#31782 = CARTESIAN_POINT ( 'NONE',  ( -1.737499999999997824, -2.741666666666666696, 3.009438278150925683 ) ) ;
#31784 = CARTESIAN_POINT ( 'NONE',  ( 2.238584135424640298, 0.5043332063416061661, 2.235947581072089907 ) ) ;
#31785 = CARTESIAN_POINT ( 'NONE',  ( -3.177206141917641613, 8.963489737286122860, 2.499999999999999556 ) ) ;
#31786 = CARTESIAN_POINT ( 'NONE',  ( 1.863391182279940494, -1.538030936729195552, -1.136358088520472931 ) ) ;
#31787 = ORIENTED_EDGE ( 'NONE', *, *, #156896, .F. ) ;
#31788 = CARTESIAN_POINT ( 'NONE',  ( 6.765155463094746580, 9.876136559377135526, 1.082531754730558626 ) ) ;
#31789 = EDGE_CURVE ( 'NONE', #125304, #116857, #37081, .T. ) ;
#31790 = CARTESIAN_POINT ( 'NONE',  ( 0.9494776711209992337, -1.818202237497710483, 0.8646994008154506028 ) ) ;
#31791 = CARTESIAN_POINT ( 'NONE',  ( 1.533958681542445301, 1.164210590399002321, 1.578835587694705334 ) ) ;
#31792 = CARTESIAN_POINT ( 'NONE',  ( -8.286004436246233951, 12.81875560892930466, 1.040834085586084257E-14 ) ) ;
#31793 = CARTESIAN_POINT ( 'NONE',  ( -8.376239975144482486, 8.666701480623698828, 1.040834085586084257E-14 ) ) ;
#31794 = CARTESIAN_POINT ( 'NONE',  ( -11.68373919224753266, 7.485257342004228320, -2.542923528616539919 ) ) ;
#31796 = CARTESIAN_POINT ( 'NONE',  ( 2.869705036365962858, 0.9450794480442193946, 1.496173807068044148 ) ) ;
#31795 = CARTESIAN_POINT ( 'NONE',  ( 4.154300538700359091, -1.549125135342351856, 1.404095012314343416 ) ) ;
#31797 = DIRECTION ( 'NONE',  ( -0.6507913734559640506, -0.7592566023653003482, 0.000000000000000000 ) ) ;
#31799 = CARTESIAN_POINT ( 'NONE',  ( 5.771479170232404421, 1.361120583587755783, 1.844262159060359174 ) ) ;
#31798 = CARTESIAN_POINT ( 'NONE',  ( 2.184835310096557404, 5.700724961754617404, 1.040834085586084257E-14 ) ) ;
#31800 = CARTESIAN_POINT ( 'NONE',  ( 4.786887925959832479, 1.292461281945065599, 1.165648420485969394 ) ) ;
#31801 = CARTESIAN_POINT ( 'NONE',  ( 7.553864141108259211, 11.96459193126834464, 1.040834085586084257E-14 ) ) ;
#31802 = CARTESIAN_POINT ( 'NONE',  ( -1.499999999999963141, 7.750000000000000000, 10.99818166789402341 ) ) ;
#31803 = CARTESIAN_POINT ( 'NONE',  ( 3.954193900006929052, 1.254965027507263464, 1.196595854207074261 ) ) ;
#31804 = CARTESIAN_POINT ( 'NONE',  ( 4.668535151219040280, -0.9243884330643321601, -1.964686384670484953 ) ) ;
#31805 = CARTESIAN_POINT ( 'NONE',  ( 5.169736645512481132, 4.925780929386339935, 0.7998128361456341429 ) ) ;
#31806 = CARTESIAN_POINT ( 'NONE',  ( 5.331267653506235327, -1.592659417495114083, -1.236803018183525449 ) ) ;
#31807 = CARTESIAN_POINT ( 'NONE',  ( 6.718719045489192965, -0.7860540964614262105, 1.895863743164223347 ) ) ;
#31808 = CARTESIAN_POINT ( 'NONE',  ( -0.7499999999999972244, 3.639583334016149863, -1.299038105676652011 ) ) ;
#31809 = CARTESIAN_POINT ( 'NONE',  ( 3.241151106802504511, -1.699520814979482264, 0.9069582849330155572 ) ) ;
#31810 = CARTESIAN_POINT ( 'NONE',  ( 1.500000000000001332, 10.40625000068279249, 0.000000000000000000 ) ) ;
#31811 = CARTESIAN_POINT ( 'NONE',  ( 5.959279902674206042, -1.877032357297861109, 1.187784507339540108 ) ) ;
#31812 = ORIENTED_EDGE ( 'NONE', *, *, #86051, .F. ) ;
#31813 = CARTESIAN_POINT ( 'NONE',  ( 6.983263157960380774, 2.077058603031848527, 2.154533585220330227 ) ) ;
#31814 = CARTESIAN_POINT ( 'NONE',  ( 1.499999999999989120, 3.275000000000020783, 1.214306433183764966E-14 ) ) ;
#31815 = CARTESIAN_POINT ( 'NONE',  ( 5.555090253297246150, 7.504024600312024340, 1.599625672291267398 ) ) ;
#31816 = CARTESIAN_POINT ( 'NONE',  ( 1.963841274844113194, -1.786346139091129270, -1.320113705855001207 ) ) ;
#31817 = CARTESIAN_POINT ( 'NONE',  ( -3.475000000000000089, -0.9959404071528829006, 0.7091675535885048065 ) ) ;
#31818 = CARTESIAN_POINT ( 'NONE',  ( 6.968527767744098433, 9.153035033833367251, 1.443375672974076540 ) ) ;
#31819 = CARTESIAN_POINT ( 'NONE',  ( -9.612367721964606204, 12.23751498042398289, -1.443375672974058777 ) ) ;
#31820 = STYLED_ITEM ( 'NONE', ( #42619 ), #74846 ) ;
#31821 = CARTESIAN_POINT ( 'NONE',  ( 7.851580356089786328, 8.332800968292465527, 0.000000000000000000 ) ) ;
#31822 = CARTESIAN_POINT ( 'NONE',  ( -3.038435823238377687, 6.558942537171132514, -0.7216878364870458196 ) ) ;
#31824 = CARTESIAN_POINT ( 'NONE',  ( 4.949704379398387033, 1.526268909138599028, 1.387654848983727485 ) ) ;
#31823 = CARTESIAN_POINT ( 'NONE',  ( 9.999301985278609806, 11.62460605670194447, 1.199719254218452047 ) ) ;
#31825 = CARTESIAN_POINT ( 'NONE',  ( -2.591579918506545344, 6.175260338232929413, 1.040834085586084257E-14 ) ) ;
#31826 = CARTESIAN_POINT ( 'NONE',  ( -1.500000000000011324, 5.660416667349481123, -0.8660254037844313801 ) ) ;
#31827 = CARTESIAN_POINT ( 'NONE',  ( 1.364683531249988757, -0.8656249996585805295, 0.000000000000000000 ) ) ;
#31828 = CARTESIAN_POINT ( 'NONE',  ( 6.134044790494318278, 0.9221746925026914621, -1.627378824227587062 ) ) ;
#31829 = CARTESIAN_POINT ( 'NONE',  ( 6.170542255345159433, 1.203217383492904746, 1.249094692781686611 ) ) ;
#31830 = CARTESIAN_POINT ( 'NONE',  ( 4.423245670630183923, -1.075405338609165318, -1.368339626032973211 ) ) ;
#31831 = CARTESIAN_POINT ( 'NONE',  ( 4.334856428067313416, 6.080418470877079429, -1.599625672291256295 ) ) ;
#31832 = EDGE_CURVE ( 'NONE', #33125, #96430, #164345, .T. ) ;
#31833 = CARTESIAN_POINT ( 'NONE',  ( 2.419810632640221115, -1.322813552229468614, -1.872022261021451639 ) ) ;
#31834 = CARTESIAN_POINT ( 'NONE',  ( -1.364683531250010295, 5.301041667008085767, -0.7879004041258300672 ) ) ;
#31835 = CARTESIAN_POINT ( 'NONE',  ( 0.9547317490294878750, 0.3612830171869831353, -1.805165878648997690 ) ) ;
#31836 = CARTESIAN_POINT ( 'NONE',  ( -0.4000000000000382694, 3.999999999999974243, 0.8338124244295226362 ) ) ;
#31837 = CARTESIAN_POINT ( 'NONE',  ( 1.887459117809231701, 1.256508940344562397, 1.324596713471258402 ) ) ;
#31838 = CARTESIAN_POINT ( 'NONE',  ( 2.514296259408643319, -1.880434619097739013, 0.7283795345095490648 ) ) ;
#31839 = CARTESIAN_POINT ( 'NONE',  ( 1.429895766826321690, 1.077743243251317429, -1.908043295719801025 ) ) ;
#31840 = CARTESIAN_POINT ( 'NONE',  ( 9.149559100784346199, 14.18285160050866445, -6.998392133554209416 ) ) ;
#31841 = CARTESIAN_POINT ( 'NONE',  ( 4.348724867337580235, 0.5594899878812797933, 2.030215228624824952 ) ) ;
#31842 = CARTESIAN_POINT ( 'NONE',  ( -7.552055258011950656, 8.769484874890757453, 1.199719254218462483 ) ) ;
#31843 = CARTESIAN_POINT ( 'NONE',  ( 1.609917502266303480, 0.6029389078928657497, -1.980602105166151095 ) ) ;
#31844 = CARTESIAN_POINT ( 'NONE',  ( 4.710568305744190276, 7.583081225755162968, 1.199719254218462483 ) ) ;
#31845 = CARTESIAN_POINT ( 'NONE',  ( 1.360316468749955821, -0.9531249996585916540, -5.204170427930421283E-14 ) ) ;
#31846 = CARTESIAN_POINT ( 'NONE',  ( 3.194099758881031814, 1.346771490053525033, 1.637864368873870990 ) ) ;
#31847 = CARTESIAN_POINT ( 'NONE',  ( -1.402160292154681736E-14, 0.9468750003414176941, -1.575800808251659024 ) ) ;
#31849 = EDGE_CURVE ( 'NONE', #201966, #130778, #15064, .T. ) ;
#31848 = CARTESIAN_POINT ( 'NONE',  ( 6.358013415952256331, 1.820405254634300363, -0.1396899356524081148 ) ) ;
#31850 = ORIENTED_EDGE ( 'NONE', *, *, #185099, .T. ) ;
#31851 = CARTESIAN_POINT ( 'NONE',  ( -6.089547271193396227, 7.133501900260939443, -1.199719254218453823 ) ) ;
#31852 = CARTESIAN_POINT ( 'NONE',  ( 9.561524646135536543, 12.17819805862340310, -1.599625672291262513 ) ) ;
#31853 = CARTESIAN_POINT ( 'NONE',  ( 6.170369307550815030, 8.292126506933040986, 1.443375672974064550 ) ) ;
#31854 = CARTESIAN_POINT ( 'NONE',  ( 0.000000000000000000, -3.543749999044085275, -4.012584370867899430 ) ) ;
#31855 = CARTESIAN_POINT ( 'NONE',  ( -5.747767057189642870, 8.793146435774861658, -1.199719254218440723 ) ) ;
#31856 = CARTESIAN_POINT ( 'NONE',  ( 3.551039915000217206, 0.3004019028194653829, 1.997212655505080203 ) ) ;
#31857 = CARTESIAN_POINT ( 'NONE',  ( 1.448413646618036399, 2.103543699351087870, 0.1036336169341102176 ) ) ;
#31859 = CARTESIAN_POINT ( 'NONE',  ( -6.282224075085783177, 8.422623735723785643, 1.599625672291269396 ) ) ;
#31858 = AXIS2_PLACEMENT_3D ( 'NONE', #188285, #87601, #35630 ) ;
#31860 = CARTESIAN_POINT ( 'NONE',  ( 8.106885785967500979, 11.54545161934907682, 1.199719254218460707 ) ) ;
#31861 = CARTESIAN_POINT ( 'NONE',  ( 5.014427361338555933, 0.7098351839037967403, 1.720451000603514524 ) ) ;
#31862 = CARTESIAN_POINT ( 'NONE',  ( 7.781490099239519509, 11.16582331816642260, 1.199719254218460707 ) ) ;
#31863 = CARTESIAN_POINT ( 'NONE',  ( 1.387358672531572079, 7.315968950354051259, 4.254625267138675504 ) ) ;
#31864 = CARTESIAN_POINT ( 'NONE',  ( -8.337901282724359930, 12.67137589657970409, 1.040834085586084257E-14 ) ) ;
#31865 = CARTESIAN_POINT ( 'NONE',  ( -6.008234629150358330, 10.16135750065076060, 0.000000000000000000 ) ) ;
#31866 = CARTESIAN_POINT ( 'NONE',  ( 6.192271402255323132, -2.050732637037344208, -0.2044092671329711397 ) ) ;
#31868 = CARTESIAN_POINT ( 'NONE',  ( -4.300870446666812619, 7.448604017583265957, 1.116033750828262949 ) ) ;
#31867 = CARTESIAN_POINT ( 'NONE',  ( -5.315678745009726924, 8.359319748223434487, -1.199719254218453823 ) ) ;
#31869 = CARTESIAN_POINT ( 'NONE',  ( -1.364683531250014514, 0.9885416670080898749, -0.7879004041258289570 ) ) ;
#31870 = CARTESIAN_POINT ( 'NONE',  ( 2.881899232214884865, -0.1729783253755692307, 1.725191050717300945 ) ) ;
#31871 = CARTESIAN_POINT ( 'NONE',  ( 1.446757823190962577, 0.5079132294574678630, -1.664563843253030750 ) ) ;
#31873 = CARTESIAN_POINT ( 'NONE',  ( 6.290620087060792009, 10.28288116830553101, -0.7216878364870267237 ) ) ;
#31872 = CARTESIAN_POINT ( 'NONE',  ( 6.691963835194851384, -0.9925954392468823162, 2.080958020993000979 ) ) ;
#31874 = CARTESIAN_POINT ( 'NONE',  ( -11.97711842482174305, 7.451475930019106464, -0.9249707317075172019 ) ) ;
#31875 = CARTESIAN_POINT ( 'NONE',  ( 2.917317126705867736, -0.2052410828034083035, 2.050554836033135597 ) ) ;
#31876 = CARTESIAN_POINT ( 'NONE',  ( 4.493637847925535667, 7.329995691633395261, -1.199719254218452047 ) ) ;
#31877 = CARTESIAN_POINT ( 'NONE',  ( 1.581407437776818581, 1.356094323556347181, -1.492024998029889638 ) ) ;
#31878 = CARTESIAN_POINT ( 'NONE',  ( 0.1331565106231598072, 7.629137130509052511, -2.545925718843544239 ) ) ;
#31879 = CARTESIAN_POINT ( 'NONE',  ( -6.134138155540168391, 6.121192367743780949, 0.000000000000000000 ) ) ;
#31880 = EDGE_CURVE ( 'NONE', #173258, #28237, #16999, .T. ) ;
#31881 = CARTESIAN_POINT ( 'NONE',  ( 1.692193703850993103, -1.961769708113933808, -0.1953840112930530781 ) ) ;
#31883 = CARTESIAN_POINT ( 'NONE',  ( -7.024532985656169792, 9.288650798055913427, 1.443375672974064550 ) ) ;
#31882 = CARTESIAN_POINT ( 'NONE',  ( 4.763870730211980487, 0.5944114921396548290, -1.817767169311027997 ) ) ;
#31884 = CARTESIAN_POINT ( 'NONE',  ( 5.918643953348324160, 1.484978324971843566, -1.632713241052483832 ) ) ;
#31885 = CARTESIAN_POINT ( 'NONE',  ( -6.794044373779495771, 8.059378203231773341, 1.082531754730549078 ) ) ;
#31886 = CARTESIAN_POINT ( 'NONE',  ( 6.851666526859736983, 9.086973262793417661, -1.599625672291269396 ) ) ;
#31887 = CARTESIAN_POINT ( 'NONE',  ( -7.767895665986912057, 8.027242796598338614, -0.7998128361456362523 ) ) ;
#31888 = CARTESIAN_POINT ( 'NONE',  ( 0.04752895628580295490, -1.845665702319599921, 0.8205699430347112022 ) ) ;
#31889 = CARTESIAN_POINT ( 'NONE',  ( -4.080641047588907888, 6.744203074620265248, -1.082531754730548412 ) ) ;
#31890 = CARTESIAN_POINT ( 'NONE',  ( 4.155530545730415248, -1.916392541607782496, -1.285185436265631642 ) ) ;
#31891 = CARTESIAN_POINT ( 'NONE',  ( 4.773855682050706761, -1.924389145058275963, 0.3807478752155256663 ) ) ;
#31892 = CARTESIAN_POINT ( 'NONE',  ( 2.342563710341159400, -1.922903400459201828, -0.3876519335672747313 ) ) ;
#31893 = FACE_OUTER_BOUND ( 'NONE', #113563, .T. ) ;
#31894 = CARTESIAN_POINT ( 'NONE',  ( -9.383668910090971593, 14.59391485664907151, 7.388226147404734157 ) ) ;
#31895 = VERTEX_POINT ( 'NONE', #173521 ) ;
#31896 = CARTESIAN_POINT ( 'NONE',  ( 0.09316046741510237983, 1.845552173327277501, 1.037660268145562004 ) ) ;
#31898 = CARTESIAN_POINT ( 'NONE',  ( -6.496328159242330536, 10.73079995242472862, 0.000000000000000000 ) ) ;
#31897 = CARTESIAN_POINT ( 'NONE',  ( -3.601662362724658895, 7.353689856487406473, -0.7998128361456281477 ) ) ;
#31899 = CARTESIAN_POINT ( 'NONE',  ( 1.148114065366242498, -1.452583890646602205, 1.131155481815901531 ) ) ;
#31900 = ORIENTED_EDGE ( 'NONE', *, *, #29437, .T. ) ;
#31901 = CARTESIAN_POINT ( 'NONE',  ( 4.118177926953592305, 2.155335829443456142, -0.2601999948229383741 ) ) ;
#31902 = CARTESIAN_POINT ( 'NONE',  ( -0.4461809497497637444, 3.122791860410086606, 1.949595486268986821 ) ) ;
#31903 = CARTESIAN_POINT ( 'NONE',  ( 1.863691559860299884, -1.706161385809309650, -1.259181899442491037 ) ) ;
#31904 = CARTESIAN_POINT ( 'NONE',  ( 1.499999999999987121, 2.827083334016148530, -0.8660254037844262731 ) ) ;
#31905 = CARTESIAN_POINT ( 'NONE',  ( 9.074484886248265880, 9.481320543578137361, 0.7998128361456462443 ) ) ;
#31906 = CARTESIAN_POINT ( 'NONE',  ( -5.810221930991193690E-16, 2.500000000682804036, -1.225000000000023626 ) ) ;
#31907 = CARTESIAN_POINT ( 'NONE',  ( 6.308853223578811509, 6.964933332891984463, 0.9108697706533327443 ) ) ;
#31908 = CARTESIAN_POINT ( 'NONE',  ( 3.057942249777849675, 2.051182028257723999, -0.1983934154812707074 ) ) ;
#31910 = CARTESIAN_POINT ( 'NONE',  ( 0.6613494997313728030, 0.9071737413179328247, 1.602200521169500957 ) ) ;
#31909 = CARTESIAN_POINT ( 'NONE',  ( -8.422639742587602285, 10.84949900448412841, -1.599625672291263179 ) ) ;
#31911 = CARTESIAN_POINT ( 'NONE',  ( -1.364683531250012516, 3.280208333674756727, 0.7879004041258379498 ) ) ;
#31912 = CARTESIAN_POINT ( 'NONE',  ( -0.02244404828157658613, -0.004869073801674199918, -2.189079685368473527 ) ) ;
#31913 = CARTESIAN_POINT ( 'NONE',  ( -6.511106444361044687, 5.279176164185805042, 2.499999999999998668 ) ) ;
#31914 = CARTESIAN_POINT ( 'NONE',  ( 11.80248046418316044, 9.800000000000000711, -1.695421849633145017 ) ) ;
#31915 = CARTESIAN_POINT ( 'NONE',  ( 2.073834635255236147, 2.165437736866062224, -0.6553434645707820749 ) ) ;
#31916 = CARTESIAN_POINT ( 'NONE',  ( -9.517460647113315630, 10.20605163116143821, 0.7216878364870438212 ) ) ;
#31917 = CARTESIAN_POINT ( 'NONE',  ( 0.8612205622890884982, -1.428740940428592898, -1.113706988620609240 ) ) ;
#31918 = CARTESIAN_POINT ( 'NONE',  ( 2.272541799296357468, -0.3318032026102230581, -1.886604652318550901 ) ) ;
#31919 = CARTESIAN_POINT ( 'NONE',  ( 2.647004975520852454, -0.3514972095969396970, -2.040143077068845123 ) ) ;
#31920 = CARTESIAN_POINT ( 'NONE',  ( -0.6823417656250003738, 2.030208333674753174, -1.181850606188749264 ) ) ;
#31921 = CARTESIAN_POINT ( 'NONE',  ( 2.184392200726268829, -1.933073530578834465, -0.3863716293817393566 ) ) ;
#31922 = CARTESIAN_POINT ( 'NONE',  ( 5.408790948643045660, 1.457530049539386141, -1.259864545333173158 ) ) ;
#31924 = CARTESIAN_POINT ( 'NONE',  ( 6.455362170788604637, 6.771378801287749383, -0.3290997004737963860 ) ) ;
#31923 = CARTESIAN_POINT ( 'NONE',  ( 0.7335963760657808752, 0.1754145531542888048, 2.301085101356622697 ) ) ;
#31925 = CARTESIAN_POINT ( 'NONE',  ( 1.364683531249990311, 3.134375000341423245, 1.214306433183764966E-14 ) ) ;
#31926 = CARTESIAN_POINT ( 'NONE',  ( 4.949704379398387033, 1.526268909138599028, 1.387654848983727485 ) ) ;
#31927 = CARTESIAN_POINT ( 'NONE',  ( -6.250472511100020334, 7.250971670160158311, 1.199719254218450271 ) ) ;
#31928 = CARTESIAN_POINT ( 'NONE',  ( 5.777746017718023097, 9.892454120646377191, 0.7998128361456462443 ) ) ;
#31929 = CARTESIAN_POINT ( 'NONE',  ( 6.756868576547260474, -1.630415217921374671, 1.332730856581629375 ) ) ;
#31930 = CARTESIAN_POINT ( 'NONE',  ( -1.201851678989727383E-14, 2.634375000341417916, 1.575800808251672791 ) ) ;
#31931 = CARTESIAN_POINT ( 'NONE',  ( 4.903692054014650026, -0.5817465652163296141, 2.081756923971528117 ) ) ;
#31932 = CARTESIAN_POINT ( 'NONE',  ( 4.934242777533356161, -1.082215927170935954, -1.705062858592779174 ) ) ;
#31933 = CARTESIAN_POINT ( 'NONE',  ( -0.1399997263889612154, 1.357298622859517856, -2.254419820505838334 ) ) ;
#31934 = CARTESIAN_POINT ( 'NONE',  ( -5.260200412422208593, 7.159986452624450770, -1.443375672974053447 ) ) ;
#31937 = CARTESIAN_POINT ( 'NONE',  ( 3.877268743828266029, 6.506935386899531437, 1.082531754730558626 ) ) ;
#31936 = CARTESIAN_POINT ( 'NONE',  ( 0.000000000000000000, -2.296874999522042327, -3.793834371823813001 ) ) ;
#31935 = CARTESIAN_POINT ( 'NONE',  ( -8.752381174298911048, 14.55265199826961364, -8.156849355156190029 ) ) ;
#31938 = CARTESIAN_POINT ( 'NONE',  ( -3.644109427023046521, 7.473487774827342278, 0.000000000000000000 ) ) ;
#31939 = CARTESIAN_POINT ( 'NONE',  ( 3.503138892209650024, -0.1435209762444041581, 2.011451614702438828 ) ) ;
#31940 = CARTESIAN_POINT ( 'NONE',  ( -7.823218330285243383, 9.085841792542966644, -1.199719254218446718 ) ) ;
#31942 = CARTESIAN_POINT ( 'NONE',  ( 0.000000000000000000, 15.50000000000019362, 0.000000000000000000 ) ) ;
#31941 = CARTESIAN_POINT ( 'NONE',  ( -2.117044542028253318, 5.621635732341564662, -0.7998128361456281477 ) ) ;
#31943 = CARTESIAN_POINT ( 'NONE',  ( -0.6823417656249969321, 5.717708333674756283, -1.181850606188749264 ) ) ;
#31945 = CARTESIAN_POINT ( 'NONE',  ( -1.364683531250014514, 9.338541667008062319, -0.7879004041258335089 ) ) ;
#31944 = CARTESIAN_POINT ( 'NONE',  ( 4.997027575558514734, 1.799266821141291661, -1.197868618907194316 ) ) ;
#31946 = CARTESIAN_POINT ( 'NONE',  ( 0.000000000000000000, 2.480000000000016858, 0.000000000000000000 ) ) ;
#31947 = CARTESIAN_POINT ( 'NONE',  ( -11.93088452921365139, 7.924368216754111849, -1.311419307916881216 ) ) ;
#31949 = CARTESIAN_POINT ( 'NONE',  ( 5.044546077387519922, -1.458546410489666600, 1.392558106302365095 ) ) ;
#31948 = CARTESIAN_POINT ( 'NONE',  ( -7.090551149822745813, 9.295395646258437949, 1.443375672974078761 ) ) ;
#31950 = CARTESIAN_POINT ( 'NONE',  ( -1.364683531250014514, -0.1989583329919157317, -0.7879004041258359514 ) ) ;
#31951 = CARTESIAN_POINT ( 'NONE',  ( 1.910387937834428174, 1.279409190829815746, -1.157040217339623034 ) ) ;
#31952 = CARTESIAN_POINT ( 'NONE',  ( 4.869313445963426190, 5.709895770826003414, 1.199719254218452935 ) ) ;
#31953 = STYLED_ITEM ( 'NONE', ( #211229 ), #26340 ) ;
#31955 = CARTESIAN_POINT ( 'NONE',  ( 5.993586425693011144, 9.150212042353954800, -1.199719254218452047 ) ) ;
#31954 = CARTESIAN_POINT ( 'NONE',  ( 7.727784370109387346, 10.99920361756089093, -1.082531754730543083 ) ) ;
#31956 = CARTESIAN_POINT ( 'NONE',  ( -11.86159218342442756, 8.823409521868983418, 1.516044442424843153 ) ) ;
#31957 = CARTESIAN_POINT ( 'NONE',  ( 6.643822754079466542, 0.7155741859487285694, -1.728458771772640512 ) ) ;
#31958 = CARTESIAN_POINT ( 'NONE',  ( 0.3990879006048999589, -0.2487020831964822098, -1.997621932491387531 ) ) ;
#31959 =( LENGTH_UNIT ( ) NAMED_UNIT ( * ) SI_UNIT ( .MILLI., .METRE. ) );
#31960 = CARTESIAN_POINT ( 'NONE',  ( 3.065657736429776126, 0.3252250816505456998, -2.182562984848686938 ) ) ;
#31961 = CARTESIAN_POINT ( 'NONE',  ( -5.763624699140874164, 8.777960344756069233, -1.082531754730549967 ) ) ;
#31962 = ORIENTED_EDGE ( 'NONE', *, *, #50413, .T. ) ;
#31963 = CARTESIAN_POINT ( 'NONE',  ( 9.856414487010592751, 10.60149777770828194, 0.7216878364870438212 ) ) ;
#31965 = CARTESIAN_POINT ( 'NONE',  ( 1.353138909097661768, 0.1455122274086443901, -2.011206940682720212 ) ) ;
#31964 = CARTESIAN_POINT ( 'NONE',  ( 2.526173596586390957, -2.097057114080549844, 0.3136139059176298871 ) ) ;
#31967 = ORIENTED_EDGE ( 'NONE', *, *, #209339, .T. ) ;
#31966 = CARTESIAN_POINT ( 'NONE',  ( 2.531291980686082521, -0.1736719688998221156, 1.803202784768900502 ) ) ;
#31968 = CARTESIAN_POINT ( 'NONE',  ( 5.677832469072920496, 9.846164657218904992, 0.000000000000000000 ) ) ;
#31969 = ORIENTED_EDGE ( 'NONE', *, *, #210296, .F. ) ;
#31970 = EDGE_CURVE ( 'NONE', #40394, #99491, #208638, .T. ) ;
#31971 = CARTESIAN_POINT ( 'NONE',  ( 6.647575389402066826, 6.649926130590872120, 1.040834085586084257E-14 ) ) ;
#31972 = AXIS2_PLACEMENT_3D ( 'NONE', #195993, #132089, #96378 ) ;
#31973 = B_SPLINE_CURVE_WITH_KNOTS ( 'NONE', 3,
 ( #22767, #128909, #29202, #194890, #95292, #15054, #61696, #94224, #80071, #31343 ),
 .UNSPECIFIED., .F., .F.,
 ( 4, 2, 2, 2, 4 ),
 ( 0.001600703253539966127, 0.001978746783904330314, 0.002356790314268694501, 0.002734833844633058689, 0.003112877374997422876 ),
 .UNSPECIFIED. ) ;
#31975 = CARTESIAN_POINT ( 'NONE',  ( 0.4619447194890722308, -1.061692323622511536, 1.594387217869216888 ) ) ;
#31974 = CARTESIAN_POINT ( 'NONE',  ( -3.928111819657352566, 5.605883094398769195, 1.599625672291267398 ) ) ;
#31976 = AXIS2_PLACEMENT_3D ( 'NONE', #209144, #12023, #60783 ) ;
#31977 = CARTESIAN_POINT ( 'NONE',  ( 7.102951435054647665E-16, -3.600000000000005862, 5.799999999999999822 ) ) ;
#31978 = B_SPLINE_CURVE_WITH_KNOTS ( 'NONE', 3,
 ( #54573, #103325, #120721, #22033 ),
 .UNSPECIFIED., .F., .F.,
 ( 4, 4 ),
 ( 0.000000000000000000, 0.0002852742075882630057 ),
 .UNSPECIFIED. ) ;
#31979 = CARTESIAN_POINT ( 'NONE',  ( 5.409340101728155936, 8.294351971116089572, -1.082531754730543971 ) ) ;
#31980 = CARTESIAN_POINT ( 'NONE',  ( 1.364683531249986537, 0.9677083336747538400, -0.7879004041258239610 ) ) ;
#31981 = DIRECTION ( 'NONE',  ( 0.000000000000000000, 0.000000000000000000, 1.000000000000000000 ) ) ;
#31982 = CARTESIAN_POINT ( 'NONE',  ( -8.513630394377489807, 12.01998699582738972, -1.199719254218446718 ) ) ;
#31983 = CARTESIAN_POINT ( 'NONE',  ( 5.401312781148372544, 1.764888628567515827, 1.247983453017486477 ) ) ;
#31984 = CARTESIAN_POINT ( 'NONE',  ( -6.780486220610186798, 8.043560357867583832, -1.082531754730549967 ) ) ;
#31985 = CARTESIAN_POINT ( 'NONE',  ( 5.234856708652227297, 7.200695141551334721, 1.443375672974065660 ) ) ;
#31986 = CARTESIAN_POINT ( 'NONE',  ( 1.705496241919310707, 1.842552997918958768, -1.049655202612943095 ) ) ;
#31987 = CARTESIAN_POINT ( 'NONE',  ( 6.704125975539116489, -1.825092170400946845, 0.04854515157103055090 ) ) ;
#31988 = CARTESIAN_POINT ( 'NONE',  ( 3.163306973099208275, 0.2928498925126362673, -1.949387327701812334 ) ) ;
#31989 = ORIENTED_EDGE ( 'NONE', *, *, #113502, .F. ) ;
#31990 = CARTESIAN_POINT ( 'NONE',  ( 6.689911425329987615, -1.285551722473629477, -1.492250998650017202 ) ) ;
#31991 = CARTESIAN_POINT ( 'NONE',  ( 1.359210844938564033, 1.913264527786652902, -0.3316978906799557536 ) ) ;
#31992 = VERTEX_POINT ( 'NONE', #171353 ) ;
#31993 = CARTESIAN_POINT ( 'NONE',  ( -4.251935539942575559, 7.316435789055923955, -0.9001278212061183392 ) ) ;
#31995 = CARTESIAN_POINT ( 'NONE',  ( 6.339319342841494453, 9.553567112360518365, -1.199719254218452047 ) ) ;
#31994 = CARTESIAN_POINT ( 'NONE',  ( -7.282137904315833410, 7.668451441222825515, 0.000000000000000000 ) ) ;
#31997 = CARTESIAN_POINT ( 'NONE',  ( 7.470706336329915764, 8.674577799595093452, -1.199719254218441611 ) ) ;
#31996 = CARTESIAN_POINT ( 'NONE',  ( 2.203177794981598492, -0.4570653145323905764, 2.039892330567660839 ) ) ;
#31999 = CARTESIAN_POINT ( 'NONE',  ( 4.977251789548238214, 7.860525283564661514, -1.082531754730548412 ) ) ;
#31998 = CARTESIAN_POINT ( 'NONE',  ( 6.120616281565444794, 9.228137197546649517, -1.199719254218440723 ) ) ;
#32001 = ORIENTED_EDGE ( 'NONE', *, *, #209714, .T. ) ;
#32000 = CARTESIAN_POINT ( 'NONE',  ( -0.1051951494144076904, -0.1375245761873785666, -1.781266614511106683 ) ) ;
#32002 = CARTESIAN_POINT ( 'NONE',  ( 4.881566871873391555, 2.059980941486462047, -0.7921658822237287456 ) ) ;
#32003 = CARTESIAN_POINT ( 'NONE',  ( 2.204404769108789797, -2.206272049354717879, 0.05393164079612458583 ) ) ;
#32004 = CARTESIAN_POINT ( 'NONE',  ( -11.01135777277262129, 12.69999999999998153, 1.399999999999998579 ) ) ;
#32005 = CARTESIAN_POINT ( 'NONE',  ( 0.3988866192712777758, -0.2342882197893907670, -1.897819253221716851 ) ) ;
#32006 = CARTESIAN_POINT ( 'NONE',  ( 0.000000000000000000, -2.079999999999998295, 0.000000000000000000 ) ) ;
#32007 = CARTESIAN_POINT ( 'NONE',  ( 8.238550898598388628, 12.76339314834017102, 0.7998128361456462443 ) ) ;
#32008 = CARTESIAN_POINT ( 'NONE',  ( 3.877443546529443452, -0.1552652338182025915, 2.064615508632794860 ) ) ;
#32010 = CARTESIAN_POINT ( 'NONE',  ( 1.780366757100563913, -1.156431984057613827, 1.826190802295484472 ) ) ;
#32009 = CARTESIAN_POINT ( 'NONE',  ( 0.000000000000000000, 4.000000000000003553, 0.000000000000000000 ) ) ;
#32011 = CARTESIAN_POINT ( 'NONE',  ( 3.280998142716429200, 1.980384277226649559, -0.9389412094223739125 ) ) ;
#32012 = LINE ( 'NONE', #66591, #96992 ) ;
#32013 = CARTESIAN_POINT ( 'NONE',  ( 0.000000000000000000, 2.800000000000024691, 1.214306433183764966E-14 ) ) ;
#32014 = CARTESIAN_POINT ( 'NONE',  ( -0.2935777296395137848, 7.111227605955122044, 1.979479841891082170 ) ) ;
#32015 = CARTESIAN_POINT ( 'NONE',  ( -1.364683531250014514, 14.40104166700806410, -0.7879004041258335089 ) ) ;
#32016 = CARTESIAN_POINT ( 'NONE',  ( -4.573896719763875574, 6.429575154514868274, -1.599625672291271394 ) ) ;
#32017 = CARTESIAN_POINT ( 'NONE',  ( 0.4928148368598186946, -2.006445878461552645, 0.2004378712678403507 ) ) ;
#32018 = CARTESIAN_POINT ( 'NONE',  ( -8.188761592974033832, 12.49737959187099179, -0.7216878364870267237 ) ) ;
#32019 = CARTESIAN_POINT ( 'NONE',  ( 4.329010850845236291, -1.929826300244817272, -0.7499136367685385052 ) ) ;
#32020 = CARTESIAN_POINT ( 'NONE',  ( 5.536746206892352085, -1.668647081869235826, 1.303048207008510317 ) ) ;
#32021 = CARTESIAN_POINT ( 'NONE',  ( 5.799137018343234473, 7.788745826199009237, -1.599625672291262513 ) ) ;
#32022 = CARTESIAN_POINT ( 'NONE',  ( 9.475937985776960559, 4.398642190548692987, 7.290290962746384551 ) ) ;
#32023 = CARTESIAN_POINT ( 'NONE',  ( 3.977371423044063103, -0.1491618029233315879, 1.963883198941584585 ) ) ;
#32024 = CARTESIAN_POINT ( 'NONE',  ( 6.052705554163346768, -1.962971892542137553, -1.183510860282228405 ) ) ;
#32025 = CARTESIAN_POINT ( 'NONE',  ( 4.143042835627613663, -1.587387879459275286, 0.9017181768668989239 ) ) ;
#32026 = CARTESIAN_POINT ( 'NONE',  ( 3.366167277942881064, 7.149221934233827014, -0.7998128361456362523 ) ) ;
#32027 = CARTESIAN_POINT ( 'NONE',  ( 5.029711800545521250, 5.930713857800314237, -1.082531754730549078 ) ) ;
#32028 = CARTESIAN_POINT ( 'NONE',  ( -5.444481204339554736, 8.509589284108232121, 1.199719254218454489 ) ) ;
#32029 = CARTESIAN_POINT ( 'NONE',  ( 6.150558962454855561, 7.204682206732687000, 1.199719254218452047 ) ) ;
#32030 = ORIENTED_EDGE ( 'NONE', *, *, #56710, .F. ) ;
#32031 = CARTESIAN_POINT ( 'NONE',  ( 4.851819109577236055, -1.426696570994885116, -1.420647396805594820 ) ) ;
#32032 = CARTESIAN_POINT ( 'NONE',  ( 6.328761054056312396, 0.8840516187795799397, -2.122072247225449626 ) ) ;
#32033 = CARTESIAN_POINT ( 'NONE',  ( 4.065250617491710905, 1.680331827152386159, 1.012218702928203706 ) ) ;
#32034 = CARTESIAN_POINT ( 'NONE',  ( -7.043624497499477499, 8.176315654292865887, 1.199719254218450271 ) ) ;
#32035 = CARTESIAN_POINT ( 'NONE',  ( -3.276266675996675204, 6.974061555304760240, -0.7998128361456281477 ) ) ;
#32036 = CARTESIAN_POINT ( 'NONE',  ( -10.10493793804576868, 0.9691415390508768546, -6.281047173807432493 ) ) ;
#32037 = CARTESIAN_POINT ( 'NONE',  ( -4.288121723672178476, 8.224835454251337552, -0.7998128361456362523 ) ) ;
#32039 = CARTESIAN_POINT ( 'NONE',  ( 5.946140033727446372, 1.768047588762114986, 0.08285011829376774661 ) ) ;
#32038 = CARTESIAN_POINT ( 'NONE',  ( 0.6969597590469852610, 1.711416582936477804, 1.200673393543179479 ) ) ;
#32040 = CARTESIAN_POINT ( 'NONE',  ( 0.000000000000000000, 2.880000000000021210, 1.214306433183764966E-14 ) ) ;
#32041 = CARTESIAN_POINT ( 'NONE',  ( 5.595633723370948331, -1.942124712531563491, 0.002075263307293323100 ) ) ;
#32042 = CARTESIAN_POINT ( 'NONE',  ( 2.238457302780196390, 0.4817095239468481283, 2.137691825660259948 ) ) ;
#32043 = CARTESIAN_POINT ( 'NONE',  ( 1.417106933825535986, -0.9663644154882103932, -1.447271084069596370 ) ) ;
#32044 = CARTESIAN_POINT ( 'NONE',  ( 5.774883364416965037, 8.824782127540085952, -1.199719254218440723 ) ) ;
#32045 = CARTESIAN_POINT ( 'NONE',  ( 1.295042460130943152, 1.303850460046240833, 1.129354085073847491 ) ) ;
#32046 = CARTESIAN_POINT ( 'NONE',  ( 1.400213348495438437, -0.7931047570679079506, -2.043190674350242819 ) ) ;
#32047 = CARTESIAN_POINT ( 'NONE',  ( 4.178501018151202118, -1.271701901513167421, 1.803451139310302986 ) ) ;
#32048 = CARTESIAN_POINT ( 'NONE',  ( 1.270657207514551246, -0.9741964446108697384, -1.940257991389877201 ) ) ;
#32049 = CARTESIAN_POINT ( 'NONE',  ( 1.217323170181688008, 3.111755683774203085, -0.7749999999999910294 ) ) ;
#32050 = CARTESIAN_POINT ( 'NONE',  ( 2.395853177668628931, -2.093565527891564582, 0.3158384217898829727 ) ) ;
#32051 = PRESENTATION_LAYER_ASSIGNMENT (  '', '', ( #125527 ) ) ;
#32052 = CARTESIAN_POINT ( 'NONE',  ( 0.000000000000000000, 0.5000000000000000000, 0.000000000000000000 ) ) ;
#32053 = ORIENTED_EDGE ( 'NONE', *, *, #13361, .F. ) ;
#32055 = CARTESIAN_POINT ( 'NONE',  ( -1.364683531250014514, 0.3427083336747508424, 0.7879004041258379498 ) ) ;
#32054 = CARTESIAN_POINT ( 'NONE',  ( 2.701037021348651646, 1.938191879511786730, 1.223809664465740354 ) ) ;
#32056 = CARTESIAN_POINT ( 'NONE',  ( 2.171277156482887882, 5.684907115872006145, -0.7998128361456291469 ) ) ;
#32057 = CARTESIAN_POINT ( 'NONE',  ( 5.355634372598031767, 6.206993841907870291, -1.199719254218445830 ) ) ;
#32058 = CARTESIAN_POINT ( 'NONE',  ( 4.776165916792348476, 2.197254790419100434, -0.3252806346676767046 ) ) ;
#32059 = CARTESIAN_POINT ( 'NONE',  ( -6.507550544879489252, 9.575597488125954015, 1.082531754730548412 ) ) ;
#32060 = CARTESIAN_POINT ( 'NONE',  ( -5.796211742350026341, 6.069872996917573538, -0.5622600474562855499 ) ) ;
#32061 = CARTESIAN_POINT ( 'NONE',  ( 5.016153647376212277, 5.914896012436124728, 1.082531754730558626 ) ) ;
#32062 = CARTESIAN_POINT ( 'NONE',  ( -7.226132685959434809, 8.493204890783200511, 1.082531754730549967 ) ) ;
#32063 =( BOUNDED_SURFACE ( )  B_SPLINE_SURFACE ( 3, 2, ( 
 ( #193736, #157001, #41122 ),
 ( #110435, #191594, #42189 ),
 ( #59476, #173255, #44313 ),
 ( #108304, #92010, #158068 ),
 ( #28049, #7510, #9656 ),
 ( #75732, #43255, #109374 ),
 ( #26966, #93072, #159114 ),
 ( #142906, #177504, #127781 ),
 ( #208906, #60539, #160181 ),
 ( #77855, #45382, #111498 ) ),
 .UNSPECIFIED., .F., .F., .T. ) 
 B_SPLINE_SURFACE_WITH_KNOTS ( ( 4, 2, 2, 2, 4 ),
 ( 3, 3 ),
 ( -2.385244779468109755E-18, 0.001523370301547610686, 0.001904212876934514116, 0.002285055452321417546, 0.003046740603095223973 ),
 ( 0.000000000000000000, 1.000000000000000000 ),
 .UNSPECIFIED. ) 
 GEOMETRIC_REPRESENTATION_ITEM ( )  RATIONAL_B_SPLINE_SURFACE ( (
 ( 1.000000000000000000, 0.8509629433967623724, 1.000000000000000000),
 ( 1.000000000000000000, 0.8506945359964187547, 1.000000000000000000),
 ( 1.000000000000000000, 0.8506364743628531677, 1.000000000000000000),
 ( 1.000000000000000000, 0.8494736702895108182, 1.000000000000000000),
 ( 1.000000000000000000, 0.8491834653876565442, 1.000000000000000000),
 ( 1.000000000000000000, 0.8486037118729093942, 1.000000000000000000),
 ( 1.000000000000000000, 0.8483092994974581469, 1.000000000000000000),
 ( 1.000000000000000000, 0.8474113007901487027, 1.000000000000000000),
 ( 1.000000000000000000, 0.8467927356708078168, 1.000000000000000000),
 ( 1.000000000000000000, 0.8462409035376579070, 1.000000000000000000) ) ) 
 REPRESENTATION_ITEM ( '' )  SURFACE ( )  );
#32064 = CARTESIAN_POINT ( 'NONE',  ( 5.261973015879598314, 5.311592404713873172, -0.7216878364870458196 ) ) ;
#32065 = ORIENTED_EDGE ( 'NONE', *, *, #122192, .F. ) ;
#32066 = CARTESIAN_POINT ( 'NONE',  ( 3.164685561777963230, 1.281361203394768111, 1.556908733426412450 ) ) ;
#32068 = CARTESIAN_POINT ( 'NONE',  ( 1.288015978462764277, -1.305315335096700613, -1.597021576285734268 ) ) ;
#32067 = CARTESIAN_POINT ( 'NONE',  ( 7.450369105909416589, 8.650851030771185890, -1.199719254218441611 ) ) ;
#32069 = DIRECTION ( 'NONE',  ( -0.000000000000000000, -1.000000000000000000, -0.000000000000000000 ) ) ;
#32070 = ADVANCED_FACE ( 'NONE', ( #5615 ), #117619, .T. ) ;
#32071 = CARTESIAN_POINT ( 'NONE',  ( 4.190878879955609371, 7.903459436674603822, -0.7216878364870338292 ) ) ;
#32072 = CARTESIAN_POINT ( 'NONE',  ( -9.586610838029429260, -7.161464053357574855, 0.003376046620574835178 ) ) ;
#32073 = CARTESIAN_POINT ( 'NONE',  ( -1.201851678989727383E-14, 3.696875000341422801, -1.575800808251660134 ) ) ;
#32074 = CARTESIAN_POINT ( 'NONE',  ( 5.296902861200166512, 1.790115547914197247, 1.263834295783084150 ) ) ;
#32075 = CARTESIAN_POINT ( 'NONE',  ( 1.951796282902381163, -1.844710420878793444, -0.8146254186931353169 ) ) ;
#32076 = CARTESIAN_POINT ( 'NONE',  ( 1.593040506729075823, -0.6195558395927207584, 1.734028948791266345 ) ) ;
#32077 = CARTESIAN_POINT ( 'NONE',  ( 8.782984583554449998, 9.141236857102018831, 1.040834085586084257E-14 ) ) ;
#32078 = CARTESIAN_POINT ( 'NONE',  ( 5.069292194207453583, 0.1776299070984053985, -1.816928125296768393 ) ) ;
#32079 = CARTESIAN_POINT ( 'NONE',  ( 6.610000000000006537, 0.002781820520842553934, 2.000159646111852929 ) ) ;
#32080 = CARTESIAN_POINT ( 'NONE',  ( -8.227100285394159940, 8.492705175914988303, 0.7998128361456602331 ) ) ;
#32082 = CARTESIAN_POINT ( 'NONE',  ( -4.471156797456668386, 8.438376373666578445, -0.7998128361456362523 ) ) ;
#32081 = CARTESIAN_POINT ( 'NONE',  ( 4.417028899805944597, 2.066919071766720517, 0.9206345982136554529 ) ) ;
#32083 = CARTESIAN_POINT ( 'NONE',  ( 0.7859291816119529095, 1.415994179718871759, 1.559173624910270783 ) ) ;
#32084 = CARTESIAN_POINT ( 'NONE',  ( -7.747558435566414659, 8.003516027774422170, -0.7998128361456362523 ) ) ;
#32085 = CARTESIAN_POINT ( 'NONE',  ( 4.633297751427938316, 0.003287558298453730800, -2.070544812459538253 ) ) ;
#32086 = CARTESIAN_POINT ( 'NONE',  ( 8.269583629331492602, 11.73526576994040482, 1.199719254218450271 ) ) ;
#32087 = CARTESIAN_POINT ( 'NONE',  ( 4.122904863638303219, 7.664607755345567597, -0.7618067034359333745 ) ) ;
#32088 =( NAMED_UNIT ( * ) PLANE_ANGLE_UNIT ( ) SI_UNIT ( $, .RADIAN. ) );
#32090 = EDGE_CURVE ( 'NONE', #20648, #185214, #46033, .T. ) ;
#32089 = CARTESIAN_POINT ( 'NONE',  ( -6.679363233026820446, 10.94434087183997129, 0.000000000000000000 ) ) ;
#32091 = UNCERTAINTY_MEASURE_WITH_UNIT (LENGTH_MEASURE( 1.000000000000000082E-05 ), #209041, 'distance_accuracy_value', 'NONE');
#32092 = CARTESIAN_POINT ( 'NONE',  ( 6.607619761813720238, 8.802252036906432764, 1.599625672291268286 ) ) ;
#32093 = CARTESIAN_POINT ( 'NONE',  ( 5.387724311900628393, 6.300193624175450147, -1.063853923354351361 ) ) ;
#32094 = CARTESIAN_POINT ( 'NONE',  ( -8.487040972474682476, 12.84537220128841817, 0.7216878364870338292 ) ) ;
#32096 = CARTESIAN_POINT ( 'NONE',  ( 1.354101172232239580, -1.613524214714330940, -1.527088627841047375 ) ) ;
#32095 = CARTESIAN_POINT ( 'NONE',  ( 1.512141599020993432, -0.7094941370262074498, 1.998545949238240027 ) ) ;
#32097 = CIRCLE ( 'NONE', #194589, 0.04999999999999991257 ) ;
#32098 = CARTESIAN_POINT ( 'NONE',  ( 5.038060948978250408, 7.997685013099862239, -1.157798351953726490 ) ) ;
#32099 = CARTESIAN_POINT ( 'NONE',  ( -7.370792787684826486, 8.628288336167626582, -1.199719254218452047 ) ) ;
#32100 = CARTESIAN_POINT ( 'NONE',  ( 6.908042961362778733, 8.018137195466769285, 1.199719254218462483 ) ) ;
#32101 = CARTESIAN_POINT ( 'NONE',  ( 3.596105239937871456, 0.8843387906064968940, -1.751336483779348585 ) ) ;
#32102 = CARTESIAN_POINT ( 'NONE',  ( 4.462605117192430804, 8.358123070033169455, 1.040834085586084257E-14 ) ) ;
#32103 = CARTESIAN_POINT ( 'NONE',  ( -4.338815981289680934, 7.218015932674029855, 1.009429000442535918 ) ) ;
#32104 = CARTESIAN_POINT ( 'NONE',  ( 4.033714395265605823, 4.664753868353354704, -1.199719254218446718 ) ) ;
#32105 = CARTESIAN_POINT ( 'NONE',  ( -5.316205630334263965, 7.295602216847000498, -1.443375672974066548 ) ) ;
#32106 = CARTESIAN_POINT ( 'NONE',  ( -7.537970219518089543, 8.857015346601659900, -1.082531754730543971 ) ) ;
#32107 = CARTESIAN_POINT ( 'NONE',  ( 2.478903650112133317, -1.459102030866548994, 1.539066919819010781 ) ) ;
#32108 = CARTESIAN_POINT ( 'NONE',  ( -6.608673532018475960, 6.674816973635147477, -0.7998128361456362523 ) ) ;
#32109 = CARTESIAN_POINT ( 'NONE',  ( 5.389097038490845648, 0.1425914310585977562, 1.956722230749983193 ) ) ;
#32110 = CARTESIAN_POINT ( 'NONE',  ( 2.922914210685311431, 2.035003303901411265, 0.7295308445595325431 ) ) ;
#32111 = CARTESIAN_POINT ( 'NONE',  ( 2.665370095338463585, 0.9869154847663293983, 1.554228294351194473 ) ) ;
#32112 = CARTESIAN_POINT ( 'NONE',  ( -4.014146127519945928, 7.627013291057631150, 0.008764090477326666462 ) ) ;
#32113 = CARTESIAN_POINT ( 'NONE',  ( 1.364683531249986537, -0.8239583329919186738, 0.7879004041258500513 ) ) ;
#32114 = CARTESIAN_POINT ( 'NONE',  ( 4.400191647014492169, 1.342938829013840207, -1.106906270395467295 ) ) ;
#32115 = CARTESIAN_POINT ( 'NONE',  ( -4.868786560638931782, 6.773613302202437403, 1.443375672974058777 ) ) ;
#32116 = CARTESIAN_POINT ( 'NONE',  ( 3.551873057100283226, 6.127307085716883428, 1.082531754730558626 ) ) ;
#32117 = CARTESIAN_POINT ( 'NONE',  ( -1.138412281109779656E-15, -9.756397064627572391, 9.569424307476239733 ) ) ;
#32118 = CARTESIAN_POINT ( 'NONE',  ( 1.762795743007524063, -1.528684080660724920, 1.528680807790387286 ) ) ;
#32119 = PRESENTATION_LAYER_ASSIGNMENT (  '', '', ( #108249 ) ) ;
#32120 = CARTESIAN_POINT ( 'NONE',  ( 5.026720154644213068, 1.994564127574052215, -0.2930270067487000252 ) ) ;
#32121 = CARTESIAN_POINT ( 'NONE',  ( -9.449669878600623463, 11.08733161553131197, -1.082531754730537976 ) ) ;
#32123 = AXIS2_PLACEMENT_3D ( 'NONE', #171223, #38037, #158195 ) ;
#32122 = CARTESIAN_POINT ( 'NONE',  ( 0.7257156204387126275, -2.052300050329861847, 0.6792298617422781737 ) ) ;
#32124 = ADVANCED_FACE ( 'NONE', ( #108991 ), #95465, .T. ) ;
#32125 = CARTESIAN_POINT ( 'NONE',  ( 2.372288100061814564, -1.215664946315485606, 1.551802774678180619 ) ) ;
#32126 = CARTESIAN_POINT ( 'NONE',  ( 6.509000000000034092, 7.052765612591089806, 2.598154238703707541 ) ) ;
#32127 = CARTESIAN_POINT ( 'NONE',  ( 3.737779845645439636, 1.932976868219363764, 0.1874624384631869700 ) ) ;
#32130 = ORIENTED_EDGE ( 'NONE', *, *, #133645, .F. ) ;
#32129 = DIRECTION ( 'NONE',  ( 0.000000000000000000, 0.000000000000000000, 1.000000000000000000 ) ) ;
#32128 = CARTESIAN_POINT ( 'NONE',  ( -8.148087131688679818, 12.44992605370473804, -0.7216878364870267237 ) ) ;
#32131 = CARTESIAN_POINT ( 'NONE',  ( -3.133342898089680695, 6.669667457830990465, 0.7216878364870338292 ) ) ;
#32132 = CARTESIAN_POINT ( 'NONE',  ( 3.953084306836263995, 6.769626237021087789, 1.199719254218452047 ) ) ;
#32134 = ORIENTED_EDGE ( 'NONE', *, *, #115015, .F. ) ;
#32133 = CARTESIAN_POINT ( 'NONE',  ( -5.764151584465413869, 6.753873599078290546, -1.199719254218453823 ) ) ;
#32135 = CARTESIAN_POINT ( 'NONE',  ( -7.497295758232720431, 10.73030023703809555, -1.082531754730543083 ) ) ;
#32136 = CARTESIAN_POINT ( 'NONE',  ( 1.290363523627102049, -0.9912053058820711193, 1.971723787660728977 ) ) ;
#32137 = CARTESIAN_POINT ( 'NONE',  ( 0.000000000000000000, -0.8968749995220406390, -3.793834371823813001 ) ) ;
#32138 = CIRCLE ( 'NONE', #201561, 11.95586206896558146 ) ;
#32139 = CARTESIAN_POINT ( 'NONE',  ( 5.366048076001885825, -1.952644961629325548, 0.1885061251027941032 ) ) ;
#32140 = CARTESIAN_POINT ( 'NONE',  ( 3.221969581791602977, 0.9480887764680032692, -1.893252576601434756 ) ) ;
#32141 = CARTESIAN_POINT ( 'NONE',  ( -0.7500000000000006661, 2.639583334016156080, -1.299038105676652011 ) ) ;
#32142 = CARTESIAN_POINT ( 'NONE',  ( 9.499700864329909678, -7.154544010627095219, 0.07538891330675548397 ) ) ;
#32143 = CARTESIAN_POINT ( 'NONE',  ( 4.558453444723221892, -1.645810703501834782, -0.8254300276653584456 ) ) ;
#32144 = VERTEX_POINT ( 'NONE', #17785 ) ;
#32145 = CARTESIAN_POINT ( 'NONE',  ( -7.640183256500752584, 8.872300873127729304, -1.199719254218446718 ) ) ;
#32146 = FACE_OUTER_BOUND ( 'NONE', #97014, .T. ) ;
#32147 = CARTESIAN_POINT ( 'NONE',  ( 5.678019686890188211, 2.088907387943875982, -0.3644037002746222664 ) ) ;
#32148 = LINE ( 'NONE', #52654, #77189 ) ;
#32149 = CARTESIAN_POINT ( 'NONE',  ( 4.964256800898067645, 8.943383367689749619, 0.7998128361456462443 ) ) ;
#32150 = AXIS2_PLACEMENT_3D ( 'NONE', #175874, #27463, #110921 ) ;
#32151 = CARTESIAN_POINT ( 'NONE',  ( 6.257116178607133428, -1.765205416791076010, -1.063208849337776485 ) ) ;
#32154 = CARTESIAN_POINT ( 'NONE',  ( 4.159580895514263688, 0.8717668643758098579, 1.621812032879976329 ) ) ;
#32153 = CARTESIAN_POINT ( 'NONE',  ( 1.345918344774723163, -0.8409936141995101311, 1.660288665089631799 ) ) ;
#32152 = CARTESIAN_POINT ( 'NONE',  ( -4.293142477272898994, 3.903087733106795021, 0.2764223219648706542 ) ) ;
#32155 = CARTESIAN_POINT ( 'NONE',  ( 6.988338112840064120, 10.24047933403371502, 1.199719254218460707 ) ) ;
#32156 = CARTESIAN_POINT ( 'NONE',  ( -11.31269326259043062, 3.603011019375360391, 3.682594235848481556 ) ) ;
#32157 =( BOUNDED_SURFACE ( )  B_SPLINE_SURFACE ( 3, 3, ( 
 ( #66773, #198919, #50565, #116686, #35369, #101444, #118823, #136094, #169646, #7123, #39648, #38587, #205331, #71051, #104664, #137167, #21231, #69982, #173949, #25523, #24441, #206405, #56969, #106839, #91631, #170711, #4973, #124194, #105757, #123142, #189100, #22296, #202110, #54837, #73196, #171783, #40733, #139302, #88409, #23379, #157683, #53770, #154477, #103589, #119903, #190157, #90553, #172870, #156616, #185877, #6055, #8206, #72126, #203191, #138233, #188020, #204247, #37513, #87335, #153402, #55899, #74291, #120988, #155544, #140386, #186955, #122056, #89489, #58030, #41812, #107925, #108985, #129523, #10332, #111114, #175004, #42877, #95895, #128459, #26590, #112189, #179261, #61232, #63367, #60160, #46068, #211729, #28735, #30883, #94820, #93755, #77475, #195503, #160871, #96962, #47139, #113256, #59093, #125253, #45005, #127387, #9281, #177118, #12465, #75353, #62300, #178193, #145729, #191214, #209586, #29810, #126315, #76406, #92691, #161948, #158737, #142515, #141466, #207474, #144657, #143594, #208524, #192275, #43936, #110051, #176064, #27660, #159794, #11397, #193360, #13540, #78540, #210672, #194427, #79610, #98023, #64433, #114321, #163010, #182426, #117508, #118573, #52447, #147827, #200796, #167269, #134789, #83865, #213846, #183501, #198668, #18854, #184559, #149956, #80689, #197614, #35109, #49258, #1525, #65464, #151027, #115379, #166188, #51387, #67589, #131615, #181373, #180319, #32997, #146780, #15658, #81745, #31939, #82803, #164078, #99074, #165127, #36180, #16718, #14593, #148879, #212795, #199741, #130577, #68665, #452, #196567, #66520, #101180, #132663, #48209, #50315, #116433, #84938, #34053, #100126, #17777, #133734, #2596, #172610, #203992, #154215, #170452, #86011, #57779, #70794, #72944, #119643, #205073, #106582, #103329, #136907, #169392, #104403, #186698, #185626, #39394, #89232, #22037, #168330, #201862, #105489, #202934, #153144, #189908, #123940, #102256, #20977, #156359, #56715, #88148, #122884, #38327, #7944, #139047, #152085, #19925, #4719, #54577, #5787, #69733, #120725, #71864, #55640, #188842, #37259, #137973, #171522, #40478, #24186, #121796, #187764, #3655, #23115, #155284, #87074, #6865, #90290, #135837, #74034, #53508, #140125, #206151, #95649, #93505, #210417, #45821, #209333, #159546, #41553, #109805, #126062, #42623, #190958, #78288, #157432, #177944, #211480, #108733, #9025, #161700, #11143, #207221, #107666, #60981, #62059, #63116, #145484, #26334, #79366, #111942, #13293, #176869, #92448, #128214, #77220, #29558, #129281, #28481, #173694, #76160, #194176, #142265, #94572, #158487, #25270, #208276, #44756, #144415, #160616, #10086, #59908, #58844, #192025, #91372, #174761, #43688, #125001, #175814, #27407, #143339, #127135, #75100, #193106, #141210, #110863, #12217, #17529, #18611, #100930, #31695, #84691, #81499, #83617, #15408, #167018, #113004, #196321, #67338, #150778, #97770, #146533, #64191, #163830, #51131, #82550, #32744, #49010, #179015, #2340, #147577, #165944, #212550, #149699, #199485, #47965, #213596, #114081, #197368, #65220, #130332, #132421, #182174, #115129, #46891, #80433, #198422, #131372, #181124, #68417, #195255, #30631, #180072, #34855, #1280, #98826, #133483, #164875, #96717, #117253, #162766, #14344, #16470, #148637, #203, #66273, #50066 ),
 ( #116189, #33803, #99882, #183252, #137726, #6615, #52195, #70539, #155030, #152889, #69480, #103080, #38080, #136658, #156101, #134544, #85757, #202683, #171268, #168079, #5533, #203745, #184307, #7687, #35931, #54332, #170200, #102009, #19677, #40217, #135588, #21784, #151838, #3414, #72695, #39147, #201609, #22862, #90043, #186443, #188584, #185376, #88975, #122623, #153966, #200549, #71613, #4467, #120471, #106326, #55390, #118321, #172349, #23939, #53258, #119388, #87893, #104152, #36996, #121545, #187516, #169135, #105228, #138790, #56461, #20730, #204810, #86825, #190706, #140949, #25012, #110612, #41301, #189650, #139866, #193914, #209078, #142011, #161439, #42367, #206962, #124746, #108478, #174502, #57531, #26079, #91114, #176612, #123688, #143085, #109552, #92193, #8768, #107409, #10884, #43428, #158242, #60715, #74850, #9831, #58591, #157173, #73770, #177683, #29295, #28224, #210150, #126879, #94317, #95388, #75907, #208026, #127960, #175557, #192836, #44495, #59653, #205897, #125811, #76959, #27147, #160358, #11961, #173432, #191773, #111676, #93251, #159285, #78034, #144159, #45561, #61793, #116989, #113812, #115924, #47698, #133214, #145215, #14075, #99617, #199220, #63916, #178755, #96454, #130072, #83348, #114861, #64967, #81235, #211222, #182989, #196067, #198164, #30367, #181912, #17271, #80165, #179812, #146270, #15149, #97508, #162505, #164618, #214380, #147317, #79097, #112743, #16203, #31431, #163565, #100674, #34606, #13020, #212282, #67079, #33544, #213344, #165683, #131121, #50867, #49798, #62848, #129009, #197109, #48748, #180861, #194986, #32483, #98557, #82285, #149433, #148378, #66010, #132159, #1014, #46622, #120204, #70281, #166753, #20477, #36731, #167814, #101747, #206438, #68151, #91665, #125286, #19414, #134284, #9313, #4213, #118064, #18348, #186179, #124228, #191246, #59128, #151579, #207509, #173982, #141501, #87632, #3147, #190187, #202414, #25554, #42910, #153704, #84427, #201349, #41843, #52989, #5272, #69216, #157717, #119126, #169937, #58062, #71350, #135335, #185106, #184049, #102818, #150516, #85492, #168873, #35668, #86564, #152626, #136397, #54070, #2077, #200289, #37813, #140421, #103889, #107955, #75387, #21521, #51940, #176098, #111154, #193397, #126352, #46105, #95927, #28772, #175038, #208557, #112223, #209625, #159834, #196598, #64468, #130610, #27698, #163047, #63401, #177154, #211763, #45041, #14626, #79646, #92725, #109019, #11434, #61266, #12502, #76444, #127425, #94854, #210707, #195539, #43971, #160905, #178230, #129554, #113289, #62335, #78574, #26624, #144694, #128494, #110086, #93795, #145762, #10367, #30919, #158772, #77510, #142552, #80721, #194462, #60192, #192312, #29845, #47176, #143630, #212830, #161982, #146812, #179296, #13573, #96995, #33029, #2624, #83895, #52474, #19954, #183532, #180350, #82836, #68695, #148911, #35138, #99107, #36206, #485, #51416, #151061, #101212, #165158, #16751, #65498, #66552, #31975, #115411, #181404, #131646, #182458, #49295, #132694, #198701, #3685, #50345, #86038, #116466, #69762, #84969, #152114, #168359, #34086, #135868, #100158, #134818, #166221, #17811, #48241, #149985, #197648, #164108, #199771, #1558, #67619, #167298, #133763, #117537, #18884, #200823, #114354, #118600, #98054, #184588, #102282, #15692, #81778, #147860 ),
 ( #213876, #24216, #9057, #22066, #136939, #41582, #171551, #40509, #188869, #170481, #53537, #186732, #205102, #23146, #106613, #139078, #88178, #89262, #157462, #119669, #154249, #21006, #185656, #107697, #7973, #56743, #74062, #37287, #138004, #140155, #5821, #202966, #71896, #105517, #204021, #75132, #201887, #153173, #55669, #90318, #87103, #72973, #122911, #103360, #169423, #4748, #121825, #155312, #70823, #54606, #173723, #120754, #6895, #38355, #104433, #206179, #172640, #187795, #156388, #39423, #57808, #25301, #123969, #189937, #91402, #160645, #96746, #12245, #11175, #209366, #113038, #78320, #14373, #195288, #46920, #190989, #42653, #176900, #193139, #129311, #28513, #94603, #179044, #194207, #177975, #63148, #108763, #127169, #95676, #43719, #208308, #92477, #29589, #174789, #26363, #207250, #30662, #62085, #61011, #141241, #109835, #59938, #192055, #175845, #27436, #125032, #93534, #158517, #159578, #77252, #10115, #143368, #76190, #144444, #162796, #44787, #58876, #110893, #142298, #126093, #210447, #128243, #45852, #111973, #161730, #13322, #79395, #145513, #211512, #184345, #35968, #34891, #2375, #67374, #117289, #102046, #115162, #15440, #134582, #50101, #133516, #199522, #49042, #146563, #65253, #83648, #116222, #51167, #17562, #181156, #182213, #168115, #212582, #32779, #114110, #64222, #200582, #100963, #149734, #167052, #130363, #16503, #18644, #98857, #81529, #164908, #198456, #82584, #80463, #196352, #31728, #148670, #183286, #180102, #165978, #1312, #47995, #97801, #163861, #237, #33837, #147609, #213628, #52230, #131402, #99917, #197399, #66310, #84723, #150812, #132457, #68453, #118358, #71648, #73806, #70574, #56499, #7724, #39180, #189684, #105265, #104187, #87927, #205931, #171305, #107444, #139900, #57564, #69516, #135624, #55427, #137762, #123721, #121579, #187550, #41336, #72731, #122657, #156140, #201645, #5569, #188620, #136692, #86861, #185412, #40252, #53292, #119425, #85794, #19715, #155066, #154001, #151874, #202717, #152926, #54368, #3448, #4504, #120508, #37030, #203782, #20767, #186484, #38116, #103116, #170237, #169173, #21821, #22897, #106363, #89013, #6654, #138827, #204846, #172387, #23975, #90077, #145251, #143121, #174536, #45595, #211257, #9865, #124780, #42403, #75941, #29329, #60751, #10918, #27180, #157204, #129049, #142042, #144194, #190739, #61826, #177720, #26112, #208057, #92224, #175590, #43466, #108510, #110645, #160392, #93286, #25048, #58627, #176646, #59684, #125844, #46657, #195024, #173469, #158275, #13054, #127993, #159322, #193948, #109585, #79135, #210188, #8801, #91150, #191801, #76994, #209113, #140987, #126914, #192871, #44527, #111711, #28258, #94351, #11993, #95423, #161476, #78068, #62880, #74880, #206996, #197143, #113850, #47732, #149467, #14110, #34640, #68184, #179845, #80199, #166786, #164654, #63951, #112778, #132190, #67116, #134315, #2110, #97542, #150548, #117027, #84458, #33577, #163600, #133249, #148415, #183024, #200323, #99650, #30403, #147349, #199255, #213376, #165719, #15182, #100711, #64999, #115958, #1051, #17307, #81271, #131153, #130106, #48781, #18380, #50901, #114897, #178790, #180895, #96490, #83385, #162540, #146303, #32517, #98591, #16238, #212315, #82322, #159460, #66047, #196099, #31469, #198199, #49833, #181948, #56230, #5301 ),
 ( #19445, #106097, #103923, #3177, #51973, #71383, #6386, #7457, #155867, #36764, #89821, #122391, #23713, #187285, #102850, #72458, #87663, #188348, #73534, #38912, #184083, #86594, #138559, #152660, #104996, #168905, #39987, #4242, #55166, #154799, #171036, #20509, #70313, #69248, #136429, #35701, #119154, #185137, #135365, #186212, #53021, #202444, #54100, #139637, #120236, #118099, #37844, #101777, #88743, #167845, #172119, #169967, #85522, #21553, #151608, #201381, #153733, #137495, #203511, #204580, #121311, #22633, #189424, #41065, #24779, #91951, #58362, #140718, #8533, #57296, #75677, #90881, #108246, #107173, #174270, #158013, #173199, #156942, #74612, #206732, #124516, #190474, #42134, #25844, #9600, #205660, #141787, #123461, #36772, #55173, #186221, #187294, #173206, #69256, #3185, #22642, #172126, #24786, #107180, #202454, #41073, #7464, #189431, #138566, #54108, #23720, #38920, #73543, #90889, #204587, #135373, #37852, #89827, #103931, #56239, #120243, #205667, #169975, #6393, #106104, #122398, #21563, #87669, #20519, #153741, #201391, #70321, #136438, #86602, #137502, #4252, #5309, #71390, #53029, #203519, #119162, #121318, #185148, #39996, #102858, #123468, #105004, #168914, #171043, #152668, #88750, #154807, #72466, #188356, #155875, #139646, #57305, #108255, #25851, #207799, #12788, #44263, #208856, #10662, #140726, #112508, #125585, #127727, #174276, #45329, #161202, #158020, #191545, #9608, #159066, #26916, #91961, #94092, #143927, #76734, #8540, #110385, #60487, #142852, #160131, #30130, #178520, #156948, #75685, #210988, #111448, #126645, #177453, #93025, #62615, #193685, #206739, #74622, #59427, #109326, #192610, #124524, #175334, #176390, #27995, #29067, #141795, #43210, #11730, #95150, #78862, #77806, #209922, #58370, #61561, #144983, #128777, #194754, #46391, #190481, #42140, #51723, #163336, #63693, #150293, #148156, #47468, #117845, #50639, #18117, #83126, #132992, #183837, #130893, #31207, #1860, #65783, #149206, #781, #64751, #162270, #81009, #82064, #129847, #195830, #214157, #196887, #131933, #96219, #13857, #48525, #113583, #79934, #67921, #116765, #99399, #182763, #146039, #32263, #34380, #114645, #97281, #180638, #197943, #98330, #212053, #179585, #14915, #164396, #198993, #147097, #181688, #165452, #213121, #15979, #49571, #115696, #33318, #17047, #66848, #134065, #100453, #166526, #84204, #200074, #122136, #154555, #69000, #138311, #205414, #87420, #89571, #86345, #72203, #23459, #54916, #57053, #121067, #119984, #103676, #7205, #187035, #123217, #155620, #73278, #85272, #151359, #71132, #153486, #139382, #137250, #203270, #35446, #88494, #204326, #171865, #2928, #21313, #55984, #152416, #102602, #201133, #188102, #135117, #52771, #101525, #167595, #170793, #169724, #19194, #3995, #168656, #70064, #136176, #202195, #118907, #53851, #184891, #38667, #36515, #5057, #20261, #185961, #37593, #104746, #22385, #6134, #39733, #105838, #190234, #157764, #41893, #140475, #189181, #78623, #207554, #109071, #76490, #61320, #124276, #75436, #126401, #143684, #193451, #142600, #92778, #40818, #42962, #59174, #108004, #174031, #11489, #90638, #111204, #144747, #25602, #156698, #28822, #26675, #206487, #106926, #208610, #209676, #210759, #62379, #91715, #12548, #45095, #160958, #110138, #9364, #127480 ),
 ( #10418, #172950, #27750, #77561, #177208, #24529, #175087, #94907, #141548, #125333, #58117, #8289, #74373, #191296, #158822, #60242, #176150, #192361, #44019, #93846, #159884, #179348, #163098, #30970, #112270, #80775, #79695, #81827, #100204, #114402, #128543, #97045, #63452, #29893, #65548, #98105, #14678, #49341, #129605, #146862, #195591, #145808, #194509, #17862, #83945, #82883, #50395, #115460, #165209, #150036, #212884, #47225, #182505, #164156, #181450, #33081, #64515, #46157, #113343, #180400, #95979, #162031, #32020, #130660, #15742, #1606, #178284, #196650, #13622, #211815, #34135, #148960, #131693, #532, #48290, #147910, #66599, #213925, #197699, #99156, #16799, #132745, #198747, #116515, #166270, #167347, #187844, #68746, #169470, #18933, #101263, #154296, #186779, #85019, #170531, #23194, #119723, #121873, #118652, #104488, #55719, #87152, #89310, #153223, #152164, #135914, #39470, #4793, #155357, #105568, #171601, #117589, #183580, #103409, #185702, #67666, #21055, #70871, #133810, #120803, #22116, #204067, #35187, #53588, #88227, #184638, #134868, #151108, #5871, #2674, #200875, #199824, #51465, #203013, #201932, #52520, #36255, #102335, #168407, #20004, #86088, #3733, #69808, #37336, #136986, #54655, #38406, #71944, #138054, #156440, #122959, #158568, #191042, #189983, #142350, #8024, #41635, #74114, #172688, #6942, #110943, #176950, #175897, #143421, #208360, #43771, #28566, #107749, #140209, #61061, #42707, #59991, #126144, #173775, #73023, #206229, #207303, #188919, #40557, #58925, #25350, #108815, #94653, #139121, #91450, #106662, #205148, #127220, #27488, #10167, #93588, #56791, #157511, #159632, #9106, #57856, #75182, #125084, #141294, #24266, #90371, #124018, #174838, #109884, #26416, #92528, #76241, #11228, #192106, #209415, #77308, #193189, #44837, #285, #212626, #112020, #160697, #180150, #115209, #116268, #50145, #145560, #198500, #164956, #132502, #81574, #211558, #181199, #196399, #16548, #182258, #147658, #78371, #195335, #32827, #46966, #213674, #63193, #148715, #113083, #163911, #49089, #65299, #129357, #179089, #178021, #30711, #144491, #13369, #79443, #29639, #80511, #161777, #96794, #162843, #33883, #14421, #12291, #146608, #210499, #197448, #62134, #66356, #64267, #128294, #130411, #194256, #45902, #95725, #48044, #114157, #98903, #31776, #97848, #15487, #131447, #82630, #170279, #201693, #151916, #168159, #83696, #55471, #68497, #70622, #117337, #202761, #104233, #101011, #134625, #167102, #102089, #184390, #183334, #37079, #86907, #19757, #166025, #53336, #3489, #85839, #103158, #187595, #121626, #99961, #18688, #154046, #54412, #69559, #120552, #36009, #5612, #136736, #149784, #17610, #150857, #52277, #135669, #67420, #118403, #119471, #185458, #186531, #34938, #200629, #169219, #38160, #21867, #20811, #152975, #1358, #4550, #87973, #84771, #2420, #133562, #71695, #137807, #199569, #51213, #203826, #44304, #77845, #6700, #138875, #162310, #40302, #143968, #204893, #72776, #128813, #161242, #56546, #145025, #212092, #94133, #96257, #90123, #78903, #30169, #61601, #63728, #127771, #126689, #110426, #13895, #193727, #129887, #79976, #146080, #89059, #155117, #209962, #160172, #39222, #45371, #111487, #105312, #95191, #211029, #178559, #122706, #28038, #62654, #156190, #106410, #188670 ),
 ( #76774, #10705, #22944, #208897, #172433, #177495, #171351, #11772, #24022, #142897, #60528, #192651, #29108, #12828, #176429, #194794, #46431, #112549, #48565, #147135, #195871, #85315, #151399, #150333, #117884, #182806, #18159, #2971, #16019, #130935, #35489, #165495, #34423, #100496, #164433, #47510, #180678, #181728, #163379, #14953, #33359, #82105, #17089, #69039, #113622, #148198, #81051, #179625, #101567, #1900, #199033, #67960, #31245, #131975, #134104, #214198, #196928, #65827, #99440, #197985, #97322, #213161, #64791, #49613, #84247, #114685, #32303, #83167, #98370, #115738, #149250, #823, #66893, #133033, #50681, #116806, #166571, #200113, #167634, #51764, #183876, #19235, #52813, #71172, #155660, #153528, #70104, #103713, #38708, #137290, #156737, #135156, #86387, #203308, #171907, #168697, #6175, #138351, #184930, #8328, #36554, #54957, #170834, #102641, #20302, #40859, #136217, #22425, #152455, #4034, #7242, #39777, #202237, #23503, #90676, #187075, #189220, #185999, #89609, #123255, #154597, #201174, #72244, #5097, #121109, #106965, #204368, #118951, #172989, #24570, #53889, #120024, #88535, #104788, #37634, #56025, #122179, #169764, #188145, #73319, #57090, #21353, #105882, #139422, #87460, #205457, #25639, #111240, #41930, #190273, #140512, #194544, #209712, #142640, #162066, #42997, #141585, #125368, #109110, #191332, #58155, #26712, #91751, #27786, #46190, #60280, #74413, #175125, #9402, #108042, #11527, #44056, #92814, #61357, #75472, #158858, #207592, #157804, #206524, #178322, #29930, #28857, #210792, #127516, #177244, #96014, #10455, #59211, #128579, #110175, #193488, #45130, #76528, #208649, #174067, #112306, #126437, #192400, #124314, #93884, #94944, #176186, #159923, #77597, #143720, #78656, #160992, #12584, #144784, #62415, #49370, #17893, #199855, #148988, #145844, #48323, #182538, #114434, #563, #212916, #1638, #180433, #16832, #116546, #66629, #64550, #130694, #31004, #196684, #211850, #80806, #146896, #97078, #147944, #14714, #32050, #98139, #183614, #164188, #51496, #15774, #35221, #50427, #117623, #133844, #81860, #101297, #213957, #13656, #79728, #63487, #197730, #65578, #100236, #129642, #131725, #179383, #163131, #115488, #83979, #181481, #33111, #99188, #195628, #47263, #165239, #198778, #82915, #34165, #150067, #132775, #166304, #67697, #113377, #37364, #184668, #104517, #154327, #87185, #18966, #120833, #70904, #21082, #170561, #40589, #122991, #188949, #86121, #6971, #121905, #169500, #55749, #103439, #73052, #138083, #151137, #167377, #3762, #119752, #137015, #134897, #185731, #153250, #54683, #39501, #102366, #53619, #22144, #187874, #171631, #186809, #203042, #85050, #4825, #38437, #168436, #20035, #204097, #68778, #89340, #2704, #200903, #88258, #5901, #71974, #139151, #105599, #52552, #205180, #56822, #118683, #36288, #23228, #155388, #152195, #69837, #135947, #201963, #159660, #143451, #28599, #156471, #92558, #61093, #9138, #173803, #57886, #209448, #74146, #8059, #172719, #12322, #27519, #174869, #194289, #75212, #25381, #157541, #141323, #207336, #90401, #58958, #124049, #60022, #78403, #158598, #106694, #125113, #41667, #140239, #43802, #76272, #191071, #93618, #107778, #42737, #91481, #190015, #24297, #210533, #62167, #127252, #94687, #11261, #193223, #128326, #108843 ),
 ( #10197, #26449, #142380, #206261, #208389, #126174, #192137, #109915, #160729, #44870, #175926, #110975, #77338, #176981, #144523, #64296, #195366, #14452, #163943, #48074, #67451, #45934, #211588, #114185, #82662, #79474, #131476, #49123, #95755, #133596, #161807, #180183, #81603, #13398, #145592, #166057, #46997, #147688, #63224, #129387, #132534, #164989, #113114, #148746, #1390, #97882, #99991, #96823, #315, #33915, #65329, #112053, #149819, #178053, #66386, #182289, #32859, #198531, #29671, #80543, #179119, #17643, #15518, #98934, #16579, #146640, #30742, #162872, #31806, #212655, #130442, #213705, #196429, #197479, #115241, #181231, #50178, #116298, #83728, #39257, #5648, #202796, #71729, #117370, #135702, #137841, #3520, #134656, #168191, #103193, #201728, #6733, #199602, #150890, #53369, #21900, #18718, #70658, #54446, #34971, #72812, #101043, #119504, #20842, #167133, #84802, #105351, #200659, #86941, #2452, #68528, #203863, #104266, #52308, #88010, #155151, #37115, #171388, #36042, #154081, #187630, #4584, #51244, #136768, #69592, #185489, #22979, #120588, #183367, #89098, #118438, #184425, #102122, #153007, #169256, #19790, #186566, #38194, #85872, #170312, #55508, #121662, #151950, #124859, #93369, #41419, #206012, #90162, #175673, #106448, #40342, #204933, #44611, #59771, #207078, #12082, #107526, #57647, #189767, #173557, #25130, #122743, #91232, #156228, #92313, #110727, #190823, #138913, #157292, #73898, #172471, #76025, #108593, #8882, #125930, #139991, #74961, #123807, #7805, #176727, #141071, #160475, #27261, #28340, #94436, #58710, #56584, #42484, #188706, #24059, #174621, #26197, #158356, #11004, #9949, #142128, #208141, #191888, #43550, #209199, #109671, #159405, #77081, #143209, #60839, #127000, #192959, #95509, #180979, #82406, #79221, #46746, #145339, #80286, #162618, #161556, #15266, #65081, #212399, #144279, #31551, #196179, #146385, #81353, #165803, #33657, #99732, #211340, #132270, #32601, #64041, #98676, #14194, #198279, #48864, #61911, #78149, #129134, #30486, #47821, #45679, #96570, #130186, #179928, #164732, #13145, #178875, #147433, #16321, #148495, #97626, #113932, #210273, #163684, #213457, #62964, #195110, #114979, #194029, #63, #128073, #112859, #111796, #49920, #131235, #29418, #177801, #197224, #66127, #116041, #182029, #2194, #55253, #21637, #203600, #152745, #68270, #186298, #53109, #87745, #121400, #4326, #149551, #52053, #37934, #118180, #70396, #134403, #5392, #184167, #20592, #120322, #136514, #200405, #35788, #34718, #101864, #1136, #84543, #150633, #100789, #151697, #18465, #167932, #19532, #187372, #85608, #3265, #86678, #105087, #39002, #17388, #69333, #71469, #104008, #135444, #170052, #201465, #137582, #202533, #67199, #83471, #119242, #185225, #36849, #199340, #102932, #168993, #54182, #153821, #166872, #133336, #50986, #117108, #183109, #124603, #74700, #171125, #24865, #41154, #172209, #106185, #207882, #72548, #93103, #126731, #23799, #138647, #10746, #8618, #122478, #22719, #190563, #125662, #192691, #60572, #155956, #208937, #175413, #142936, #92042, #7542, #191624, #206815, #26996, #44345, #158099, #88833, #205748, #43287, #57380, #9687, #73626, #159144, #123544, #174356, #59505, #75765, #139725, #189508, #188439, #107263, #154888, #89904, #173283, #40073, #90968 ) ),
 .UNSPECIFIED., .T., .F., .T. ) 
 B_SPLINE_SURFACE_WITH_KNOTS ( ( 4, 3, 4 ),
 ( 4, 1, 1, 1, 1, 1, 1, 1, 1, 1, 1, 1, 1, 1, 1, 1, 1, 1, 1, 1, 1, 1, 1, 1, 1, 1, 1, 1, 1, 1, 1, 1, 1, 1, 1, 1, 1, 1, 1, 1, 1, 1, 1, 1, 1, 1, 1, 1, 1, 1, 1, 1, 1, 1, 1, 1, 1, 1, 1, 1, 1, 1, 1, 1, 1, 1, 1, 1, 1, 1, 1, 1, 1, 1, 1, 1, 1, 1, 1, 1, 1, 1, 1, 1, 1, 1, 1, 1, 1, 1, 1, 1, 1, 1, 1, 1, 1, 1, 1, 1, 1, 1, 1, 1, 1, 1, 1, 1, 1, 1, 1, 1, 1, 1, 1, 1, 1, 1, 1, 1, 1, 1, 1, 1, 1, 1, 1, 1, 1, 1, 1, 1, 1, 1, 1, 1, 1, 1, 1, 1, 1, 1, 1, 1, 1, 1, 1, 1, 1, 1, 1, 1, 1, 1, 1, 1, 1, 1, 1, 1, 1, 1, 1, 1, 1, 1, 1, 1, 1, 1, 1, 1, 1, 1, 1, 1, 1, 1, 1, 1, 1, 1, 1, 1, 1, 1, 1, 1, 1, 1, 1, 1, 1, 1, 1, 1, 1, 1, 1, 1, 1, 1, 1, 1, 1, 1, 1, 1, 1, 1, 1, 1, 1, 1, 1, 1, 1, 1, 1, 1, 1, 1, 1, 1, 1, 1, 1, 1, 1, 1, 1, 1, 1, 1, 1, 1, 1, 1, 1, 1, 1, 1, 1, 1, 1, 1, 1, 1, 1, 1, 1, 1, 1, 1, 1, 1, 1, 1, 1, 1, 1, 1, 1, 1, 1, 1, 1, 1, 1, 1, 1, 1, 1, 1, 1, 1, 1, 1, 1, 1, 1, 1, 1, 1, 1, 1, 1, 1, 1, 1, 1, 1, 1, 1, 1, 1, 1, 1, 1, 1, 1, 1, 1, 1, 1, 1, 1, 1, 1, 1, 1, 1, 1, 1, 1, 1, 1, 1, 1, 1, 1, 1, 1, 1, 1, 1, 1, 1, 1, 1, 1, 1, 1, 1, 1, 1, 1, 1, 1, 1, 1, 1, 1, 1, 1, 1, 1, 1, 1, 1, 1, 1, 1, 1, 1, 1, 1, 1, 1, 1, 1, 1, 1, 1, 1, 1, 1, 1, 1, 1, 1, 1, 1, 1, 1, 1, 1, 1, 1, 1, 1, 1, 1, 1, 4 ),
 ( 0.000000000000000000, 0.5000000000000000000, 1.000000000000000000 ),
 ( 0.000000000000000000, 0.002600034503794030130, 0.005208798665460326327, 0.007813183304800875098, 0.01041632952039499814, 0.01302078637366306003, 0.01562487905948694092, 0.01822913957756216313, 0.02083328395591756144, 0.02343739818322774712, 0.02604168118785421884, 0.02864568517727394958, 0.03125004130332968699, 0.03385401862675675722, 0.03645834363201481965, 0.03906241290072134942, 0.04166661303991354287, 0.04427083116291704451, 0.04687488238457573897, 0.04947921467585455341, 0.05208318889621989245, 0.05468754274347345512, 0.05729155431138267807, 0.05989582568988525285, 0.06249996760622017478, 0.06510408932096034551, 0.06770837349117478365, 0.07031237295078232585, 0.07291672927807971161, 0.07552070761765239393, 0.07812503204114096267, 0.08072910085791458468, 0.08333330089851145872, 0.08593751883178461781, 0.08854156980611090078, 0.09114590188302622298, 0.09374987588873062716, 0.09635422952249227124, 0.09895824087764454324, 0.1015625120427016276, 0.1041666537503683765, 0.1067707752516706410, 0.1093750592157429480, 0.1119790584643299974, 0.1145834145867499904, 0.1171873927198607973, 0.1197917169388799108, 0.1223957855539345302, 0.1249999853896588409, 0.1276042031245507580, 0.1302082538950744550, 0.1328125857752754935, 0.1354165595809520839, 0.1380209130188291833, 0.1406249241787864424, 0.1432291951479887082, 0.1458333366646657747, 0.1484374579699756502, 0.1510417417453218114, 0.1536457408005802994, 0.1562500967354857329, 0.1588540746797905134, 0.1614583987117299280, 0.1640624671426803571, 0.1666666667910262079, 0.1692708843450304312, 0.1718749349293641482, 0.1744792666302357464, 0.1770832402535473249, 0.1796875935129024493, 0.1822916044953091785, 0.1848958752860835608, 0.1875000166293293857, 0.1901041377562054102, 0.1927084213602507368, 0.1953124202398235920, 0.1979167760045740521, 0.2005207537777317084, 0.2031250776399721736, 0.2057291459044250093, 0.2083333453828807025, 0.2109375627734847158, 0.2135416131892344249, 0.2161459447281551538, 0.2187499181867580689, 0.2213542712849473904, 0.2239582821074418695, 0.2265625527372090720, 0.2291666939245756707, 0.2317708148905701926, 0.2343750983407339450, 0.2369790970622578097, 0.2395834526742069426, 0.2421874302938704648, 0.2447917540037867212, 0.2473958221193426621, 0.2500000214453905190, 0.2526042386900758108, 0.2552082889548416555, 0.2578126203491843960, 0.2604165936607292231, 0.2630209466151033904, 0.2656249572953180982, 0.2682292277814931625, 0.2708333688305272213, 0.2734374896531870935, 0.2760417729668830367, 0.2786457715479891406, 0.2812501270244852081, 0.2838541045083020076, 0.2864584280832634389, 0.2890624960675178268, 0.2916666952586349781, 0.2942709123748779576, 0.2968749625062547248, 0.2994792937733871119, 0.3020832669555192918, 0.3046876197834237909, 0.3072916303389863768, 0.3098959006989794318, 0.3125000416272227799, 0.3151041623240899980, 0.3177084455187270673, 0.3203124439770417831, 0.3229167993354283839, 0.3255207767010412923, 0.3281251001584127303, 0.3307291680289564662, 0.3333333671026155187, 0.3359375841078879321, 0.3385416341234662174, 0.3411459652807516951, 0.3437499383511121720, 0.3463542910698884647, 0.3489583015184220538, 0.3515625717696388985, 0.3541667125946290073, 0.3567708331832410984, 0.3593751162762241491, 0.3619791146293697692, 0.3645834698869864221, 0.3671874471520340522, 0.3697917705091763874, 0.3723958382835964032, 0.3750000372572658280, 0.3776042541690359799, 0.3802083040864021046, 0.3828126351512001757, 0.3854166081274262856, 0.3880209607544118922, 0.3906249711135359459, 0.3932292412733790488, 0.3958333820126498370, 0.3984375025105409418, 0.4010417855192715542, 0.4036457837848667074, 0.4062501389590495449, 0.4088541161411674008, 0.4114584394154381930, 0.4140625071113177014, 0.4166667060024629166, 0.4192709228381954478, 0.4218749726749327911, 0.4244793036646000717, 0.4270832765643259310, 0.4296876291168554296, 0.4322916394041865784, 0.4348959094900549660, 0.4375000501611374104, 0.4401041705858387276, 0.4427084535277153732, 0.4453124517233759683, 0.4479168068314584583, 0.4505207839482789911, 0.4531251071570330247, 0.4557291747919532399, 0.4583333736180368323, 0.4609375903951940523, 0.4635416401688834398, 0.4661459711007739370, 0.4687499439416310532, 0.4713542964370365795, 0.4739583066701890113, 0.4765625766994796009, 0.4791667173199026797, 0.4817708376889431876, 0.4843751205813623395, 0.4869791187247021202, 0.4895834737840155659, 0.4921874508531692838, 0.4947917740137594000, 0.4973958416052992049, 0.5000000403837819851, 0.5026042571198243714, 0.5052083068480445194, 0.5078126377395105751, 0.5104166105391289010, 0.5130209629947408700, 0.5156249731913270518, 0.5182292431814352618, 0.5208333837687260104, 0.5234375040996330775, 0.5260417869599895990, 0.5286457850686206994, 0.5312501400964950715, 0.5338541171356111503, 0.5364584402653888029, 0.5390625078311259699, 0.5416667065794673608, 0.5442709232918542250, 0.5468749729921829061, 0.5494793038605755298, 0.5520832766365837418, 0.5546876290697317913, 0.5572916392473630243, 0.5598959092156829964, 0.5625000497873680061, 0.5651041700976676685, 0.5677084529433557014, 0.5703124510348895893, 0.5729168060486536929, 0.5755207830753605869, 0.5781251061916765632, 0.5807291737491879768, 0.5833333724848467350, 0.5859375891910368894, 0.5885416388810509325, 0.5911459697437208005, 0.5937499425137473530, 0.5963542949417601768, 0.5989583051180477069, 0.6015625750819736384, 0.6041667156555785567, 0.6067708359627971282, 0.6093751188112106476, 0.6119791169032582356, 0.6145834719202413199, 0.6171874489521673723, 0.6197917720723722379, 0.6223958396392350600, 0.6250000383796699976, 0.6276042550971219214, 0.6302083047943985994, 0.6328126356686964993, 0.6354166084503697354, 0.6380209608905765828, 0.6406249710831318778, 0.6432292410600577437, 0.6458333816531092175, 0.6484375019747732338, 0.6510417848433065480, 0.6536457829534795261, 0.6562501379910111732, 0.6588541150457848383, 0.6614584381872300467, 0.6640625057810221055, 0.6666667045436925898, 0.6692709212898660942, 0.6718749710119833463, 0.6744793019152608426, 0.6770832747262099938, 0.6796876271959411131, 0.6822916374223763070, 0.6848959074296973037, 0.6875000480597228680, 0.6901041684133596421, 0.6927084513194080584, 0.6953124494653194487, 0.6979168045407300180, 0.7005207816359816375, 0.7031251048160196415, 0.7057291724543196532, 0.7083333712566866058, 0.7109375880490425015, 0.7135416378135795989, 0.7161459687631898108, 0.7187499416210458847, 0.7213542941376326345, 0.7239583044155618596, 0.7265625744706748490, 0.7291667151552034820, 0.7317708355583423252, 0.7343751185193033715, 0.7369791167185673064, 0.7395834718491895998, 0.7421874490025512916, 0.7447917722385364314, 0.7473958399389256657, 0.7500000387984516736, 0.7526042556544531026, 0.7552083054789914263, 0.7578126364922896929, 0.7604166094146853627, 0.7630209619954617661, 0.7656249723425013753, 0.7682292424628052174, 0.7708333832193684509, 0.7734375036895410060, 0.7760417867228139865, 0.7786457849930478181, 0.7812501401962168579, 0.7838541174253229604, 0.7864584407346123518, 0.7890625085146746320, 0.7916667074488250577, 0.7942709243859374935, 0.7968749742880611997, 0.7994793053824050810, 0.8020832783869765725, 0.8046876310492792062, 0.8072916414830481058, 0.8098959116859448804, 0.8125000525320774658, 0.8151041730868179291, 0.8177084562098055898, 0.8203124545686294455, 0.8229168098616829186, 0.8255207871841712119, 0.8281251105841250792, 0.8307291784614470043, 0.8333333774876906519, 0.8359375945233833427, 0.8385416445206798075, 0.8411459757134309712, 0.8437499488178175078, 0.8463543015789862789, 0.8489583121171074831, 0.8515625824200027116, 0.8541667233732427311, 0.8567708440300897399, 0.8593751272601987123, 0.8619791257252362726, 0.8645834811255164176, 0.8671874585590289009, 0.8697917820670107991, 0.8723958500591838527, 0.8750000491949933012, 0.8776042663467393812, 0.8802083164568000884, 0.8828126477653241988, 0.8854166209871692228, 0.8880209738645485906, 0.8906249845246493324, 0.8932292549449527552, 0.8958333960228427317, 0.8984375167993386979, 0.9010418001539796107, 0.9036457987428592187, 0.9062501542677121602, 0.9088541318298947180, 0.9114584554632734203, 0.9140625235878931942, 0.9166667228507454634, 0.9192709401360219523, 0.9218749903764450471, 0.9244793218181143191, 0.9270832951750564987, 0.9296876481859919217, 0.9322916589857459524, 0.9348959295408556525, 0.9375000707608250883, 0.9401041916746273319, 0.9427084751713679101, 0.9453124739016935951, 0.9479168295687272483, 0.9505208072738278169, 0.9531251310501845930, 0.9557291993520028450, 0.9583333987332913750, 0.9609376160454207172, 0.9635416666839513589, 0.9661459986354887786, 0.9687499708159389433, 0.9713543235632202677, 0.9739583390673558494, 0.9765626083347638264, 0.9791667417950460361, 0.9817708662416058107, 0.9843751381318576188, 0.9869792129215403387, 0.9895836736503123010, 0.9921868305638316121, 0.9947912020913856068, 0.9973999845648282569, 1.000000000000000000 ),
 .UNSPECIFIED. ) 
 GEOMETRIC_REPRESENTATION_ITEM ( )  RATIONAL_B_SPLINE_SURFACE ( (
 ( 1.000000000000000222, 1.000000000000000222, 1.000000000000000222, 1.000000000000000222, 0.9999999999999996669, 0.9999999999999997780, 1.000000000000000444, 1.000000000000000000, 1.000000000000000000, 1.000000000000000000, 0.9999999999999997780, 1.000000000000000000, 1.000000000000000000, 1.000000000000000000, 1.000000000000000000, 0.9999999999999997780, 1.000000000000000222, 0.9999999999999996669, 1.000000000000000000, 0.9999999999999997780, 1.000000000000000222, 1.000000000000000000, 1.000000000000000222, 0.9999999999999996669, 1.000000000000000000, 1.000000000000000222, 0.9999999999999996669, 1.000000000000000444, 1.000000000000000000, 0.9999999999999997780, 1.000000000000000222, 1.000000000000000222, 1.000000000000000222, 1.000000000000000000, 1.000000000000000000, 0.9999999999999997780, 1.000000000000000000, 1.000000000000000000, 1.000000000000000000, 1.000000000000000000, 1.000000000000000222, 1.000000000000000222, 1.000000000000000000, 1.000000000000000000, 1.000000000000000000, 0.9999999999999996669, 1.000000000000000222, 1.000000000000000000, 1.000000000000000000, 0.9999999999999997780, 0.9999999999999997780, 1.000000000000000000, 0.9999999999999996669, 1.000000000000000222, 0.9999999999999997780, 1.000000000000000222, 0.9999999999999997780, 0.9999999999999997780, 1.000000000000000222, 1.000000000000000222, 0.9999999999999997780, 1.000000000000000222, 1.000000000000000000, 1.000000000000000222, 1.000000000000000000, 0.9999999999999997780, 1.000000000000000000, 1.000000000000000000, 1.000000000000000222, 1.000000000000000222, 1.000000000000000000, 0.9999999999999997780, 1.000000000000000000, 1.000000000000000222, 0.9999999999999997780, 1.000000000000000444, 0.9999999999999996669, 1.000000000000000000, 1.000000000000000222, 0.9999999999999997780, 0.9999999999999997780, 0.9999999999999997780, 1.000000000000000000, 0.9999999999999997780, 1.000000000000000000, 0.9999999999999997780, 1.000000000000000222, 1.000000000000000000, 1.000000000000000222, 1.000000000000000000, 0.9999999999999997780, 1.000000000000000000, 1.000000000000000000, 0.9999999999999997780, 1.000000000000000222, 1.000000000000000000, 1.000000000000000000, 1.000000000000000000, 1.000000000000000222, 0.9999999999999996669, 1.000000000000000222, 1.000000000000000000, 1.000000000000000000, 0.9999999999999997780, 1.000000000000000000, 0.9999999999999997780, 1.000000000000000000, 1.000000000000000222, 1.000000000000000000, 0.9999999999999997780, 1.000000000000000222, 1.000000000000000222, 0.9999999999999996669, 1.000000000000000222, 1.000000000000000000, 1.000000000000000444, 0.9999999999999996669, 1.000000000000000000, 1.000000000000000222, 1.000000000000000222, 1.000000000000000222, 1.000000000000000222, 1.000000000000000000, 0.9999999999999997780, 1.000000000000000222, 1.000000000000000000, 1.000000000000000222, 0.9999999999999996669, 1.000000000000000000, 1.000000000000000000, 1.000000000000000222, 1.000000000000000222, 0.9999999999999997780, 1.000000000000000000, 0.9999999999999997780, 1.000000000000000222, 1.000000000000000000, 1.000000000000000222, 1.000000000000000000, 1.000000000000000444, 0.9999999999999996669, 1.000000000000000444, 0.9999999999999996669, 0.9999999999999997780, 0.9999999999999997780, 1.000000000000000222, 1.000000000000000000, 0.9999999999999997780, 1.000000000000000000, 0.9999999999999997780, 0.9999999999999996669, 1.000000000000000222, 1.000000000000000000, 0.9999999999999997780, 1.000000000000000000, 1.000000000000000000, 1.000000000000000222, 1.000000000000000000, 1.000000000000000000, 1.000000000000000444, 0.9999999999999997780, 1.000000000000000222, 1.000000000000000222, 0.9999999999999997780, 1.000000000000000444, 0.9999999999999996669, 1.000000000000000000, 0.9999999999999997780, 1.000000000000000222, 0.9999999999999997780, 1.000000000000000222, 1.000000000000000000, 1.000000000000000222, 0.9999999999999997780, 0.9999999999999997780, 1.000000000000000000, 1.000000000000000000, 0.9999999999999997780, 1.000000000000000222, 0.9999999999999997780, 1.000000000000000000, 1.000000000000000000, 1.000000000000000222, 1.000000000000000000, 0.9999999999999997780, 1.000000000000000222, 1.000000000000000444, 1.000000000000000000, 1.000000000000000000, 1.000000000000000000, 1.000000000000000000, 0.9999999999999997780, 1.000000000000000000, 1.000000000000000222, 1.000000000000000000, 1.000000000000000222, 0.9999999999999996669, 1.000000000000000000, 1.000000000000000000, 0.9999999999999994449, 1.000000000000000444, 1.000000000000000000, 1.000000000000000222, 0.9999999999999997780, 1.000000000000000000, 1.000000000000000222, 1.000000000000000000, 0.9999999999999996669, 1.000000000000000444, 0.9999999999999997780, 1.000000000000000444, 0.9999999999999996669, 1.000000000000000000, 0.9999999999999996669, 1.000000000000000444, 1.000000000000000000, 0.9999999999999997780, 1.000000000000000222, 1.000000000000000000, 0.9999999999999997780, 1.000000000000000444, 1.000000000000000222, 0.9999999999999997780, 1.000000000000000000, 1.000000000000000222, 0.9999999999999997780, 1.000000000000000222, 1.000000000000000222, 1.000000000000000000, 1.000000000000000000, 0.9999999999999996669, 1.000000000000000222, 0.9999999999999997780, 1.000000000000000000, 0.9999999999999997780, 1.000000000000000444, 1.000000000000000000, 1.000000000000000000, 0.9999999999999997780, 1.000000000000000444, 1.000000000000000000, 0.9999999999999997780, 1.000000000000000444, 0.9999999999999996669, 1.000000000000000444, 1.000000000000000000, 1.000000000000000444, 1.000000000000000222, 1.000000000000000222, 0.9999999999999997780, 1.000000000000000000, 0.9999999999999997780, 1.000000000000000444, 0.9999999999999996669, 1.000000000000000000, 1.000000000000000000, 1.000000000000000222, 1.000000000000000000, 1.000000000000000222, 1.000000000000000000, 1.000000000000000000, 0.9999999999999997780, 1.000000000000000000, 1.000000000000000000, 0.9999999999999997780, 1.000000000000000000, 1.000000000000000000, 0.9999999999999997780, 1.000000000000000000, 1.000000000000000222, 1.000000000000000000, 1.000000000000000000, 1.000000000000000000, 1.000000000000000000, 0.9999999999999996669, 1.000000000000000222, 1.000000000000000000, 0.9999999999999997780, 1.000000000000000000, 1.000000000000000222, 1.000000000000000000, 1.000000000000000222, 1.000000000000000222, 1.000000000000000000, 1.000000000000000222, 1.000000000000000000, 1.000000000000000000, 1.000000000000000000, 1.000000000000000222, 0.9999999999999996669, 1.000000000000000222, 0.9999999999999996669, 1.000000000000000222, 1.000000000000000222, 1.000000000000000222, 1.000000000000000222, 0.9999999999999996669, 1.000000000000000444, 1.000000000000000000, 1.000000000000000000, 1.000000000000000222, 1.000000000000000444, 0.9999999999999996669, 1.000000000000000444, 1.000000000000000222, 0.9999999999999996669, 1.000000000000000222, 0.9999999999999997780, 1.000000000000000000, 1.000000000000000000, 0.9999999999999997780, 1.000000000000000000, 0.9999999999999997780, 1.000000000000000000, 1.000000000000000000, 1.000000000000000444, 0.9999999999999997780, 1.000000000000000222, 0.9999999999999997780, 0.9999999999999997780, 1.000000000000000000, 1.000000000000000000, 0.9999999999999996669, 1.000000000000000000, 1.000000000000000222, 1.000000000000000222, 0.9999999999999997780, 1.000000000000000222, 0.9999999999999997780, 0.9999999999999997780, 1.000000000000000000, 1.000000000000000000, 1.000000000000000000, 1.000000000000000222, 1.000000000000000000, 1.000000000000000222, 1.000000000000000000, 0.9999999999999996669, 0.9999999999999997780, 1.000000000000000444, 0.9999999999999996669, 1.000000000000000444, 0.9999999999999997780, 0.9999999999999997780, 1.000000000000000222, 0.9999999999999997780, 1.000000000000000222, 1.000000000000000000, 1.000000000000000000, 0.9999999999999997780, 1.000000000000000222, 1.000000000000000222, 1.000000000000000000, 1.000000000000000222, 1.000000000000000000, 1.000000000000000000, 0.9999999999999997780, 1.000000000000000000, 1.000000000000000000, 0.9999999999999997780, 1.000000000000000000, 0.9999999999999996669, 1.000000000000000222, 0.9999999999999997780, 1.000000000000000222, 0.9999999999999997780, 1.000000000000000000, 0.9999999999999997780, 1.000000000000000222, 0.9999999999999997780, 1.000000000000000000, 1.000000000000000000, 1.000000000000000000, 1.000000000000000000, 0.9999999999999997780, 1.000000000000000222, 1.000000000000000000, 0.9999999999999997780, 1.000000000000000000, 1.000000000000000000, 1.000000000000000222, 1.000000000000000222, 1.000000000000000000, 1.000000000000000222, 1.000000000000000000, 1.000000000000000000, 1.000000000000000000),
 ( 0.3333333333333334259, 0.3333333333333334259, 0.3333333333333334259, 0.3333333333333333703, 0.3333333333333333148, 0.3333333333333333703, 0.3333333333333334259, 0.3333333333333333703, 0.3333333333333333703, 0.3333333333333334259, 0.3333333333333332593, 0.3333333333333334259, 0.3333333333333333703, 0.3333333333333333703, 0.3333333333333333703, 0.3333333333333333703, 0.3333333333333333703, 0.3333333333333333148, 0.3333333333333334259, 0.3333333333333333148, 0.3333333333333334259, 0.3333333333333333148, 0.3333333333333333703, 0.3333333333333333703, 0.3333333333333333148, 0.3333333333333334814, 0.3333333333333332593, 0.3333333333333334814, 0.3333333333333333148, 0.3333333333333333148, 0.3333333333333334259, 0.3333333333333333703, 0.3333333333333334814, 0.3333333333333332593, 0.3333333333333334259, 0.3333333333333333703, 0.3333333333333333703, 0.3333333333333333148, 0.3333333333333333703, 0.3333333333333333703, 0.3333333333333334814, 0.3333333333333333703, 0.3333333333333334259, 0.3333333333333333703, 0.3333333333333333148, 0.3333333333333333148, 0.3333333333333333703, 0.3333333333333334259, 0.3333333333333333703, 0.3333333333333333703, 0.3333333333333333148, 0.3333333333333333703, 0.3333333333333332593, 0.3333333333333334259, 0.3333333333333333148, 0.3333333333333333703, 0.3333333333333333703, 0.3333333333333333703, 0.3333333333333333703, 0.3333333333333335369, 0.3333333333333332593, 0.3333333333333334259, 0.3333333333333333703, 0.3333333333333334259, 0.3333333333333334259, 0.3333333333333333148, 0.3333333333333334259, 0.3333333333333334259, 0.3333333333333334259, 0.3333333333333334814, 0.3333333333333333703, 0.3333333333333333148, 0.3333333333333333148, 0.3333333333333333703, 0.3333333333333334259, 0.3333333333333333703, 0.3333333333333333703, 0.3333333333333333703, 0.3333333333333333703, 0.3333333333333333148, 0.3333333333333333703, 0.3333333333333332593, 0.3333333333333333703, 0.3333333333333333148, 0.3333333333333333148, 0.3333333333333333703, 0.3333333333333333703, 0.3333333333333333148, 0.3333333333333333703, 0.3333333333333333703, 0.3333333333333333703, 0.3333333333333333703, 0.3333333333333334259, 0.3333333333333332593, 0.3333333333333334259, 0.3333333333333333148, 0.3333333333333333703, 0.3333333333333333148, 0.3333333333333334814, 0.3333333333333332038, 0.3333333333333335369, 0.3333333333333332593, 0.3333333333333333703, 0.3333333333333333703, 0.3333333333333333148, 0.3333333333333333703, 0.3333333333333333148, 0.3333333333333334259, 0.3333333333333334259, 0.3333333333333332593, 0.3333333333333334814, 0.3333333333333333703, 0.3333333333333332593, 0.3333333333333334814, 0.3333333333333334259, 0.3333333333333334259, 0.3333333333333332593, 0.3333333333333333703, 0.3333333333333333703, 0.3333333333333334259, 0.3333333333333333703, 0.3333333333333334259, 0.3333333333333333703, 0.3333333333333333148, 0.3333333333333334814, 0.3333333333333333703, 0.3333333333333334259, 0.3333333333333333703, 0.3333333333333333703, 0.3333333333333333148, 0.3333333333333334259, 0.3333333333333334259, 0.3333333333333333703, 0.3333333333333333148, 0.3333333333333333148, 0.3333333333333334259, 0.3333333333333334814, 0.3333333333333333148, 0.3333333333333334259, 0.3333333333333334814, 0.3333333333333333148, 0.3333333333333334814, 0.3333333333333332038, 0.3333333333333333703, 0.3333333333333333148, 0.3333333333333333703, 0.3333333333333334259, 0.3333333333333332038, 0.3333333333333334259, 0.3333333333333333148, 0.3333333333333332038, 0.3333333333333334259, 0.3333333333333333148, 0.3333333333333334259, 0.3333333333333332593, 0.3333333333333334259, 0.3333333333333333703, 0.3333333333333334259, 0.3333333333333333703, 0.3333333333333334259, 0.3333333333333333703, 0.3333333333333333703, 0.3333333333333334814, 0.3333333333333333703, 0.3333333333333335369, 0.3333333333333332038, 0.3333333333333333703, 0.3333333333333333703, 0.3333333333333333703, 0.3333333333333333148, 0.3333333333333333703, 0.3333333333333333703, 0.3333333333333334259, 0.3333333333333333148, 0.3333333333333334259, 0.3333333333333333148, 0.3333333333333334814, 0.3333333333333332593, 0.3333333333333333703, 0.3333333333333334259, 0.3333333333333333148, 0.3333333333333333703, 0.3333333333333333148, 0.3333333333333334259, 0.3333333333333332593, 0.3333333333333333703, 0.3333333333333334814, 0.3333333333333333703, 0.3333333333333333703, 0.3333333333333333703, 0.3333333333333333703, 0.3333333333333333148, 0.3333333333333333703, 0.3333333333333333703, 0.3333333333333334259, 0.3333333333333333703, 0.3333333333333333703, 0.3333333333333333703, 0.3333333333333333703, 0.3333333333333332038, 0.3333333333333334814, 0.3333333333333333703, 0.3333333333333333703, 0.3333333333333333148, 0.3333333333333333148, 0.3333333333333334259, 0.3333333333333334259, 0.3333333333333332593, 0.3333333333333335369, 0.3333333333333332593, 0.3333333333333334814, 0.3333333333333332593, 0.3333333333333334259, 0.3333333333333332038, 0.3333333333333335369, 0.3333333333333333148, 0.3333333333333333703, 0.3333333333333334259, 0.3333333333333333148, 0.3333333333333333148, 0.3333333333333335369, 0.3333333333333334259, 0.3333333333333333703, 0.3333333333333333148, 0.3333333333333334259, 0.3333333333333333148, 0.3333333333333334259, 0.3333333333333334259, 0.3333333333333333703, 0.3333333333333333703, 0.3333333333333333148, 0.3333333333333333703, 0.3333333333333333703, 0.3333333333333334259, 0.3333333333333333703, 0.3333333333333335369, 0.3333333333333333148, 0.3333333333333333703, 0.3333333333333332593, 0.3333333333333335369, 0.3333333333333333148, 0.3333333333333333148, 0.3333333333333334814, 0.3333333333333332593, 0.3333333333333334814, 0.3333333333333333703, 0.3333333333333334259, 0.3333333333333334814, 0.3333333333333333703, 0.3333333333333333703, 0.3333333333333333148, 0.3333333333333332593, 0.3333333333333334814, 0.3333333333333333148, 0.3333333333333333703, 0.3333333333333333703, 0.3333333333333333703, 0.3333333333333333703, 0.3333333333333334259, 0.3333333333333333703, 0.3333333333333333703, 0.3333333333333333148, 0.3333333333333333703, 0.3333333333333334259, 0.3333333333333332593, 0.3333333333333334814, 0.3333333333333333703, 0.3333333333333333703, 0.3333333333333334259, 0.3333333333333333703, 0.3333333333333334259, 0.3333333333333333703, 0.3333333333333334259, 0.3333333333333332593, 0.3333333333333333703, 0.3333333333333334259, 0.3333333333333333148, 0.3333333333333333148, 0.3333333333333333703, 0.3333333333333334814, 0.3333333333333333148, 0.3333333333333333703, 0.3333333333333334259, 0.3333333333333333703, 0.3333333333333333703, 0.3333333333333333148, 0.3333333333333333703, 0.3333333333333333148, 0.3333333333333335369, 0.3333333333333332593, 0.3333333333333333703, 0.3333333333333333148, 0.3333333333333333703, 0.3333333333333334259, 0.3333333333333334259, 0.3333333333333333703, 0.3333333333333333148, 0.3333333333333334259, 0.3333333333333334259, 0.3333333333333333148, 0.3333333333333334259, 0.3333333333333335369, 0.3333333333333332593, 0.3333333333333333703, 0.3333333333333335369, 0.3333333333333332038, 0.3333333333333334259, 0.3333333333333333148, 0.3333333333333333703, 0.3333333333333333703, 0.3333333333333333703, 0.3333333333333333148, 0.3333333333333333703, 0.3333333333333333703, 0.3333333333333334259, 0.3333333333333334259, 0.3333333333333333148, 0.3333333333333334259, 0.3333333333333333148, 0.3333333333333333703, 0.3333333333333333148, 0.3333333333333334259, 0.3333333333333332038, 0.3333333333333333703, 0.3333333333333334259, 0.3333333333333335369, 0.3333333333333333148, 0.3333333333333333703, 0.3333333333333333703, 0.3333333333333333703, 0.3333333333333333703, 0.3333333333333333703, 0.3333333333333333703, 0.3333333333333334259, 0.3333333333333333703, 0.3333333333333333703, 0.3333333333333333703, 0.3333333333333332038, 0.3333333333333333703, 0.3333333333333335369, 0.3333333333333333148, 0.3333333333333334814, 0.3333333333333333703, 0.3333333333333332593, 0.3333333333333335369, 0.3333333333333333148, 0.3333333333333333703, 0.3333333333333333703, 0.3333333333333333148, 0.3333333333333333703, 0.3333333333333334259, 0.3333333333333334259, 0.3333333333333333703, 0.3333333333333334259, 0.3333333333333333148, 0.3333333333333333703, 0.3333333333333332593, 0.3333333333333333703, 0.3333333333333333703, 0.3333333333333333703, 0.3333333333333333703, 0.3333333333333333703, 0.3333333333333333703, 0.3333333333333333148, 0.3333333333333334259, 0.3333333333333333703, 0.3333333333333334259, 0.3333333333333333148, 0.3333333333333334259, 0.3333333333333333148, 0.3333333333333333703, 0.3333333333333334259, 0.3333333333333333703, 0.3333333333333333148, 0.3333333333333333148, 0.3333333333333334259, 0.3333333333333333703, 0.3333333333333333703, 0.3333333333333334259, 0.3333333333333333703, 0.3333333333333333148, 0.3333333333333334814, 0.3333333333333333703, 0.3333333333333334259, 0.3333333333333333703, 0.3333333333333333703, 0.3333333333333333703),
 ( 0.3333333333333334259, 0.3333333333333334259, 0.3333333333333334259, 0.3333333333333333703, 0.3333333333333333148, 0.3333333333333333703, 0.3333333333333334259, 0.3333333333333333703, 0.3333333333333333703, 0.3333333333333334259, 0.3333333333333332593, 0.3333333333333334259, 0.3333333333333333703, 0.3333333333333333703, 0.3333333333333333703, 0.3333333333333333703, 0.3333333333333333703, 0.3333333333333333148, 0.3333333333333334259, 0.3333333333333333148, 0.3333333333333334259, 0.3333333333333333148, 0.3333333333333333703, 0.3333333333333333703, 0.3333333333333333148, 0.3333333333333334814, 0.3333333333333332593, 0.3333333333333334814, 0.3333333333333333148, 0.3333333333333333148, 0.3333333333333334259, 0.3333333333333333703, 0.3333333333333334814, 0.3333333333333332593, 0.3333333333333334259, 0.3333333333333333703, 0.3333333333333333703, 0.3333333333333333148, 0.3333333333333333703, 0.3333333333333333703, 0.3333333333333334814, 0.3333333333333333703, 0.3333333333333334259, 0.3333333333333333703, 0.3333333333333333148, 0.3333333333333333148, 0.3333333333333333703, 0.3333333333333334259, 0.3333333333333333703, 0.3333333333333333703, 0.3333333333333333148, 0.3333333333333333703, 0.3333333333333332593, 0.3333333333333334259, 0.3333333333333333148, 0.3333333333333333703, 0.3333333333333333703, 0.3333333333333333703, 0.3333333333333333703, 0.3333333333333335369, 0.3333333333333332593, 0.3333333333333334259, 0.3333333333333333703, 0.3333333333333334259, 0.3333333333333334259, 0.3333333333333333148, 0.3333333333333334259, 0.3333333333333334259, 0.3333333333333334259, 0.3333333333333334814, 0.3333333333333333703, 0.3333333333333333148, 0.3333333333333333148, 0.3333333333333333703, 0.3333333333333334259, 0.3333333333333333703, 0.3333333333333333703, 0.3333333333333333703, 0.3333333333333333703, 0.3333333333333333148, 0.3333333333333333703, 0.3333333333333332593, 0.3333333333333333703, 0.3333333333333333148, 0.3333333333333333148, 0.3333333333333333703, 0.3333333333333333703, 0.3333333333333333148, 0.3333333333333333703, 0.3333333333333333703, 0.3333333333333333703, 0.3333333333333333703, 0.3333333333333334259, 0.3333333333333332593, 0.3333333333333334259, 0.3333333333333333148, 0.3333333333333333703, 0.3333333333333333148, 0.3333333333333334814, 0.3333333333333332038, 0.3333333333333335369, 0.3333333333333332593, 0.3333333333333333703, 0.3333333333333333703, 0.3333333333333333148, 0.3333333333333333703, 0.3333333333333333148, 0.3333333333333334259, 0.3333333333333334259, 0.3333333333333332593, 0.3333333333333334814, 0.3333333333333333703, 0.3333333333333332593, 0.3333333333333334814, 0.3333333333333334259, 0.3333333333333334259, 0.3333333333333332593, 0.3333333333333333703, 0.3333333333333333703, 0.3333333333333334259, 0.3333333333333333703, 0.3333333333333334259, 0.3333333333333333703, 0.3333333333333333148, 0.3333333333333334814, 0.3333333333333333703, 0.3333333333333334259, 0.3333333333333333703, 0.3333333333333333703, 0.3333333333333333148, 0.3333333333333334259, 0.3333333333333334259, 0.3333333333333333703, 0.3333333333333333148, 0.3333333333333333148, 0.3333333333333334259, 0.3333333333333334814, 0.3333333333333333148, 0.3333333333333334259, 0.3333333333333334814, 0.3333333333333333148, 0.3333333333333334814, 0.3333333333333332038, 0.3333333333333333703, 0.3333333333333333148, 0.3333333333333333703, 0.3333333333333334259, 0.3333333333333332038, 0.3333333333333334259, 0.3333333333333333148, 0.3333333333333332038, 0.3333333333333334259, 0.3333333333333333148, 0.3333333333333334259, 0.3333333333333332593, 0.3333333333333334259, 0.3333333333333333703, 0.3333333333333334259, 0.3333333333333333703, 0.3333333333333334259, 0.3333333333333333703, 0.3333333333333333703, 0.3333333333333334814, 0.3333333333333333703, 0.3333333333333335369, 0.3333333333333332038, 0.3333333333333333703, 0.3333333333333333703, 0.3333333333333333703, 0.3333333333333333148, 0.3333333333333333703, 0.3333333333333333703, 0.3333333333333334259, 0.3333333333333333148, 0.3333333333333334259, 0.3333333333333333148, 0.3333333333333334814, 0.3333333333333332593, 0.3333333333333333703, 0.3333333333333334259, 0.3333333333333333148, 0.3333333333333333703, 0.3333333333333333148, 0.3333333333333334259, 0.3333333333333332593, 0.3333333333333333703, 0.3333333333333334814, 0.3333333333333333703, 0.3333333333333333703, 0.3333333333333333703, 0.3333333333333333703, 0.3333333333333333148, 0.3333333333333333703, 0.3333333333333333703, 0.3333333333333334259, 0.3333333333333333703, 0.3333333333333333703, 0.3333333333333333703, 0.3333333333333333703, 0.3333333333333332038, 0.3333333333333334814, 0.3333333333333333703, 0.3333333333333333703, 0.3333333333333333148, 0.3333333333333333148, 0.3333333333333334259, 0.3333333333333334259, 0.3333333333333332593, 0.3333333333333335369, 0.3333333333333332593, 0.3333333333333334814, 0.3333333333333332593, 0.3333333333333334259, 0.3333333333333332038, 0.3333333333333335369, 0.3333333333333333148, 0.3333333333333333703, 0.3333333333333334259, 0.3333333333333333148, 0.3333333333333333148, 0.3333333333333335369, 0.3333333333333334259, 0.3333333333333333703, 0.3333333333333333148, 0.3333333333333334259, 0.3333333333333333148, 0.3333333333333334259, 0.3333333333333334259, 0.3333333333333333703, 0.3333333333333333703, 0.3333333333333333148, 0.3333333333333333703, 0.3333333333333333703, 0.3333333333333334259, 0.3333333333333333703, 0.3333333333333335369, 0.3333333333333333148, 0.3333333333333333703, 0.3333333333333332593, 0.3333333333333335369, 0.3333333333333333148, 0.3333333333333333148, 0.3333333333333334814, 0.3333333333333332593, 0.3333333333333334814, 0.3333333333333333703, 0.3333333333333334259, 0.3333333333333334814, 0.3333333333333333703, 0.3333333333333333703, 0.3333333333333333148, 0.3333333333333332593, 0.3333333333333334814, 0.3333333333333333148, 0.3333333333333333703, 0.3333333333333333703, 0.3333333333333333703, 0.3333333333333333703, 0.3333333333333334259, 0.3333333333333333703, 0.3333333333333333703, 0.3333333333333333148, 0.3333333333333333703, 0.3333333333333334259, 0.3333333333333332593, 0.3333333333333334814, 0.3333333333333333703, 0.3333333333333333703, 0.3333333333333334259, 0.3333333333333333703, 0.3333333333333334259, 0.3333333333333333703, 0.3333333333333334259, 0.3333333333333332593, 0.3333333333333333703, 0.3333333333333334259, 0.3333333333333333148, 0.3333333333333333148, 0.3333333333333333703, 0.3333333333333334814, 0.3333333333333333148, 0.3333333333333333703, 0.3333333333333334259, 0.3333333333333333703, 0.3333333333333333703, 0.3333333333333333148, 0.3333333333333333703, 0.3333333333333333148, 0.3333333333333335369, 0.3333333333333332593, 0.3333333333333333703, 0.3333333333333333148, 0.3333333333333333703, 0.3333333333333334259, 0.3333333333333334259, 0.3333333333333333703, 0.3333333333333333148, 0.3333333333333334259, 0.3333333333333334259, 0.3333333333333333148, 0.3333333333333334259, 0.3333333333333335369, 0.3333333333333332593, 0.3333333333333333703, 0.3333333333333335369, 0.3333333333333332038, 0.3333333333333334259, 0.3333333333333333148, 0.3333333333333333703, 0.3333333333333333703, 0.3333333333333333703, 0.3333333333333333148, 0.3333333333333333703, 0.3333333333333333703, 0.3333333333333334259, 0.3333333333333334259, 0.3333333333333333148, 0.3333333333333334259, 0.3333333333333333148, 0.3333333333333333703, 0.3333333333333333148, 0.3333333333333334259, 0.3333333333333332038, 0.3333333333333333703, 0.3333333333333334259, 0.3333333333333335369, 0.3333333333333333148, 0.3333333333333333703, 0.3333333333333333703, 0.3333333333333333703, 0.3333333333333333703, 0.3333333333333333703, 0.3333333333333333703, 0.3333333333333334259, 0.3333333333333333703, 0.3333333333333333703, 0.3333333333333333703, 0.3333333333333332038, 0.3333333333333333703, 0.3333333333333335369, 0.3333333333333333148, 0.3333333333333334814, 0.3333333333333333703, 0.3333333333333332593, 0.3333333333333335369, 0.3333333333333333148, 0.3333333333333333703, 0.3333333333333333703, 0.3333333333333333148, 0.3333333333333333703, 0.3333333333333334259, 0.3333333333333334259, 0.3333333333333333703, 0.3333333333333334259, 0.3333333333333333148, 0.3333333333333333703, 0.3333333333333332593, 0.3333333333333333703, 0.3333333333333333703, 0.3333333333333333703, 0.3333333333333333703, 0.3333333333333333703, 0.3333333333333333703, 0.3333333333333333148, 0.3333333333333334259, 0.3333333333333333703, 0.3333333333333334259, 0.3333333333333333148, 0.3333333333333334259, 0.3333333333333333148, 0.3333333333333333703, 0.3333333333333334259, 0.3333333333333333703, 0.3333333333333333148, 0.3333333333333333148, 0.3333333333333334259, 0.3333333333333333703, 0.3333333333333333703, 0.3333333333333334259, 0.3333333333333333703, 0.3333333333333333148, 0.3333333333333334814, 0.3333333333333333703, 0.3333333333333334259, 0.3333333333333333703, 0.3333333333333333703, 0.3333333333333333703),
 ( 1.000000000000000222, 1.000000000000000222, 1.000000000000000222, 1.000000000000000222, 0.9999999999999996669, 0.9999999999999997780, 1.000000000000000444, 1.000000000000000000, 1.000000000000000000, 1.000000000000000000, 0.9999999999999997780, 1.000000000000000000, 1.000000000000000000, 1.000000000000000000, 1.000000000000000000, 0.9999999999999997780, 1.000000000000000222, 0.9999999999999996669, 1.000000000000000000, 0.9999999999999997780, 1.000000000000000222, 1.000000000000000000, 1.000000000000000222, 0.9999999999999996669, 1.000000000000000000, 1.000000000000000222, 0.9999999999999996669, 1.000000000000000444, 1.000000000000000000, 0.9999999999999997780, 1.000000000000000222, 1.000000000000000222, 1.000000000000000222, 1.000000000000000000, 1.000000000000000000, 0.9999999999999997780, 1.000000000000000000, 1.000000000000000000, 1.000000000000000000, 1.000000000000000000, 1.000000000000000222, 1.000000000000000222, 1.000000000000000000, 1.000000000000000000, 1.000000000000000000, 0.9999999999999996669, 1.000000000000000222, 1.000000000000000000, 1.000000000000000000, 0.9999999999999997780, 0.9999999999999997780, 1.000000000000000000, 0.9999999999999996669, 1.000000000000000222, 0.9999999999999997780, 1.000000000000000222, 0.9999999999999997780, 0.9999999999999997780, 1.000000000000000222, 1.000000000000000222, 0.9999999999999997780, 1.000000000000000222, 1.000000000000000000, 1.000000000000000222, 1.000000000000000000, 0.9999999999999997780, 1.000000000000000000, 1.000000000000000000, 1.000000000000000222, 1.000000000000000222, 1.000000000000000000, 0.9999999999999997780, 1.000000000000000000, 1.000000000000000222, 0.9999999999999997780, 1.000000000000000444, 0.9999999999999996669, 1.000000000000000000, 1.000000000000000222, 0.9999999999999997780, 0.9999999999999997780, 0.9999999999999997780, 1.000000000000000000, 0.9999999999999997780, 1.000000000000000000, 0.9999999999999997780, 1.000000000000000222, 1.000000000000000000, 1.000000000000000222, 1.000000000000000000, 0.9999999999999997780, 1.000000000000000000, 1.000000000000000000, 0.9999999999999997780, 1.000000000000000222, 1.000000000000000000, 1.000000000000000000, 1.000000000000000000, 1.000000000000000222, 0.9999999999999996669, 1.000000000000000222, 1.000000000000000000, 1.000000000000000000, 0.9999999999999997780, 1.000000000000000000, 0.9999999999999997780, 1.000000000000000000, 1.000000000000000222, 1.000000000000000000, 0.9999999999999997780, 1.000000000000000222, 1.000000000000000222, 0.9999999999999996669, 1.000000000000000222, 1.000000000000000000, 1.000000000000000444, 0.9999999999999996669, 1.000000000000000000, 1.000000000000000222, 1.000000000000000222, 1.000000000000000222, 1.000000000000000222, 1.000000000000000000, 0.9999999999999997780, 1.000000000000000222, 1.000000000000000000, 1.000000000000000222, 0.9999999999999996669, 1.000000000000000000, 1.000000000000000000, 1.000000000000000222, 1.000000000000000222, 0.9999999999999997780, 1.000000000000000000, 0.9999999999999997780, 1.000000000000000222, 1.000000000000000000, 1.000000000000000222, 1.000000000000000000, 1.000000000000000444, 0.9999999999999996669, 1.000000000000000444, 0.9999999999999996669, 0.9999999999999997780, 0.9999999999999997780, 1.000000000000000222, 1.000000000000000000, 0.9999999999999997780, 1.000000000000000000, 0.9999999999999997780, 0.9999999999999996669, 1.000000000000000222, 1.000000000000000000, 0.9999999999999997780, 1.000000000000000000, 1.000000000000000000, 1.000000000000000222, 1.000000000000000000, 1.000000000000000000, 1.000000000000000444, 0.9999999999999997780, 1.000000000000000222, 1.000000000000000222, 0.9999999999999997780, 1.000000000000000444, 0.9999999999999996669, 1.000000000000000000, 0.9999999999999997780, 1.000000000000000222, 0.9999999999999997780, 1.000000000000000222, 1.000000000000000000, 1.000000000000000222, 0.9999999999999997780, 0.9999999999999997780, 1.000000000000000000, 1.000000000000000000, 0.9999999999999997780, 1.000000000000000222, 0.9999999999999997780, 1.000000000000000000, 1.000000000000000000, 1.000000000000000222, 1.000000000000000000, 0.9999999999999997780, 1.000000000000000222, 1.000000000000000444, 1.000000000000000000, 1.000000000000000000, 1.000000000000000000, 1.000000000000000000, 0.9999999999999997780, 1.000000000000000000, 1.000000000000000222, 1.000000000000000000, 1.000000000000000222, 0.9999999999999996669, 1.000000000000000000, 1.000000000000000000, 0.9999999999999994449, 1.000000000000000444, 1.000000000000000000, 1.000000000000000222, 0.9999999999999997780, 1.000000000000000000, 1.000000000000000222, 1.000000000000000000, 0.9999999999999996669, 1.000000000000000444, 0.9999999999999997780, 1.000000000000000444, 0.9999999999999996669, 1.000000000000000000, 0.9999999999999996669, 1.000000000000000444, 1.000000000000000000, 0.9999999999999997780, 1.000000000000000222, 1.000000000000000000, 0.9999999999999997780, 1.000000000000000444, 1.000000000000000222, 0.9999999999999997780, 1.000000000000000000, 1.000000000000000222, 0.9999999999999997780, 1.000000000000000222, 1.000000000000000222, 1.000000000000000000, 1.000000000000000000, 0.9999999999999996669, 1.000000000000000222, 0.9999999999999997780, 1.000000000000000000, 0.9999999999999997780, 1.000000000000000444, 1.000000000000000000, 1.000000000000000000, 0.9999999999999997780, 1.000000000000000444, 1.000000000000000000, 0.9999999999999997780, 1.000000000000000444, 0.9999999999999996669, 1.000000000000000444, 1.000000000000000000, 1.000000000000000444, 1.000000000000000222, 1.000000000000000222, 0.9999999999999997780, 1.000000000000000000, 0.9999999999999997780, 1.000000000000000444, 0.9999999999999996669, 1.000000000000000000, 1.000000000000000000, 1.000000000000000222, 1.000000000000000000, 1.000000000000000222, 1.000000000000000000, 1.000000000000000000, 0.9999999999999997780, 1.000000000000000000, 1.000000000000000000, 0.9999999999999997780, 1.000000000000000000, 1.000000000000000000, 0.9999999999999997780, 1.000000000000000000, 1.000000000000000222, 1.000000000000000000, 1.000000000000000000, 1.000000000000000000, 1.000000000000000000, 0.9999999999999996669, 1.000000000000000222, 1.000000000000000000, 0.9999999999999997780, 1.000000000000000000, 1.000000000000000222, 1.000000000000000000, 1.000000000000000222, 1.000000000000000222, 1.000000000000000000, 1.000000000000000222, 1.000000000000000000, 1.000000000000000000, 1.000000000000000000, 1.000000000000000222, 0.9999999999999996669, 1.000000000000000222, 0.9999999999999996669, 1.000000000000000222, 1.000000000000000222, 1.000000000000000222, 1.000000000000000222, 0.9999999999999996669, 1.000000000000000444, 1.000000000000000000, 1.000000000000000000, 1.000000000000000222, 1.000000000000000444, 0.9999999999999996669, 1.000000000000000444, 1.000000000000000222, 0.9999999999999996669, 1.000000000000000222, 0.9999999999999997780, 1.000000000000000000, 1.000000000000000000, 0.9999999999999997780, 1.000000000000000000, 0.9999999999999997780, 1.000000000000000000, 1.000000000000000000, 1.000000000000000444, 0.9999999999999997780, 1.000000000000000222, 0.9999999999999997780, 0.9999999999999997780, 1.000000000000000000, 1.000000000000000000, 0.9999999999999996669, 1.000000000000000000, 1.000000000000000222, 1.000000000000000222, 0.9999999999999997780, 1.000000000000000222, 0.9999999999999997780, 0.9999999999999997780, 1.000000000000000000, 1.000000000000000000, 1.000000000000000000, 1.000000000000000222, 1.000000000000000000, 1.000000000000000222, 1.000000000000000000, 0.9999999999999996669, 0.9999999999999997780, 1.000000000000000444, 0.9999999999999996669, 1.000000000000000444, 0.9999999999999997780, 0.9999999999999997780, 1.000000000000000222, 0.9999999999999997780, 1.000000000000000222, 1.000000000000000000, 1.000000000000000000, 0.9999999999999997780, 1.000000000000000222, 1.000000000000000222, 1.000000000000000000, 1.000000000000000222, 1.000000000000000000, 1.000000000000000000, 0.9999999999999997780, 1.000000000000000000, 1.000000000000000000, 0.9999999999999997780, 1.000000000000000000, 0.9999999999999996669, 1.000000000000000222, 0.9999999999999997780, 1.000000000000000222, 0.9999999999999997780, 1.000000000000000000, 0.9999999999999997780, 1.000000000000000222, 0.9999999999999997780, 1.000000000000000000, 1.000000000000000000, 1.000000000000000000, 1.000000000000000000, 0.9999999999999997780, 1.000000000000000222, 1.000000000000000000, 0.9999999999999997780, 1.000000000000000000, 1.000000000000000000, 1.000000000000000222, 1.000000000000000222, 1.000000000000000000, 1.000000000000000222, 1.000000000000000000, 1.000000000000000000, 1.000000000000000000),
 ( 0.3333333333333334259, 0.3333333333333334259, 0.3333333333333334259, 0.3333333333333333703, 0.3333333333333333148, 0.3333333333333333703, 0.3333333333333334259, 0.3333333333333333703, 0.3333333333333333703, 0.3333333333333334259, 0.3333333333333332593, 0.3333333333333334259, 0.3333333333333333703, 0.3333333333333333703, 0.3333333333333333703, 0.3333333333333333703, 0.3333333333333333703, 0.3333333333333333148, 0.3333333333333334259, 0.3333333333333333148, 0.3333333333333334259, 0.3333333333333333148, 0.3333333333333333703, 0.3333333333333333703, 0.3333333333333333148, 0.3333333333333334814, 0.3333333333333332593, 0.3333333333333334814, 0.3333333333333333148, 0.3333333333333333148, 0.3333333333333334259, 0.3333333333333333703, 0.3333333333333334814, 0.3333333333333332593, 0.3333333333333334259, 0.3333333333333333703, 0.3333333333333333703, 0.3333333333333333148, 0.3333333333333333703, 0.3333333333333333703, 0.3333333333333334814, 0.3333333333333333703, 0.3333333333333334259, 0.3333333333333333703, 0.3333333333333333148, 0.3333333333333333148, 0.3333333333333333703, 0.3333333333333334259, 0.3333333333333333703, 0.3333333333333333703, 0.3333333333333333148, 0.3333333333333333703, 0.3333333333333332593, 0.3333333333333334259, 0.3333333333333333148, 0.3333333333333333703, 0.3333333333333333703, 0.3333333333333333703, 0.3333333333333333703, 0.3333333333333335369, 0.3333333333333332593, 0.3333333333333334259, 0.3333333333333333703, 0.3333333333333334259, 0.3333333333333334259, 0.3333333333333333148, 0.3333333333333334259, 0.3333333333333334259, 0.3333333333333334259, 0.3333333333333334814, 0.3333333333333333703, 0.3333333333333333148, 0.3333333333333333148, 0.3333333333333333703, 0.3333333333333334259, 0.3333333333333333703, 0.3333333333333333703, 0.3333333333333333703, 0.3333333333333333703, 0.3333333333333333148, 0.3333333333333333703, 0.3333333333333332593, 0.3333333333333333703, 0.3333333333333333148, 0.3333333333333333148, 0.3333333333333333703, 0.3333333333333333703, 0.3333333333333333148, 0.3333333333333333703, 0.3333333333333333703, 0.3333333333333333703, 0.3333333333333333703, 0.3333333333333334259, 0.3333333333333332593, 0.3333333333333334259, 0.3333333333333333148, 0.3333333333333333703, 0.3333333333333333148, 0.3333333333333334814, 0.3333333333333332038, 0.3333333333333335369, 0.3333333333333332593, 0.3333333333333333703, 0.3333333333333333703, 0.3333333333333333148, 0.3333333333333333703, 0.3333333333333333148, 0.3333333333333334259, 0.3333333333333334259, 0.3333333333333332593, 0.3333333333333334814, 0.3333333333333333703, 0.3333333333333332593, 0.3333333333333334814, 0.3333333333333334259, 0.3333333333333334259, 0.3333333333333332593, 0.3333333333333333703, 0.3333333333333333703, 0.3333333333333334259, 0.3333333333333333703, 0.3333333333333334259, 0.3333333333333333703, 0.3333333333333333148, 0.3333333333333334814, 0.3333333333333333703, 0.3333333333333334259, 0.3333333333333333703, 0.3333333333333333703, 0.3333333333333333148, 0.3333333333333334259, 0.3333333333333334259, 0.3333333333333333703, 0.3333333333333333148, 0.3333333333333333148, 0.3333333333333334259, 0.3333333333333334814, 0.3333333333333333148, 0.3333333333333334259, 0.3333333333333334814, 0.3333333333333333148, 0.3333333333333334814, 0.3333333333333332038, 0.3333333333333333703, 0.3333333333333333148, 0.3333333333333333703, 0.3333333333333334259, 0.3333333333333332038, 0.3333333333333334259, 0.3333333333333333148, 0.3333333333333332038, 0.3333333333333334259, 0.3333333333333333148, 0.3333333333333334259, 0.3333333333333332593, 0.3333333333333334259, 0.3333333333333333703, 0.3333333333333334259, 0.3333333333333333703, 0.3333333333333334259, 0.3333333333333333703, 0.3333333333333333703, 0.3333333333333334814, 0.3333333333333333703, 0.3333333333333335369, 0.3333333333333332038, 0.3333333333333333703, 0.3333333333333333703, 0.3333333333333333703, 0.3333333333333333148, 0.3333333333333333703, 0.3333333333333333703, 0.3333333333333334259, 0.3333333333333333148, 0.3333333333333334259, 0.3333333333333333148, 0.3333333333333334814, 0.3333333333333332593, 0.3333333333333333703, 0.3333333333333334259, 0.3333333333333333148, 0.3333333333333333703, 0.3333333333333333148, 0.3333333333333334259, 0.3333333333333332593, 0.3333333333333333703, 0.3333333333333334814, 0.3333333333333333703, 0.3333333333333333703, 0.3333333333333333703, 0.3333333333333333703, 0.3333333333333333148, 0.3333333333333333703, 0.3333333333333333703, 0.3333333333333334259, 0.3333333333333333703, 0.3333333333333333703, 0.3333333333333333703, 0.3333333333333333703, 0.3333333333333332038, 0.3333333333333334814, 0.3333333333333333703, 0.3333333333333333703, 0.3333333333333333148, 0.3333333333333333148, 0.3333333333333334259, 0.3333333333333334259, 0.3333333333333332593, 0.3333333333333335369, 0.3333333333333332593, 0.3333333333333334814, 0.3333333333333332593, 0.3333333333333334259, 0.3333333333333332038, 0.3333333333333335369, 0.3333333333333333148, 0.3333333333333333703, 0.3333333333333334259, 0.3333333333333333148, 0.3333333333333333148, 0.3333333333333335369, 0.3333333333333334259, 0.3333333333333333703, 0.3333333333333333148, 0.3333333333333334259, 0.3333333333333333148, 0.3333333333333334259, 0.3333333333333334259, 0.3333333333333333703, 0.3333333333333333703, 0.3333333333333333148, 0.3333333333333333703, 0.3333333333333333703, 0.3333333333333334259, 0.3333333333333333703, 0.3333333333333335369, 0.3333333333333333148, 0.3333333333333333703, 0.3333333333333332593, 0.3333333333333335369, 0.3333333333333333148, 0.3333333333333333148, 0.3333333333333334814, 0.3333333333333332593, 0.3333333333333334814, 0.3333333333333333703, 0.3333333333333334259, 0.3333333333333334814, 0.3333333333333333703, 0.3333333333333333703, 0.3333333333333333148, 0.3333333333333332593, 0.3333333333333334814, 0.3333333333333333148, 0.3333333333333333703, 0.3333333333333333703, 0.3333333333333333703, 0.3333333333333333703, 0.3333333333333334259, 0.3333333333333333703, 0.3333333333333333703, 0.3333333333333333148, 0.3333333333333333703, 0.3333333333333334259, 0.3333333333333332593, 0.3333333333333334814, 0.3333333333333333703, 0.3333333333333333703, 0.3333333333333334259, 0.3333333333333333703, 0.3333333333333334259, 0.3333333333333333703, 0.3333333333333334259, 0.3333333333333332593, 0.3333333333333333703, 0.3333333333333334259, 0.3333333333333333148, 0.3333333333333333148, 0.3333333333333333703, 0.3333333333333334814, 0.3333333333333333148, 0.3333333333333333703, 0.3333333333333334259, 0.3333333333333333703, 0.3333333333333333703, 0.3333333333333333148, 0.3333333333333333703, 0.3333333333333333148, 0.3333333333333335369, 0.3333333333333332593, 0.3333333333333333703, 0.3333333333333333148, 0.3333333333333333703, 0.3333333333333334259, 0.3333333333333334259, 0.3333333333333333703, 0.3333333333333333148, 0.3333333333333334259, 0.3333333333333334259, 0.3333333333333333148, 0.3333333333333334259, 0.3333333333333335369, 0.3333333333333332593, 0.3333333333333333703, 0.3333333333333335369, 0.3333333333333332038, 0.3333333333333334259, 0.3333333333333333148, 0.3333333333333333703, 0.3333333333333333703, 0.3333333333333333703, 0.3333333333333333148, 0.3333333333333333703, 0.3333333333333333703, 0.3333333333333334259, 0.3333333333333334259, 0.3333333333333333148, 0.3333333333333334259, 0.3333333333333333148, 0.3333333333333333703, 0.3333333333333333148, 0.3333333333333334259, 0.3333333333333332038, 0.3333333333333333703, 0.3333333333333334259, 0.3333333333333335369, 0.3333333333333333148, 0.3333333333333333703, 0.3333333333333333703, 0.3333333333333333703, 0.3333333333333333703, 0.3333333333333333703, 0.3333333333333333703, 0.3333333333333334259, 0.3333333333333333703, 0.3333333333333333703, 0.3333333333333333703, 0.3333333333333332038, 0.3333333333333333703, 0.3333333333333335369, 0.3333333333333333148, 0.3333333333333334814, 0.3333333333333333703, 0.3333333333333332593, 0.3333333333333335369, 0.3333333333333333148, 0.3333333333333333703, 0.3333333333333333703, 0.3333333333333333148, 0.3333333333333333703, 0.3333333333333334259, 0.3333333333333334259, 0.3333333333333333703, 0.3333333333333334259, 0.3333333333333333148, 0.3333333333333333703, 0.3333333333333332593, 0.3333333333333333703, 0.3333333333333333703, 0.3333333333333333703, 0.3333333333333333703, 0.3333333333333333703, 0.3333333333333333703, 0.3333333333333333148, 0.3333333333333334259, 0.3333333333333333703, 0.3333333333333334259, 0.3333333333333333148, 0.3333333333333334259, 0.3333333333333333148, 0.3333333333333333703, 0.3333333333333334259, 0.3333333333333333703, 0.3333333333333333148, 0.3333333333333333148, 0.3333333333333334259, 0.3333333333333333703, 0.3333333333333333703, 0.3333333333333334259, 0.3333333333333333703, 0.3333333333333333148, 0.3333333333333334814, 0.3333333333333333703, 0.3333333333333334259, 0.3333333333333333703, 0.3333333333333333703, 0.3333333333333333703),
 ( 0.3333333333333334259, 0.3333333333333334259, 0.3333333333333334259, 0.3333333333333333703, 0.3333333333333333148, 0.3333333333333333703, 0.3333333333333334259, 0.3333333333333333703, 0.3333333333333333703, 0.3333333333333334259, 0.3333333333333332593, 0.3333333333333334259, 0.3333333333333333703, 0.3333333333333333703, 0.3333333333333333703, 0.3333333333333333703, 0.3333333333333333703, 0.3333333333333333148, 0.3333333333333334259, 0.3333333333333333148, 0.3333333333333334259, 0.3333333333333333148, 0.3333333333333333703, 0.3333333333333333703, 0.3333333333333333148, 0.3333333333333334814, 0.3333333333333332593, 0.3333333333333334814, 0.3333333333333333148, 0.3333333333333333148, 0.3333333333333334259, 0.3333333333333333703, 0.3333333333333334814, 0.3333333333333332593, 0.3333333333333334259, 0.3333333333333333703, 0.3333333333333333703, 0.3333333333333333148, 0.3333333333333333703, 0.3333333333333333703, 0.3333333333333334814, 0.3333333333333333703, 0.3333333333333334259, 0.3333333333333333703, 0.3333333333333333148, 0.3333333333333333148, 0.3333333333333333703, 0.3333333333333334259, 0.3333333333333333703, 0.3333333333333333703, 0.3333333333333333148, 0.3333333333333333703, 0.3333333333333332593, 0.3333333333333334259, 0.3333333333333333148, 0.3333333333333333703, 0.3333333333333333703, 0.3333333333333333703, 0.3333333333333333703, 0.3333333333333335369, 0.3333333333333332593, 0.3333333333333334259, 0.3333333333333333703, 0.3333333333333334259, 0.3333333333333334259, 0.3333333333333333148, 0.3333333333333334259, 0.3333333333333334259, 0.3333333333333334259, 0.3333333333333334814, 0.3333333333333333703, 0.3333333333333333148, 0.3333333333333333148, 0.3333333333333333703, 0.3333333333333334259, 0.3333333333333333703, 0.3333333333333333703, 0.3333333333333333703, 0.3333333333333333703, 0.3333333333333333148, 0.3333333333333333703, 0.3333333333333332593, 0.3333333333333333703, 0.3333333333333333148, 0.3333333333333333148, 0.3333333333333333703, 0.3333333333333333703, 0.3333333333333333148, 0.3333333333333333703, 0.3333333333333333703, 0.3333333333333333703, 0.3333333333333333703, 0.3333333333333334259, 0.3333333333333332593, 0.3333333333333334259, 0.3333333333333333148, 0.3333333333333333703, 0.3333333333333333148, 0.3333333333333334814, 0.3333333333333332038, 0.3333333333333335369, 0.3333333333333332593, 0.3333333333333333703, 0.3333333333333333703, 0.3333333333333333148, 0.3333333333333333703, 0.3333333333333333148, 0.3333333333333334259, 0.3333333333333334259, 0.3333333333333332593, 0.3333333333333334814, 0.3333333333333333703, 0.3333333333333332593, 0.3333333333333334814, 0.3333333333333334259, 0.3333333333333334259, 0.3333333333333332593, 0.3333333333333333703, 0.3333333333333333703, 0.3333333333333334259, 0.3333333333333333703, 0.3333333333333334259, 0.3333333333333333703, 0.3333333333333333148, 0.3333333333333334814, 0.3333333333333333703, 0.3333333333333334259, 0.3333333333333333703, 0.3333333333333333703, 0.3333333333333333148, 0.3333333333333334259, 0.3333333333333334259, 0.3333333333333333703, 0.3333333333333333148, 0.3333333333333333148, 0.3333333333333334259, 0.3333333333333334814, 0.3333333333333333148, 0.3333333333333334259, 0.3333333333333334814, 0.3333333333333333148, 0.3333333333333334814, 0.3333333333333332038, 0.3333333333333333703, 0.3333333333333333148, 0.3333333333333333703, 0.3333333333333334259, 0.3333333333333332038, 0.3333333333333334259, 0.3333333333333333148, 0.3333333333333332038, 0.3333333333333334259, 0.3333333333333333148, 0.3333333333333334259, 0.3333333333333332593, 0.3333333333333334259, 0.3333333333333333703, 0.3333333333333334259, 0.3333333333333333703, 0.3333333333333334259, 0.3333333333333333703, 0.3333333333333333703, 0.3333333333333334814, 0.3333333333333333703, 0.3333333333333335369, 0.3333333333333332038, 0.3333333333333333703, 0.3333333333333333703, 0.3333333333333333703, 0.3333333333333333148, 0.3333333333333333703, 0.3333333333333333703, 0.3333333333333334259, 0.3333333333333333148, 0.3333333333333334259, 0.3333333333333333148, 0.3333333333333334814, 0.3333333333333332593, 0.3333333333333333703, 0.3333333333333334259, 0.3333333333333333148, 0.3333333333333333703, 0.3333333333333333148, 0.3333333333333334259, 0.3333333333333332593, 0.3333333333333333703, 0.3333333333333334814, 0.3333333333333333703, 0.3333333333333333703, 0.3333333333333333703, 0.3333333333333333703, 0.3333333333333333148, 0.3333333333333333703, 0.3333333333333333703, 0.3333333333333334259, 0.3333333333333333703, 0.3333333333333333703, 0.3333333333333333703, 0.3333333333333333703, 0.3333333333333332038, 0.3333333333333334814, 0.3333333333333333703, 0.3333333333333333703, 0.3333333333333333148, 0.3333333333333333148, 0.3333333333333334259, 0.3333333333333334259, 0.3333333333333332593, 0.3333333333333335369, 0.3333333333333332593, 0.3333333333333334814, 0.3333333333333332593, 0.3333333333333334259, 0.3333333333333332038, 0.3333333333333335369, 0.3333333333333333148, 0.3333333333333333703, 0.3333333333333334259, 0.3333333333333333148, 0.3333333333333333148, 0.3333333333333335369, 0.3333333333333334259, 0.3333333333333333703, 0.3333333333333333148, 0.3333333333333334259, 0.3333333333333333148, 0.3333333333333334259, 0.3333333333333334259, 0.3333333333333333703, 0.3333333333333333703, 0.3333333333333333148, 0.3333333333333333703, 0.3333333333333333703, 0.3333333333333334259, 0.3333333333333333703, 0.3333333333333335369, 0.3333333333333333148, 0.3333333333333333703, 0.3333333333333332593, 0.3333333333333335369, 0.3333333333333333148, 0.3333333333333333148, 0.3333333333333334814, 0.3333333333333332593, 0.3333333333333334814, 0.3333333333333333703, 0.3333333333333334259, 0.3333333333333334814, 0.3333333333333333703, 0.3333333333333333703, 0.3333333333333333148, 0.3333333333333332593, 0.3333333333333334814, 0.3333333333333333148, 0.3333333333333333703, 0.3333333333333333703, 0.3333333333333333703, 0.3333333333333333703, 0.3333333333333334259, 0.3333333333333333703, 0.3333333333333333703, 0.3333333333333333148, 0.3333333333333333703, 0.3333333333333334259, 0.3333333333333332593, 0.3333333333333334814, 0.3333333333333333703, 0.3333333333333333703, 0.3333333333333334259, 0.3333333333333333703, 0.3333333333333334259, 0.3333333333333333703, 0.3333333333333334259, 0.3333333333333332593, 0.3333333333333333703, 0.3333333333333334259, 0.3333333333333333148, 0.3333333333333333148, 0.3333333333333333703, 0.3333333333333334814, 0.3333333333333333148, 0.3333333333333333703, 0.3333333333333334259, 0.3333333333333333703, 0.3333333333333333703, 0.3333333333333333148, 0.3333333333333333703, 0.3333333333333333148, 0.3333333333333335369, 0.3333333333333332593, 0.3333333333333333703, 0.3333333333333333148, 0.3333333333333333703, 0.3333333333333334259, 0.3333333333333334259, 0.3333333333333333703, 0.3333333333333333148, 0.3333333333333334259, 0.3333333333333334259, 0.3333333333333333148, 0.3333333333333334259, 0.3333333333333335369, 0.3333333333333332593, 0.3333333333333333703, 0.3333333333333335369, 0.3333333333333332038, 0.3333333333333334259, 0.3333333333333333148, 0.3333333333333333703, 0.3333333333333333703, 0.3333333333333333703, 0.3333333333333333148, 0.3333333333333333703, 0.3333333333333333703, 0.3333333333333334259, 0.3333333333333334259, 0.3333333333333333148, 0.3333333333333334259, 0.3333333333333333148, 0.3333333333333333703, 0.3333333333333333148, 0.3333333333333334259, 0.3333333333333332038, 0.3333333333333333703, 0.3333333333333334259, 0.3333333333333335369, 0.3333333333333333148, 0.3333333333333333703, 0.3333333333333333703, 0.3333333333333333703, 0.3333333333333333703, 0.3333333333333333703, 0.3333333333333333703, 0.3333333333333334259, 0.3333333333333333703, 0.3333333333333333703, 0.3333333333333333703, 0.3333333333333332038, 0.3333333333333333703, 0.3333333333333335369, 0.3333333333333333148, 0.3333333333333334814, 0.3333333333333333703, 0.3333333333333332593, 0.3333333333333335369, 0.3333333333333333148, 0.3333333333333333703, 0.3333333333333333703, 0.3333333333333333148, 0.3333333333333333703, 0.3333333333333334259, 0.3333333333333334259, 0.3333333333333333703, 0.3333333333333334259, 0.3333333333333333148, 0.3333333333333333703, 0.3333333333333332593, 0.3333333333333333703, 0.3333333333333333703, 0.3333333333333333703, 0.3333333333333333703, 0.3333333333333333703, 0.3333333333333333703, 0.3333333333333333148, 0.3333333333333334259, 0.3333333333333333703, 0.3333333333333334259, 0.3333333333333333148, 0.3333333333333334259, 0.3333333333333333148, 0.3333333333333333703, 0.3333333333333334259, 0.3333333333333333703, 0.3333333333333333148, 0.3333333333333333148, 0.3333333333333334259, 0.3333333333333333703, 0.3333333333333333703, 0.3333333333333334259, 0.3333333333333333703, 0.3333333333333333148, 0.3333333333333334814, 0.3333333333333333703, 0.3333333333333334259, 0.3333333333333333703, 0.3333333333333333703, 0.3333333333333333703),
 ( 1.000000000000000222, 1.000000000000000222, 1.000000000000000222, 1.000000000000000222, 0.9999999999999996669, 0.9999999999999997780, 1.000000000000000444, 1.000000000000000000, 1.000000000000000000, 1.000000000000000000, 0.9999999999999997780, 1.000000000000000000, 1.000000000000000000, 1.000000000000000000, 1.000000000000000000, 0.9999999999999997780, 1.000000000000000222, 0.9999999999999996669, 1.000000000000000000, 0.9999999999999997780, 1.000000000000000222, 1.000000000000000000, 1.000000000000000222, 0.9999999999999996669, 1.000000000000000000, 1.000000000000000222, 0.9999999999999996669, 1.000000000000000444, 1.000000000000000000, 0.9999999999999997780, 1.000000000000000222, 1.000000000000000222, 1.000000000000000222, 1.000000000000000000, 1.000000000000000000, 0.9999999999999997780, 1.000000000000000000, 1.000000000000000000, 1.000000000000000000, 1.000000000000000000, 1.000000000000000222, 1.000000000000000222, 1.000000000000000000, 1.000000000000000000, 1.000000000000000000, 0.9999999999999996669, 1.000000000000000222, 1.000000000000000000, 1.000000000000000000, 0.9999999999999997780, 0.9999999999999997780, 1.000000000000000000, 0.9999999999999996669, 1.000000000000000222, 0.9999999999999997780, 1.000000000000000222, 0.9999999999999997780, 0.9999999999999997780, 1.000000000000000222, 1.000000000000000222, 0.9999999999999997780, 1.000000000000000222, 1.000000000000000000, 1.000000000000000222, 1.000000000000000000, 0.9999999999999997780, 1.000000000000000000, 1.000000000000000000, 1.000000000000000222, 1.000000000000000222, 1.000000000000000000, 0.9999999999999997780, 1.000000000000000000, 1.000000000000000222, 0.9999999999999997780, 1.000000000000000444, 0.9999999999999996669, 1.000000000000000000, 1.000000000000000222, 0.9999999999999997780, 0.9999999999999997780, 0.9999999999999997780, 1.000000000000000000, 0.9999999999999997780, 1.000000000000000000, 0.9999999999999997780, 1.000000000000000222, 1.000000000000000000, 1.000000000000000222, 1.000000000000000000, 0.9999999999999997780, 1.000000000000000000, 1.000000000000000000, 0.9999999999999997780, 1.000000000000000222, 1.000000000000000000, 1.000000000000000000, 1.000000000000000000, 1.000000000000000222, 0.9999999999999996669, 1.000000000000000222, 1.000000000000000000, 1.000000000000000000, 0.9999999999999997780, 1.000000000000000000, 0.9999999999999997780, 1.000000000000000000, 1.000000000000000222, 1.000000000000000000, 0.9999999999999997780, 1.000000000000000222, 1.000000000000000222, 0.9999999999999996669, 1.000000000000000222, 1.000000000000000000, 1.000000000000000444, 0.9999999999999996669, 1.000000000000000000, 1.000000000000000222, 1.000000000000000222, 1.000000000000000222, 1.000000000000000222, 1.000000000000000000, 0.9999999999999997780, 1.000000000000000222, 1.000000000000000000, 1.000000000000000222, 0.9999999999999996669, 1.000000000000000000, 1.000000000000000000, 1.000000000000000222, 1.000000000000000222, 0.9999999999999997780, 1.000000000000000000, 0.9999999999999997780, 1.000000000000000222, 1.000000000000000000, 1.000000000000000222, 1.000000000000000000, 1.000000000000000444, 0.9999999999999996669, 1.000000000000000444, 0.9999999999999996669, 0.9999999999999997780, 0.9999999999999997780, 1.000000000000000222, 1.000000000000000000, 0.9999999999999997780, 1.000000000000000000, 0.9999999999999997780, 0.9999999999999996669, 1.000000000000000222, 1.000000000000000000, 0.9999999999999997780, 1.000000000000000000, 1.000000000000000000, 1.000000000000000222, 1.000000000000000000, 1.000000000000000000, 1.000000000000000444, 0.9999999999999997780, 1.000000000000000222, 1.000000000000000222, 0.9999999999999997780, 1.000000000000000444, 0.9999999999999996669, 1.000000000000000000, 0.9999999999999997780, 1.000000000000000222, 0.9999999999999997780, 1.000000000000000222, 1.000000000000000000, 1.000000000000000222, 0.9999999999999997780, 0.9999999999999997780, 1.000000000000000000, 1.000000000000000000, 0.9999999999999997780, 1.000000000000000222, 0.9999999999999997780, 1.000000000000000000, 1.000000000000000000, 1.000000000000000222, 1.000000000000000000, 0.9999999999999997780, 1.000000000000000222, 1.000000000000000444, 1.000000000000000000, 1.000000000000000000, 1.000000000000000000, 1.000000000000000000, 0.9999999999999997780, 1.000000000000000000, 1.000000000000000222, 1.000000000000000000, 1.000000000000000222, 0.9999999999999996669, 1.000000000000000000, 1.000000000000000000, 0.9999999999999994449, 1.000000000000000444, 1.000000000000000000, 1.000000000000000222, 0.9999999999999997780, 1.000000000000000000, 1.000000000000000222, 1.000000000000000000, 0.9999999999999996669, 1.000000000000000444, 0.9999999999999997780, 1.000000000000000444, 0.9999999999999996669, 1.000000000000000000, 0.9999999999999996669, 1.000000000000000444, 1.000000000000000000, 0.9999999999999997780, 1.000000000000000222, 1.000000000000000000, 0.9999999999999997780, 1.000000000000000444, 1.000000000000000222, 0.9999999999999997780, 1.000000000000000000, 1.000000000000000222, 0.9999999999999997780, 1.000000000000000222, 1.000000000000000222, 1.000000000000000000, 1.000000000000000000, 0.9999999999999996669, 1.000000000000000222, 0.9999999999999997780, 1.000000000000000000, 0.9999999999999997780, 1.000000000000000444, 1.000000000000000000, 1.000000000000000000, 0.9999999999999997780, 1.000000000000000444, 1.000000000000000000, 0.9999999999999997780, 1.000000000000000444, 0.9999999999999996669, 1.000000000000000444, 1.000000000000000000, 1.000000000000000444, 1.000000000000000222, 1.000000000000000222, 0.9999999999999997780, 1.000000000000000000, 0.9999999999999997780, 1.000000000000000444, 0.9999999999999996669, 1.000000000000000000, 1.000000000000000000, 1.000000000000000222, 1.000000000000000000, 1.000000000000000222, 1.000000000000000000, 1.000000000000000000, 0.9999999999999997780, 1.000000000000000000, 1.000000000000000000, 0.9999999999999997780, 1.000000000000000000, 1.000000000000000000, 0.9999999999999997780, 1.000000000000000000, 1.000000000000000222, 1.000000000000000000, 1.000000000000000000, 1.000000000000000000, 1.000000000000000000, 0.9999999999999996669, 1.000000000000000222, 1.000000000000000000, 0.9999999999999997780, 1.000000000000000000, 1.000000000000000222, 1.000000000000000000, 1.000000000000000222, 1.000000000000000222, 1.000000000000000000, 1.000000000000000222, 1.000000000000000000, 1.000000000000000000, 1.000000000000000000, 1.000000000000000222, 0.9999999999999996669, 1.000000000000000222, 0.9999999999999996669, 1.000000000000000222, 1.000000000000000222, 1.000000000000000222, 1.000000000000000222, 0.9999999999999996669, 1.000000000000000444, 1.000000000000000000, 1.000000000000000000, 1.000000000000000222, 1.000000000000000444, 0.9999999999999996669, 1.000000000000000444, 1.000000000000000222, 0.9999999999999996669, 1.000000000000000222, 0.9999999999999997780, 1.000000000000000000, 1.000000000000000000, 0.9999999999999997780, 1.000000000000000000, 0.9999999999999997780, 1.000000000000000000, 1.000000000000000000, 1.000000000000000444, 0.9999999999999997780, 1.000000000000000222, 0.9999999999999997780, 0.9999999999999997780, 1.000000000000000000, 1.000000000000000000, 0.9999999999999996669, 1.000000000000000000, 1.000000000000000222, 1.000000000000000222, 0.9999999999999997780, 1.000000000000000222, 0.9999999999999997780, 0.9999999999999997780, 1.000000000000000000, 1.000000000000000000, 1.000000000000000000, 1.000000000000000222, 1.000000000000000000, 1.000000000000000222, 1.000000000000000000, 0.9999999999999996669, 0.9999999999999997780, 1.000000000000000444, 0.9999999999999996669, 1.000000000000000444, 0.9999999999999997780, 0.9999999999999997780, 1.000000000000000222, 0.9999999999999997780, 1.000000000000000222, 1.000000000000000000, 1.000000000000000000, 0.9999999999999997780, 1.000000000000000222, 1.000000000000000222, 1.000000000000000000, 1.000000000000000222, 1.000000000000000000, 1.000000000000000000, 0.9999999999999997780, 1.000000000000000000, 1.000000000000000000, 0.9999999999999997780, 1.000000000000000000, 0.9999999999999996669, 1.000000000000000222, 0.9999999999999997780, 1.000000000000000222, 0.9999999999999997780, 1.000000000000000000, 0.9999999999999997780, 1.000000000000000222, 0.9999999999999997780, 1.000000000000000000, 1.000000000000000000, 1.000000000000000000, 1.000000000000000000, 0.9999999999999997780, 1.000000000000000222, 1.000000000000000000, 0.9999999999999997780, 1.000000000000000000, 1.000000000000000000, 1.000000000000000222, 1.000000000000000222, 1.000000000000000000, 1.000000000000000222, 1.000000000000000000, 1.000000000000000000, 1.000000000000000000) ) ) 
 REPRESENTATION_ITEM ( '' )  SURFACE ( )  );
#32158 = CARTESIAN_POINT ( 'NONE',  ( -5.420227550413282636, 9.545625585449309725, 0.7998128361456291469 ) ) ;
#32159 = CARTESIAN_POINT ( 'NONE',  ( -2.200615117903204077, 5.615171720908647579, 1.040834085586084257E-14 ) ) ;
#32160 = CARTESIAN_POINT ( 'NONE',  ( 2.930518499080053907, 1.225513248159842083, -1.835134156090315605 ) ) ;
#32161 = CARTESIAN_POINT ( 'NONE',  ( 4.745575995134789338, -1.744828745684245508, -1.440138369970354493 ) ) ;
#32162 = CARTESIAN_POINT ( 'NONE',  ( -7.049876689426113785, 8.287572894827684777, -1.082531754730544860 ) ) ;
#32163 = CARTESIAN_POINT ( 'NONE',  ( 5.027533431531807651, -0.2580777524966316738, 1.792966082415799800 ) ) ;
#32164 = CARTESIAN_POINT ( 'NONE',  ( 5.436718845459293625, -1.505851745483515858, 1.184076087961029700 ) ) ;
#32165 = CARTESIAN_POINT ( 'NONE',  ( 0.6823417656249899377, 4.988541667008086655, -1.181850606188754593 ) ) ;
#32166 = CARTESIAN_POINT ( 'NONE',  ( 6.455916552660014851, 1.865467424361374249, -0.1398750677365916961 ) ) ;
#32167 = CARTESIAN_POINT ( 'NONE',  ( 5.459367789976862895, 1.521435002614815790, 1.071484558867175529 ) ) ;
#32168 = CARTESIAN_POINT ( 'NONE',  ( -1.387358672527355008, 7.251968950354660493, 4.302625267139497112 ) ) ;
#32169 = CARTESIAN_POINT ( 'NONE',  ( 6.649276393164253562, -1.424495517243940856, -1.050074490644896441 ) ) ;
#32170 = CARTESIAN_POINT ( 'NONE',  ( 1.042204282965590201, 0.8216761606248854655, 1.841732292558920570 ) ) ;
#32172 = CARTESIAN_POINT ( 'NONE',  ( 3.387430394310109616, 1.903944824823229798, -0.9005924351132842398 ) ) ;
#32171 = CARTESIAN_POINT ( 'NONE',  ( -4.744990574658554117, 4.638169879964154418, 1.214306433183764966E-14 ) ) ;
#32173 = CARTESIAN_POINT ( 'NONE',  ( 8.829384350997564468, 11.32403438096243775, 1.599625672291281386 ) ) ;
#32175 = CARTESIAN_POINT ( 'NONE',  ( -8.157201976916404362, 12.66848607304450702, -0.7998128361456281477 ) ) ;
#32174 = FACE_OUTER_BOUND ( 'NONE', #59146, .T. ) ;
#32176 = FACE_OUTER_BOUND ( 'NONE', #14656, .T. ) ;
#32177 = CARTESIAN_POINT ( 'NONE',  ( 2.232681213900446160, 1.316219961256912763, -1.532148775131780383 ) ) ;
#32178 = CARTESIAN_POINT ( 'NONE',  ( -1.201851678989727383E-14, 2.071875000341422801, 1.575800808251672791 ) ) ;
#32179 = CARTESIAN_POINT ( 'NONE',  ( 4.630273154266905777, 5.360739087188218122, 1.199719254218464037 ) ) ;
#32180 = CARTESIAN_POINT ( 'NONE',  ( 2.847126979364768218, -1.798887516807456954, 1.198237791991546564 ) ) ;
#32181 = CARTESIAN_POINT ( 'NONE',  ( 6.889999999999973035, 7.629137130509070275, 2.319999999999996287 ) ) ;
#32184 = DIRECTION ( 'NONE',  ( 0.000000000000000000, -1.000000000000000000, 0.000000000000000000 ) ) ;
#32183 = CARTESIAN_POINT ( 'NONE',  ( -6.509799877575631832, 5.178456542363093718, -2.499999999999995115 ) ) ;
#32182 = CARTESIAN_POINT ( 'NONE',  ( 4.573896719763862251, 6.429575154514868274, -1.599625672291273171 ) ) ;
#32185 = CARTESIAN_POINT ( 'NONE',  ( 8.500599125643985232, 11.90082083235127008, -1.082531754730543083 ) ) ;
#32186 = CARTESIAN_POINT ( 'NONE',  ( 0.7499999999999920064, 4.014583334016149863, 1.299038105676669330 ) ) ;
#32187 = CARTESIAN_POINT ( 'NONE',  ( -7.863365906246068349, 9.236643647784308797, -1.082531754730543971 ) ) ;
#32188 = CARTESIAN_POINT ( 'NONE',  ( 1.364683531249988757, 0.8843750003414210248, 0.000000000000000000 ) ) ;
#32189 = CARTESIAN_POINT ( 'NONE',  ( 1.101424459656743071, -0.5276332240332289869, 2.126988402630063835 ) ) ;
#32190 = CARTESIAN_POINT ( 'NONE',  ( 0.1495493664682667478, 8.232402834745700559, 1.999498275786589119 ) ) ;
#32191 = CARTESIAN_POINT ( 'NONE',  ( 2.430887666589570451, 2.194555640652501527, 0.5498776597147712053 ) ) ;
#32192 = CARTESIAN_POINT ( 'NONE',  ( -7.995557903757128493, 10.35123685918189729, 1.599625672291295375 ) ) ;
#32193 = CARTESIAN_POINT ( 'NONE',  ( -5.056828107772872727, 5.001980335264194721, -0.7216878364870197293 ) ) ;
#32194 = CARTESIAN_POINT ( 'NONE',  ( -1.364683531250010295, 3.842708333674751398, 0.7879004041258379498 ) ) ;
#32195 = CARTESIAN_POINT ( 'NONE',  ( 4.631618433768171172, 8.327536854573105884, -0.3785340233409782984 ) ) ;
#32196 = CARTESIAN_POINT ( 'NONE',  ( -6.009258394948636914E-15, 11.68750000000000000, -1.732050807568875195 ) ) ;
#32197 = CARTESIAN_POINT ( 'NONE',  ( 7.512626515748109135, 8.897724035528543851, 1.082531754730549967 ) ) ;
#32198 = CARTESIAN_POINT ( 'NONE',  ( 3.040057762974816224, 1.755912757559551007, 0.2203070401886226548 ) ) ;
#32199 = CARTESIAN_POINT ( 'NONE',  ( 6.229534195615700654, -2.079954537573494466, 0.7377168454194837910 ) ) ;
#32200 = AXIS2_PLACEMENT_3D ( 'NONE', #176607, #78028, #75902 ) ;
#32201 = CARTESIAN_POINT ( 'NONE',  ( -8.012344526598182026E-15, 8.796875000341401574, -1.575800808251669460 ) ) ;
#32202 = ORIENTED_EDGE ( 'NONE', *, *, #87069, .T. ) ;
#32203 = CARTESIAN_POINT ( 'NONE',  ( -5.611095471209320174, 7.639640364534566075, 1.599625672291263179 ) ) ;
#32204 = CARTESIAN_POINT ( 'NONE',  ( 5.624625116526842383, 0.3961212581503182339, 1.976953148079656719 ) ) ;
#32206 = VERTEX_POINT ( 'NONE', #34061 ) ;
#32205 = CARTESIAN_POINT ( 'NONE',  ( 4.851724922005476337, -1.286371495869711667, -1.275854292049487304 ) ) ;
#32207 = EDGE_CURVE ( 'NONE', #170100, #101997, #163678, .T. ) ;
#32208 = CARTESIAN_POINT ( 'NONE',  ( 2.078771448894382701, -0.08914341469279042640, -1.868647664167771394 ) ) ;
#32209 = CARTESIAN_POINT ( 'NONE',  ( 3.362232293424003426, -2.068089847843882279, 0.09686330349460009481 ) ) ;
#32210 = CARTESIAN_POINT ( 'NONE',  ( -6.360183458142173230, 9.473945563590925545, 1.082531754730549967 ) ) ;
#32211 = CARTESIAN_POINT ( 'NONE',  ( 1.564566645345835116, 0.6029492335615972420, 1.814891859350221459 ) ) ;
#32212 = CARTESIAN_POINT ( 'NONE',  ( -0.6500572981163014186, 3.349925512430769636, 0.06817653764027252483 ) ) ;
#32213 = CARTESIAN_POINT ( 'NONE',  ( -9.470156251935129887, 4.005132839944305800, -6.837168546664702085 ) ) ;
#32214 = CARTESIAN_POINT ( 'NONE',  ( -5.477447344779489136, 6.303105555648046199, 0.9994663861491676071 ) ) ;
#32215 = B_SPLINE_CURVE_WITH_KNOTS ( 'NONE', 3,
 ( #142858, #75689, #208861, #154812, #176395, #144988, #213126, #65788, #194759, #112512 ),
 .UNSPECIFIED., .F., .F.,
 ( 4, 2, 2, 2, 4 ),
 ( 0.000000000000000000, 0.0003519860449266724498, 0.0007039720898533448996, 0.001055958134780017295, 0.001407944179706689799 ),
 .UNSPECIFIED. ) ;
#32216 = CARTESIAN_POINT ( 'NONE',  ( 1.364683531249990311, 4.196875000341417028, 1.214306433183764966E-14 ) ) ;
#32217 = CARTESIAN_POINT ( 'NONE',  ( 1.072351618572921605, 0.7776387867773438822, 1.747342548420704578 ) ) ;
#32218 = EDGE_CURVE ( 'NONE', #162762, #201902, #71870, .T. ) ;
#32219 = CARTESIAN_POINT ( 'NONE',  ( 2.682025323810240280, -1.127217178123595565, -1.605522638798158264 ) ) ;
#32220 = CARTESIAN_POINT ( 'NONE',  ( 0.3509351863830567075, -0.9528684895154272416, 1.776737725368633614 ) ) ;
#32221 = CARTESIAN_POINT ( 'NONE',  ( -3.949167883330528372, 7.829389307186077396, 1.214306433183764966E-14 ) ) ;
#32223 = CARTESIAN_POINT ( 'NONE',  ( -1.749999999999999778, 2.143131898507868051E-16, 0.000000000000000000 ) ) ;
#32222 = CARTESIAN_POINT ( 'NONE',  ( 8.392660782059197189, 9.750191319612612872, 1.199719254218462483 ) ) ;
#32224 = CARTESIAN_POINT ( 'NONE',  ( 0.2275331484566482099, -1.145445245298154946, -1.479381579510357980 ) ) ;
#32225 = CARTESIAN_POINT ( 'NONE',  ( -1.364683531250000748, 2.259375000341422357, 1.214306433183764966E-14 ) ) ;
#32226 = CARTESIAN_POINT ( 'NONE',  ( 2.426041559740747200, -1.990683941386611311, 0.2996653706425453367 ) ) ;
#32228 = CARTESIAN_POINT ( 'NONE',  ( 1.757563674541680721, 2.025006261547353414, -0.6180173261674735130 ) ) ;
#32227 = CARTESIAN_POINT ( 'NONE',  ( -7.890482213473404727, 8.307910125248191946, 0.7216878364870578100 ) ) ;
#32229 = CARTESIAN_POINT ( 'NONE',  ( 8.125020845233269284, 14.19599321528319891, -8.831577418034537885 ) ) ;
#32230 = CARTESIAN_POINT ( 'NONE',  ( 3.490741092712910998, 2.019281663078629219, 0.4563312328872348722 ) ) ;
#32231 = CARTESIAN_POINT ( 'NONE',  ( 4.869313445963426190, 5.709895770826003414, 1.199719254218452935 ) ) ;
#32233 = CARTESIAN_POINT ( 'NONE',  ( 3.167801447087334576, 6.847518788243868393, -0.7998128361456291469 ) ) ;
#32232 = CARTESIAN_POINT ( 'NONE',  ( 5.718719656712253574, -0.05221879637645754357, 2.090152071033167136 ) ) ;
#32235 = EDGE_LOOP ( 'NONE', ( #117717, #170910, #146245, #42548, #35236 ) ) ;
#32234 = CARTESIAN_POINT ( 'NONE',  ( 3.680510133705969800, -1.759192178946006990, -0.4875382671739314500 ) ) ;
#32236 = CARTESIAN_POINT ( 'NONE',  ( 10.24048609702354717, 10.84165528948263457, -0.7998128361456281477 ) ) ;
#32238 = AXIS2_PLACEMENT_3D ( 'NONE', #93763, #127396, #73202 ) ;
#32237 = CARTESIAN_POINT ( 'NONE',  ( 10.16812126801399607, 13.45311586547773963, 7.234909159705820159 ) ) ;
#32239 = CARTESIAN_POINT ( 'NONE',  ( 6.141676493652540536, -1.594220855400224401, -1.526124331276897950 ) ) ;
#32240 = CARTESIAN_POINT ( 'NONE',  ( -1.364683531250014514, 10.40104166700806587, -0.7879004041258335089 ) ) ;
#32241 = ORIENTED_EDGE ( 'NONE', *, *, #26940, .F. ) ;
#32242 = CARTESIAN_POINT ( 'NONE',  ( 5.549440478958017842, -1.726947976793650197, 0.8215754744917986852 ) ) ;
#32243 = CARTESIAN_POINT ( 'NONE',  ( -8.109748439268576803, 12.61312361245537517, 0.7998128361456481317 ) ) ;
#32244 = CARTESIAN_POINT ( 'NONE',  ( 7.579171565239241737, 8.801120566655981747, 1.199719254218462483 ) ) ;
#32245 = CARTESIAN_POINT ( 'NONE',  ( -1.360316468750042862, 0.9010416670080623192, -0.7853790794159041244 ) ) ;
#32246 = CARTESIAN_POINT ( 'NONE',  ( 3.836594282542909795, 6.459481848733281240, 1.082531754730558626 ) ) ;
#32247 = EDGE_CURVE ( 'NONE', #207943, #84441, #133741, .T. ) ;
#32248 = CARTESIAN_POINT ( 'NONE',  ( -11.86145016429273191, 12.69999999999999929, 1.099999999999996758 ) ) ;
#32249 = CARTESIAN_POINT ( 'NONE',  ( -6.328223859912621485, 6.936542968411253618, 0.8711560941448781570 ) ) ;
#32250 = CARTESIAN_POINT ( 'NONE',  ( 0.2570343420702363435, 1.821350608449383124, -0.2692129421619017804 ) ) ;
#32251 = ORIENTED_EDGE ( 'NONE', *, *, #198010, .T. ) ;
#32252 = CARTESIAN_POINT ( 'NONE',  ( -7.533490631048818109, 8.818102486758951031, -1.199719254218452047 ) ) ;
#32253 = CARTESIAN_POINT ( 'NONE',  ( 4.956247902659736582, 0.7144662795386286236, 1.728917671469521800 ) ) ;
#32254 = CARTESIAN_POINT ( 'NONE',  ( -0.02338929933909209349, 2.063686797106215387, -2.128951798380565918 ) ) ;
#32255 = DIRECTION ( 'NONE',  ( 0.000000000000000000, 0.000000000000000000, -1.000000000000000000 ) ) ;
#32256 = CARTESIAN_POINT ( 'NONE',  ( 0.02465192458550417853, 14.53714098577670910, 11.97749476893806353 ) ) ;
#32257 = COLOUR_RGB ( '', 0.31764706, 0.68627451, 0.89019608) ;
#32258 = AXIS2_PLACEMENT_3D ( 'NONE', #65654, #115562, #98209 ) ;
#32259 = CARTESIAN_POINT ( 'NONE',  ( -6.480434237652138663, 8.583592582059388576, 1.443375672974078761 ) ) ;
#32260 = CARTESIAN_POINT ( 'NONE',  ( 4.985647801523278133, 6.839675073242382553, -1.599625672291256295 ) ) ;
#32261 = CARTESIAN_POINT ( 'NONE',  ( 1.182395473146230946, 1.177546377092754337, -1.578453288034264990 ) ) ;
#32262 = EDGE_CURVE ( 'NONE', #170262, #211395, #66296, .T. ) ;
#32263 = CARTESIAN_POINT ( 'NONE',  ( 2.179314750421776026, 1.560514648525725967, 1.277027416600539755 ) ) ;
#32264 = CARTESIAN_POINT ( 'NONE',  ( -8.239604668803112375, 10.63595808506888396, -1.599625672291263179 ) ) ;
#32265 = CARTESIAN_POINT ( 'NONE',  ( 4.532168488718122390, 8.509556680138327778, 0.7998128361456271485 ) ) ;
#32266 = CARTESIAN_POINT ( 'NONE',  ( -0.07933194154489606187, -9.746166700180788567, -9.499668754385620417 ) ) ;
#32267 = CARTESIAN_POINT ( 'NONE',  ( 2.009981539508858273, -1.034714594384738229, -1.931790675223004738 ) ) ;
#32268 = CARTESIAN_POINT ( 'NONE',  ( 0.08058608058607655278, -8.407420853759283830, 10.99970480893082225 ) ) ;
#32269 = CARTESIAN_POINT ( 'NONE',  ( -9.969323024750229578, 10.52529837183042716, -0.7998128361456291469 ) ) ;
#32270 = DIRECTION ( 'NONE',  ( -1.561558963378126405E-12, 1.000000000000000000, -1.535693738323023938E-12 ) ) ;
#32271 = CARTESIAN_POINT ( 'NONE',  ( 10.33293948230768144, 2.515145635913765165, -5.518992160705104233 ) ) ;
#32272 = CARTESIAN_POINT ( 'NONE',  ( 4.638297949650961982, 5.544340708415133712, -1.082531754730548412 ) ) ;
#32273 = CARTESIAN_POINT ( 'NONE',  ( 7.910292558569346433, 11.31609285405122556, -1.199719254218446718 ) ) ;
#32274 = AXIS2_PLACEMENT_3D ( 'NONE', #29191, #128899, #148283 ) ;
#32275 = DIRECTION ( 'NONE',  ( -0.000000000000000000, 1.000000000000000000, 0.000000000000000000 ) ) ;
#32276 = CARTESIAN_POINT ( 'NONE',  ( 5.370438244788902971, 9.279612028980123384, -0.7216878364870458196 ) ) ;
#32277 = ORIENTED_EDGE ( 'NONE', *, *, #24826, .F. ) ;
#32279 = CARTESIAN_POINT ( 'NONE',  ( 1.840491241682026047, 1.157229580565920513, -1.647056139248611384 ) ) ;
#32278 = CARTESIAN_POINT ( 'NONE',  ( 5.073706409418358376, -1.018251046719556685, 1.533866337327425278 ) ) ;
#32280 = CARTESIAN_POINT ( 'NONE',  ( 3.480086682454126557, 2.076208366568982555, 0.9861560518420305899 ) ) ;
#32282 = CARTESIAN_POINT ( 'NONE',  ( 0.6021283177516533192, 1.855420301818105910, 0.1446146731104556993 ) ) ;
#32281 = DIRECTION ( 'NONE',  ( 0.000000000000000000, -1.000000000000000000, 0.000000000000000000 ) ) ;
#32283 = CARTESIAN_POINT ( 'NONE',  ( -3.285556943750000070, -2.909374999522040817, 0.000000000000000000 ) ) ;
#32284 = CARTESIAN_POINT ( 'NONE',  ( 0.000000000000000000, 7.500000000000000000, 0.000000000000000000 ) ) ;
#32285 = CARTESIAN_POINT ( 'NONE',  ( 5.396708386617175890, -1.867154475869851504, -0.4128305108781898936 ) ) ;
#32286 = CARTESIAN_POINT ( 'NONE',  ( -8.995998617867369873, 10.45408546138876993, 1.199719254218462483 ) ) ;
#32287 = CARTESIAN_POINT ( 'NONE',  ( -5.885648082108231982, 7.959951743916638733, 1.443375672974058777 ) ) ;
#32289 = CARTESIAN_POINT ( 'NONE',  ( 3.362029495745801899, 0.8400119854848131506, 1.671504782411597612 ) ) ;
#32288 = CARTESIAN_POINT ( 'NONE',  ( 3.245728744149275702, 2.090933975402937683, -0.002398190518447183318 ) ) ;
#32290 = CARTESIAN_POINT ( 'NONE',  ( 7.375272376154084597, 9.627570410311676596, -1.443375672974057666 ) ) ;
#32291 = CARTESIAN_POINT ( 'NONE',  ( 6.444863656277017405, -1.483217659742748218, -1.090817886357238198 ) ) ;
#32292 = CARTESIAN_POINT ( 'NONE',  ( 2.737856954955798727, 5.281584649835344258, 1.199719254218452047 ) ) ;
#32294 = CARTESIAN_POINT ( 'NONE',  ( 3.520313441042647540, 7.258782781191745137, 0.7998128361456321445 ) ) ;
#32293 = CARTESIAN_POINT ( 'NONE',  ( -0.04325334852942971930, -8.075271019047999488, -11.00023204605253113 ) ) ;
#32295 = CARTESIAN_POINT ( 'NONE',  ( 5.496639145235802104, -0.4250261254647030307, -1.671567591930831043 ) ) ;
#32296 = CARTESIAN_POINT ( 'NONE',  ( -5.526920175865215334, 9.599823971818089774, 0.7998128361456481317 ) ) ;
#32297 = CARTESIAN_POINT ( 'NONE',  ( 0.5450593487147866734, -1.257523079656326148, 1.194353625382915673 ) ) ;
#32298 = DIRECTION ( 'NONE',  ( 3.330669073875478989E-16, -3.540251991789410786E-16, -1.000000000000000000 ) ) ;
#32299 = LINE ( 'NONE', #164429, #169323 ) ;
#32300 = CARTESIAN_POINT ( 'NONE',  ( 4.873980352634836422, -2.130485078384927178, 0.4170503277054308788 ) ) ;
#32301 = CARTESIAN_POINT ( 'NONE',  ( 3.562960707638890501, -1.610701098693729350, -0.8595150645765645692 ) ) ;
#32302 = CARTESIAN_POINT ( 'NONE',  ( 0.7780835697005838991, -1.044612314895682292, -1.660310580060719188 ) ) ;
#32303 = CARTESIAN_POINT ( 'NONE',  ( 5.366459209908462036, -2.066393128712967098, -0.4610789482254721294 ) ) ;
#32305 = CARTESIAN_POINT ( 'NONE',  ( 1.364683531249988535, 3.467708333674749621, -0.7879004041258239610 ) ) ;
#32304 = CARTESIAN_POINT ( 'NONE',  ( 6.110887424941569002, -0.2848874328069994633, 2.274520343394012212 ) ) ;
#32306 = CARTESIAN_POINT ( 'NONE',  ( -4.308793891044708779, 3.921347715840572956, 1.214306433183764966E-14 ) ) ;
#32307 = CARTESIAN_POINT ( 'NONE',  ( 7.944187942603509356, 11.35563746875774882, 1.199719254218460707 ) ) ;
#32308 = CARTESIAN_POINT ( 'NONE',  ( 1.910938629679886480, -0.5684797485801665884, -2.042784538176869003 ) ) ;
#32309 = CARTESIAN_POINT ( 'NONE',  ( -3.958617665510279160, 5.641473247893851628, -1.443375672974053447 ) ) ;
#32310 = CARTESIAN_POINT ( 'NONE',  ( 2.189868734255736360, 1.000000000000000888, -11.69137891449145172 ) ) ;
#32311 = CARTESIAN_POINT ( 'NONE',  ( -4.026408433134269771, 6.680931691089825541, 1.082531754730560403 ) ) ;
#32312 = CARTESIAN_POINT ( 'NONE',  ( 6.315302488195832176, -1.857785929941946135, -1.123309179604212504 ) ) ;
#32314 = CARTESIAN_POINT ( 'NONE',  ( 0.7500000000000006661, 12.36458333401613174, 1.299038105676657340 ) ) ;
#32313 = CARTESIAN_POINT ( 'NONE',  ( 6.983263157960330147, 2.416677186285462575, 2.534499922921686021 ) ) ;
#32316 = EDGE_LOOP ( 'NONE', ( #40118, #70708, #187879, #121294 ) ) ;
#32315 = CARTESIAN_POINT ( 'NONE',  ( 1.963841274844113194, -1.786346139091129270, -1.320113705855001207 ) ) ;
#32317 = CARTESIAN_POINT ( 'NONE',  ( -0.1042281025761494367, -0.9885194109933435058, -2.072332397174360352 ) ) ;
#32319 = CARTESIAN_POINT ( 'NONE',  ( 5.963753124799120897, -0.5065058054696270906, 1.999279329544477513 ) ) ;
#32318 = CARTESIAN_POINT ( 'NONE',  ( 3.985207087413062066, 6.736826471035503694, -1.199719254218452047 ) ) ;
#32321 = CARTESIAN_POINT ( 'NONE',  ( 3.475000000000000533, -3.354166666666667851, 2.006292185433948827 ) ) ;
#32320 = CARTESIAN_POINT ( 'NONE',  ( 5.825163275726873202, 6.825053905550038991, 1.199719254218452047 ) ) ;
#32322 = CARTESIAN_POINT ( 'NONE',  ( 5.631432701629774051, 7.663367133358481631, 1.599625672291269396 ) ) ;
#32323 = CARTESIAN_POINT ( 'NONE',  ( 3.285556943750000070, -3.871874999522042504, 0.000000000000000000 ) ) ;
#32324 = DIRECTION ( 'NONE',  ( 0.7592566023653005702, 0.6507913734559639396, 0.000000000000000000 ) ) ;
#32325 = CARTESIAN_POINT ( 'NONE',  ( 4.563899478665734755, -1.199029595066217313, 1.397436126395680267 ) ) ;
#32326 = CARTESIAN_POINT ( 'NONE',  ( 4.599240423533799138, 6.388866465587984322, 1.599625672291267398 ) ) ;
#32327 = CARTESIAN_POINT ( 'NONE',  ( -0.2104748580754201015, 7.629137130509078268, -2.703678718140526627 ) ) ;
#32328 = CARTESIAN_POINT ( 'NONE',  ( 1.869703332329395895, 0.8828569656042523084, 1.481527559500251501 ) ) ;
#32329 = CARTESIAN_POINT ( 'NONE',  ( 0.2999999999999860556, 4.000000000000010658, 1.007084189318397938 ) ) ;
#32330 =( BOUNDED_SURFACE ( )  B_SPLINE_SURFACE ( 3, 3, ( 
 ( #186996, #59137, #58074, #157728, #204286, #171824, #23418, #205373, #122096, #154514 ),
 ( #72163, #89529, #42919, #9323, #40778, #6095, #139343, #57008, #137209, #22340 ),
 ( #87376, #123180, #189140, #106884, #172910, #24484, #41854, #207518, #153446, #90596 ),
 ( #54876, #104703, #88454, #156655, #173992, #8248, #203231, #74332, #140434, #124236 ),
 ( #121029, #107964, #25564, #125296, #191254, #38627, #43979, #60201, #161994, #94865 ),
 ( #158780, #209636, #14639, #193408, #192321, #211775, #196613, #27709, #113302, #109029 ),
 ( #126362, #142561, #160919, #110098, #210717, #128505, #159844, #130621, #26633, #111164 ) ),
 .UNSPECIFIED., .T., .F., .T. ) 
 B_SPLINE_SURFACE_WITH_KNOTS ( ( 4, 3, 4 ),
 ( 4, 1, 1, 1, 1, 1, 1, 4 ),
 ( 0.000000000000000000, 0.5000000000000000000, 1.000000000000000000 ),
 ( 0.000000000000000000, 0.09853459476447307130, 0.1926867929487333375, 0.2613852218134048999, 0.3629775382994345767, 0.5216635214973427415, 0.7338723600040717443, 1.000000000000000000 ),
 .UNSPECIFIED. ) 
 GEOMETRIC_REPRESENTATION_ITEM ( )  RATIONAL_B_SPLINE_SURFACE ( (
 ( 1.000000000000000000, 1.000000000000000000, 1.000000000000000222, 1.000000000000000000, 0.9999999999999997780, 1.000000000000000000, 0.9999999999999997780, 0.9999999999999997780, 1.000000000000000000, 1.000000000000000000),
 ( 0.3333333333333333703, 0.3333333333333333703, 0.3333333333333334259, 0.3333333333333333703, 0.3333333333333332593, 0.3333333333333334259, 0.3333333333333333148, 0.3333333333333333148, 0.3333333333333333703, 0.3333333333333333703),
 ( 0.3333333333333333703, 0.3333333333333333703, 0.3333333333333334259, 0.3333333333333333703, 0.3333333333333332593, 0.3333333333333334259, 0.3333333333333333148, 0.3333333333333333148, 0.3333333333333333703, 0.3333333333333333703),
 ( 1.000000000000000000, 1.000000000000000000, 1.000000000000000222, 1.000000000000000000, 0.9999999999999997780, 1.000000000000000000, 0.9999999999999997780, 0.9999999999999997780, 1.000000000000000000, 1.000000000000000000),
 ( 0.3333333333333333703, 0.3333333333333333703, 0.3333333333333334259, 0.3333333333333333703, 0.3333333333333332593, 0.3333333333333334259, 0.3333333333333333148, 0.3333333333333333148, 0.3333333333333333703, 0.3333333333333333703),
 ( 0.3333333333333333703, 0.3333333333333333703, 0.3333333333333334259, 0.3333333333333333703, 0.3333333333333332593, 0.3333333333333334259, 0.3333333333333333148, 0.3333333333333333148, 0.3333333333333333703, 0.3333333333333333703),
 ( 1.000000000000000000, 1.000000000000000000, 1.000000000000000222, 1.000000000000000000, 0.9999999999999997780, 1.000000000000000000, 0.9999999999999997780, 0.9999999999999997780, 1.000000000000000000, 1.000000000000000000) ) ) 
 REPRESENTATION_ITEM ( '' )  SURFACE ( )  );
#32331 = CARTESIAN_POINT ( 'NONE',  ( -1.364683531250012516, 4.551041667008082214, -0.7879004041258300672 ) ) ;
#32332 = CARTESIAN_POINT ( 'NONE',  ( 1.124742813458483814, 1.347236035482470839, -1.817372803150618221 ) ) ;
#32333 = CARTESIAN_POINT ( 'NONE',  ( 3.897179185067170870, 1.779300596213341690, -1.126466309965125756 ) ) ;
#32334 = CARTESIAN_POINT ( 'NONE',  ( -3.634467696915153034, 6.397906858779740524, 1.199719254218452935 ) ) ;
#32335 = CARTESIAN_POINT ( 'NONE',  ( 2.020411781336392210, 1.649200945362235826, 0.6424177339450982682 ) ) ;
#32336 = CARTESIAN_POINT ( 'NONE',  ( 7.124973419181436007, 8.271222729588529887, -1.199719254218446718 ) ) ;
#32337 = CARTESIAN_POINT ( 'NONE',  ( 4.380693030546913391, 7.164540064729805202, 1.082531754730549078 ) ) ;
#32339 = EDGE_CURVE ( 'NONE', #52497, #33202, #212030, .T. ) ;
#32338 = CARTESIAN_POINT ( 'NONE',  ( -6.250472511100020334, 7.250971670160158311, 1.199719254218450271 ) ) ;
#32340 = UNCERTAINTY_MEASURE_WITH_UNIT (LENGTH_MEASURE( 1.000000000000000082E-05 ), #87568, 'distance_accuracy_value', 'NONE');
#32341 = CARTESIAN_POINT ( 'NONE',  ( 4.812781342726850653, 8.558735966582574406, 0.7216878364870438212 ) ) ;
#32342 = CARTESIAN_POINT ( 'NONE',  ( -1.500000000000013101, 2.129166666666693519, -0.8660254037844313801 ) ) ;
#32343 = CARTESIAN_POINT ( 'NONE',  ( 5.396815004230996138, -2.167347303010109805, -0.4865036897706440100 ) ) ;
#32344 = CARTESIAN_POINT ( 'NONE',  ( 2.959115643078192193, 0.3208686883675835877, -2.167707805308824121 ) ) ;
#32345 = CARTESIAN_POINT ( 'NONE',  ( -3.927058049452637700, 7.733318157670055371, -0.7998128361456281477 ) ) ;
#32346 = CARTESIAN_POINT ( 'NONE',  ( 0.4996389044603895546, 7.815212647110186595, -1.937417588921664047 ) ) ;
#32347 = DIRECTION ( 'NONE',  ( 0.000000000000000000, -1.000000000000000000, -1.804652791718263484E-16 ) ) ;
#32348 = VECTOR ( 'NONE', #148885, 1000.000000000000114 ) ;
#32349 = CARTESIAN_POINT ( 'NONE',  ( -0.6823417656250212460, 3.801041667008085767, 1.181850606188767472 ) ) ;
#32350 = CARTESIAN_POINT ( 'NONE',  ( 6.609999999999973674, 0.5530568637619069916, 2.330679033986877258 ) ) ;
#32351 = CARTESIAN_POINT ( 'NONE',  ( -5.111060722671894929, 5.065251719313053513, 0.000000000000000000 ) ) ;
#32352 = CARTESIAN_POINT ( 'NONE',  ( 5.554972086574996304, 0.4156608669513594534, 2.079290889414136423 ) ) ;
#32353 = CARTESIAN_POINT ( 'NONE',  ( -5.316205630334251531, 9.216340645449683677, -0.7216878364870338292 ) ) ;
#32354 = ORIENTED_EDGE ( 'NONE', *, *, #6983, .F. ) ;
#32357 = PRESENTATION_LAYER_ASSIGNMENT (  '', '', ( #11631 ) ) ;
#32356 = CARTESIAN_POINT ( 'NONE',  ( -3.443407828190952813, 6.961133532957347825, 0.7216878364870233931 ) ) ;
#32355 = CARTESIAN_POINT ( 'NONE',  ( -5.153507786970276783, 6.145418851954329575, -1.082531754730549967 ) ) ;
#32358 = CARTESIAN_POINT ( 'NONE',  ( 5.626797444871351139, 6.523350759560078593, 1.199719254218462483 ) ) ;
#32359 = CARTESIAN_POINT ( 'NONE',  ( 6.075717905342373548, -0.9791751913862613010, 1.559117742379905858 ) ) ;
#32360 = DIRECTION ( 'NONE',  ( 0.000000000000000000, 1.000000000000000000, 0.000000000000000000 ) ) ;
#32361 = DIRECTION ( 'NONE',  ( -0.6483454320283799088, 0.000000000000000000, 0.7613463080411786432 ) ) ;
#32362 = CARTESIAN_POINT ( 'NONE',  ( -1.201851678989727383E-14, 4.134375000341417028, 1.575800808251672791 ) ) ;
#32363 = CARTESIAN_POINT ( 'NONE',  ( 2.067524827727816650, -1.070173352442949311, 1.372458522238986234 ) ) ;
#32364 = CARTESIAN_POINT ( 'NONE',  ( 4.532503425670185493, 4.182342172903648070, 1.214306433183764966E-14 ) ) ;
#32365 = CARTESIAN_POINT ( 'NONE',  ( 0.5901948623465642640, 1.011764341257429978, -1.680720577067334354 ) ) ;
#32366 = CARTESIAN_POINT ( 'NONE',  ( 0.6823417656249864960, -0.5114583329919111243, -1.181850606188749264 ) ) ;
#32367 = CARTESIAN_POINT ( 'NONE',  ( -1.286956418854592332, 4.087185210396952151, 0.5511290012047664888 ) ) ;
#32368 = CARTESIAN_POINT ( 'NONE',  ( 6.174726448494309849, -2.051094451480539149, -0.6828207641706719455 ) ) ;
#32369 = CARTESIAN_POINT ( 'NONE',  ( -2.950870989268691957, 6.594433254122103349, -0.7998128361456281477 ) ) ;
#32370 = MECHANICAL_DESIGN_GEOMETRIC_PRESENTATION_REPRESENTATION (  '', ( #139542 ), #91154 ) ;
#32371 = CARTESIAN_POINT ( 'NONE',  ( -5.219525951136837705, 9.033271343060892633, -0.7216878364870207285 ) ) ;
#32372 = CARTESIAN_POINT ( 'NONE',  ( 5.418883921851007202, 1.995750516393671514, 0.8311057252617033431 ) ) ;
#32374 = ORIENTED_EDGE ( 'NONE', *, *, #73951, .F. ) ;
#32373 = DIRECTION ( 'NONE',  ( 0.000000000000000000, 0.000000000000000000, -1.000000000000000000 ) ) ;
#32375 = CARTESIAN_POINT ( 'NONE',  ( -1.201851678989727383E-14, 2.571875000341417472, 1.575800808251672791 ) ) ;
#32376 = CARTESIAN_POINT ( 'NONE',  ( 6.362572844203587152, -1.395794784517788045, 1.392370165595870679 ) ) ;
#32377 = CARTESIAN_POINT ( 'NONE',  ( 5.167242596723413683, -0.5858957144197572964, -1.632003580468445847 ) ) ;
#32379 = CARTESIAN_POINT ( 'NONE',  ( 1.716621854089026344, 2.046377219401524616, 0.7848826361863747714 ) ) ;
#32378 = CARTESIAN_POINT ( 'NONE',  ( -0.6801582343750074422, -0.8177083329919260235, 1.178068619123834759 ) ) ;
#32380 = CARTESIAN_POINT ( 'NONE',  ( 3.593080373992099119, -0.4475695053229776788, -2.263611109821815681 ) ) ;
#32381 = CARTESIAN_POINT ( 'NONE',  ( 4.499328421682089463, 1.652694973434418291, 1.230784805264173221 ) ) ;
#32382 = CARTESIAN_POINT ( 'NONE',  ( 0.6736475468689150370, -1.079418705485206020, 1.614127575861698416 ) ) ;
#32383 = CARTESIAN_POINT ( 'NONE',  ( -7.998947441938374148, 8.434452891790657603, 1.040834085586084257E-14 ) ) ;
#32385 = EDGE_CURVE ( 'NONE', #35700, #401, #22380, .T. ) ;
#32384 = CARTESIAN_POINT ( 'NONE',  ( -5.842637852846353397, 5.781108681267656202, 0.7998128361456281477 ) ) ;
#32386 = CARTESIAN_POINT ( 'NONE',  ( -9.608224291022223085, 14.88196956744644872, 7.189021211163121983 ) ) ;
#32387 = CARTESIAN_POINT ( 'NONE',  ( 3.867525618572264623, -1.764951123045129577, -1.175235903013646332 ) ) ;
#32388 = CARTESIAN_POINT ( 'NONE',  ( 0.8619541869999207684, -0.05229984143813663777, -2.015912905633105101 ) ) ;
#32389 = CARTESIAN_POINT ( 'NONE',  ( -5.490689023410187275, 8.389259046411751797, 1.082531754730548412 ) ) ;
#32390 = CARTESIAN_POINT ( 'NONE',  ( 4.313639225654395837, -0.3805011380913872476, 2.173570407251994574 ) ) ;
#32391 = CARTESIAN_POINT ( 'NONE',  ( 1.642778471875001811, -0.4302083328553765740, 2.845375778867859751 ) ) ;
#32392 = FACE_OUTER_BOUND ( 'NONE', #77688, .T. ) ;
#32393 = CARTESIAN_POINT ( 'NONE',  ( -5.589704470584107909, 9.743348658981940247, -0.7998128361456362523 ) ) ;
#32395 = DIRECTION ( 'NONE',  ( 0.000000000000000000, 0.000000000000000000, -1.000000000000000000 ) ) ;
#32394 = CARTESIAN_POINT ( 'NONE',  ( -5.628650723579520232, 7.468463085569896798, -1.343613510788654875 ) ) ;
#32396 = CARTESIAN_POINT ( 'NONE',  ( 0.3282377607281235510, 2.176335450315365350, -1.225000000000017408 ) ) ;
#32397 = ORIENTED_EDGE ( 'NONE', *, *, #124309, .T. ) ;
#32398 = CARTESIAN_POINT ( 'NONE',  ( 4.135659164760732587, -1.419885373862592726, -1.493960738838293389 ) ) ;
#32399 = CARTESIAN_POINT ( 'NONE',  ( 1.360316468749949825, 2.244791667008100511, 0.7853790794158780342 ) ) ;
#32400 = CARTESIAN_POINT ( 'NONE',  ( -5.687809136132860210, 6.594531066031826150, -1.199719254218446718 ) ) ;
#32401 = CARTESIAN_POINT ( 'NONE',  ( 3.317061382196756281, 1.590690956008104395, -1.244364558649863728 ) ) ;
#32402 = CARTESIAN_POINT ( 'NONE',  ( 1.499999999999985123, -0.7041666666666481778, -0.8660254037844323793 ) ) ;
#32403 = CARTESIAN_POINT ( 'NONE',  ( 10.54788032175191326, 11.40820791823982994, 0.7216878364870317197 ) ) ;
#32404 = CARTESIAN_POINT ( 'NONE',  ( 7.958799866421889746, 9.244020251369077457, -1.199719254218441611 ) ) ;
#32405 = CARTESIAN_POINT ( 'NONE',  ( 3.590745217537123057, -0.4003831998886059340, -2.021439917362640504 ) ) ;
#32406 = CARTESIAN_POINT ( 'NONE',  ( 1.214306433183764966E-14, 2.428612866367529932E-14, 1.500000000000001332 ) ) ;
#32407 = CARTESIAN_POINT ( 'NONE',  ( 5.331380718671758778, 7.243030143248949670, -1.599625672291256295 ) ) ;
#32408 = CARTESIAN_POINT ( 'NONE',  ( -0.2411972340276023752, 5.722880186377757639, -2.494559970919587588 ) ) ;
#32409 = CARTESIAN_POINT ( 'NONE',  ( 0.7965151530783078915, 1.503791256141374211, 1.061989520254283059 ) ) ;
#32410 = CARTESIAN_POINT ( 'NONE',  ( 6.551417122825020201, -1.769646310455678995, -1.318412661681533260 ) ) ;
#32411 = CARTESIAN_POINT ( 'NONE',  ( 4.701645408888975197, 8.707279753670952971, 0.000000000000000000 ) ) ;
#32412 = CARTESIAN_POINT ( 'NONE',  ( 1.511231465835579879, 1.905624552496063995, 1.020381674553122231 ) ) ;
#32413 = CARTESIAN_POINT ( 'NONE',  ( -3.551873057100300990, 5.166937871415542283, 1.443375672974064550 ) ) ;
#32414 = CARTESIAN_POINT ( 'NONE',  ( 2.466030083290056130, -1.032479112849067793, 1.731996155473938259 ) ) ;
#32415 = ADVANCED_FACE ( 'NONE', ( #19930 ), #83872, .F. ) ;
#32416 = CARTESIAN_POINT ( 'NONE',  ( 1.810362406828632365, -1.941531176516932522, 1.229804462443480295 ) ) ;
#32417 = AXIS2_PLACEMENT_3D ( 'NONE', #92406, #158445, #10045 ) ;
#32418 = CARTESIAN_POINT ( 'NONE',  ( 0.3736316133628528879, 1.073300769168658908, 1.531925686032776124 ) ) ;
#32419 = AXIS2_PLACEMENT_3D ( 'NONE', #31526, #143182, #128047 ) ;
#32420 = CARTESIAN_POINT ( 'NONE',  ( 5.084826545086224669, -0.2406546161831616404, -1.956650619579934469 ) ) ;
#32421 = CARTESIAN_POINT ( 'NONE',  ( 5.208220363674559650, 1.197307938467083055, -1.622483861274232719 ) ) ;
#32423 = DIRECTION ( 'NONE',  ( 0.000000000000000000, 0.000000000000000000, 1.000000000000000000 ) ) ;
#32422 = CARTESIAN_POINT ( 'NONE',  ( 1.364683531249988757, 2.134375000341422357, 1.214306433183764966E-14 ) ) ;
#32425 = CARTESIAN_POINT ( 'NONE',  ( 5.813134535821789406, 1.856751089961257373, 0.9939634876292826604 ) ) ;
#32424 = CARTESIAN_POINT ( 'NONE',  ( -5.391338639728555648, 9.441645512991978961, -0.7998128361456231517 ) ) ;
#32426 = VECTOR ( 'NONE', #114822, 1000.000000000000000 ) ;
#32427 = CARTESIAN_POINT ( 'NONE',  ( 6.654741963219192868, -0.5482099483974657295, -1.996413779700876301 ) ) ;
#32428 = CARTESIAN_POINT ( 'NONE',  ( 6.226218857173709154, 8.287007971501239467, 1.599625672291281386 ) ) ;
#32429 = CARTESIAN_POINT ( 'NONE',  ( -6.388916700537716764, 8.476822122092563916, 1.599625672291283607 ) ) ;
#32430 = CARTESIAN_POINT ( 'NONE',  ( 6.639320575229251453, 2.441375407831634536, 2.385816205380648203 ) ) ;
#32431 = CARTESIAN_POINT ( 'NONE',  ( 5.203380996274193038, 1.779418458119955915, -0.9556711282029080046 ) ) ;
#32432 = CARTESIAN_POINT ( 'NONE',  ( -1.500000000000013101, 0.9520833340161557468, 0.8660254037844403729 ) ) ;
#32433 = CARTESIAN_POINT ( 'NONE',  ( 3.844573663522454332, 2.296428955072826295, 0.2277027427845106922 ) ) ;
#32434 = CARTESIAN_POINT ( 'NONE',  ( 1.551709131853472368, 1.559248165652558082, 1.350213067335771511 ) ) ;
#32435 = CARTESIAN_POINT ( 'NONE',  ( 7.456621297836078632, 8.762108271306003004, 1.082531754730558626 ) ) ;
#32436 = CARTESIAN_POINT ( 'NONE',  ( 7.503511670520385479, 7.718794801887437274, 0.7998128361456281477 ) ) ;
#32437 = CARTESIAN_POINT ( 'NONE',  ( 4.362691568547328202, 8.311833606605697256, -0.7998128361456381397 ) ) ;
#32438 = CARTESIAN_POINT ( 'NONE',  ( -1.402160292154681736E-14, 0.2593750003414224681, -1.575800808251665908 ) ) ;
#32439 = CARTESIAN_POINT ( 'NONE',  ( 5.876533236880477240, 5.820653295974182129, 0.7998128361456352531 ) ) ;
#32440 = CARTESIAN_POINT ( 'NONE',  ( 5.436456408955479880, 9.286356877182658565, -0.7216878364870267237 ) ) ;
#32442 = CARTESIAN_POINT ( 'NONE',  ( -1.378881877344243945, 4.087185210397143109, 0.5904953584335903560 ) ) ;
#32441 = CARTESIAN_POINT ( 'NONE',  ( 4.264261594705793357, -2.165624863444326920, 0.1558643175220644772 ) ) ;
#32444 = CARTESIAN_POINT ( 'NONE',  ( 3.315785976855676775, 1.165629053876730659, -1.425327459889616177 ) ) ;
#32443 = CARTESIAN_POINT ( 'NONE',  ( -5.477130870240893401, 6.452702772444876445, 1.082531754730548412 ) ) ;
#32445 = CARTESIAN_POINT ( 'NONE',  ( 0.6823417656249899377, 4.926041667008086655, -1.181850606188754593 ) ) ;
#32446 = CARTESIAN_POINT ( 'NONE',  ( 4.265290774032561849, 2.125562838249666964, -0.5332280334861272397 ) ) ;
#32447 = CARTESIAN_POINT ( 'NONE',  ( 8.128354040209304188, 14.19343821084924961, 8.828530592764916918 ) ) ;
#32448 = CARTESIAN_POINT ( 'NONE',  ( 6.016560025881092066, 1.524636124814653382, -1.671835012792993735 ) ) ;
#32449 = FACE_OUTER_BOUND ( 'NONE', #179560, .T. ) ;
#32450 = CARTESIAN_POINT ( 'NONE',  ( 4.632842592818133376, 8.443130954262043630, -0.3954830847591808696 ) ) ;
#32451 = CARTESIAN_POINT ( 'NONE',  ( -4.950135482320914271, 8.789258806100786359, -0.7216878364870338292 ) ) ;
#32452 = CARTESIAN_POINT ( 'NONE',  ( 3.255366281057017197, 6.812028071292901998, -0.7216878364870338292 ) ) ;
#32453 = CARTESIAN_POINT ( 'NONE',  ( 6.485617131683707903, 1.222450955268041373, 1.279935727357548458 ) ) ;
#32454 = CARTESIAN_POINT ( 'NONE',  ( 3.668611300974702782, 0.7265845916090816203, 1.877559629772174166 ) ) ;
#32455 = CARTESIAN_POINT ( 'NONE',  ( 6.120616281565444794, 9.228137197546649517, -1.199719254218440723 ) ) ;
#32456 = CARTESIAN_POINT ( 'NONE',  ( 2.889785439676189505, 1.488280975668257344, 1.490260817651526182 ) ) ;
#32457 = CARTESIAN_POINT ( 'NONE',  ( 1.704550880262687640, 1.788078052428695219, 0.6877594758711459422 ) ) ;
#32458 = CARTESIAN_POINT ( 'NONE',  ( 4.871457266011829823, 4.577788319968905562, -0.7998128361456221525 ) ) ;
#32460 = EDGE_CURVE ( 'NONE', #205126, #1142, #73682, .T. ) ;
#32459 = CARTESIAN_POINT ( 'NONE',  ( 3.508217419976053630, 1.969739563948954331, 0.002549893942540777322 ) ) ;
#32461 = CARTESIAN_POINT ( 'NONE',  ( 4.869401706892690029, -1.708532917064720991, -1.076912495999365449 ) ) ;
#32462 = CARTESIAN_POINT ( 'NONE',  ( 0.7955152940811484052, -0.6771210053572243037, 1.743984199989514927 ) ) ;
#32463 = CARTESIAN_POINT ( 'NONE',  ( 0.9769180011504545735, 1.811320799089161993, 0.7541596914439269161 ) ) ;
#32464 = CARTESIAN_POINT ( 'NONE',  ( 0.3867804997886997720, -1.801505969789623629, -0.6421655129100201087 ) ) ;
#32465 = CARTESIAN_POINT ( 'NONE',  ( 5.843201017809841247, 5.919415396974013532, 1.040834085586084257E-14 ) ) ;
#32466 = CARTESIAN_POINT ( 'NONE',  ( -1.364683531250012516, 1.092708333674754506, 0.7879004041258379498 ) ) ;
#32467 = CARTESIAN_POINT ( 'NONE',  ( 6.192256348250350761, -1.861847689568534081, -0.1814220289034565448 ) ) ;
#32468 = CARTESIAN_POINT ( 'NONE',  ( 2.672702088255949078E-15, 1.625000000682787160, 1.224999999999980549 ) ) ;
#32469 = CARTESIAN_POINT ( 'NONE',  ( 6.983263157960365675, -0.006178392973848687020, 2.053544886540019210 ) ) ;
#32470 = CARTESIAN_POINT ( 'NONE',  ( 1.381394743813993964, -0.05274132383669553892, 2.069866178704109938 ) ) ;
#32471 = CARTESIAN_POINT ( 'NONE',  ( -1.201851678989727383E-14, 1.712500000000019229, 1.732050807568877637 ) ) ;
#32472 = CARTESIAN_POINT ( 'NONE',  ( 7.474622759835693131, 7.614814729430110951, -0.7998128361456281477 ) ) ;
#32473 = CARTESIAN_POINT ( 'NONE',  ( -8.365544474831901667, 9.718555627847388578, 1.199719254218462483 ) ) ;
#32474 = CARTESIAN_POINT ( 'NONE',  ( 6.527324610336440180, 6.579909898339485252, 0.7998128361456331437 ) ) ;
#32475 = CARTESIAN_POINT ( 'NONE',  ( 5.162787349232583090, 0.6159572760087471677, 2.029033592890214788 ) ) ;
#32476 = CARTESIAN_POINT ( 'NONE',  ( 4.492547798081839794, 6.334668079219206049, 1.599625672291262513 ) ) ;
#32477 = CARTESIAN_POINT ( 'NONE',  ( -1.201851678989727383E-14, 1.571875000341420581, 1.575800808251672791 ) ) ;
#32479 = EDGE_CURVE ( 'NONE', #102469, #141519, #35632, .T. ) ;
#32478 = CARTESIAN_POINT ( 'NONE',  ( -1.500000000000013101, 1.879166666666692187, -0.8660254037844313801 ) ) ;
#32481 = CARTESIAN_POINT ( 'NONE',  ( 4.253507506385319381, 5.985511395581417204, 1.599625672291267398 ) ) ;
#32480 = CARTESIAN_POINT ( 'NONE',  ( 6.180128940399614912, -1.088687182605744042, -1.631870318916525120 ) ) ;
#32482 = CARTESIAN_POINT ( 'NONE',  ( 4.446638634790680555, 1.314796391739966985, 1.528506369862133285 ) ) ;
#32483 = CARTESIAN_POINT ( 'NONE',  ( 3.239363768214057249, 0.4605203156026844158, -1.859431460922003509 ) ) ;
#32484 = CARTESIAN_POINT ( 'NONE',  ( -1.907519672996902838, 3.236073672982390903, -0.4612874649730039911 ) ) ;
#32485 = CARTESIAN_POINT ( 'NONE',  ( 1.575987392057216940, -1.168677030305173004, 1.853764812240476623 ) ) ;
#32486 = CARTESIAN_POINT ( 'NONE',  ( 0.3985077402203209274, -4.205987624083768139, -0.9999999999999993339 ) ) ;
#32487 = CARTESIAN_POINT ( 'NONE',  ( 3.479631686803522417, 1.184185218286455621, 1.448006030947253331 ) ) ;
#32488 = CARTESIAN_POINT ( 'NONE',  ( -0.7500000000000006661, -0.1104166659838465292, -1.299038105676652011 ) ) ;
#32489 = CARTESIAN_POINT ( 'NONE',  ( -8.345207244411405156, 9.694828859023472134, 1.199719254218462483 ) ) ;
#32491 = CARTESIAN_POINT ( 'NONE',  ( 5.659793223991267830, 1.261623160278273481, 1.700126385781860927 ) ) ;
#32490 = CARTESIAN_POINT ( 'NONE',  ( -3.131570295076647525, 6.597323077657299528, 1.040834085586084257E-14 ) ) ;
#32492 = LINE ( 'NONE', #81245, #49118 ) ;
#32493 = CYLINDRICAL_SURFACE ( 'NONE', #8475, 1.500000000000000222 ) ;
#32495 = CARTESIAN_POINT ( 'NONE',  ( -4.167236710886554896, 7.875866928964825320, -0.1619875888596494506 ) ) ;
#32494 = CARTESIAN_POINT ( 'NONE',  ( 2.103177918021365223, -0.4551342947399418248, 2.040444103505714146 ) ) ;
#32497 = VERTEX_POINT ( 'NONE', #86017 ) ;
#32496 = CARTESIAN_POINT ( 'NONE',  ( 1.289626238417174831, -0.7804147442260088718, 1.538193839892360471 ) ) ;
#32498 = CARTESIAN_POINT ( 'NONE',  ( 7.233438648090761980, 8.397765496649418182, 1.199719254218462483 ) ) ;
#32499 = CARTESIAN_POINT ( 'NONE',  ( 3.486133158594716510E-16, 2.437499999999986677, -1.225000000000021849 ) ) ;
#32500 = CARTESIAN_POINT ( 'NONE',  ( 0.000000000000000000, -6.583980363594976737, 0.000000000000000000 ) ) ;
#32501 = CARTESIAN_POINT ( 'NONE',  ( -1.436838838544753694, 7.449283400311743186, 4.203727439823589762 ) ) ;
#32503 = CARTESIAN_POINT ( 'NONE',  ( 10.04622863760192963, 10.82294762006482713, -0.7216878364870257245 ) ) ;
#32502 = CARTESIAN_POINT ( 'NONE',  ( 5.849453209292126310, 8.911780279894442103, 1.199719254218462483 ) ) ;
#32504 = CARTESIAN_POINT ( 'NONE',  ( -1.889772045536167067, 3.296949564223877083, 0.4024211290685098530 ) ) ;
#32506 = CARTESIAN_POINT ( 'NONE',  ( 2.086290463123147365, -1.113812826415590651, 1.428500571052490953 ) ) ;
#32505 = CARTESIAN_POINT ( 'NONE',  ( 5.017399365509065845, 8.011327138806002779, -1.199719254218450271 ) ) ;
#32507 = CARTESIAN_POINT ( 'NONE',  ( -7.640183256500752584, 8.872300873127729304, -1.199719254218446718 ) ) ;
#32508 = CARTESIAN_POINT ( 'NONE',  ( 4.222474775652216294, 7.013638773981186958, 1.199719254218462483 ) ) ;
#32509 = CARTESIAN_POINT ( 'NONE',  ( -5.955741603288206676, 7.127506980570093020, 1.099513196254948699 ) ) ;
#32510 = CARTESIAN_POINT ( 'NONE',  ( 5.224688093219824303, 7.188831756880171397, -1.599625672291283607 ) ) ;
#32511 = CARTESIAN_POINT ( 'NONE',  ( 6.639320575229251453, 2.090987163941595561, 2.106969785032047238 ) ) ;
#32512 = DIRECTION ( 'NONE',  ( 0.000000000000000000, 0.000000000000000000, -1.000000000000000000 ) ) ;
#32513 = CARTESIAN_POINT ( 'NONE',  ( -11.48784849554592924, 11.33049527181932348, 3.469614872287846374 ) ) ;
#32514 = CARTESIAN_POINT ( 'NONE',  ( 7.782016984564043227, 12.02284421539267356, 0.7216878364870438212 ) ) ;
#32515 = ORIENTED_EDGE ( 'NONE', *, *, #118802, .F. ) ;
#32516 = CARTESIAN_POINT ( 'NONE',  ( 3.121387120179277996, 0.2756568158089545695, -1.840403582779404745 ) ) ;
#32517 = CARTESIAN_POINT ( 'NONE',  ( 0.06975588353394339414, -0.9023057962903738849, 1.689756990376343859 ) ) ;
#32518 = CARTESIAN_POINT ( 'NONE',  ( 6.229514091203088633, -1.813738808949336478, 0.6494875524521417365 ) ) ;
#32519 = CARTESIAN_POINT ( 'NONE',  ( 5.951642636407408204, 1.565221049572671497, 1.355249363302114096 ) ) ;
#32520 = CARTESIAN_POINT ( 'NONE',  ( 7.785697387528199762E-15, 0.5624999999999894529, 1.224999999999973443 ) ) ;
#32521 = CARTESIAN_POINT ( 'NONE',  ( 4.622017735560743468, 8.339529265130579461, 0.3277269337885590494 ) ) ;
#32522 = CARTESIAN_POINT ( 'NONE',  ( -11.52460864928264961, 11.37999999999998302, 3.346683403123524858 ) ) ;
#32523 = CARTESIAN_POINT ( 'NONE',  ( -4.663641653420935285, 5.503632019488245319, 1.082531754730560403 ) ) ;
#32524 = CARTESIAN_POINT ( 'NONE',  ( 7.605760987586388744, 11.81721221891873697, 1.040834085586084257E-14 ) ) ;
#32525 = CARTESIAN_POINT ( 'NONE',  ( 4.434397634191796556, -1.137439385922611290, 1.607554744723362017 ) ) ;
#32526 = ADVANCED_FACE ( 'NONE', ( #184565 ), #153150, .F. ) ;
#32527 = CARTESIAN_POINT ( 'NONE',  ( 1.787894333202539654, 2.028250040683087008, -0.6185522307536188702 ) ) ;
#32528 = CARTESIAN_POINT ( 'NONE',  ( -4.557512192488103686, 8.468847991211438497, -0.7998128361456281477 ) ) ;
#32529 = CARTESIAN_POINT ( 'NONE',  ( 6.777182134110200096, 7.629137130509069387, 2.789055895399249696 ) ) ;
#32530 = CARTESIAN_POINT ( 'NONE',  ( 4.584065335196261692, 7.401807753487379848, 1.082531754730549078 ) ) ;
#32531 = CARTESIAN_POINT ( 'NONE',  ( 6.087848540548081999, -2.180536604488235941, -0.2183335821156970336 ) ) ;
#32532 = FILL_AREA_STYLE ('',( #14122 ) ) ;
#32533 = CARTESIAN_POINT ( 'NONE',  ( 4.032187520235196665, 1.031363847994439142, -1.626874456138996949 ) ) ;
#32534 = CARTESIAN_POINT ( 'NONE',  ( -5.669280788808708671, 9.765911353585494226, 0.7998128361456481317 ) ) ;
#32535 = EDGE_CURVE ( 'NONE', #144405, #53136, #96838, .T. ) ;
#32536 = CARTESIAN_POINT ( 'NONE',  ( 0.6569167496461197908, -1.539450689919025450, -0.9809549629347170674 ) ) ;
#32537 = CARTESIAN_POINT ( 'NONE',  ( 0.5752038918783763943, -2.079344756725898691, -0.7397341299467048437 ) ) ;
#32538 = ORIENTED_EDGE ( 'NONE', *, *, #101958, .T. ) ;
#32539 = ORIENTED_EDGE ( 'NONE', *, *, #210296, .T. ) ;
#32540 = CARTESIAN_POINT ( 'NONE',  ( 6.244967536942622743, -0.2852903188887367936, -1.948516424197583197 ) ) ;
#32541 = CARTESIAN_POINT ( 'NONE',  ( 1.698673089578231599, 1.615691133820891467, 1.077277171393706379 ) ) ;
#32542 = CARTESIAN_POINT ( 'NONE',  ( 6.309976275596433481, -1.946771231211348319, 1.221538734657970693 ) ) ;
#32544 = CARTESIAN_POINT ( 'NONE',  ( 5.119887769377023723, 1.841019424034021412, -0.2705144023524996277 ) ) ;
#32543 = CARTESIAN_POINT ( 'NONE',  ( -6.688968683495758683, 8.897159112202094988, -1.599625672291271394 ) ) ;
#32545 = CARTESIAN_POINT ( 'NONE',  ( 4.362691568547328202, 8.311833606605697256, -0.7998128361456381397 ) ) ;
#32546 = FILL_AREA_STYLE ('',( #99679 ) ) ;
#32547 = CARTESIAN_POINT ( 'NONE',  ( -5.555090253297260361, 7.504024600312024340, 1.599625672291269396 ) ) ;
#32548 = FACE_OUTER_BOUND ( 'NONE', #42243, .T. ) ;
#32549 = CARTESIAN_POINT ( 'NONE',  ( 1.892365914234435120, -0.5883382831698009685, -2.111031122750434808 ) ) ;
#32550 = CARTESIAN_POINT ( 'NONE',  ( 4.907688418466886304, 5.788353245375237321, -1.082531754730548412 ) ) ;
#32551 = ORIENTED_EDGE ( 'NONE', *, *, #21794, .T. ) ;
#32552 = CARTESIAN_POINT ( 'NONE',  ( 10.99622371251743225, -6.863149499369291640, -0.2970643657731165121 ) ) ;
#32553 = CARTESIAN_POINT ( 'NONE',  ( 11.41381675112453387, 10.19999999999999929, -3.704697986577184299 ) ) ;
#32554 = CARTESIAN_POINT ( 'NONE',  ( 1.312830284664792790, 1.609138963534262778, 0.8624270714618911260 ) ) ;
#32555 = CARTESIAN_POINT ( 'NONE',  ( -2.462777459176719308, 6.024990802348131780, -0.7998128361456281477 ) ) ;
#32556 = CARTESIAN_POINT ( 'NONE',  ( -6.462985781203115287, 6.858296038324478872, -0.6802466501308057634 ) ) ;
#32557 = CARTESIAN_POINT ( 'NONE',  ( -1.817608056788086346, 0.8389924079203545659, 1.022373108394139196 ) ) ;
#32558 = CARTESIAN_POINT ( 'NONE',  ( 1.423205080756849483, 7.980384757729337863, -10.65537363484302524 ) ) ;
#32559 = CARTESIAN_POINT ( 'NONE',  ( 6.199803715563785289, -0.6102442156579389598, 1.720816905678754782 ) ) ;
#32560 = CARTESIAN_POINT ( 'NONE',  ( 4.944172655442597097, -0.9282843415348587257, 1.728263438747808856 ) ) ;
#32561 = CARTESIAN_POINT ( 'NONE',  ( -7.178152263431422320, 10.46192917639026554, 1.199719254218453823 ) ) ;
#32562 = CARTESIAN_POINT ( 'NONE',  ( 6.124532705071213279, 8.168374127381657246, -1.599625672291262513 ) ) ;
#32563 = CARTESIAN_POINT ( 'NONE',  ( 5.039744756118590630, -2.013340025477545758, 0.6656774797743277849 ) ) ;
#32564 = CARTESIAN_POINT ( 'NONE',  ( 4.441096743985088580, -1.694418930461354611, -1.389946530008886905 ) ) ;
#32565 = AXIS2_PLACEMENT_3D ( 'NONE', #119250, #185234, #5400 ) ;
#32566 = CARTESIAN_POINT ( 'NONE',  ( -8.670602931139386627, 10.07445716020612103, 1.199719254218462483 ) ) ;
#32567 = DIRECTION ( 'NONE',  ( 0.000000000000000000, 0.000000000000000000, 1.000000000000000000 ) ) ;
#32568 = CARTESIAN_POINT ( 'NONE',  ( 2.430607852509637290, -1.277051959022021066, 1.629327859714514659 ) ) ;
#32570 = CARTESIAN_POINT ( 'NONE',  ( 1.364683531249988757, 0.1968750003414204697, 0.000000000000000000 ) ) ;
#32569 = CARTESIAN_POINT ( 'NONE',  ( -0.03952929641551498896, -5.422159130394869742, -11.00000000000004974 ) ) ;
#32572 = ORIENTED_EDGE ( 'NONE', *, *, #175320, .T. ) ;
#32571 = VECTOR ( 'NONE', #6899, 1000.000000000000114 ) ;
#32573 = CARTESIAN_POINT ( 'NONE',  ( 3.147439182535469726, 1.035885224147353512, 2.052142740569740109 ) ) ;
#32574 = CARTESIAN_POINT ( 'NONE',  ( 8.487040972474689582, 9.964264558384387627, -1.082531754730543083 ) ) ;
#32576 = CARTESIAN_POINT ( 'NONE',  ( -3.285556943750000070, -1.509374999522042238, 0.000000000000000000 ) ) ;
#32575 = CARTESIAN_POINT ( 'NONE',  ( 5.641601317062233001, 7.675230518029648508, -1.443375672974078761 ) ) ;
#32577 = CARTESIAN_POINT ( 'NONE',  ( 6.620655732516645742, 3.706282450693794139, 2.340867613974298767 ) ) ;
#32578 = CARTESIAN_POINT ( 'NONE',  ( -10.07315204383574070, 4.605425058967329122, -6.523384448309665906 ) ) ;
#32579 = CARTESIAN_POINT ( 'NONE',  ( 4.031144971506396502, -1.339966268285474715, -1.405800288483616045 ) ) ;
#32580 = EDGE_LOOP ( 'NONE', ( #187456, #182201, #113529, #66728 ) ) ;
#32581 = CARTESIAN_POINT ( 'NONE',  ( 0.07933191607487939667, -9.582912294610213877, 9.499668754598326714 ) ) ;
#32582 = CARTESIAN_POINT ( 'NONE',  ( 3.550944491985886575, 0.2853618425060593378, 1.890879049853078087 ) ) ;
#32583 = DIRECTION ( 'NONE',  ( 0.6483454320283800199, 0.000000000000000000, -0.7613463080411787542 ) ) ;
#32584 = CARTESIAN_POINT ( 'NONE',  ( 4.998908393266289885, 1.432429904705156520, -0.9603719661937599739 ) ) ;
#32585 = CARTESIAN_POINT ( 'NONE',  ( 3.344935638061694139, -1.780668040901035143, -0.9463001528628791625 ) ) ;
#32586 = CARTESIAN_POINT ( 'NONE',  ( 5.608098314261791728, -0.05969564267381716194, 2.298051806275173359 ) ) ;
#32587 = CARTESIAN_POINT ( 'NONE',  ( -1.500000000000001110, 9.770833333333333925, 0.8660254037844418162 ) ) ;
#32588 = CARTESIAN_POINT ( 'NONE',  ( 0.3818278861203865393, 2.057605126571937060, -0.7983354260262252033 ) ) ;
#32589 = CARTESIAN_POINT ( 'NONE',  ( -5.994113311017573054, 6.165756082374834079, 0.7216878364870257245 ) ) ;
#32590 = CARTESIAN_POINT ( 'NONE',  ( 6.010986587707961348, 1.561705629380090832, 0.8325338966498199156 ) ) ;
#32592 = CARTESIAN_POINT ( 'NONE',  ( 1.922231132759700589, 1.317440867170904362, -1.875679006090027690 ) ) ;
#32591 = CARTESIAN_POINT ( 'NONE',  ( 6.658989722967328717, 7.797851427330578566, 1.199719254218452935 ) ) ;
#32593 = B_SPLINE_CURVE_WITH_KNOTS ( 'NONE', 3,
 ( #158107, #56327, #157040, #172218 ),
 .UNSPECIFIED., .F., .F.,
 ( 4, 4 ),
 ( 0.000000000000000000, 0.0005811582027346231649 ),
 .UNSPECIFIED. ) ;
#32594 = CARTESIAN_POINT ( 'NONE',  ( 0.7259949354544228406, 0.1236639744153274628, 1.736007293746767655 ) ) ;
#32595 = CARTESIAN_POINT ( 'NONE',  ( -7.014364370223741929, 9.276787413384745662, -1.599625672291271394 ) ) ;
#32596 = CARTESIAN_POINT ( 'NONE',  ( -11.33772463945036968, 12.69999999999999929, -3.600000000000000977 ) ) ;
#32597 = CARTESIAN_POINT ( 'NONE',  ( -6.563028877466991595, 9.814561569423593923, 1.199719254218452935 ) ) ;
#32598 = CARTESIAN_POINT ( 'NONE',  ( -7.511572993685796537E-15, 0.3593750003414036831, -1.570758158831792262 ) ) ;
#32599 = CARTESIAN_POINT ( 'NONE',  ( 11.33772463945037146, 10.89999999999998259, 3.679999999999999272 ) ) ;
#32600 = CARTESIAN_POINT ( 'NONE',  ( 1.012457490462664644, 2.168662962709181574, -0.1065306264821704596 ) ) ;
#32601 = CARTESIAN_POINT ( 'NONE',  ( 2.501185699981960830, -0.1928336239410358699, 2.007256303757164240 ) ) ;
#32602 = CARTESIAN_POINT ( 'NONE',  ( -1.402160292154681736E-14, 0.3687500006828169363, -1.732050807568870754 ) ) ;
#32603 = CARTESIAN_POINT ( 'NONE',  ( 5.250583079984638246, 0.5609921762826737268, 1.843012466491249723 ) ) ;
#32604 = CARTESIAN_POINT ( 'NONE',  ( -1.402160292154681736E-14, 12.42187500034139802, 1.575800808251682339 ) ) ;
#32605 = CARTESIAN_POINT ( 'NONE',  ( 2.303257990033405367, -0.3847559998488152000, -2.187706203110438175 ) ) ;
#32606 = ORIENTED_EDGE ( 'NONE', *, *, #189930, .F. ) ;
#32607 = CARTESIAN_POINT ( 'NONE',  ( -4.094037528094973233, 3.811616672697257346, 2.445516385416635963 ) ) ;
#32608 = CARTESIAN_POINT ( 'NONE',  ( 0.000000000000000000, 3.500000000000003109, 0.000000000000000000 ) ) ;
#32609 = CARTESIAN_POINT ( 'NONE',  ( 8.971744963941056028, 11.49012176272984931, 1.599625672291281386 ) ) ;
#32610 = CARTESIAN_POINT ( 'NONE',  ( 5.073663595168481422, -0.9608294848038684277, 1.450969404730037660 ) ) ;
#32611 = CARTESIAN_POINT ( 'NONE',  ( 3.068751266904270025, 1.422870340827029345, -1.350941015047700366 ) ) ;
#32613 = CARTESIAN_POINT ( 'NONE',  ( -6.561783159334130922, 9.638868871656395498, -1.082531754730538864 ) ) ;
#32612 = CARTESIAN_POINT ( 'NONE',  ( 5.009901455449552010, 5.803638771901306725, -1.199719254218452047 ) ) ;
#32614 = DIRECTION ( 'NONE',  ( 0.000000000000000000, 1.000000000000000000, 0.000000000000000000 ) ) ;
#32615 = CARTESIAN_POINT ( 'NONE',  ( 4.657670937300908420, 0.5017462980881717272, -2.205921056424357651 ) ) ;
#32616 = CARTESIAN_POINT ( 'NONE',  ( 0.7134213396373456639, -1.741552128810987421, -1.105017490550715742 ) ) ;
#32617 = CARTESIAN_POINT ( 'NONE',  ( -6.235860587281615075, 9.362588887548838557, -1.199719254218440723 ) ) ;
#32618 = CARTESIAN_POINT ( 'NONE',  ( -4.270455198180246548, 4.084545274072787890, 0.7216878364870317197 ) ) ;
#32619 = VECTOR ( 'NONE', #21453, 1000.000000000000000 ) ;
#32620 = CARTESIAN_POINT ( 'NONE',  ( 1.903560677580185656, 1.881515123832262715, 1.256258119677531315 ) ) ;
#32621 = ORIENTED_EDGE ( 'NONE', *, *, #134538, .F. ) ;
#32622 = CARTESIAN_POINT ( 'NONE',  ( -1.500000000000015099, 1.160416667349484898, -0.8660254037844313801 ) ) ;
#32623 = CARTESIAN_POINT ( 'NONE',  ( 2.231529376059933956, -1.218349341866202362, -1.419469154777988296 ) ) ;
#32624 = CARTESIAN_POINT ( 'NONE',  ( 1.705275228087951955, 1.618143048327233435, 0.6241232001420042863 ) ) ;
#32625 = CARTESIAN_POINT ( 'NONE',  ( 5.671465802443460547, 1.304529079428708549, 1.760837017921567771 ) ) ;
#32626 = CARTESIAN_POINT ( 'NONE',  ( 6.704155097142892927, -2.307279366673311127, 0.04705588035085367382 ) ) ;
#32627 = CARTESIAN_POINT ( 'NONE',  ( 1.288041055883992536, -0.9272951443832450069, 1.840570288256936804 ) ) ;
#32628 = CARTESIAN_POINT ( 'NONE',  ( 4.259667731375265554, 0.9167342216760937523, 1.711951518900257430 ) ) ;
#32629 = CARTESIAN_POINT ( 'NONE',  ( -2.765500147063310266, 6.170241238308400433, 1.040834085586084257E-14 ) ) ;
#32630 = AXIS2_PLACEMENT_3D ( 'NONE', #91669, #76448, #142555 ) ;
#32631 = CARTESIAN_POINT ( 'NONE',  ( 6.573518820989788125, 1.789947451694914982, -0.5432430119688207437 ) ) ;
#32632 = CARTESIAN_POINT ( 'NONE',  ( 1.500000000000001110, -8.632537233970167800E-14, -2.052068128417951165 ) ) ;
#32633 = EDGE_CURVE ( 'NONE', #151743, #109340, #142994, .T. ) ;
#32634 = CARTESIAN_POINT ( 'NONE',  ( 4.073938026035560434, 7.494178044256873505, -0.5588469191320240004 ) ) ;
#32635 = CARTESIAN_POINT ( 'NONE',  ( 6.520861224751243412, 2.010896128390584625, -0.1455136175190149816 ) ) ;
#32636 = CARTESIAN_POINT ( 'NONE',  ( 1.360316468749973584, 0.7864583336747016373, -0.7853790794159161148 ) ) ;
#32637 = CARTESIAN_POINT ( 'NONE',  ( 6.100232455412330168, -0.2440331339308223768, 2.001510902166554473 ) ) ;
#32638 = CARTESIAN_POINT ( 'NONE',  ( -8.618179199781044630, 13.20629283305325963, 0.7998128361456341429 ) ) ;
#32639 = CARTESIAN_POINT ( 'NONE',  ( 6.598014311344812199, 10.84943379654430906, 1.040834085586084257E-14 ) ) ;
#32640 = CARTESIAN_POINT ( 'NONE',  ( 3.067887898442204442, 6.801229324816399746, 0.7998128361456271485 ) ) ;
#32642 = PRESENTATION_STYLE_ASSIGNMENT (( #83513 ) ) ;
#32641 = CARTESIAN_POINT ( 'NONE',  ( 2.560947663861262491, -1.588335953301520220, -0.9000364273514869229 ) ) ;
#32643 = CARTESIAN_POINT ( 'NONE',  ( -0.1296875068448125334, 4.095146142119266308, -2.381513845672214913 ) ) ;
#32644 = ORIENTED_EDGE ( 'NONE', *, *, #20109, .T. ) ;
#32645 = CARTESIAN_POINT ( 'NONE',  ( -5.600926855776894975, 6.667407765562058053, -1.082531754730549967 ) ) ;
#32646 = CARTESIAN_POINT ( 'NONE',  ( 3.285556943750000514, -3.551041666188707424, 1.896917185911906500 ) ) ;
#32647 = CARTESIAN_POINT ( 'NONE',  ( -7.648771216403934758, 12.07531685244661723, -0.7998128361456291469 ) ) ;
#32648 = CARTESIAN_POINT ( 'NONE',  ( 0.3518269803744868418, -1.431374087835567632, -1.425298768015555551 ) ) ;
#32649 = CARTESIAN_POINT ( 'NONE',  ( 6.568989397875739655, -1.719265429537725431, 1.406094356362475706 ) ) ;
#32650 = ORIENTED_EDGE ( 'NONE', *, *, #27143, .F. ) ;
#32651 = CARTESIAN_POINT ( 'NONE',  ( -4.925354943514475003, 8.968274210734028529, 0.000000000000000000 ) ) ;
#32652 = CARTESIAN_POINT ( 'NONE',  ( 5.515469562660962666, 5.329135999392899947, 0.7998128361456341429 ) ) ;
#32653 = CARTESIAN_POINT ( 'NONE',  ( 6.789916310432966284, -0.8843476597930698402, 1.859958747594625317 ) ) ;
#32654 = CARTESIAN_POINT ( 'NONE',  ( 4.992814645674491736, -2.006446365708704160, 0.2004330516618065550 ) ) ;
#32655 = EDGE_LOOP ( 'NONE', ( #115956, #113285, #195009, #23475 ) ) ;
#32656 = DIRECTION ( 'NONE',  ( 0.000000000000000000, 0.000000000000000000, -1.000000000000000000 ) ) ;
#32657 = CARTESIAN_POINT ( 'NONE',  ( 6.481679955784983349, 9.719654494127929922, -1.199719254218452047 ) ) ;
#32660 = ORIENTED_EDGE ( 'NONE', *, *, #6374, .T. ) ;
#32659 = CARTESIAN_POINT ( 'NONE',  ( 1.499999999999990896, 8.627523663848661428, -2.579999999999989413 ) ) ;
#32658 = CARTESIAN_POINT ( 'NONE',  ( -4.956387674247580755, 7.940146832334256111, 1.199719254218452935 ) ) ;
#32661 = CARTESIAN_POINT ( 'NONE',  ( 6.493754380866193721, 6.839952184459461293, 0.5864284347954504817 ) ) ;
#32662 = CARTESIAN_POINT ( 'NONE',  ( 4.956407584168041502, 1.492027487219639514, 1.356091576722208369 ) ) ;
#32663 = CARTESIAN_POINT ( 'NONE',  ( 4.857273802806507668, 1.820629801081237620, -0.2732171615176108848 ) ) ;
#32664 = CARTESIAN_POINT ( 'NONE',  ( -0.7641400526929537085, -4.157144623729230659, -0.6764706046374679982 ) ) ;
#32665 = CARTESIAN_POINT ( 'NONE',  ( 3.668876216774307863, -1.550535085938867352, 1.709345553852769095 ) ) ;
#32666 = CARTESIAN_POINT ( 'NONE',  ( 6.261886844665240481, 8.398896966899865646, 1.599625672291268286 ) ) ;
#32667 = CARTESIAN_POINT ( 'NONE',  ( 5.518883860308030798, 1.994880785013030788, 0.8329173350848093627 ) ) ;
#32668 = CARTESIAN_POINT ( 'NONE',  ( 6.109920781252839994, 10.27999134477033216, 1.040834085586084257E-14 ) ) ;
#32669 = CARTESIAN_POINT ( 'NONE',  ( 0.6966983018150345597, 1.588492033560371830, 1.117026046969020303 ) ) ;
#32670 = ADVANCED_FACE ( 'NONE', ( #40483 ), #139726, .T. ) ;
#32671 = CARTESIAN_POINT ( 'NONE',  ( -4.460796234096120472, 5.163016013655583158, 1.199719254218462483 ) ) ;
#32672 = ORIENTED_EDGE ( 'NONE', *, *, #177588, .T. ) ;
#32673 = EDGE_CURVE ( 'NONE', #77529, #123242, #174766, .T. ) ;
#32674 = CARTESIAN_POINT ( 'NONE',  ( -9.404345922919858936, 15.50976053221675599, -7.453791880891735389 ) ) ;
#32675 = CARTESIAN_POINT ( 'NONE',  ( -4.842197138736131556, 5.678260079060780008, 1.199719254218452935 ) ) ;
#32676 = CLOSED_SHELL ( 'NONE', ( #134755, #169434, #75205, #197107, #33036, #66139, #173474, #206242, #14385, #198198, #46146, #81158, #94222, #214049, #24176, #10376, #135408, #152018, #143141, #192819, #35568, #21012, #175193, #157787, #101103, #145317, #55827, #163490, #86239, #36249, #125288, #55927, #74771, #133060, #169204, #197622, #77868, #116367, #141351, #169296, #143536, #7720, #186074, #46551, #115007, #105592, #198182, #86694, #149381, #98352, #60652, #30072, #185816, #95835, #61220, #16025, #10478, #120967, #189006, #48566, #87889, #86095, #7322, #136503, #185241, #162075, #154563, #55200, #146262, #150547, #135185, #143583, #39677, #101631, #40567, #146365, #202610, #1037, #151177, #34286, #76119, #213132, #60799, #43714, #190216, #9062, #2404, #111806, #15532, #98770, #147970, #99019, #145158, #114086, #136888, #22947, #15900, #113029, #70312, #100155, #25342, #146775, #212553, #172902, #163756, #105052, #191869, #60737, #196848, #121375, #106360, #72370, #111664, #65706, #171225, #196354, #50792, #186082, #128748, #27695, #39092, #173118, #180544, #50933, #140161, #66312, #40584, #170192, #69155, #30374, #47427, #27868, #165716, #143840, #146923, #175851, #10427, #12269, #36362, #121529, #22375, #68069, #138807, #126979, #209951, #93174, #181100, #150077, #87990, #120289, #133288, #208777, #93262, #189039, #72107, #96551, #70585, #144802, #31013, #83439, #22259, #177060, #203686, #155273, #32124, #203276, #73844, #73824, #44794, #49779, #59695, #67434, #64700, #173700, #18346, #700, #47594, #67615, #83397, #130489, #143171, #16928, #131070, #154453, #93398, #64653, #149288, #10546, #44536, #149471, #166168, #85012, #166422, #145987, #190768, #164824, #97191, #195777, #81120, #28542, #92742, #138008, #78549, #104042, #4062, #143974, #33077, #123133, #152840, #174852, #100264, #83027, #134672, #6508, #12661, #129857, #34373, #110536, #212203, #122460, #14322, #121705, #162137, #149566, #203343, #162916, #167196, #131555, #160853, #133311, #42805, #168286, #148360, #7162, #147303, #39361, #92686, #195279, #116428, #101222, #105167, #180011, #53360, #121612, #104148, #202720, #138556, #79919, #209118, #103616, #203116, #36680, #81679, #54371, #114357, #38413, #36230, #112278, #38177, #32670, #130424, #69419, #79880, #68434, #156833, #55407, #74008, #102261, #124045, #76215, #130902, #183529, #40612, #27512, #95314, #187021, #182283, #169250, #23143, #44223, #57608, #43267, #97754, #176115, #57047, #91304 ) ) ;
#32677 = CARTESIAN_POINT ( 'NONE',  ( 3.010468980803046257, 1.356049738124785353, -1.288842618233053683 ) ) ;
#32680 = CARTESIAN_POINT ( 'NONE',  ( -4.925354943514475003, 8.968274210734028529, 0.000000000000000000 ) ) ;
#32679 = CARTESIAN_POINT ( 'NONE',  ( -1.201851678989727383E-14, 0.7437500006828187127, 1.732050807568877637 ) ) ;
#32678 = CARTESIAN_POINT ( 'NONE',  ( 1.722773492080275748, 1.414811824084385661, -1.286832238068566392 ) ) ;
#32681 = CARTESIAN_POINT ( 'NONE',  ( 2.596532132193625664, -2.201043451360765957, -0.1612727490639675743 ) ) ;
#32682 = CARTESIAN_POINT ( 'NONE',  ( -1.566597853259662276, 8.754643479813401186, -2.463935000415734322 ) ) ;
#32683 = CARTESIAN_POINT ( 'NONE',  ( 3.460355519985863548, 5.060167411448709629, 1.599625672291267398 ) ) ;
#32684 = CARTESIAN_POINT ( 'NONE',  ( 6.848276988234151652, 7.162280372460873679, -0.7216878364870317197 ) ) ;
#32685 = CARTESIAN_POINT ( 'NONE',  ( -4.959585264500673496, 4.680604318205876524, 1.214306433183764966E-14 ) ) ;
#32686 = CARTESIAN_POINT ( 'NONE',  ( -5.763624699140868834, 9.738329559057408602, -0.7216878364870338292 ) ) ;
#32687 = CARTESIAN_POINT ( 'NONE',  ( 0.5265599218138971027, 1.885207356905926668, 0.5763402985480212681 ) ) ;
#32688 = CARTESIAN_POINT ( 'NONE',  ( 1.677271382912606246, -2.191714306423699021, -0.7221938283701042627 ) ) ;
#32689 = CARTESIAN_POINT ( 'NONE',  ( 1.767943819387544968, -1.947426213878332035, 0.2369139692007388165 ) ) ;
#32690 = CARTESIAN_POINT ( 'NONE',  ( 5.330950330247254065, -1.940297947978512960, -0.6998911787638012472 ) ) ;
#32691 = CARTESIAN_POINT ( 'NONE',  ( 5.843201017809841247, 5.919415396974013532, 1.040834085586084257E-14 ) ) ;
#32692 = CARTESIAN_POINT ( 'NONE',  ( 5.855142236255289845, 7.924361590421551860, -1.599625672291281386 ) ) ;
#32693 = ORIENTED_EDGE ( 'NONE', *, *, #148616, .T. ) ;
#32694 = CARTESIAN_POINT ( 'NONE',  ( -0.6823417656249969321, 4.280208333674755394, -1.181850606188749264 ) ) ;
#32695 = CARTESIAN_POINT ( 'NONE',  ( 10.87798840695972657, -6.646059016331632208, -0.1412570932017882808 ) ) ;
#32696 = CARTESIAN_POINT ( 'NONE',  ( 3.782361668088245921, 6.396210465202840645, -1.082531754730548412 ) ) ;
#32697 = CARTESIAN_POINT ( 'NONE',  ( 1.323347942641838415, -1.961697495959934479, -0.9305402519725998189 ) ) ;
#32699 = CARTESIAN_POINT ( 'NONE',  ( 6.550350952284553330, -1.418464805562440922, 1.173678288350611609 ) ) ;
#32698 = DIRECTION ( 'NONE',  ( -0.1510067114093955887, 0.000000000000000000, 0.9885327375000383388 ) ) ;
#32700 = DIRECTION ( 'NONE',  ( 0.000000000000000000, -1.000000000000000000, 0.000000000000000000 ) ) ;
#32701 = CARTESIAN_POINT ( 'NONE',  ( -7.728718841570993092, -6.124285368609180047, 7.728718841571021514 ) ) ;
#32702 = CARTESIAN_POINT ( 'NONE',  ( 1.405301488743180061, -0.4598193086536165319, 1.813012767170335993 ) ) ;
#32703 = CARTESIAN_POINT ( 'NONE',  ( 5.606754022945427351, 1.640879930231559758, -1.407263238018638507 ) ) ;
#32704 = CARTESIAN_POINT ( 'NONE',  ( -5.988731108142371085, 6.089685199429741402, 0.6933981374793452002 ) ) ;
#32705 = FILL_AREA_STYLE_COLOUR ( '', #172428 ) ;
#32706 = EDGE_CURVE ( 'NONE', #94850, #156724, #213031, .T. ) ;
#32707 = CARTESIAN_POINT ( 'NONE',  ( 0.6823417656249917140, 5.155208333674749177, 1.181850606188765695 ) ) ;
#32708 = CARTESIAN_POINT ( 'NONE',  ( 1.260255548581414642, 1.910129771108992625, 0.09294656408432439010 ) ) ;
#32709 = CARTESIAN_POINT ( 'NONE',  ( 3.467426238747231881, 1.726840169280913662, -0.3869839817904097701 ) ) ;
#32710 = CARTESIAN_POINT ( 'NONE',  ( 0.7328884408557728714, 1.767063509844998492, 0.7314339715377634610 ) ) ;
#32712 = CARTESIAN_POINT ( 'NONE',  ( 5.185127790529111991, 1.568658432645179124, 1.099198482053822534 ) ) ;
#32711 = CARTESIAN_POINT ( 'NONE',  ( 1.528150327639969719, -3.232243495192087757, 2.908546201585544999 ) ) ;
#32713 = CARTESIAN_POINT ( 'NONE',  ( 6.109808257530946918, 0.5734047718448382902, -1.884209069281018500 ) ) ;
#32714 = CARTESIAN_POINT ( 'NONE',  ( -1.001543065824772872E-14, 4.712500000000017231, 1.732050807568877637 ) ) ;
#32715 = CARTESIAN_POINT ( 'NONE',  ( 1.441811196653530747, -1.994930912159533332, 0.7194735443712959588 ) ) ;
#32716 = CARTESIAN_POINT ( 'NONE',  ( 2.609770642201842072, -0.3830433331901555993, -0.1872689674646474400 ) ) ;
#32717 = CARTESIAN_POINT ( 'NONE',  ( 4.487079325084206260, 1.670935625628103605, -0.8411387520786617333 ) ) ;
#32719 = VERTEX_POINT ( 'NONE', #171527 ) ;
#32718 = CARTESIAN_POINT ( 'NONE',  ( 0.8030139110496161692, 1.490934425176414502, 1.053415343471690857 ) ) ;
#32721 = CARTESIAN_POINT ( 'NONE',  ( 1.499999999999990896, 4.275000000000021672, 1.214306433183764966E-14 ) ) ;
#32720 = CARTESIAN_POINT ( 'NONE',  ( 4.213639274598267370, -0.3785452818781535611, 2.174016619501429215 ) ) ;
#32722 = CARTESIAN_POINT ( 'NONE',  ( -1.364683531250012516, 5.051041667008085767, -0.7879004041258300672 ) ) ;
#32723 = CARTESIAN_POINT ( 'NONE',  ( 1.574752048370867907, 1.386759265612296455, -1.527078818449955966 ) ) ;
#32724 = CARTESIAN_POINT ( 'NONE',  ( 5.636439174979242850, 7.598931675607687453, -1.599625672291262513 ) ) ;
#32726 = CARTESIAN_POINT ( 'NONE',  ( -8.365544474831901667, 9.718555627847388578, 1.199719254218462483 ) ) ;
#32725 = VECTOR ( 'NONE', #62122, 1000.000000000000114 ) ;
#32727 = LINE ( 'NONE', #180056, #22943 ) ;
#32728 = CARTESIAN_POINT ( 'NONE',  ( 8.594979316059474073, 12.11489407112305372, 1.199719254218450271 ) ) ;
#32729 = CARTESIAN_POINT ( 'NONE',  ( -3.424353449663152027, -0.02084536078685375604, -0.4190369511457813223 ) ) ;
#32730 = FACE_OUTER_BOUND ( 'NONE', #101919, .T. ) ;
#32731 = ORIENTED_EDGE ( 'NONE', *, *, #61327, .T. ) ;
#32732 = CARTESIAN_POINT ( 'NONE',  ( 4.668459276380106715, -0.8822503692092443783, -1.873099891353036561 ) ) ;
#32734 = CARTESIAN_POINT ( 'NONE',  ( 1.364683531249986537, -0.8239583329919186738, 0.7879004041258500513 ) ) ;
#32733 = AXIS2_PLACEMENT_3D ( 'NONE', #80411, #68396, #199466 ) ;
#32735 = CARTESIAN_POINT ( 'NONE',  ( 1.001511639980020130, 1.766541945284912263, 1.245431700958275600 ) ) ;
#32736 = CARTESIAN_POINT ( 'NONE',  ( -6.127277117991962285, 7.006264510460848527, -0.9572512136472415278 ) ) ;
#32737 = CARTESIAN_POINT ( 'NONE',  ( 2.508468462390922138, -2.014426205243079693, -0.1462163075645859234 ) ) ;
#32738 = CARTESIAN_POINT ( 'NONE',  ( 5.097642140193346272, 6.530873256209153155, -1.245904388912087324 ) ) ;
#32739 = VERTEX_POINT ( 'NONE', #187769 ) ;
#32740 = EDGE_CURVE ( 'NONE', #36910, #71609, #60755, .T. ) ;
#32742 = CARTESIAN_POINT ( 'NONE',  ( 8.948018195339340508, 9.541702104091804415, -0.7216878364870197293 ) ) ;
#32741 = CARTESIAN_POINT ( 'NONE',  ( 1.737499999999999378, -2.916666666666668295, -3.009438278150925683 ) ) ;
#32743 = CARTESIAN_POINT ( 'NONE',  ( 0.06970559732634250272, 14.49275370307429078, 11.99964040566942636 ) ) ;
#32744 = CARTESIAN_POINT ( 'NONE',  ( 0.4445464637146989695, -1.457232572767804379, 1.394089106691732693 ) ) ;
#32745 = CARTESIAN_POINT ( 'NONE',  ( 5.442994344319362021, -1.727133847215430729, -1.348975639928217118 ) ) ;
#32746 = AXIS2_PLACEMENT_3D ( 'NONE', #18418, #83423, #33615 ) ;
#32747 = CARTESIAN_POINT ( 'NONE',  ( -1.201851678989727383E-14, 3.868750000682817713, -1.732050807568863648 ) ) ;
#32748 = CARTESIAN_POINT ( 'NONE',  ( 3.691585721427274702, 1.799035686688513325, -0.6489376663148455071 ) ) ;
#32749 = CARTESIAN_POINT ( 'NONE',  ( -4.334856428067329404, 6.080418470877079429, -1.599625672291256295 ) ) ;
#32750 = CARTESIAN_POINT ( 'NONE',  ( 2.995988758495615745, 6.439144618312774959, -0.7216878364870267237 ) ) ;
#32752 = CARTESIAN_POINT ( 'NONE',  ( 1.810172953844836341, 1.158670025852935437, -1.650096248209935945 ) ) ;
#32751 = CARTESIAN_POINT ( 'NONE',  ( -9.449669878600616357, 12.04770082983265844, -1.443375672974058777 ) ) ;
#32753 = CARTESIAN_POINT ( 'NONE',  ( 1.364683531249996529, 12.77604166700806587, 0.7879004041258405033 ) ) ;
#32755 = CARTESIAN_POINT ( 'NONE',  ( -8.100070429521727178, 8.414780020722290033, 0.7998128361456341429 ) ) ;
#32754 = CARTESIAN_POINT ( 'NONE',  ( 0.2930494462585155335, 1.901387222806522503, -1.280258756811911702 ) ) ;
#32756 = CARTESIAN_POINT ( 'NONE',  ( 3.838627834895870450, 0.2530714650476103555, 1.705954220825799617 ) ) ;
#32757 = CARTESIAN_POINT ( 'NONE',  ( -0.1399997263889820043, 5.722209607272843002, -2.594334538518060729 ) ) ;
#32758 = CARTESIAN_POINT ( 'NONE',  ( 3.765413976293345844, 5.416068943807445635, 1.599625672291267398 ) ) ;
#32759 = CARTESIAN_POINT ( 'NONE',  ( 0.000000000000000000, 1.000000000000000888, 0.000000000000000000 ) ) ;
#32760 =( BOUNDED_CURVE ( )  B_SPLINE_CURVE ( 3, ( #138442, #56114, #91838, #208739 ),
 .UNSPECIFIED., .F., .T. ) 
 B_SPLINE_CURVE_WITH_KNOTS ( ( 4, 4 ),
 ( 0.000000000000000000, 0.5000000000000027756 ),
 .UNSPECIFIED. ) 
 CURVE ( )  GEOMETRIC_REPRESENTATION_ITEM ( )  RATIONAL_B_SPLINE_CURVE ( ( 1.000000000000000000, 0.3333333333333296511, 0.3333333333333333703, 1.000000000000003775 ) ) 
 REPRESENTATION_ITEM ( '' )  );
#32761 = ADVANCED_FACE ( 'NONE', ( #7949 ), #161870, .T. ) ;
#32762 = CARTESIAN_POINT ( 'NONE',  ( 0.3911966820569385828, 1.383097094795827209, 1.259704262696823118 ) ) ;
#32763 = CARTESIAN_POINT ( 'NONE',  ( 4.542145155778077203, 5.257923088951247159, -1.199719254218452047 ) ) ;
#32764 = CARTESIAN_POINT ( 'NONE',  ( 0.07516593201273641389, 2.869485459350088696, -2.532657826882792840 ) ) ;
#32765 = EDGE_LOOP ( 'NONE', ( #67711, #147045, #158950, #208148, #37988, #202252 ) ) ;
#32766 = CARTESIAN_POINT ( 'NONE',  ( 0.3212534483023680165, -1.847719145540312358, -0.9339786784923130858 ) ) ;
#32767 = ORIENTED_EDGE ( 'NONE', *, *, #82056, .F. ) ;
#32768 = CARTESIAN_POINT ( 'NONE',  ( 5.514259914679787045, -1.811656974672648746, 0.006318095929410197376 ) ) ;
#32769 = ORIENTED_EDGE ( 'NONE', *, *, #168266, .T. ) ;
#32770 = CARTESIAN_POINT ( 'NONE',  ( 6.042093733545556233, 7.078139439671806699, -1.199719254218452047 ) ) ;
#32771 = CARTESIAN_POINT ( 'NONE',  ( 7.253312916980309666, -6.796015482748904546, -7.253312916980335423 ) ) ;
#32772 = CARTESIAN_POINT ( 'NONE',  ( 5.918593472536316291, -0.6585524616501952089, -1.687715565691887187 ) ) ;
#32773 = CARTESIAN_POINT ( 'NONE',  ( 6.848276988234151652, 7.162280372460873679, -0.7216878364870317197 ) ) ;
#32774 = CARTESIAN_POINT ( 'NONE',  ( -11.84668730067608422, 10.19999999999999929, -1.400000000000001688 ) ) ;
#32775 = CARTESIAN_POINT ( 'NONE',  ( 2.484552680892829546, -0.3758780662847274190, -2.158817762932266682 ) ) ;
#32776 = ORIENTED_EDGE ( 'NONE', *, *, #115310, .T. ) ;
#32778 = CARTESIAN_POINT ( 'NONE',  ( 10.05067194643221207, 10.62020544712608938, 0.7998128361456462443 ) ) ;
#32777 = CARTESIAN_POINT ( 'NONE',  ( 6.654761307663171976, -0.4979203083825957110, -1.793151784937331961 ) ) ;
#32779 = CARTESIAN_POINT ( 'NONE',  ( 3.937047882288559286, -1.594636078160330150, -1.061121380078999143 ) ) ;
#32780 = DIRECTION ( 'NONE',  ( -1.000000000000000000, 5.578564026256490882E-16, 2.058387550816952846E-48 ) ) ;
#32781 = COLOUR_RGB ( '', 0.72549020, 0.75294118, 0.79215686) ;
#32782 = B_SPLINE_CURVE_WITH_KNOTS ( 'NONE', 3,
 ( #165785, #182008, #17368, #118160, #69313, #83452, #1118 ),
 .UNSPECIFIED., .F., .F.,
 ( 4, 3, 4 ),
 ( 0.0001126021369358783168, 0.001495765174703651531, 0.002006790696433101342 ),
 .UNSPECIFIED. ) ;
#32783 = CARTESIAN_POINT ( 'NONE',  ( 0.6823417656249882723, -0.4072916663252490466, 1.181850606188755259 ) ) ;
#32784 = CARTESIAN_POINT ( 'NONE',  ( 5.165293337126522388, 8.969999960048859577, 1.040834085586084257E-14 ) ) ;
#32785 = EDGE_CURVE ( 'NONE', #171070, #130050, #168293, .T. ) ;
#32787 = CARTESIAN_POINT ( 'NONE',  ( 5.471900407082693540, -0.9496530807377671080, 1.892462605218522720 ) ) ;
#32786 = CARTESIAN_POINT ( 'NONE',  ( -8.622622508611375025, 12.04318144581317895, 1.082531754730560403 ) ) ;
#32788 = CARTESIAN_POINT ( 'NONE',  ( 0.8312129145573650124, 0.1600495679085281175, 2.155820468135719814 ) ) ;
#32789 = CARTESIAN_POINT ( 'NONE',  ( -5.906512197408906317, 6.919960980845699439, -1.199719254218453823 ) ) ;
#32790 = PRESENTATION_LAYER_ASSIGNMENT (  '', '', ( #174599 ) ) ;
#32791 = CARTESIAN_POINT ( 'NONE',  ( 3.607351389687783794, 6.366271167014519783, 1.199719254218451159 ) ) ;
#32792 = CARTESIAN_POINT ( 'NONE',  ( 1.096400207583309028, -0.4391605778215034173, -1.771851442210800709 ) ) ;
#32793 = CARTESIAN_POINT ( 'NONE',  ( -5.413783410558481002, 5.210502155273325720, -0.7998128361456221525 ) ) ;
#32794 = ADVANCED_FACE ( 'NONE', ( #104368 ), #72908, .T. ) ;
#32795 = CARTESIAN_POINT ( 'NONE',  ( 3.012524388372894713, 1.323457619556423381, -1.257707024427484388 ) ) ;
#32796 = CARTESIAN_POINT ( 'NONE',  ( 8.350859280846272270, 13.12796858787615406, 8.536646826506961716 ) ) ;
#32797 = EDGE_LOOP ( 'NONE', ( #100071, #188417, #54427, #14248 ) ) ;
#32798 = CARTESIAN_POINT ( 'NONE',  ( 2.594150448275188481, 0.9308562254837976502, -1.735710503097695145 ) ) ;
#32799 = ORIENTED_EDGE ( 'NONE', *, *, #197971, .T. ) ;
#32800 = CARTESIAN_POINT ( 'NONE',  ( 5.302268720778519295, 1.468090865803386880, -1.271420572733022780 ) ) ;
#32801 = CARTESIAN_POINT ( 'NONE',  ( -5.901542003698421190, 10.10715911428198055, 0.000000000000000000 ) ) ;
#32803 = CARTESIAN_POINT ( 'NONE',  ( 5.238584497427841491, 1.261362679698872169, -1.704546977916908457 ) ) ;
#32802 = CARTESIAN_POINT ( 'NONE',  ( 5.169401708560450004, 9.252995436621013425, 0.000000000000000000 ) ) ;
#32804 = CARTESIAN_POINT ( 'NONE',  ( -1.734723475976807094E-14, 4.000000000000003553, -1.734723475976807094E-14 ) ) ;
#32805 = CARTESIAN_POINT ( 'NONE',  ( 3.018110381800835018, -1.909997030407738938, 0.09613604992317337228 ) ) ;
#32806 = CARTESIAN_POINT ( 'NONE',  ( 4.757767692435503015, 7.006667324785019524, -1.397933448811568224 ) ) ;
#32807 = DIRECTION ( 'NONE',  ( 0.000000000000000000, 0.000000000000000000, -1.000000000000000000 ) ) ;
#32808 = CARTESIAN_POINT ( 'NONE',  ( 5.239300017038202917, 5.077214539491492928, 0.000000000000000000 ) ) ;
#32809 = CARTESIAN_POINT ( 'NONE',  ( 4.147904930777053245, 6.926640621626830807, -1.199719254218452047 ) ) ;
#32810 = CARTESIAN_POINT ( 'NONE',  ( 3.861980204584365861, 0.6760143841026149403, -1.896330825423567568 ) ) ;
#32811 = DIRECTION ( 'NONE',  ( 0.000000000000000000, 1.000000000000000000, 0.000000000000000000 ) ) ;
#32812 = CARTESIAN_POINT ( 'NONE',  ( 4.723181480036696023, -0.08661695748878039947, 1.823760500460340550 ) ) ;
#32813 = CARTESIAN_POINT ( 'NONE',  ( 0.7134375191242479097, -1.748147108003229810, -1.108949491591210146 ) ) ;
#32814 = CARTESIAN_POINT ( 'NONE',  ( -7.700668062882065179, 10.96756792579566664, -1.082531754730543971 ) ) ;
#32815 =( BOUNDED_SURFACE ( )  B_SPLINE_SURFACE ( 3, 2, ( 
 ( #205060, #56702, #193091 ),
 ( #11129, #43673, #29542 ),
 ( #143325, #211464, #194159 ),
 ( #10070, #27391, #208262 ),
 ( #94558, #14325, #175799 ),
 ( #30615, #93491, #209318 ),
 ( #190945, #174744, #44740 ),
 ( #109791, #26318, #92430 ),
 ( #110847, #192008, #127121 ),
 ( #60965, #126046, #95634 ),
 ( #28466, #128199, #42609 ),
 ( #13278, #12203, #59895 ),
 ( #45807, #78274, #176852 ),
 ( #160600, #179000, #77206 ),
 ( #161684, #145470, #144401 ),
 ( #111927, #159530, #76146 ),
 ( #210402, #62045, #177928 ),
 ( #79352, #63099, #96703 ) ),
 .UNSPECIFIED., .F., .F., .T. ) 
 B_SPLINE_SURFACE_WITH_KNOTS ( ( 4, 2, 2, 2, 2, 2, 2, 2, 4 ),
 ( 3, 3 ),
 ( 0.000000000000000000, 0.0002366965742690631822, 0.0004733931485381263644, 0.0007100897228071895466, 0.0009467862970762527287, 0.001183482871345315803, 0.001420179445614379093, 0.001656876019883442384, 0.001893572594152505457 ),
 ( 0.000000000000000000, 1.000000000000000000 ),
 .UNSPECIFIED. ) 
 GEOMETRIC_REPRESENTATION_ITEM ( )  RATIONAL_B_SPLINE_SURFACE ( (
 ( 1.000000000000000000, 0.5647844906712728985, 1.000000000000000000),
 ( 1.000000000000000000, 0.5466263600439142945, 1.000000000000000000),
 ( 1.000000000000000000, 0.5350732119542429555, 1.000000000000000000),
 ( 1.000000000000000000, 0.5340116227283870920, 1.000000000000000000),
 ( 1.000000000000000000, 0.5448366076419797199, 1.000000000000000000),
 ( 1.000000000000000000, 0.5794957582366657700, 1.000000000000000000),
 ( 1.000000000000000000, 0.6029004271911160284, 1.000000000000000000),
 ( 1.000000000000000000, 0.6471109807879786846, 1.000000000000000000),
 ( 1.000000000000000000, 0.6680936278988408583, 1.000000000000000000),
 ( 1.000000000000000000, 0.6979136174567169837, 1.000000000000000000),
 ( 1.000000000000000000, 0.7066420332305399787, 1.000000000000000000),
 ( 1.000000000000000000, 0.7075346919462069950, 1.000000000000000000),
 ( 1.000000000000000000, 0.6996296472763482432, 1.000000000000000000),
 ( 1.000000000000000000, 0.6710614938507178939, 1.000000000000000000),
 ( 1.000000000000000000, 0.6504127778617547762, 1.000000000000000000),
 ( 1.000000000000000000, 0.6064966788548298293, 1.000000000000000000),
 ( 1.000000000000000000, 0.5828236970731119904, 1.000000000000000000),
 ( 1.000000000000000000, 0.5649783097559315515, 1.000000000000000000) ) ) 
 REPRESENTATION_ITEM ( '' )  SURFACE ( )  );
#32816 = CARTESIAN_POINT ( 'NONE',  ( -6.387810837761664473, 6.908839790476999809, 0.8166356711787735589 ) ) ;
#32817 = CARTESIAN_POINT ( 'NONE',  ( 11.33772463945036790, 11.00911576511426304, -3.600000000000000089 ) ) ;
#32818 = CARTESIAN_POINT ( 'NONE',  ( 5.436355746168001879, 1.843147576875401983, 0.3187000444574567548 ) ) ;
#32819 = CARTESIAN_POINT ( 'NONE',  ( 6.938021921891177612, 9.117444880338284818, -1.599625672291262513 ) ) ;
#32820 = CARTESIAN_POINT ( 'NONE',  ( -4.355193658487826802, 6.104145239700998538, -1.599625672291256517 ) ) ;
#32821 = CARTESIAN_POINT ( 'NONE',  ( -1.364683531250010295, 10.94270833367473372, 0.7879004041258445001 ) ) ;
#32822 = CARTESIAN_POINT ( 'NONE',  ( -5.575427483717760424, 7.527751369135936343, 1.599625672291269396 ) ) ;
#32823 = CARTESIAN_POINT ( 'NONE',  ( 4.220665892555866883, 3.818531717603609987, -0.7998128361456211532 ) ) ;
#32824 = CARTESIAN_POINT ( 'NONE',  ( -7.014364370223741929, 9.276787413384745662, -1.599625672291271394 ) ) ;
#32825 = CARTESIAN_POINT ( 'NONE',  ( -4.706651882238427120, 8.642844295920152575, 1.040834085586084257E-14 ) ) ;
#32826 = CARTESIAN_POINT ( 'NONE',  ( 6.666846200133992539, 1.614693783697606522, -1.451540455714307010 ) ) ;
#32827 = CARTESIAN_POINT ( 'NONE',  ( 2.513409721704229494, -1.974398269817168483, 0.7648893725459534609 ) ) ;
#32828 = CARTESIAN_POINT ( 'NONE',  ( 7.944187942603509356, 11.35563746875774882, 1.199719254218460707 ) ) ;
#32829 = CARTESIAN_POINT ( 'NONE',  ( -5.514013019825418915, 5.994650414344389056, -0.9619886414689113874 ) ) ;
#32830 = CARTESIAN_POINT ( 'NONE',  ( 6.596543124887806364, 2.046857425119428697, 0.3097440254393943881 ) ) ;
#32831 = CARTESIAN_POINT ( 'NONE',  ( 4.137223920935246824, 7.648466568186386816, 0.7801199165378830402 ) ) ;
#32832 = CARTESIAN_POINT ( 'NONE',  ( 5.829642864196168617, 6.863966765392747860, 1.082531754730558626 ) ) ;
#32834 = CARTESIAN_POINT ( 'NONE',  ( 5.639828713160493834, 5.682147708216442439, 1.040834085586084257E-14 ) ) ;
#32833 = CARTESIAN_POINT ( 'NONE',  ( -1.737500000000000266, -3.558333333333333570, -3.009438278150923907 ) ) ;
#32835 = CARTESIAN_POINT ( 'NONE',  ( 2.871321604122719418, 2.176383266876817046, -0.7197843628353149947 ) ) ;
#32837 = DIRECTION ( 'NONE',  ( 1.598721155460225418E-14, 0.000000000000000000, 1.000000000000000000 ) ) ;
#32836 = CARTESIAN_POINT ( 'NONE',  ( -6.387350227228854038, 6.552219065274637266, 2.500000000000690559 ) ) ;
#32838 = CARTESIAN_POINT ( 'NONE',  ( 2.531394148431935776, -0.1834752923718513118, 1.903540536635806912 ) ) ;
#32839 = ORIENTED_EDGE ( 'NONE', *, *, #117837, .F. ) ;
#32840 = CARTESIAN_POINT ( 'NONE',  ( 6.873620692004076105, 10.00267932643801672, -1.082531754730537976 ) ) ;
#32841 = CARTESIAN_POINT ( 'NONE',  ( 0.8264323289940983530, -0.9090603351678091526, -1.796376205119714298 ) ) ;
#32842 = CARTESIAN_POINT ( 'NONE',  ( 1.059338230090471011, 1.600537254139059673, 1.134074526779847769 ) ) ;
#32843 = CARTESIAN_POINT ( 'NONE',  ( -8.435144125996554720, 12.99275191363802229, 0.7998128361456341429 ) ) ;
#32844 = CARTESIAN_POINT ( 'NONE',  ( -5.879432169820529630, 10.01108796476595764, -0.7998128361456221525 ) ) ;
#32845 = FACE_OUTER_BOUND ( 'NONE', #147880, .T. ) ;
#32846 = ADVANCED_FACE ( 'NONE', ( #154182 ), #5750, .T. ) ;
#32848 = CARTESIAN_POINT ( 'NONE',  ( 2.201683042903946230, -1.769559083619182349, 0.04015057502057895605 ) ) ;
#32847 = CARTESIAN_POINT ( 'NONE',  ( 3.574242788201603016, -2.014869992041759872, -0.5574694344734670848 ) ) ;
#32849 = CARTESIAN_POINT ( 'NONE',  ( -2.788906526875773208E-15, 12.18750000000000178, -1.499999999999998446 ) ) ;
#32850 = AXIS2_PLACEMENT_3D ( 'NONE', #52167, #121516, #184279 ) ;
#32852 = CARTESIAN_POINT ( 'NONE',  ( 5.279328977631358555, 1.536242920967767711, 1.701453964730540447 ) ) ;
#32851 = CARTESIAN_POINT ( 'NONE',  ( 8.283668668269706714, 8.766627655843896250, 1.040834085586084257E-14 ) ) ;
#32853 = CARTESIAN_POINT ( 'NONE',  ( 4.013389373331836651, -0.8969206028703354816, -1.491242602974415243 ) ) ;
#32854 = CARTESIAN_POINT ( 'NONE',  ( 8.860417081730671995, 10.29590700256267155, 1.199719254218453823 ) ) ;
#32855 = CARTESIAN_POINT ( 'NONE',  ( 5.923986774528332333, 5.876015756563318426, -0.7998128361456481317 ) ) ;
#32856 = CARTESIAN_POINT ( 'NONE',  ( 4.446485213073447795, 1.132808404574834782, 1.312715084458302872 ) ) ;
#32857 = CARTESIAN_POINT ( 'NONE',  ( 4.633362100890871638, 0.004430012494727622249, -2.171350061612055349 ) ) ;
#32858 = CARTESIAN_POINT ( 'NONE',  ( 4.532503425670185493, 4.182342172903648070, 1.214306433183764966E-14 ) ) ;
#32859 = CARTESIAN_POINT ( 'NONE',  ( 5.542203953035277131, 0.8216685229280199509, 1.841735684200429990 ) ) ;
#32860 = CARTESIAN_POINT ( 'NONE',  ( 0.9375000000000007772, 1.451031289061083251, -1.451031289061159413 ) ) ;
#32861 = CARTESIAN_POINT ( 'NONE',  ( 0.7499999999999920064, 4.264583334016150751, 1.299038105676669330 ) ) ;
#32862 = CARTESIAN_POINT ( 'NONE',  ( 2.309485145960771035, -0.4240201670873133266, 1.878992650109307716 ) ) ;
#32863 = CARTESIAN_POINT ( 'NONE',  ( -1.402160292154681736E-14, 9.343750000682801371, 1.732050807568881190 ) ) ;
#32864 = CARTESIAN_POINT ( 'NONE',  ( 6.117462548578989967, 1.846355941783444976, 1.234888080409371369 ) ) ;
#32865 = ORIENTED_EDGE ( 'NONE', *, *, #27529, .F. ) ;
#32866 = CARTESIAN_POINT ( 'NONE',  ( 6.883263157960335832, 7.629137130509037412, 2.646189081643287810 ) ) ;
#32867 = CARTESIAN_POINT ( 'NONE',  ( -0.7500000000000215383, 3.691666666666690411, 1.299038105676671107 ) ) ;
#32868 = CARTESIAN_POINT ( 'NONE',  ( 5.991813822235618758, 9.077867661661846554, 1.199719254218462483 ) ) ;
#32869 = CARTESIAN_POINT ( 'NONE',  ( 1.752877424878969803, 2.197725149470313166, 0.3219655503990859757 ) ) ;
#32870 = CARTESIAN_POINT ( 'NONE',  ( 6.812952578306354035, -1.517200236233799071, 1.243500037895749921 ) ) ;
#32871 = CARTESIAN_POINT ( 'NONE',  ( 7.605760987586388744, 11.81721221891873697, 1.040834085586084257E-14 ) ) ;
#32872 = CARTESIAN_POINT ( 'NONE',  ( -10.10046125205658463, 11.84658821789661509, -1.082531754730537976 ) ) ;
#32873 = CIRCLE ( 'NONE', #181598, 0.07999999999999994615 ) ;
#32874 = CARTESIAN_POINT ( 'NONE',  ( 3.607351389687783794, 6.366271167014519783, 1.199719254218451159 ) ) ;
#32875 = CARTESIAN_POINT ( 'NONE',  ( -3.933273961740340496, 5.682181936820735579, 1.443375672974065660 ) ) ;
#32877 = CARTESIAN_POINT ( 'NONE',  ( 4.404768648179163471, 0.5469982912414109721, 1.988780625590305329 ) ) ;
#32876 = DIRECTION ( 'NONE',  ( 0.000000000000000000, -1.000000000000000000, 0.000000000000000000 ) ) ;
#32878 = CARTESIAN_POINT ( 'NONE',  ( -4.386226389220933441, 5.076017861301227008, -1.199719254218446718 ) ) ;
#32879 = VECTOR ( 'NONE', #140731, 1000.000000000000000 ) ;
#32880 = CARTESIAN_POINT ( 'NONE',  ( 1.364683531249986537, 0.1135416670080857532, 0.7879004041258500513 ) ) ;
#32881 = CARTESIAN_POINT ( 'NONE',  ( 5.905500869136258046, -0.4549164269060863020, 1.814235589242949587 ) ) ;
#32882 = CARTESIAN_POINT ( 'NONE',  ( 4.781731028689206298, 1.437863813525115830, -0.9690746147167289548 ) ) ;
#32883 = CARTESIAN_POINT ( 'NONE',  ( 4.001278354253400948, -1.735443821832120870, 0.1328310682092836426 ) ) ;
#32884 = CARTESIAN_POINT ( 'NONE',  ( 5.495132332240461714, 5.305409230568988832, 0.7998128361456341429 ) ) ;
#32885 = CARTESIAN_POINT ( 'NONE',  ( 2.454944477651953783, -1.996203790030710801, -1.126857184891062236 ) ) ;
#32886 = CARTESIAN_POINT ( 'NONE',  ( 1.364683531249986537, -1.136458332991912235, 0.7879004041258500513 ) ) ;
#32887 = CARTESIAN_POINT ( 'NONE',  ( 5.214434122969894503, 1.932256357821033887, 0.7989942847940935122 ) ) ;
#32888 = CARTESIAN_POINT ( 'NONE',  ( 0.6910384644343779970, -0.6650364481293036256, 1.717017257891314097 ) ) ;
#32889 = CARTESIAN_POINT ( 'NONE',  ( -3.147653791585856009, 8.920000000000001705, -2.419999999999835616 ) ) ;
#32890 = CARTESIAN_POINT ( 'NONE',  ( 3.024064729735044921, -1.777011313454954999, 0.9530116517338580451 ) ) ;
#32891 = CARTESIAN_POINT ( 'NONE',  ( 0.8850414913617115076, 1.931072968267994794, -1.036053359626129655 ) ) ;
#32892 = CARTESIAN_POINT ( 'NONE',  ( 7.322014706700720410, 14.95386301424541031, -9.100409427799018403 ) ) ;
#32893 = CARTESIAN_POINT ( 'NONE',  ( -5.879432169820529630, 10.01108796476595764, -0.7998128361456221525 ) ) ;
#32894 = CARTESIAN_POINT ( 'NONE',  ( 1.486871883557450369, 1.994755712061954123, 0.5540851298423480342 ) ) ;
#32895 = CARTESIAN_POINT ( 'NONE',  ( 4.168242161197552420, 6.950367390450747251, -1.199719254218452047 ) ) ;
#32896 = CARTESIAN_POINT ( 'NONE',  ( 0.6801582343749970061, -0.1614583329919219712, -1.178068619123852079 ) ) ;
#32897 = CARTESIAN_POINT ( 'NONE',  ( 3.809332071562030908, 1.790574611000576244, -1.135637872363919110 ) ) ;
#32898 = CARTESIAN_POINT ( 'NONE',  ( -0.6823417656250246877, -0.4489583329919111243, 1.181850606188755259 ) ) ;
#32899 = CARTESIAN_POINT ( 'NONE',  ( 6.498675964634617941, -0.4922777150685350156, -1.758009983081544991 ) ) ;
#32900 = VERTEX_POINT ( 'NONE', #160574 ) ;
#32901 = CARTESIAN_POINT ( 'NONE',  ( -6.642568916052639771, 6.714361588341672515, 0.000000000000000000 ) ) ;
#32902 = CARTESIAN_POINT ( 'NONE',  ( 9.103410076571945453, 12.70806329172093818, 1.199719254218450271 ) ) ;
#32903 = CARTESIAN_POINT ( 'NONE',  ( 6.983858524370782916, 7.320458831286981827, 0.7216878364870328300 ) ) ;
#32904 = CARTESIAN_POINT ( 'NONE',  ( -1.737499999999997824, -3.047916665710751705, 3.009438278150925683 ) ) ;
#32905 = CARTESIAN_POINT ( 'NONE',  ( -6.230135280679522936, 7.227244901336242755, 1.199719254218450271 ) ) ;
#32906 = CARTESIAN_POINT ( 'NONE',  ( 3.761977063697896639, 0.6766415394236917624, -1.903234751996728757 ) ) ;
#32907 = CARTESIAN_POINT ( 'NONE',  ( 6.545939543708723107, 0.8506627741289953804, -2.036432556493542823 ) ) ;
#32909 = EDGE_CURVE ( 'NONE', #181928, #174805, #205362, .T. ) ;
#32908 = CARTESIAN_POINT ( 'NONE',  ( -7.144220599758281054, 7.299621885998258897, 0.7998128361456341429 ) ) ;
#32910 = CARTESIAN_POINT ( 'NONE',  ( 8.646349277213076334, 11.11049346154719508, 1.599625672291281386 ) ) ;
#32911 = CARTESIAN_POINT ( 'NONE',  ( 5.067181549875774849, 1.617961714123143047, 0.9193176493522186021 ) ) ;
#32912 = CARTESIAN_POINT ( 'NONE',  ( 8.076906825439115423, 10.44614393447756129, -1.599625672291262513 ) ) ;
#32913 = CARTESIAN_POINT ( 'NONE',  ( 11.86239285000046095, 13.80000000000000249, -1.812080536912752837 ) ) ;
#32914 = CARTESIAN_POINT ( 'NONE',  ( -2.754277761870538299, 6.365074488824250309, 1.040834085586084257E-14 ) ) ;
#32915 = CARTESIAN_POINT ( 'NONE',  ( -7.718669524881690336, 7.899535955317097624, 0.7998128361456462443 ) ) ;
#32916 = CARTESIAN_POINT ( 'NONE',  ( 6.561407802241105536, 0.3549014609278942078, -2.029936712941163623 ) ) ;
#32917 = VECTOR ( 'NONE', #165961, 1000.000000000000000 ) ;
#32919 = CARTESIAN_POINT ( 'NONE',  ( -4.612682051294048513, 7.132468998681293471, 1.371008595254997964 ) ) ;
#32918 = CARTESIAN_POINT ( 'NONE',  ( -7.045397100956844127, 8.248660034984974132, -1.199719254218452047 ) ) ;
#32920 = CARTESIAN_POINT ( 'NONE',  ( 1.364683531249988757, 0.6343750003414208027, 0.000000000000000000 ) ) ;
#32921 = CARTESIAN_POINT ( 'NONE',  ( 2.231429653443087080, -1.583367121652721421, -0.7069697159475217818 ) ) ;
#32922 = CARTESIAN_POINT ( 'NONE',  ( 1.183123967286016986, -0.7853004192260810701, 1.553138493749019133 ) ) ;
#32924 = CARTESIAN_POINT ( 'NONE',  ( 5.992340707560141588, 9.934888558888093968, 0.7216878364870438212 ) ) ;
#32923 = CARTESIAN_POINT ( 'NONE',  ( 0.4116873800214932988, 2.009943462479982124, 1.133530718095694168 ) ) ;
#32925 = CARTESIAN_POINT ( 'NONE',  ( -10.45911201557330195, 5.175391108250987138, -5.201428006079835242 ) ) ;
#32926 = CARTESIAN_POINT ( 'NONE',  ( 2.126313425470290674, 1.189129703756890644, -1.682874868902742405 ) ) ;
#32927 = ADVANCED_FACE ( 'NONE', ( #191985 ), #41513, .F. ) ;
#32928 = EDGE_CURVE ( 'NONE', #8531, #144405, #132626, .T. ) ;
#32929 = CARTESIAN_POINT ( 'NONE',  ( 1.001327120302420548, 1.985796081718914419, 0.3474166314290441648 ) ) ;
#32930 = CARTESIAN_POINT ( 'NONE',  ( 9.319695500903007357, 13.69389061776176142, -7.486440698825377105 ) ) ;
#32931 = CARTESIAN_POINT ( 'NONE',  ( -4.261005416444848315, 8.193199762486115034, 0.7998128361456352531 ) ) ;
#32932 = CARTESIAN_POINT ( 'NONE',  ( 6.578970801323708706, -0.09418725797194843485, -1.868394071727994543 ) ) ;
#32933 = AXIS2_PLACEMENT_3D ( 'NONE', #32223, #66809, #162234 ) ;
#32935 = CARTESIAN_POINT ( 'NONE',  ( -6.672020991700860826, 7.917017590806697314, 1.082531754730549078 ) ) ;
#32934 = CARTESIAN_POINT ( 'NONE',  ( 4.131050151015442928, 1.750605847248308145, 0.7702136748066327199 ) ) ;
#32936 = CARTESIAN_POINT ( 'NONE',  ( 5.637410271038987730, -1.996576301129053377, 0.9405272304151901519 ) ) ;
#32937 = CARTESIAN_POINT ( 'NONE',  ( -5.587368702163209910, 9.532697562583475559, 0.000000000000000000 ) ) ;
#32938 = CARTESIAN_POINT ( 'NONE',  ( 6.444921918449731280, 8.612437886315108315, 1.599625672291268286 ) ) ;
#32939 = VECTOR ( 'NONE', #76755, 1000.000000000000000 ) ;
#32940 = CARTESIAN_POINT ( 'NONE',  ( -3.973948422136981407, 5.729635473950147606, -1.443375672974066548 ) ) ;
#32941 = CARTESIAN_POINT ( 'NONE',  ( 0.3990893844944528590, -0.2493554465154389221, -2.004162882155545056 ) ) ;
#32942 = EDGE_LOOP ( 'NONE', ( #102992, #210329 ) ) ;
#32943 = CARTESIAN_POINT ( 'NONE',  ( -1.500000000000001110, 12.80208333401612819, 0.8660254037844418162 ) ) ;
#32944 = CARTESIAN_POINT ( 'NONE',  ( 5.087122877145462851, -0.2765918260761930925, -2.290891016797763413 ) ) ;
#32945 = CARTESIAN_POINT ( 'NONE',  ( 4.492601031306558745, 1.923586649950057792, 0.3847822903023030428 ) ) ;
#32946 = CARTESIAN_POINT ( 'NONE',  ( 1.815213341579174688, -1.679845371888911698, -1.013028538569618719 ) ) ;
#32947 = CARTESIAN_POINT ( 'NONE',  ( 10.07387183015377197, 11.71160420905630062, -1.199719254218440723 ) ) ;
#32948 = CARTESIAN_POINT ( 'NONE',  ( -9.380156870162490890, 14.53091807600370622, 7.484187822888271668 ) ) ;
#32949 = ORIENTED_EDGE ( 'NONE', *, *, #65677, .T. ) ;
#32950 = CARTESIAN_POINT ( 'NONE',  ( 6.491432910188612126, -0.4373703761123280964, 1.975813455233149218 ) ) ;
#32952 = CARTESIAN_POINT ( 'NONE',  ( -8.995998617867369873, 10.45408546138876993, 1.199719254218462483 ) ) ;
#32951 = CARTESIAN_POINT ( 'NONE',  ( -3.927058049452637700, 7.733318157670055371, -0.7998128361456281477 ) ) ;
#32953 = CARTESIAN_POINT ( 'NONE',  ( 0.7613493127172387132, 0.9053670157611827252, 1.603083849714491027 ) ) ;
#32954 = EDGE_LOOP ( 'NONE', ( #9052, #15428, #25799, #91825, #131115 ) ) ;
#32955 = CARTESIAN_POINT ( 'NONE',  ( 4.592743594998466072, 2.127975290613278503, 0.4296678846467619772 ) ) ;
#32956 = CARTESIAN_POINT ( 'NONE',  ( 9.818094122049513928, 11.89513723134471590, -6.902820345984630457 ) ) ;
#32957 = CARTESIAN_POINT ( 'NONE',  ( 2.320699612028754188, -0.8158636990020677882, -1.957571985684476212 ) ) ;
#32958 = CARTESIAN_POINT ( 'NONE',  ( 1.499999999999987121, 2.577083334016147198, -0.8660254037844262731 ) ) ;
#32959 = CARTESIAN_POINT ( 'NONE',  ( 7.377608144130607393, 11.75895993479440982, -0.7998128361456291469 ) ) ;
#32960 = CARTESIAN_POINT ( 'NONE',  ( 6.587573780899039555, 6.778200402807202707, -0.2451836268814889253 ) ) ;
#32961 = CARTESIAN_POINT ( 'NONE',  ( 1.546242023939500276, 2.058303352229321703, 0.1039559743286587457 ) ) ;
#32963 = DIRECTION ( 'NONE',  ( -1.124869321039521280E-29, -7.437565543542506798E-15, 1.000000000000000000 ) ) ;
#32962 = CARTESIAN_POINT ( 'NONE',  ( -9.691380875670077444, 10.20103253123691189, 0.7998128361456462443 ) ) ;
#32964 = CARTESIAN_POINT ( 'NONE',  ( -1.364683531249997417, 3.759375000341423689, 1.214306433183764966E-14 ) ) ;
#32965 = CARTESIAN_POINT ( 'NONE',  ( -0.02244404828160087226, 0.2256878572204877031, -2.222431841814066278 ) ) ;
#32966 = CARTESIAN_POINT ( 'NONE',  ( -1.854049621773892653, 5.499999999999998224, -0.7500000000000015543 ) ) ;
#32967 = CARTESIAN_POINT ( 'NONE',  ( 5.848291733227988232, 0.9385554955868085081, -1.666026892748099009 ) ) ;
#32968 = CARTESIAN_POINT ( 'NONE',  ( 11.84668730067608244, 12.69999999999999929, -1.400000000000001688 ) ) ;
#32969 = CARTESIAN_POINT ( 'NONE',  ( 1.687200700035433876, -0.3313812920804170559, -2.237873883018532073 ) ) ;
#32970 = CARTESIAN_POINT ( 'NONE',  ( -7.700668062882059850, 11.92793714009701311, -0.7216878364870267237 ) ) ;
#32971 = CARTESIAN_POINT ( 'NONE',  ( 1.880848235559588799, -1.657448921354220506, -0.7316143304627804600 ) ) ;
#32972 = CARTESIAN_POINT ( 'NONE',  ( 2.307709453281155731, -1.106667911223922829, -1.563510803672981231 ) ) ;
#32973 = CARTESIAN_POINT ( 'NONE',  ( 2.910663983731573090, 0.6951178490613962868, 1.950330170896700022 ) ) ;
#32974 = CARTESIAN_POINT ( 'NONE',  ( -1.364683531250014514, 2.051041667008086655, -0.7879004041258289570 ) ) ;
#32975 = CARTESIAN_POINT ( 'NONE',  ( 1.164844247922683707, -1.781316891034259164, -0.8450378345598685836 ) ) ;
#32976 = CARTESIAN_POINT ( 'NONE',  ( 5.900991307970250510, 1.573582866467116759, -1.111162877451849162 ) ) ;
#32978 = CARTESIAN_POINT ( 'NONE',  ( 5.410124943364367667, 7.538760657221164507, -1.247639402986647550 ) ) ;
#32977 = CARTESIAN_POINT ( 'NONE',  ( 0.9444605492630732124, 0.9306326543588975264, -2.111904739147156818 ) ) ;
#32979 = CARTESIAN_POINT ( 'NONE',  ( -1.364683531250000748, 1.759375000341421913, 0.000000000000000000 ) ) ;
#32980 = CARTESIAN_POINT ( 'NONE',  ( 5.529752758335351182, 1.988887524167002985, -0.5466100825702590038 ) ) ;
#32981 = CARTESIAN_POINT ( 'NONE',  ( -4.726989112658928072, 8.666571064744069020, 1.040834085586084257E-14 ) ) ;
#32982 = CARTESIAN_POINT ( 'NONE',  ( 7.558834334818744338, 8.777393797832065303, 1.199719254218462483 ) ) ;
#32983 = CARTESIAN_POINT ( 'NONE',  ( -1.230761180058581372, 2.896116465842660137, 0.7750000000000117906 ) ) ;
#32985 = CARTESIAN_POINT ( 'NONE',  ( 0.7499999999999902300, 5.566666666666685082, -1.299038105676658228 ) ) ;
#32984 = CARTESIAN_POINT ( 'NONE',  ( -0.005051300619423290325, -0.4623140147347043483, -2.061856797492032545 ) ) ;
#32986 = CARTESIAN_POINT ( 'NONE',  ( 1.364683531249986537, 2.717708333674754062, -0.7879004041258239610 ) ) ;
#32987 = CARTESIAN_POINT ( 'NONE',  ( 5.395850447034295172, -0.7835752172833524432, 2.014745138864987073 ) ) ;
#32988 = CARTESIAN_POINT ( 'NONE',  ( 5.233071810066631357, 1.866936204443689462, 0.7709723521613828234 ) ) ;
#32989 = DIRECTION ( 'NONE',  ( -0.000000000000000000, 1.000000000000000000, 9.023263958591317418E-17 ) ) ;
#32990 = CARTESIAN_POINT ( 'NONE',  ( -5.748293942514186128, 6.769059690097084747, -1.082531754730544860 ) ) ;
#32991 = B_SPLINE_SURFACE_WITH_KNOTS ( 'NONE', 1, 3, ( 
 ( #69655, #88069, #119563, #1448, #135763, #70715, #169315, #153068, #4645, #202854, #154142, #5710, #55569, #39317, #149883, #67513, #10007, #158407, #189827, #174680, #27325, #125985, #41476, #208199, #140046, #191942, #59832, #43607, #172531, #155208, #60900, #24115, #124921, #76083, #173619, #106504, #91295, #188762, #90218, #25191, #109725, #11065, #207144, #107586, #190883, #56639, #157353, #175732, #93427, #204995, #42549, #159466, #77144, #23039, #138972, #156282, #142184, #127059, #122803, #73954, #40402, #171450, #108652, #89155, #8942, #143265, #26253, #209255, #75022, #7866, #141134, #206071, #58767, #57705, #193021, #123862, #92370, #105412, #6789, #72866, #12140, #66192, #29477, #65141, #213518, #95568, #28402, #161618, #45742, #179991, #32661, #46809, #211402, #13211, #79284, #131297, #112923, #162683, #181045, #80348, #94496, #145402, #163747, #178936, #210336, #146448, #130249, #97689, #63032, #30550, #196240, #195176, #197288, #15326, #81416, #129199, #113996, #98740, #48928, #96629, #147497, #14257, #115047, #164798, #16390, #111860, #160534, #125, #177865, #128129, #82469, #212462, #144336, #78212, #44673, #64107, #148559, #47883, #31614, #132337, #110785, #176787, #61975, #194092, #153888, #152813, #53179, #70462, #104071, #1200, #150698, #17452, #183176, #2260, #19602, #119307, #166939, #116101, #198343, #83536, #185293, #49983, #149618, #68336, #120389, #200471, #170118, #133401, #199405, #136579, #5457, #186364, #21704, #51051, #84609, #34780, #36917, #67262, #37999, #117174, #54252, #71537, #103000, #86743, #100854, #169056, #85674, #134468, #18532, #182092, #118246, #33723, #20653, #4391, #52118, #87816, #184228, #35852, #202599, #99801, #101930, #165866, #167996, #201531, #151762, #3331, #69401, #135508, #122544, #88898, #203667, #107325, #55316, #172273, #58513, #189572, #42285, #23860, #154952, #73691, #72615, #7607, #204731, #108397 ),
 ( #138714, #124668, #206881, #56381, #121467, #188505, #6537, #91035, #174421, #89967, #40136, #106249, #156019, #190625, #139789, #205816, #25997, #57448, #187437, #123609, #8684, #41219, #171191, #173349, #24931, #157095, #74766, #140869, #92106, #158161, #9752, #75828, #141935, #207948, #137647, #39065, #105151, #22781, #5079, #151381, #137271, #71154, #54938, #183858, #166552, #72225, #35471, #200095, #121090, #52794, #1882, #84228, #116789, #167618, #88517, #53873, #19217, #85295, #117867, #37616, #104768, #118933, #69022, #101549, #2950, #203291, #184913, #20284, #38689, #152438, #18140, #135139, #21335, #36537, #67942, #4017, #202219, #169746, #201155, #102624, #120006, #168680, #187057, #87441, #153510, #86368, #185982, #170817, #22408, #70086, #154579, #136201, #6156, #138332, #204348, #103696, #150316, #182786, #34404, #51744, #100476, #134086, #90082, #26117, #125850, #56501, #42408, #189688, #142046, #138831, #23979, #157209, #209119, #74884, #192876, #7727, #73811, #159326, #94355, #60757, #44531, #139905, #173475, #123726, #191806, #172391, #126918, #156145, #143125, #28263, #43471, #175595, #205936, #109589, #108514, #8806, #57568, #160397, #207000, #122662, #27184, #93290, #25052, #110649, #140992, #41339, #10923, #72734, #107448, #76998, #204848, #174541, #188625, #91155, #58631, #124784, #190744, #40256, #92228, #106368, #176650, #158279, #9869, #75945, #208062, #59687, #66050, #48785, #14114, #30409, #144198, #112783, #78074, #97547, #196103, #62884, #145255, #80204, #45599, #128477, #95428, #177724, #32521, #197147, #193951, #33580, #211260, #98596, #180899, #129053, #210194, #195028, #13060, #147353, #132194, #146306, #178793, #46662, #96494, #164658, #212319, #130112, #148418, #47738, #61830, #162543, #131156, #63956, #29334, #113854, #163604, #65004, #179849, #31473, #15186, #81276, #16241, #114902, #82326, #213380, #198202, #49836, #115962, #181952 ) ),
 .UNSPECIFIED., .F., .T., .F.,
 ( 2, 2 ),
 ( 4, 2, 2, 2, 2, 2, 2, 2, 2, 2, 2, 2, 2, 2, 2, 2, 2, 2, 2, 2, 2, 2, 2, 2, 2, 2, 2, 2, 2, 2, 2, 2, 2, 2, 2, 2, 2, 2, 2, 2, 2, 2, 2, 2, 2, 2, 2, 2, 2, 2, 2, 2, 2, 2, 2, 2, 2, 2, 2, 2, 2, 2, 2, 2, 2, 2, 2, 2, 2, 2, 2, 2, 2, 2, 2, 2, 2, 2, 2, 2, 2, 2, 2, 2, 2, 2, 2, 2, 2, 2, 2, 2, 2, 2, 2, 2, 2, 2, 2, 2, 2, 2, 2, 2, 2, 2, 2, 2, 2, 2, 2, 4 ),
 ( 0.000000000000000000, 1.000000000000000000 ),
 ( 0.0003185708494972700616, 0.0004481554763622086794, 0.0005777401032271472971, 0.0007073247300920859149, 0.0008369093569570245326, 0.0009017016703894938957, 0.0009664939838219631504, 0.001031286297254432405, 0.001096078610686901768, 0.001225663237551840277, 0.001290455550984309641, 0.001322851707700544322, 0.001355247864416779004, 0.001420040177849248367, 0.001484832491281717730, 0.001614417118146656239, 0.001679209431579125385, 0.001744001745011594749, 0.001808794058444064112, 0.001873586371876533475, 0.001938378685309002621, 0.002003170998741471767, 0.002067963312173941130, 0.002132755625606410493, 0.002197547939038879856, 0.002229944095755114538, 0.002262340252471349220, 0.002391924879336287946, 0.002521509506201226672, 0.002586301819633696035, 0.002651094133066165398, 0.002715886446498634761, 0.002780678759931104124, 0.002910263386796042417, 0.002975055700228511346, 0.003039848013660980709, 0.003104640327093450072, 0.003169432640525919435, 0.003299017267390858162, 0.003428601894255796888, 0.003493394207688266251, 0.003558186521120735614, 0.003622978834553204977, 0.003687771147985673906, 0.003817355774850612199, 0.003946940401715550925, 0.003979336558431785173, 0.004011732715148020288, 0.004076525028580489651, 0.004141317342012959014, 0.004206109655445428377, 0.004270901968877897741, 0.004335694282310367104, 0.004400486595742836467, 0.004465278909175305830, 0.004594863536040244556, 0.004659655849472713919, 0.004724448162905183282, 0.004789240476337652645, 0.004854032789770122008, 0.004918825103202591371, 0.004983617416635060735, 0.005048409730067530098, 0.005113202043499999461, 0.005177994356932468824, 0.005210390513648703939, 0.005242786670364938187, 0.005372371297229876913, 0.005501955924094814772, 0.005566748237527284135, 0.005631540550959752631, 0.005696332864392221994, 0.005761125177824691357, 0.005890709804689630083, 0.005955502118122099446, 0.006020294431554568809, 0.006085086744987038172, 0.006149879058419507535, 0.006214671371851976898, 0.006279463685284446262, 0.006409048312149384988, 0.006473840625581854351, 0.006506236782298089466, 0.006538632939014323714, 0.006603425252446793077, 0.006668217565879262440, 0.006797802192744201166, 0.006862594506176670529, 0.006927386819609139892, 0.006992179133041609256, 0.007056971446474078619, 0.007121763759906547982, 0.007186556073339017345, 0.007251348386771486708, 0.007316140700203956071, 0.007380933013636425434, 0.007445725327068894797, 0.007510517640501363293, 0.007575309953933832656, 0.007704894580798770515, 0.007769686894231239878, 0.007834479207663709241, 0.007866875364379945224, 0.007899271521096179471, 0.007964063834528647967, 0.008093648461393586693, 0.008158440774826056924, 0.008223233088258525419, 0.008288025401690993915, 0.008352817715123464146, 0.008482402341988402872, 0.008611986968853341598 ),
 .UNSPECIFIED. ) ;
#32992 = ADVANCED_FACE ( 'NONE', ( #207184 ), #193064, .F. ) ;
#32995 = CARTESIAN_POINT ( 'NONE',  ( 5.843201017809841247, 5.919415396974013532, 1.040834085586084257E-14 ) ) ;
#32994 = CARTESIAN_POINT ( 'NONE',  ( 1.642778471875000035, -1.976041666188709689, -2.845375778867859751 ) ) ;
#32993 = CARTESIAN_POINT ( 'NONE',  ( 6.003228155800906407, 10.22579295840155744, 0.000000000000000000 ) ) ;
#32996 = CARTESIAN_POINT ( 'NONE',  ( -4.980641328173854632, 6.904110530993182948, 1.599625672291263179 ) ) ;
#32997 = CARTESIAN_POINT ( 'NONE',  ( 3.573454097414618946, 1.463926983822515293, 1.387100322000796027 ) ) ;
#32998 = CARTESIAN_POINT ( 'NONE',  ( -7.343712760096452463, 11.71941532008788833, -0.7998128361456291469 ) ) ;
#33000 = CARTESIAN_POINT ( 'NONE',  ( -10.99683038201373719, -5.197079954928573109, 0.2726351642629477601 ) ) ;
#32999 = CARTESIAN_POINT ( 'NONE',  ( -4.277761160311629673, 4.949475094240346706, 1.199719254218462483 ) ) ;
#33001 = CARTESIAN_POINT ( 'NONE',  ( 1.364683531249988535, 5.655208333674751842, -0.7879004041258300672 ) ) ;
#33003 = CARTESIAN_POINT ( 'NONE',  ( -1.364683531250014514, 9.588541667008064096, -0.7879004041258335089 ) ) ;
#33002 = CARTESIAN_POINT ( 'NONE',  ( 5.155217493315787713, -1.824165352752779246, -1.159627250419709155 ) ) ;
#33004 = CARTESIAN_POINT ( 'NONE',  ( -11.50317709352769313, 6.904469223105409448, -3.423499370531426056 ) ) ;
#33006 = CARTESIAN_POINT ( 'NONE',  ( 5.958611281643053204, -1.915606116362132072, -0.6298603123368745615 ) ) ;
#33005 = CARTESIAN_POINT ( 'NONE',  ( -7.334597914868741242, 8.619747657844088806, -1.082531754730543083 ) ) ;
#33007 = CARTESIAN_POINT ( 'NONE',  ( -0.6823417656250003738, -0.2197916663252488800, -1.181850606188749264 ) ) ;
#33008 = CARTESIAN_POINT ( 'NONE',  ( 0.9962403866136140262, -0.4152203131645367806, -1.674012925115143213 ) ) ;
#33009 = CARTESIAN_POINT ( 'NONE',  ( 3.386504508363381571, 7.172948703057747011, -0.7998128361456362523 ) ) ;
#33011 = CARTESIAN_POINT ( 'NONE',  ( 7.289443866002793371, 8.533381260871966134, 1.199719254218452047 ) ) ;
#33010 = CARTESIAN_POINT ( 'NONE',  ( 6.792271770766432404, 10.86814146596211472, 1.040834085586084257E-14 ) ) ;
#33012 = CARTESIAN_POINT ( 'NONE',  ( -11.81385154090469847, 8.719572692708162265, 2.126314287815780357 ) ) ;
#33013 = CARTESIAN_POINT ( 'NONE',  ( 6.854772330626868637, -1.445518619047950981, 1.186913843143226233 ) ) ;
#33014 = CARTESIAN_POINT ( 'NONE',  ( 0.5924399621960573237, -1.116526876179738226, 1.674895298907061569 ) ) ;
#33015 = CARTESIAN_POINT ( 'NONE',  ( 6.539320575229279342, 6.038407674219216759, 2.491644695858772796 ) ) ;
#33016 = CARTESIAN_POINT ( 'NONE',  ( 2.507895228403643539, 5.869702166538802501, -0.7216878364870267237 ) ) ;
#33017 = CARTESIAN_POINT ( 'NONE',  ( 2.907470687441279455, 1.863611109782586484, 1.181582751932461095 ) ) ;
#33018 = CARTESIAN_POINT ( 'NONE',  ( -6.577113915960836721, 8.766661883411348555, -1.443375672974066548 ) ) ;
#33019 = ORIENTED_EDGE ( 'NONE', *, *, #185379, .T. ) ;
#33020 = CARTESIAN_POINT ( 'NONE',  ( 8.337901282279995385, 11.71100668175994386, -1.082531754730543083 ) ) ;
#33022 = CARTESIAN_POINT ( 'NONE',  ( 1.300407892936685794, 1.352140309104767013, -1.496066053310755262 ) ) ;
#33021 = CARTESIAN_POINT ( 'NONE',  ( 2.367978261241600713, 0.5630001329197281690, -2.044326955284565539 ) ) ;
#33023 = CARTESIAN_POINT ( 'NONE',  ( 2.267558116911760902, 0.4800365151868010716, -1.746770699433045415 ) ) ;
#33024 = CARTESIAN_POINT ( 'NONE',  ( 5.528692779322568640, 9.672168352510192690, 0.7998128361456341429 ) ) ;
#33025 = CARTESIAN_POINT ( 'NONE',  ( 6.297764839082774735, -0.7330946318361495351, 2.033732118066629457 ) ) ;
#33026 = TOROIDAL_SURFACE ( 'NONE', #36416, 6.330000000000000959, 0.08000000000000000167 ) ;
#33027 = CARTESIAN_POINT ( 'NONE',  ( 6.124532705071213279, 8.168374127381657246, -1.599625672291262513 ) ) ;
#33029 = CARTESIAN_POINT ( 'NONE',  ( 0.8310839537030527691, -1.512174478060366534, -1.176066492228915017 ) ) ;
#33028 = CARTESIAN_POINT ( 'NONE',  ( -4.771579997005698459, 7.654261532226910525, -1.199719254218452047 ) ) ;
#33030 = CARTESIAN_POINT ( 'NONE',  ( -15.75000000000000000, 12.69999999999999929, 0.6999999999999992895 ) ) ;
#33031 = CARTESIAN_POINT ( 'NONE',  ( 2.725000000000005862, 0.000000000000000000, 0.000000000000000000 ) ) ;
#33032 = CARTESIAN_POINT ( 'NONE',  ( 4.487385655998867406, 8.179107665399927285, 0.7216878364870438212 ) ) ;
#33033 = CARTESIAN_POINT ( 'NONE',  ( -1.364683531250014514, 0.8010416670080889867, -0.7879004041258289570 ) ) ;
#33034 = CARTESIAN_POINT ( 'NONE',  ( -2.868184766391971952, 6.360316304183658787, -0.2869589966386392743 ) ) ;
#33035 = CARTESIAN_POINT ( 'NONE',  ( -7.784352752540590004, 12.23349531127272094, 0.7998128361456481317 ) ) ;
#33036 = ADVANCED_FACE ( 'NONE', ( #177905 ), #85985, .F. ) ;
#33037 = CARTESIAN_POINT ( 'NONE',  ( 4.293933718354110418, -0.8299404887524585162, 1.996233173270183903 ) ) ;
#33038 = CARTESIAN_POINT ( 'NONE',  ( -6.373741612200205076, 8.529394195690610303, 1.443375672974064550 ) ) ;
#33039 = CARTESIAN_POINT ( 'NONE',  ( 5.939880696562888751, 7.062853913145737295, -1.082531754730548412 ) ) ;
#33040 = CARTESIAN_POINT ( 'NONE',  ( 2.074623746436579985, 0.9110886696130392481, 1.915067268644244702 ) ) ;
#33041 = CARTESIAN_POINT ( 'NONE',  ( 6.598675984083053336, -0.4903212918116289232, -1.758449130657411041 ) ) ;
#33042 = CARTESIAN_POINT ( 'NONE',  ( 3.602765292730988556, 1.556248219076960870, -1.210034843411099681 ) ) ;
#33043 = CARTESIAN_POINT ( 'NONE',  ( 5.976807594091997800, -1.347613670528555740, 1.357171208065083512 ) ) ;
#33044 = ORIENTED_EDGE ( 'NONE', *, *, #87216, .T. ) ;
#33046 = ADVANCED_FACE ( 'NONE', ( #44716 ), #22007, .F. ) ;
#33045 = LINE ( 'NONE', #83911, #187624 ) ;
#33047 = CARTESIAN_POINT ( 'NONE',  ( 6.478958751509338754, 1.837172605331442332, 0.7103315708588151534 ) ) ;
#33048 = CARTESIAN_POINT ( 'NONE',  ( 1.306472565299764410, 1.712382563992039586, 0.9159111323687963990 ) ) ;
#33049 = VERTEX_POINT ( 'NONE', #66235 ) ;
#33050 = CARTESIAN_POINT ( 'NONE',  ( -4.122561227007127016, 6.967349310553715647, 1.199719254218452935 ) ) ;
#33052 = CARTESIAN_POINT ( 'NONE',  ( 1.833628573703703912, 2.520495649928286674, -2.499561746654547889 ) ) ;
#33051 = CARTESIAN_POINT ( 'NONE',  ( -7.593975437430151132, 8.032261896522864930, -0.7216878364870338292 ) ) ;
#33054 = CARTESIAN_POINT ( 'NONE',  ( 5.960781091502512119, 10.10599504006161986, 0.7998128361456462443 ) ) ;
#33053 = CARTESIAN_POINT ( 'NONE',  ( 2.343796043118621775, 2.090200655756014658, 0.05028463699395351039 ) ) ;
#33056 = CARTESIAN_POINT ( 'NONE',  ( 5.411112705185558092, 6.445957923205511086, -1.082531754730548412 ) ) ;
#33055 = CARTESIAN_POINT ( 'NONE',  ( 5.472687561410540802, 9.536552588287639409, 0.7998128361456462443 ) ) ;
#33058 = VERTEX_POINT ( 'NONE', #132384 ) ;
#33057 = CARTESIAN_POINT ( 'NONE',  ( -0.1110810684432986112, 0.002541288824218449188, -1.796853612742685513 ) ) ;
#33059 = CARTESIAN_POINT ( 'NONE',  ( 4.951907052881864502, 0.6945806438464277033, -2.094803410698709900 ) ) ;
#33060 = CARTESIAN_POINT ( 'NONE',  ( 2.063769564651290356, 0.3772465526380370804, -2.174136642525636098 ) ) ;
#33061 = CARTESIAN_POINT ( 'NONE',  ( -7.065207446497166366, 9.336104335703744539, 0.000000000000000000 ) ) ;
#33062 = CARTESIAN_POINT ( 'NONE',  ( 0.8559432719405724033, 0.7744784914341161786, -1.748599447100062321 ) ) ;
#33063 = DIRECTION ( 'NONE',  ( -0.9999980456341537316, 0.000000000000000000, -0.001977050295949950038 ) ) ;
#33064 = CARTESIAN_POINT ( 'NONE',  ( 11.35569630219380777, 13.61268439291370314, -3.554478010595023107 ) ) ;
#33065 = CARTESIAN_POINT ( 'NONE',  ( 3.771986465066007099, -2.040223509676724944, 0.3510349978646867264 ) ) ;
#33066 = CARTESIAN_POINT ( 'NONE',  ( -4.225337428953291230, 8.081310767087481750, 0.7998128361456341429 ) ) ;
#33068 = CARTESIAN_POINT ( 'NONE',  ( 2.026462046419864826, 1.244889377058140845, -1.767065586814352773 ) ) ;
#33067 = CARTESIAN_POINT ( 'NONE',  ( -4.274898507010545856, 3.881803101134051470, -0.7998128361456221525 ) ) ;
#33069 = CARTESIAN_POINT ( 'NONE',  ( 4.177398808104064720, 1.432170664236757540, 1.658919600136643524 ) ) ;
#33070 = CARTESIAN_POINT ( 'NONE',  ( -4.320273482414311417, 8.054419775615775379, 0.2990372400716989065 ) ) ;
#33071 = CARTESIAN_POINT ( 'NONE',  ( 3.851925040058331806, 5.587274861525073355, -1.443375672974066548 ) ) ;
#33072 = CARTESIAN_POINT ( 'NONE',  ( 1.483013432599452175, 7.294277089886983312, 4.259227663826820276 ) ) ;
#33073 = CARTESIAN_POINT ( 'NONE',  ( 1.364683531249996529, 14.27604166700806942, 0.7879004041258405033 ) ) ;
#33074 = CARTESIAN_POINT ( 'NONE',  ( -5.354544322754380303, 5.211666229493680191, 0.7998128361456281477 ) ) ;
#33075 = PRODUCT_DEFINITION_CONTEXT ( 'detailed design', #211010, 'design' ) ;
#33076 = CARTESIAN_POINT ( 'NONE',  ( 5.942016496743827147, -1.492280758002052510, -0.8831153342708076837 ) ) ;
#33077 = ADVANCED_FACE ( 'NONE', ( #114042 ), #65248, .T. ) ;
#33079 = CARTESIAN_POINT ( 'NONE',  ( -8.026063749610043985, 12.30756544127966912, -0.7216878364870267237 ) ) ;
#33078 = VECTOR ( 'NONE', #89822, 1000.000000000000000 ) ;
#33080 = CARTESIAN_POINT ( 'NONE',  ( 5.172746982222708567, 1.431596967658786745, -1.495705434250683918 ) ) ;
#33081 = CARTESIAN_POINT ( 'NONE',  ( 5.659793223991267830, 1.261623160278273481, 1.700126385781860927 ) ) ;
#33082 = CARTESIAN_POINT ( 'NONE',  ( 5.612185521052973414, 8.634967976948757951, -1.199719254218440723 ) ) ;
#33083 = CARTESIAN_POINT ( 'NONE',  ( -0.6823417656249969321, 5.717708333674756283, -1.181850606188749264 ) ) ;
#33084 = CARTESIAN_POINT ( 'NONE',  ( 3.801571140118775727, -1.488283618643148287, -1.289908803443328145 ) ) ;
#33085 = CARTESIAN_POINT ( 'NONE',  ( 5.560555354427807906, -2.070165260436385601, -0.9845844755148360772 ) ) ;
#33086 = CARTESIAN_POINT ( 'NONE',  ( 2.648829494986388422, -1.517897411861212076, 1.014145048410304284 ) ) ;
#33087 = AXIS2_PLACEMENT_3D ( 'NONE', #170549, #5889, #71962 ) ;
#33088 = CARTESIAN_POINT ( 'NONE',  ( 6.536439455564150514, 9.679577560583279450, 1.082531754730549078 ) ) ;
#33089 = CARTESIAN_POINT ( 'NONE',  ( 4.704316113817540668, 5.551085556617666228, -1.082531754730548412 ) ) ;
#33090 = CARTESIAN_POINT ( 'NONE',  ( -5.747767057189642870, 8.793146435774861658, -1.199719254218440723 ) ) ;
#33091 = CARTESIAN_POINT ( 'NONE',  ( 6.554440917563797875, 6.611545590104705994, -0.7998128361456481317 ) ) ;
#33092 = VERTEX_POINT ( 'NONE', #163791 ) ;
#33093 = CARTESIAN_POINT ( 'NONE',  ( 3.832292871861494810, -1.038684978035837592, -1.724458057284683710 ) ) ;
#33094 = CARTESIAN_POINT ( 'NONE',  ( 4.487127722112081329, 0.09209952633786910869, 1.959694304038139379 ) ) ;
#33095 = CARTESIAN_POINT ( 'NONE',  ( -7.555971681517696936, 7.709721804725773175, 0.7998128361456462443 ) ) ;
#33096 = CARTESIAN_POINT ( 'NONE',  ( -3.598799709423620374, 6.286017863381107240, 1.199719254218464037 ) ) ;
#33097 = CARTESIAN_POINT ( 'NONE',  ( -6.773846765307993678, -7.473374494058229622, -6.773846765307958151 ) ) ;
#33100 = B_SPLINE_CURVE_WITH_KNOTS ( 'NONE', 3,
 ( #74789, #36942, #5480, #86767, #103023, #107347, #152838 ),
 .UNSPECIFIED., .F., .F.,
 ( 4, 3, 4 ),
 ( 0.0001135037246156260884, 0.0006171834326598004457, 0.002007692286214980693 ),
 .UNSPECIFIED. ) ;
#33099 = CARTESIAN_POINT ( 'NONE',  ( 5.436323762753620947, 1.744125921451036065, 0.2996227856876289564 ) ) ;
#33098 = CARTESIAN_POINT ( 'NONE',  ( 0.2223640086436579066, 2.001884549173582606, 0.6031067468692548061 ) ) ;
#33101 = CARTESIAN_POINT ( 'NONE',  ( -8.283668668269720925, 8.766627655843896250, 1.056142170575426150E-14 ) ) ;
#33102 = CARTESIAN_POINT ( 'NONE',  ( 1.711130781365449716, -0.2659051965858104660, 2.175189728913041964 ) ) ;
#33103 = CARTESIAN_POINT ( 'NONE',  ( 0.9249085282522085949, -1.102964995092512890, -1.346285399390812598 ) ) ;
#33104 = CARTESIAN_POINT ( 'NONE',  ( 5.449487677688982679, 8.445153826357429949, -1.199719254218446718 ) ) ;
#33105 = CARTESIAN_POINT ( 'NONE',  ( 0.1335669894368864130, 4.084991946249068029, -2.708374394877795410 ) ) ;
#33106 = CARTESIAN_POINT ( 'NONE',  ( 1.488428555967473921, -0.2500744359604460954, -1.706524604440103898 ) ) ;
#33107 = CARTESIAN_POINT ( 'NONE',  ( 0.6619992422990974568, 1.085049530943157148, 1.904046507712559455 ) ) ;
#33108 = CARTESIAN_POINT ( 'NONE',  ( 2.631697372267821855, -2.058793095894187353, 0.7952504953367269813 ) ) ;
#33109 = CARTESIAN_POINT ( 'NONE',  ( 1.393694035345336424, -1.963709693186867833, 0.9261614696171887040 ) ) ;
#33110 = CARTESIAN_POINT ( 'NONE',  ( 0.000000000000000000, 5.499999999999998224, -2.000000000000000000 ) ) ;
#33111 = CARTESIAN_POINT ( 'NONE',  ( 1.938805156862877022, -1.633297379596149845, 1.347353381010838458 ) ) ;
#33112 = CARTESIAN_POINT ( 'NONE',  ( 6.662118508819760088, -7.185026885899511662, -6.772457744868767726 ) ) ;
#33113 = CARTESIAN_POINT ( 'NONE',  ( 6.000991310419570901, 1.574649422783209740, -1.109465276731670613 ) ) ;
#33114 = ORIENTED_EDGE ( 'NONE', *, *, #14697, .F. ) ;
#33116 = CARTESIAN_POINT ( 'NONE',  ( -0.6823417656250246877, -0.3864583329919110688, 1.181850606188755259 ) ) ;
#33115 = CARTESIAN_POINT ( 'NONE',  ( 2.402247335887615964, -0.8806970201959153366, -2.116636687559919849 ) ) ;
#33117 = CARTESIAN_POINT ( 'NONE',  ( 3.928111819657337911, 5.605883094398769195, 1.599625672291267398 ) ) ;
#33118 = CARTESIAN_POINT ( 'NONE',  ( 6.030679399980265920, 5.930214142932100252, -0.7998128361456281477 ) ) ;
#33119 = CARTESIAN_POINT ( 'NONE',  ( 5.408899451717416262, -0.5379699361975317506, -2.155043070319954790 ) ) ;
#33120 = CARTESIAN_POINT ( 'NONE',  ( -7.293923454472094114, 9.532663335016016148, 1.443375672974090751 ) ) ;
#33121 = CARTESIAN_POINT ( 'NONE',  ( -0.3618152180564696563, -5.223163831703879545, -10.97113184882213055 ) ) ;
#33122 = CARTESIAN_POINT ( 'NONE',  ( 5.504247177468179153, 7.444707678511436555, 1.443375672974062551 ) ) ;
#33123 = CARTESIAN_POINT ( 'NONE',  ( -6.765155463094763455, 8.915767345075790828, 1.443375672974078761 ) ) ;
#33124 = CARTESIAN_POINT ( 'NONE',  ( 5.126391479742934187, 6.113783160189109722, -1.082531754730548412 ) ) ;
#33125 = VERTEX_POINT ( 'NONE', #34820 ) ;
#33126 = CARTESIAN_POINT ( 'NONE',  ( 2.971327447312217984, -1.987046587055636637, -0.3419355124290662240 ) ) ;
#33128 = CARTESIAN_POINT ( 'NONE',  ( 1.094667215044333952, 2.031392189445472063, 0.3564975109212295545 ) ) ;
#33127 = CARTESIAN_POINT ( 'NONE',  ( 5.425234023762710578, 9.481190127698507553, -0.7998128361456291469 ) ) ;
#33129 = CARTESIAN_POINT ( 'NONE',  ( 4.465904445180872706, 4.989870290919971474, 0.9171369020453674636 ) ) ;
#33130 = CARTESIAN_POINT ( 'NONE',  ( 5.844973620822844218, 6.952128991449046502, 1.082531754730549967 ) ) ;
#33131 = CARTESIAN_POINT ( 'NONE',  ( 2.960184520039609524, -4.109567588314592790, -1.425549731837409961 ) ) ;
#33132 = CARTESIAN_POINT ( 'NONE',  ( -1.201851678989727383E-14, 3.321875000341421025, 1.575800808251672791 ) ) ;
#33133 = CARTESIAN_POINT ( 'NONE',  ( 4.259861650310483583, 1.032037387010206198, 1.933225914978464299 ) ) ;
#33134 = CARTESIAN_POINT ( 'NONE',  ( 1.459611520199757706, -1.915600648959712382, -0.6298732728240025169 ) ) ;
#33135 = CARTESIAN_POINT ( 'NONE',  ( 1.294213439101927321, 1.504999338701202394, -1.060447551955064016 ) ) ;
#33136 = CARTESIAN_POINT ( 'NONE',  ( 4.593604542485023146, -1.840816577468977533, -0.04244875611379012037 ) ) ;
#33137 = CARTESIAN_POINT ( 'NONE',  ( 7.904567251967224095, 9.180748867838630645, 1.199719254218462483 ) ) ;
#33138 = CARTESIAN_POINT ( 'NONE',  ( 2.343750000000001332, 1.895863743164134307, 0.7852924748298687474 ) ) ;
#33139 = CARTESIAN_POINT ( 'NONE',  ( 4.981388616008130654, 1.702979688329594676, -0.6582044668519275721 ) ) ;
#33140 = CARTESIAN_POINT ( 'NONE',  ( 5.590470263882489910, -0.4872053753022275169, 1.956560708789633285 ) ) ;
#33141 = CARTESIAN_POINT ( 'NONE',  ( -9.826962411806732689, 10.35921099006301382, -0.7998128361456291469 ) ) ;
#33143 = CARTESIAN_POINT ( 'NONE',  ( -6.200875153403786477, 8.327716660428123419, -1.599625672291271394 ) ) ;
#33142 = CARTESIAN_POINT ( 'NONE',  ( 4.856464543430921488, 0.8614301073998543723, 2.092300974686135184 ) ) ;
#33144 = CARTESIAN_POINT ( 'NONE',  ( 0.5925747745999773164, -2.090437052192719136, -0.2555399532009738350 ) ) ;
#33145 = CARTESIAN_POINT ( 'NONE',  ( -6.912678218121246942, 9.158153569265168770, 1.599625672291269396 ) ) ;
#33146 = CARTESIAN_POINT ( 'NONE',  ( 4.369627354678314646, -0.3570511267821044332, 2.039192500141631115 ) ) ;
#33147 = CARTESIAN_POINT ( 'NONE',  ( 8.703444544968814256, 12.24143683818393313, -1.199719254218446718 ) ) ;
#33148 = CARTESIAN_POINT ( 'NONE',  ( 1.499999999999821032, 7.240846818246208905, -4.154462424328212222 ) ) ;
#33149 = APPLICATION_PROTOCOL_DEFINITION ( 'draft international standard', 'automotive_design', 1998, #82292 ) ;
#33150 = CARTESIAN_POINT ( 'NONE',  ( -9.203287345578106127, 9.631590079462940324, 0.7998128361456462443 ) ) ;
#33151 = CARTESIAN_POINT ( 'NONE',  ( 11.04986610412592363, 11.10944100431282600, 1.056385672146459953 ) ) ;
#33152 = CARTESIAN_POINT ( 'NONE',  ( 7.014364370223726830, 9.276787413384745662, -1.599625672291269396 ) ) ;
#33153 = CARTESIAN_POINT ( 'NONE',  ( 5.678179657697552507, 6.109196432984326464, -0.7486794562398890740 ) ) ;
#33154 = CARTESIAN_POINT ( 'NONE',  ( -2.591579918506545344, 6.175260338232929413, 1.040834085586084257E-14 ) ) ;
#33156 = CARTESIAN_POINT ( 'NONE',  ( 2.145073868429191677, 2.156049884074415779, 0.5345358195362903686 ) ) ;
#33155 = CARTESIAN_POINT ( 'NONE',  ( 0.3520121086563637314, -1.504009422257305495, -1.495223887398588358 ) ) ;
#33157 = DIRECTION ( 'NONE',  ( 0.000000000000000000, 1.000000000000000000, 0.000000000000000000 ) ) ;
#33158 = CARTESIAN_POINT ( 'NONE',  ( -7.533490631048818109, 8.818102486758951031, -1.199719254218452047 ) ) ;
#33159 = CARTESIAN_POINT ( 'NONE',  ( 6.810273232766058449, 6.839740281182199233, 1.040834085586084257E-14 ) ) ;
#33160 = CARTESIAN_POINT ( 'NONE',  ( 2.928120951529111338, 1.047165451586975049, 1.658829547137883775 ) ) ;
#33161 = CARTESIAN_POINT ( 'NONE',  ( 5.880485940025228508, 7.883652901494672349, 1.599625672291267398 ) ) ;
#33162 = CARTESIAN_POINT ( 'NONE',  ( -4.015022313999534909, 7.625723350685065682, -0.07359193599470841007 ) ) ;
#33163 = CARTESIAN_POINT ( 'NONE',  ( 3.171717870593107058, 5.787755718078879674, -1.199719254218446718 ) ) ;
#33164 = CARTESIAN_POINT ( 'NONE',  ( -6.021229618244897885, 7.157760988441397743, 1.082531754730548412 ) ) ;
#33165 = CARTESIAN_POINT ( 'NONE',  ( -6.873620692448438874, 10.96304854125777695, 0.000000000000000000 ) ) ;
#33166 = CARTESIAN_POINT ( 'NONE',  ( 2.109781586379317897, 1.642293606977158538, 1.341614810521203349 ) ) ;
#33167 = CARTESIAN_POINT ( 'NONE',  ( -5.692444392891315097, 7.734547439830227411, -1.599625672291271394 ) ) ;
#33168 = CARTESIAN_POINT ( 'NONE',  ( 4.439869198996494681, 1.279870211898268550, 1.486999339763886097 ) ) ;
#33169 = CARTESIAN_POINT ( 'NONE',  ( 3.643588467267334874, -1.635511012911139650, -1.413612897787956513 ) ) ;
#33170 = CARTESIAN_POINT ( 'NONE',  ( 2.806014743833366687, 1.331929863061011243, -1.271513748034671432 ) ) ;
#33171 = UNCERTAINTY_MEASURE_WITH_UNIT (LENGTH_MEASURE( 1.000000000000000082E-05 ), #177270, 'distance_accuracy_value', 'NONE');
#33172 = CARTESIAN_POINT ( 'NONE',  ( -4.068573627943592008, 7.549288226164498461, -0.4708643921484123585 ) ) ;
#33173 = CARTESIAN_POINT ( 'NONE',  ( -1.364683531250014514, -0.6989583329919100141, -0.7879004041258359514 ) ) ;
#33174 = CARTESIAN_POINT ( 'NONE',  ( 4.716618446111438878, -0.08105245650613655817, 1.738572149171065062 ) ) ;
#33175 = CARTESIAN_POINT ( 'NONE',  ( 4.929342268689171469, 7.989555622611471897, -1.003472558803005565 ) ) ;
#33176 = CARTESIAN_POINT ( 'NONE',  ( 5.666945020832181434, 5.713783400500082266, 0.7216878364870317197 ) ) ;
#33177 = CARTESIAN_POINT ( 'NONE',  ( -10.45911050446410506, 5.175404930453152197, 5.201426885097844455 ) ) ;
#33178 = EDGE_CURVE ( 'NONE', #83814, #10371, #103305, .T. ) ;
#33179 = CARTESIAN_POINT ( 'NONE',  ( 1.815512348505427642, -0.2646426633909418347, 2.145385951886819242 ) ) ;
#33180 = CARTESIAN_POINT ( 'NONE',  ( 4.235703761680151835, -1.880146911114020325, -0.7282675588539261335 ) ) ;
#33181 = CARTESIAN_POINT ( 'NONE',  ( -7.985389288324685531, 12.26011190311341537, -0.7216878364870267237 ) ) ;
#33182 = CARTESIAN_POINT ( 'NONE',  ( 1.358524781292804517, 0.8764843271744371389, 1.976213614152767750 ) ) ;
#33183 = CARTESIAN_POINT ( 'NONE',  ( 2.407442502341358814, -0.4355224260998523111, 1.922489325443673236 ) ) ;
#33184 = DIRECTION ( 'NONE',  ( 0.000000000000000000, 0.000000000000000000, 1.000000000000000000 ) ) ;
#33185 = CARTESIAN_POINT ( 'NONE',  ( 3.649888709942475273, 0.7017510601828327310, 1.811005675494174350 ) ) ;
#33188 = ORIENTED_EDGE ( 'NONE', *, *, #184990, .F. ) ;
#33187 = CARTESIAN_POINT ( 'NONE',  ( -4.421367491832313590, 6.251624388594711590, 1.443375672974065660 ) ) ;
#33186 = CARTESIAN_POINT ( 'NONE',  ( -8.609064354553318310, 12.98773281371349775, 0.7216878364870317197 ) ) ;
#33189 = CARTESIAN_POINT ( 'NONE',  ( -4.950135482320939140, 4.947781948895412008, -0.7216878364870338292 ) ) ;
#33190 = CARTESIAN_POINT ( 'NONE',  ( 3.061108821635398769, 6.793320401875094561, -0.7998128361456362523 ) ) ;
#33191 = CARTESIAN_POINT ( 'NONE',  ( -5.631432701629818460, 7.663367133358481631, 1.599625672291263179 ) ) ;
#33192 = CARTESIAN_POINT ( 'NONE',  ( -8.459924664802993988, 12.81373650900478189, 1.040834085586084257E-14 ) ) ;
#33193 = CARTESIAN_POINT ( 'NONE',  ( 1.255210933454937283, -1.738917431694649407, 1.358592805172780693 ) ) ;
#33194 = CARTESIAN_POINT ( 'NONE',  ( 3.285556943749998737, -3.405208332855374831, -1.896917185911906500 ) ) ;
#33195 = ADVANCED_FACE ( 'NONE', ( #162728 ), #16836, .T. ) ;
#33196 = CARTESIAN_POINT ( 'NONE',  ( 5.102378460580520247, 1.956245014681293970, 0.1482201060269832671 ) ) ;
#33197 = ORIENTED_EDGE ( 'NONE', *, *, #19314, .F. ) ;
#33198 = CARTESIAN_POINT ( 'NONE',  ( 3.309862381128574338, -1.264700674563856264, -1.697971918580774675 ) ) ;
#33199 = CARTESIAN_POINT ( 'NONE',  ( 1.499999999999989120, 2.785416667349484676, 0.8660254037844524744 ) ) ;
#33200 = CARTESIAN_POINT ( 'NONE',  ( 5.029711800989886683, 4.970344644017389513, 1.040834085586084257E-14 ) ) ;
#33201 = CARTESIAN_POINT ( 'NONE',  ( 4.066218318298571610, -1.718653781379267276, -0.6607852518168353395 ) ) ;
#33202 = VERTEX_POINT ( 'NONE', #135551 ) ;
#33203 = UNCERTAINTY_MEASURE_WITH_UNIT (LENGTH_MEASURE( 1.000000000000000082E-05 ), #161297, 'distance_accuracy_value', 'NONE');
#33204 = CARTESIAN_POINT ( 'NONE',  ( -7.133561379084627063, 11.47423870890741782, 0.7998128361456481317 ) ) ;
#33205 = CARTESIAN_POINT ( 'NONE',  ( -4.772106882330241717, 5.630174786549132726, -1.082531754730544860 ) ) ;
#33206 = CARTESIAN_POINT ( 'NONE',  ( 5.537388447972660721, -0.05000006065614125139, 2.120159173171487055 ) ) ;
#33207 = CARTESIAN_POINT ( 'NONE',  ( 4.299907273828439180, 8.168308919441841454, 1.040834085586084257E-14 ) ) ;
#33208 = CARTESIAN_POINT ( 'NONE',  ( 5.536423053809180317, 2.029556968340691547, 0.3564751269278207957 ) ) ;
#33211 = CARTESIAN_POINT ( 'NONE',  ( 2.436835438956724165, -1.365703447793526371, -1.235134912642745775 ) ) ;
#33210 = CARTESIAN_POINT ( 'NONE',  ( 0.7833917827068856976, -1.768883884249613736, 0.5786898513908571573 ) ) ;
#33209 = CARTESIAN_POINT ( 'NONE',  ( 4.068855497876980643, 7.761098824249519801, -0.7216878364870392693 ) ) ;
#33212 = CARTESIAN_POINT ( 'NONE',  ( 7.365103760721646076, 9.615707025640515937, 1.599625672291281386 ) ) ;
#33213 = CARTESIAN_POINT ( 'NONE',  ( -3.023105066167323329, 5.702484939155337607, -2.500000000000000444 ) ) ;
#33214 = CARTESIAN_POINT ( 'NONE',  ( -11.89197415570408900, 9.800000000000000711, 0.8055989572471843330 ) ) ;
#33215 = FACE_OUTER_BOUND ( 'NONE', #120667, .T. ) ;
#33216 = STYLED_ITEM ( 'NONE', ( #190387 ), #95835 ) ;
#33217 = CARTESIAN_POINT ( 'NONE',  ( 2.895379187063460424, 1.892502543702856865, -1.135010264495312837 ) ) ;
#33218 = CARTESIAN_POINT ( 'NONE',  ( 5.272873185648853323, -2.127775705341850898, -0.7691360568998426572 ) ) ;
#33219 = CARTESIAN_POINT ( 'NONE',  ( -7.212574532790102744, 8.477387045419011002, -1.082531754730550855 ) ) ;
#33220 = CARTESIAN_POINT ( 'NONE',  ( 5.062699594374425516, 0.5334270428436416189, 1.731249764757249343 ) ) ;
#33221 = CARTESIAN_POINT ( 'NONE',  ( 5.102711585370895975, 1.772601733252886280, 0.7270577078305997532 ) ) ;
#33222 = CARTESIAN_POINT ( 'NONE',  ( 1.364683531249988535, 5.717708333674752730, -0.7879004041258300672 ) ) ;
#33223 = CARTESIAN_POINT ( 'NONE',  ( 4.944154083221365070, 1.865701114312174225, 0.1370711555178441010 ) ) ;
#33224 = CARTESIAN_POINT ( 'NONE',  ( 4.949569884170424316, 1.378596123743974555, 1.250361270004763714 ) ) ;
#33225 = CARTESIAN_POINT ( 'NONE',  ( -1.364683531249997417, 5.509375000341417916, 1.214306433183764966E-14 ) ) ;
#33226 = AXIS2_PLACEMENT_3D ( 'NONE', #139668, #107204, #9628 ) ;
#33227 = CARTESIAN_POINT ( 'NONE',  ( 6.666889860676148416, -1.620333765578816587, -0.7124167289687727278 ) ) ;
#33228 = CARTESIAN_POINT ( 'NONE',  ( 0.2687680251878405424, -0.2516378192510167477, -2.000730910237565663 ) ) ;
#33230 = CARTESIAN_POINT ( 'NONE',  ( 3.018300108557407935, -1.038308444602775271, -1.832253800920932596 ) ) ;
#33229 = CARTESIAN_POINT ( 'NONE',  ( -3.592547517496941900, 5.214391408544949869, -1.443375672974051449 ) ) ;
#33231 = CARTESIAN_POINT ( 'NONE',  ( 9.561524646135536543, 12.17819805862340310, -1.599625672291262513 ) ) ;
#33233 = CARTESIAN_POINT ( 'NONE',  ( 0.07479286986305370977, 0.004866263145587856019, -1.855573292446038414 ) ) ;
#33232 = CARTESIAN_POINT ( 'NONE',  ( 0.4019237886466816012, 11.95758545099816494, -1.499999999999998668 ) ) ;
#33234 = CARTESIAN_POINT ( 'NONE',  ( -3.469446951953614189E-15, -1.000000000000000888, 2.602085213965210642E-15 ) ) ;
#33235 = CARTESIAN_POINT ( 'NONE',  ( 1.564719475598770337, 0.6377593443319184985, 1.916497437154760508 ) ) ;
#33236 = CARTESIAN_POINT ( 'NONE',  ( -1.364683531250014514, 1.738541667008085545, -0.7879004041258289570 ) ) ;
#33237 = VECTOR ( 'NONE', #56520, 1000.000000000000000 ) ;
#33238 = CARTESIAN_POINT ( 'NONE',  ( 5.009901455449552010, 5.803638771901306725, -1.199719254218452047 ) ) ;
#33239 = CARTESIAN_POINT ( 'NONE',  ( 3.040462492942562545, 2.144887288335277198, 0.2678724578094940356 ) ) ;
#33240 = CARTESIAN_POINT ( 'NONE',  ( 6.610000000000028741, 4.695285100415147461, 2.562642482393460597 ) ) ;
#33243 = DIRECTION ( 'NONE',  ( 0.6507913734559627184, -0.7592566023653016805, 0.000000000000000000 ) ) ;
#33242 = CARTESIAN_POINT ( 'NONE',  ( -6.518203450479830963, 5.167241622962447600, -2.437504649502885812 ) ) ;
#33241 = CARTESIAN_POINT ( 'NONE',  ( 3.237364818613055473, 6.998952398349030268, -1.734723475976807094E-15 ) ) ;
#33244 = CARTESIAN_POINT ( 'NONE',  ( 7.890482213029013536, 12.14938698193514277, 1.040834085586084257E-14 ) ) ;
#33245 = CARTESIAN_POINT ( 'NONE',  ( -7.845789747616925602, -6.699703214240756211, 7.710100441483631606 ) ) ;
#33246 = CARTESIAN_POINT ( 'NONE',  ( -8.514157279702036618, 9.035531035848267223, -0.7216878364870278340 ) ) ;
#33247 = CARTESIAN_POINT ( 'NONE',  ( 0.6619992422990974568, 1.085049530943157148, 1.904046507712559455 ) ) ;
#33248 = CARTESIAN_POINT ( 'NONE',  ( 0.4020909550005648536, 7.366597533580820034, 1.962779437971595931 ) ) ;
#33249 = CARTESIAN_POINT ( 'NONE',  ( 1.165308694782108301, -2.046298710749935079, -0.9655196508330918803 ) ) ;
#33250 = CARTESIAN_POINT ( 'NONE',  ( -8.667740277838301921, 9.006785167099828016, -0.7998128361456291469 ) ) ;
#33251 = CARTESIAN_POINT ( 'NONE',  ( -4.650083499362882122, 6.448183387388563226, 1.443375672974064550 ) ) ;
#33252 = CARTESIAN_POINT ( 'NONE',  ( -1.364683531249997417, 2.821875000341422801, 1.214306433183764966E-14 ) ) ;
#33253 = CARTESIAN_POINT ( 'NONE',  ( 4.594471896879979589, 8.374412622790375238, -0.01639726577711345112 ) ) ;
#33254 = CARTESIAN_POINT ( 'NONE',  ( -1.402160292154681736E-14, 11.06250000000000355, 1.732050807568881190 ) ) ;
#33255 = CARTESIAN_POINT ( 'NONE',  ( 3.040771591214902259, 6.769593633051179005, -0.7998128361456362523 ) ) ;
#33256 = CARTESIAN_POINT ( 'NONE',  ( 3.514700139928600198, 1.598748483301600354, 0.7592613872578843903 ) ) ;
#33257 = B_SPLINE_CURVE_WITH_KNOTS ( 'NONE', 3,
 ( #160575, #122317, #88667, #154727, #84382, #136350, #86515, #36686 ),
 .UNSPECIFIED., .F., .F.,
 ( 4, 2, 2, 4 ),
 ( 7.043516722447106004E-16, 0.0002305131806122208513, 0.0004610263612237373507, 0.0009220527224467680184 ),
 .UNSPECIFIED. ) ;
#33258 = CARTESIAN_POINT ( 'NONE',  ( 6.018643902988223715, 1.486383190695803158, -1.631276885294789203 ) ) ;
#33259 = CARTESIAN_POINT ( 'NONE',  ( -1.364683531250000748, 14.92187500034139447, 0.000000000000000000 ) ) ;
#33260 = ORIENTED_EDGE ( 'NONE', *, *, #66919, .F. ) ;
#33261 = CARTESIAN_POINT ( 'NONE',  ( -5.692444392891315097, 7.734547439830227411, -1.599625672291271394 ) ) ;
#33262 = CARTESIAN_POINT ( 'NONE',  ( 5.571888728144736902, -0.9040954357531080232, 1.802425742427179012 ) ) ;
#33263 = EDGE_LOOP ( 'NONE', ( #160788, #202164 ) ) ;
#33264 = CARTESIAN_POINT ( 'NONE',  ( 2.658895327995167701, -1.626580691111864985, -0.9237732865615968514 ) ) ;
#33265 = CARTESIAN_POINT ( 'NONE',  ( 3.555589372526322567, 1.629040189086952140, 1.277421477176057252 ) ) ;
#33266 = CARTESIAN_POINT ( 'NONE',  ( -6.522881301506166629, 9.663759714182251770, 1.082531754730549967 ) ) ;
#33267 = CARTESIAN_POINT ( 'NONE',  ( 2.390748813209525814, -1.831196095803063528, -0.5514187292172747501 ) ) ;
#33268 = FILL_AREA_STYLE ('',( #180589 ) ) ;
#33269 = CARTESIAN_POINT ( 'NONE',  ( -10.81659741420782872, 5.544487526538591560, -6.534070432124610583 ) ) ;
#33270 = CARTESIAN_POINT ( 'NONE',  ( -0.09916492693111574053, -9.919999999999998153, -9.499482423651645746 ) ) ;
#33271 = CARTESIAN_POINT ( 'NONE',  ( 1.364683531249990311, 4.696875000341417916, 1.214306433183764966E-14 ) ) ;
#33272 = CARTESIAN_POINT ( 'NONE',  ( 1.125099709691119276, 1.687896996356451629, 0.8989547360247207575 ) ) ;
#33273 = CARTESIAN_POINT ( 'NONE',  ( 5.180624094197585627, 8.097792972322238825, -1.082531754730548412 ) ) ;
#33274 = CARTESIAN_POINT ( 'NONE',  ( 2.576550507925364109, 1.283677811227203147, -1.483670167215108693 ) ) ;
#33275 = CARTESIAN_POINT ( 'NONE',  ( -6.518203450479830963, 5.167241622962448488, -2.437504649502885368 ) ) ;
#33276 = CARTESIAN_POINT ( 'NONE',  ( -6.283277845290492714, 6.295188672452495915, -0.7998128361456362523 ) ) ;
#33277 = CARTESIAN_POINT ( 'NONE',  ( 5.449516625918088053, -1.916229881892789866, 0.9086369058012438993 ) ) ;
#33278 = CARTESIAN_POINT ( 'NONE',  ( 9.073431116043567002, 11.60875560684942265, -1.599625672291262513 ) ) ;
#33279 = CARTESIAN_POINT ( 'NONE',  ( 6.450460791689297757, 0.6159929566152704261, 1.872736359496610659 ) ) ;
#33280 = CARTESIAN_POINT ( 'NONE',  ( -1.364683531250012516, 2.030208333674750953, 0.7879004041258379498 ) ) ;
#33281 = CARTESIAN_POINT ( 'NONE',  ( 2.127199591969671122, 1.800101769773830185, 0.9015413830680671925 ) ) ;
#33283 = CARTESIAN_POINT ( 'NONE',  ( 1.511481539699152776, -1.992283995360244253, 0.7168839309619617906 ) ) ;
#33282 = CARTESIAN_POINT ( 'NONE',  ( -8.202319746587722449, 8.671720580548228696, 1.040834085586084257E-14 ) ) ;
#33285 = EDGE_CURVE ( 'NONE', #56590, #155561, #183979, .T. ) ;
#33284 = CARTESIAN_POINT ( 'NONE',  ( 9.310341921297071721, 11.46515425228529494, -7.574253667434096116 ) ) ;
#33286 = CARTESIAN_POINT ( 'NONE',  ( 3.174344110969638866, -1.018096006688212096, -1.802650257252853772 ) ) ;
#33287 = CARTESIAN_POINT ( 'NONE',  ( 4.573896719763862251, 6.429575154514868274, -1.599625672291273171 ) ) ;
#33289 = CARTESIAN_POINT ( 'NONE',  ( 3.354752944377597856, 6.001296637494123232, -1.199719254218446718 ) ) ;
#33288 = CARTESIAN_POINT ( 'NONE',  ( 6.210894578592706772, -0.2570060295814159401, 2.074700711848826096 ) ) ;
#33291 = EDGE_LOOP ( 'NONE', ( #68939, #163624, #94778 ) ) ;
#33290 = CARTESIAN_POINT ( 'NONE',  ( 4.172732250082421324, -1.703408510751417193, -0.6570589383413026896 ) ) ;
#33292 = CARTESIAN_POINT ( 'NONE',  ( 8.594979316059474073, 12.11489407112305372, 1.199719254218450271 ) ) ;
#33293 = CARTESIAN_POINT ( 'NONE',  ( -1.284279953904132077, 2.878360285806111474, -0.7749999999999936939 ) ) ;
#33294 = CARTESIAN_POINT ( 'NONE',  ( 9.262911828397729863, 13.60048340123860200, -6.822320103072770259 ) ) ;
#33295 = CARTESIAN_POINT ( 'NONE',  ( 4.946401613871812764, 2.200551846729232430, 0.1665617540023768828 ) ) ;
#33296 = CARTESIAN_POINT ( 'NONE',  ( 0.6823417656249934904, 10.25520833367472839, 1.181850606188764807 ) ) ;
#33297 = ORIENTED_EDGE ( 'NONE', *, *, #20260, .F. ) ;
#33298 = CARTESIAN_POINT ( 'NONE',  ( 3.879479457080482696, 0.2311173251203814394, -1.898182577502210977 ) ) ;
#33299 = CARTESIAN_POINT ( 'NONE',  ( -9.134442807305063639, 11.67993591332117376, 1.599625672291281386 ) ) ;
#33300 = CARTESIAN_POINT ( 'NONE',  ( 7.806797523370503811, 8.002351953554066810, 1.040834085586084257E-14 ) ) ;
#33301 = CARTESIAN_POINT ( 'NONE',  ( -3.355169270512988773E-14, 1.234375000341463746, 1.570758158831764062 ) ) ;
#33302 = CARTESIAN_POINT ( 'NONE',  ( 3.985733972293228344, 7.593847367743336463, 1.040834085586084257E-14 ) ) ;
#33303 = CARTESIAN_POINT ( 'NONE',  ( 6.567925981381852907, -1.350348970527824211, 1.726830949945204363 ) ) ;
#33304 = CARTESIAN_POINT ( 'NONE',  ( 7.859932111734047488, 14.38583806649917918, -9.009653343056649888 ) ) ;
#33305 = CARTESIAN_POINT ( 'NONE',  ( 0.8020088176248600931, 1.394402496181508466, -1.202495849378336423 ) ) ;
#33306 = ORIENTED_EDGE ( 'NONE', *, *, #151300, .F. ) ;
#33307 = CARTESIAN_POINT ( 'NONE',  ( 11.86239285000045740, 9.719999999999982876, 1.812080536912751061 ) ) ;
#33308 = CARTESIAN_POINT ( 'NONE',  ( 5.290257391050456448, -1.856285702826396156, -0.2301478561287788605 ) ) ;
#33309 = DIRECTION ( 'NONE',  ( 0.000000000000000000, 0.000000000000000000, -1.000000000000000000 ) ) ;
#33310 = VECTOR ( 'NONE', #6600, 1000.000000000000000 ) ;
#33311 = DIRECTION ( 'NONE',  ( 0.000000000000000000, -1.000000000000000000, 0.000000000000000000 ) ) ;
#33313 = EDGE_CURVE ( 'NONE', #171893, #109221, #72658, .T. ) ;
#33312 =( BOUNDED_SURFACE ( )  B_SPLINE_SURFACE ( 1, 2, ( 
 ( #8205, #159793, #176063, #9280, #141465, #58029, #140385, #75352, #207473, #7122, #124193, #111113, #209585, #40732, #205330, #175003, #11396, #125252, #61231, #126314, #191213, #107924, #139301, #190156, #155543, #26589, #25522, #158736, #106838, #43935, #24440, #127386, #89488, #42876, #193359, #60159, #177117, #108984, #92690, #76405, #208523, #56968, #189099, #123141, #116432, #79609, #196566, #197613, #16717, #64432, #82802, #178192, #179260, #160870, #63366, #180318, #94819, #148878, #95894, #98022, #31938, #14592, #30882, #47138, #66519, #12464, #212794, #194426, #165126, #128458, #78539, #210671, #48208, #49257, #195502, #161947, #144656, #213845, #164077, #132662, #451, #32996, #46067, #114320, #81744, #62299, #130576, #145728, #15657, #112188, #211728, #80688, #198667, #96961, #50314, #29809, #13539, #115378, #65463, #147826, #28734, #131614, #181372, #129522, #99073, #113255, #163009, #146779, #38326, #137972, #154214, #51386, #17776, #87073, #70793, #86010, #117507, #20976, #102255, #83864, #153143, #4718, #133733, #149955, #35108, #53507, #101179, #1524, #203991, #167268, #183500, #186697, #118572, #67588, #104402, #185625, #136906, #152084, #119642, #84937, #202933, #54576, #170451, #120724, #168329, #36179, #22036, #37258, #88147, #5786, #199740, #18853, #71863, #151026, #52446, #2595, #55639, #182425, #100125, #34052, #68664, #201861, #166187, #134788, #200795, #184558, #19924, #103328, #3654, #69732, #135836, #169391, #57778, #207220, #159545, #92447, #58843, #91371, #6864, #141209, #126061, #192024, #25269, #56714, #43687, #157431, #77219, #72943, #90289, #205072, #187763, #125000, #105488, #206150, #39393, #7943, #190957, #74033, #122883, #173693, #188841, #107665, #106581, #109804, #172609, #139046, #40477, #175813, #171521, #24185, #42622, #41552, #10085, #174760, #156358, #23114, #140124, #123939, #108732, #27406, #189907, #9024, #75099, #143338, #26333, #158486, #76159, #142264, #208275, #59907, #93504, #155283, #11142, #209332, #121795, #89231, #12216, #194175, #129280, #146532, #211479 ),
 ( #160615, #127134, #28480, #14343, #18335, #60980, #13292, #84415, #34595, #68137, #46890, #95648, #62058, #128213, #134270, #78287, #79365, #151567, #111941, #80432, #150505, #51929, #96716, #118053, #210416, #63115, #193105, #161699, #212549, #44755, #184038, #45820, #130331, #64190, #113003, #195254, #145483, #101733, #110862, #30630, #144414, #200278, #177943, #176868, #94571, #196320, #2065, #179014, #29557, #162765, #100663, #47964, #167803, #35655, #19401, #114080, #180071, #166741, #85481, #187244, #120192, #72415, #69204, #186168, #203469, #123418, #5261, #189381, #152616, #4202, #89780, #188306, #38870, #57257, #106054, #104955, #70270, #155827, #169926, #41024, #20465, #73493, #173157, #107133, #86551, #52978, #122350, #172078, #121269, #136385, #56189, #137454, #119113, #39948, #23670, #168863, #185093, #202402, #88700, #7411, #90839, #54056, #139594, #205617, #71337, #55123, #37802, #103877, #170996, #22594, #135324, #21510, #24738, #3134, #87622, #36720, #154759, #201338, #6343, #102806, #153692, #138516, #204540, #74574, #43164, #8490, #27949, #109277, #11685, #174231, #45280, #91914, #111401, #59381, #142806, #62569, #159021, #128732, #157973, #9563, #29020, #127677, #126599, #210943, #177404, #192562, #75640, #95104, #175286, #194705, #25805, #12740, #112462, #46346, #141747, #206692, #61512, #161152, #60440, #207755, #209873, #76690, #58320, #193637, #78814, #108208, #124477, #125537, #94043, #144938, #30082, #191498, #178472, #156902, #10615, #208809, #26872, #92975, #44217, #110338, #140676, #176341, #190434, #42093, #160082, #77758, #143880, #116709, #15932, #150238, #132936, #98284, #114596, #13812, #196839, #162225, #181638, #48479, #165401, #113533, #198942, #31159, #50586, #96174, #180587, #182710, #66796, #100403, #82015, #130845, #97232, #163285, #166471, #195781, #32210, #183784, #147050, #49521, #34328, #84151, #131884, #1807, #14868, #164343, #79884, #148106, #33266, #145993, #67865, #80957, #16997, #99350, #214109, #65736, #197892, #134012, #212005, #115643, #47418, #18063, #179539 ) ),
 .UNSPECIFIED., .F., .F., .T. ) 
 B_SPLINE_SURFACE_WITH_KNOTS ( ( 2, 2 ),
 ( 3, 2, 2, 2, 2, 2, 2, 2, 2, 2, 2, 2, 2, 2, 2, 2, 2, 2, 2, 2, 2, 2, 2, 2, 2, 2, 2, 2, 2, 2, 2, 2, 2, 2, 2, 2, 2, 2, 2, 2, 2, 2, 2, 2, 2, 2, 2, 2, 2, 2, 2, 2, 2, 2, 2, 2, 2, 2, 2, 2, 2, 2, 2, 2, 2, 2, 2, 2, 2, 2, 2, 2, 2, 2, 2, 2, 2, 2, 2, 2, 2, 2, 2, 2, 2, 2, 2, 2, 2, 2, 2, 2, 2, 2, 2, 2, 2, 2, 2, 2, 2, 2, 2, 2, 2, 2, 2, 2, 2, 2, 2, 2, 2, 2, 2, 2, 2, 2, 2, 2, 3 ),
 ( 0.000000000000000000, 1.000000000000000000 ),
 ( 0.000000000000000000, 0.008333333333333333218, 0.01666666666666666644, 0.02500000000000000139, 0.03333333333333333287, 0.04166666666666666435, 0.05000000000000000278, 0.05833333333333333426, 0.06666666666666666574, 0.07499999999999999722, 0.08333333333333332871, 0.09166666666666666019, 0.1000000000000000056, 0.1083333333333333370, 0.1166666666666666685, 0.1250000000000000000, 0.1333333333333333315, 0.1416666666666666630, 0.1499999999999999944, 0.1583333333333333259, 0.1666666666666666574, 0.1749999999999999889, 0.1833333333333333204, 0.1916666666666666796, 0.2000000000000000111, 0.2083333333333333426, 0.2166666666666666741, 0.2250000000000000056, 0.2333333333333333370, 0.2416666666666666685, 0.2500000000000000000, 0.2583333333333333592, 0.2666666666666666630, 0.2750000000000000222, 0.2833333333333333259, 0.2916666666666666852, 0.2999999999999999889, 0.3083333333333333481, 0.3166666666666666519, 0.3250000000000000111, 0.3333333333333333148, 0.3416666666666666741, 0.3499999999999999778, 0.3583333333333333370, 0.3666666666666666408, 0.3750000000000000000, 0.3833333333333333592, 0.3916666666666666630, 0.4000000000000000222, 0.4083333333333333259, 0.4166666666666666852, 0.4249999999999999889, 0.4333333333333333481, 0.4416666666666666519, 0.4500000000000000111, 0.4583333333333333148, 0.4666666666666666741, 0.4749999999999999778, 0.4833333333333333370, 0.4916666666666666408, 0.5000000000000000000, 0.5083333333333333037, 0.5166666666666667185, 0.5250000000000000222, 0.5333333333333333259, 0.5416666666666666297, 0.5500000000000000444, 0.5583333333333333481, 0.5666666666666666519, 0.5749999999999999556, 0.5833333333333333703, 0.5916666666666666741, 0.5999999999999999778, 0.6083333333333332815, 0.6166666666666666963, 0.6250000000000000000, 0.6333333333333333037, 0.6416666666666667185, 0.6500000000000000222, 0.6583333333333333259, 0.6666666666666666297, 0.6750000000000000444, 0.6833333333333333481, 0.6916666666666666519, 0.6999999999999999556, 0.7083333333333333703, 0.7166666666666666741, 0.7249999999999999778, 0.7333333333333332815, 0.7416666666666666963, 0.7500000000000000000, 0.7583333333333333037, 0.7666666666666667185, 0.7750000000000000222, 0.7833333333333333259, 0.7916666666666666297, 0.8000000000000000444, 0.8083333333333333481, 0.8166666666666666519, 0.8249999999999999556, 0.8333333333333333703, 0.8416666666666666741, 0.8499999999999999778, 0.8583333333333332815, 0.8666666666666666963, 0.8750000000000000000, 0.8833333333333333037, 0.8916666666666667185, 0.9000000000000000222, 0.9083333333333333259, 0.9166666666666666297, 0.9250000000000000444, 0.9333333333333333481, 0.9416666666666666519, 0.9499999999999999556, 0.9583333333333333703, 0.9666666666666666741, 0.9749999999999999778, 0.9833333333333332815, 0.9916666666666666963, 1.000000000000000000 ),
 .UNSPECIFIED. ) 
 GEOMETRIC_REPRESENTATION_ITEM ( )  RATIONAL_B_SPLINE_SURFACE ( (
 ( 1.000000000000000000, 0.8660254037844387076, 1.000000000000000000, 0.8660254037844387076, 1.000000000000000000, 0.8660254037844387076, 1.000000000000000000, 0.8660254037844387076, 1.000000000000000000, 0.8660254037844387076, 1.000000000000000000, 0.8660254037844387076, 1.000000000000000000, 0.8660254037844387076, 1.000000000000000000, 0.8660254037844387076, 1.000000000000000000, 0.8660254037844387076, 1.000000000000000000, 0.8660254037844387076, 1.000000000000000000, 0.8660254037844387076, 1.000000000000000000, 0.8660254037844387076, 1.000000000000000000, 0.8660254037844387076, 1.000000000000000000, 0.8660254037844387076, 1.000000000000000000, 0.8660254037844387076, 1.000000000000000000, 0.8660254037844387076, 1.000000000000000000, 0.8660254037844387076, 1.000000000000000000, 0.8660254037844387076, 1.000000000000000000, 0.8660254037844387076, 1.000000000000000000, 0.8660254037844387076, 1.000000000000000000, 0.8660254037844387076, 1.000000000000000000, 0.8660254037844387076, 1.000000000000000000, 0.8660254037844387076, 1.000000000000000000, 0.8660254037844387076, 1.000000000000000000, 0.8660254037844387076, 1.000000000000000000, 0.8660254037844387076, 1.000000000000000000, 0.8660254037844387076, 1.000000000000000000, 0.8660254037844387076, 1.000000000000000000, 0.8660254037844387076, 1.000000000000000000, 0.8660254037844387076, 1.000000000000000000, 0.8660254037844387076, 1.000000000000000000, 0.8660254037844387076, 1.000000000000000000, 0.8660254037844387076, 1.000000000000000000, 0.8660254037844387076, 1.000000000000000000, 0.8660254037844387076, 1.000000000000000000, 0.8660254037844387076, 1.000000000000000000, 0.8660254037844387076, 1.000000000000000000, 0.8660254037844387076, 1.000000000000000000, 0.8660254037844387076, 1.000000000000000000, 0.8660254037844387076, 1.000000000000000000, 0.8660254037844387076, 1.000000000000000000, 0.8660254037844387076, 1.000000000000000000, 0.8660254037844387076, 1.000000000000000000, 0.8660254037844387076, 1.000000000000000000, 0.8660254037844387076, 1.000000000000000000, 0.8660254037844387076, 1.000000000000000000, 0.8660254037844387076, 1.000000000000000000, 0.8660254037844387076, 1.000000000000000000, 0.8660254037844387076, 1.000000000000000000, 0.8660254037844387076, 1.000000000000000000, 0.8660254037844387076, 1.000000000000000000, 0.8660254037844387076, 1.000000000000000000, 0.8660254037844387076, 1.000000000000000000, 0.8660254037844387076, 1.000000000000000000, 0.8660254037844387076, 1.000000000000000000, 0.8660254037844387076, 1.000000000000000000, 0.8660254037844387076, 1.000000000000000000, 0.8660254037844387076, 1.000000000000000000, 0.8660254037844387076, 1.000000000000000000, 0.8660254037844387076, 1.000000000000000000, 0.8660254037844387076, 1.000000000000000000, 0.8660254037844387076, 1.000000000000000000, 0.8660254037844387076, 1.000000000000000000, 0.8660254037844387076, 1.000000000000000000, 0.8660254037844387076, 1.000000000000000000, 0.8660254037844387076, 1.000000000000000000, 0.8660254037844387076, 1.000000000000000000, 0.8660254037844387076, 1.000000000000000000, 0.8660254037844387076, 1.000000000000000000, 0.8660254037844387076, 1.000000000000000000, 0.8660254037844387076, 1.000000000000000000, 0.8660254037844387076, 1.000000000000000000, 0.8660254037844387076, 1.000000000000000000, 0.8660254037844387076, 1.000000000000000000, 0.8660254037844387076, 1.000000000000000000, 0.8660254037844387076, 1.000000000000000000, 0.8660254037844387076, 1.000000000000000000, 0.8660254037844387076, 1.000000000000000000, 0.8660254037844387076, 1.000000000000000000, 0.8660254037844387076, 1.000000000000000000, 0.8660254037844387076, 1.000000000000000000, 0.8660254037844387076, 1.000000000000000000, 0.8660254037844387076, 1.000000000000000000, 0.8660254037844387076, 1.000000000000000000, 0.8660254037844387076, 1.000000000000000000, 0.8660254037844387076, 1.000000000000000000, 0.8660254037844387076, 1.000000000000000000, 0.8660254037844387076, 1.000000000000000000, 0.8660254037844387076, 1.000000000000000000, 0.8660254037844387076, 1.000000000000000000, 0.8660254037844387076, 1.000000000000000000, 0.8660254037844387076, 1.000000000000000000, 0.8660254037844387076, 1.000000000000000000, 0.8660254037844387076, 1.000000000000000000, 0.8660254037844387076, 1.000000000000000000, 0.8660254037844387076, 1.000000000000000000, 0.8660254037844387076, 1.000000000000000000, 0.8660254037844387076, 1.000000000000000000, 0.8660254037844387076, 1.000000000000000000, 0.8660254037844387076, 1.000000000000000000, 0.8660254037844387076, 1.000000000000000000, 0.8660254037844387076, 1.000000000000000000, 0.8660254037844387076, 1.000000000000000000, 0.8660254037844387076, 1.000000000000000000, 0.8660254037844387076, 1.000000000000000000, 0.8660254037844387076, 1.000000000000000000, 0.8660254037844387076, 1.000000000000000000, 0.8660254037844387076, 1.000000000000000000, 0.8660254037844387076, 1.000000000000000000, 0.8660254037844387076, 1.000000000000000000, 0.8660254037844387076, 1.000000000000000000, 0.8660254037844387076, 1.000000000000000000, 0.8660254037844387076, 1.000000000000000000, 0.8660254037844387076, 1.000000000000000000, 0.8660254037844387076, 1.000000000000000000, 0.8660254037844387076, 1.000000000000000000, 0.8660254037844387076, 1.000000000000000000, 0.8660254037844387076, 1.000000000000000000, 0.8660254037844387076, 1.000000000000000000, 0.8660254037844387076, 1.000000000000000000),
 ( 1.000000000000000000, 0.8660254037844387076, 1.000000000000000000, 0.8660254037844387076, 1.000000000000000000, 0.8660254037844387076, 1.000000000000000000, 0.8660254037844387076, 1.000000000000000000, 0.8660254037844387076, 1.000000000000000000, 0.8660254037844387076, 1.000000000000000000, 0.8660254037844387076, 1.000000000000000000, 0.8660254037844387076, 1.000000000000000000, 0.8660254037844387076, 1.000000000000000000, 0.8660254037844387076, 1.000000000000000000, 0.8660254037844387076, 1.000000000000000000, 0.8660254037844387076, 1.000000000000000000, 0.8660254037844387076, 1.000000000000000000, 0.8660254037844387076, 1.000000000000000000, 0.8660254037844387076, 1.000000000000000000, 0.8660254037844387076, 1.000000000000000000, 0.8660254037844387076, 1.000000000000000000, 0.8660254037844387076, 1.000000000000000000, 0.8660254037844387076, 1.000000000000000000, 0.8660254037844387076, 1.000000000000000000, 0.8660254037844387076, 1.000000000000000000, 0.8660254037844387076, 1.000000000000000000, 0.8660254037844387076, 1.000000000000000000, 0.8660254037844387076, 1.000000000000000000, 0.8660254037844387076, 1.000000000000000000, 0.8660254037844387076, 1.000000000000000000, 0.8660254037844387076, 1.000000000000000000, 0.8660254037844387076, 1.000000000000000000, 0.8660254037844387076, 1.000000000000000000, 0.8660254037844387076, 1.000000000000000000, 0.8660254037844387076, 1.000000000000000000, 0.8660254037844387076, 1.000000000000000000, 0.8660254037844387076, 1.000000000000000000, 0.8660254037844387076, 1.000000000000000000, 0.8660254037844387076, 1.000000000000000000, 0.8660254037844387076, 1.000000000000000000, 0.8660254037844387076, 1.000000000000000000, 0.8660254037844387076, 1.000000000000000000, 0.8660254037844387076, 1.000000000000000000, 0.8660254037844387076, 1.000000000000000000, 0.8660254037844387076, 1.000000000000000000, 0.8660254037844387076, 1.000000000000000000, 0.8660254037844387076, 1.000000000000000000, 0.8660254037844387076, 1.000000000000000000, 0.8660254037844387076, 1.000000000000000000, 0.8660254037844387076, 1.000000000000000000, 0.8660254037844387076, 1.000000000000000000, 0.8660254037844387076, 1.000000000000000000, 0.8660254037844387076, 1.000000000000000000, 0.8660254037844387076, 1.000000000000000000, 0.8660254037844387076, 1.000000000000000000, 0.8660254037844387076, 1.000000000000000000, 0.8660254037844387076, 1.000000000000000000, 0.8660254037844387076, 1.000000000000000000, 0.8660254037844387076, 1.000000000000000000, 0.8660254037844387076, 1.000000000000000000, 0.8660254037844387076, 1.000000000000000000, 0.8660254037844387076, 1.000000000000000000, 0.8660254037844387076, 1.000000000000000000, 0.8660254037844387076, 1.000000000000000000, 0.8660254037844387076, 1.000000000000000000, 0.8660254037844387076, 1.000000000000000000, 0.8660254037844387076, 1.000000000000000000, 0.8660254037844387076, 1.000000000000000000, 0.8660254037844387076, 1.000000000000000000, 0.8660254037844387076, 1.000000000000000000, 0.8660254037844387076, 1.000000000000000000, 0.8660254037844387076, 1.000000000000000000, 0.8660254037844387076, 1.000000000000000000, 0.8660254037844387076, 1.000000000000000000, 0.8660254037844387076, 1.000000000000000000, 0.8660254037844387076, 1.000000000000000000, 0.8660254037844387076, 1.000000000000000000, 0.8660254037844387076, 1.000000000000000000, 0.8660254037844387076, 1.000000000000000000, 0.8660254037844387076, 1.000000000000000000, 0.8660254037844387076, 1.000000000000000000, 0.8660254037844387076, 1.000000000000000000, 0.8660254037844387076, 1.000000000000000000, 0.8660254037844387076, 1.000000000000000000, 0.8660254037844387076, 1.000000000000000000, 0.8660254037844387076, 1.000000000000000000, 0.8660254037844387076, 1.000000000000000000, 0.8660254037844387076, 1.000000000000000000, 0.8660254037844387076, 1.000000000000000000, 0.8660254037844387076, 1.000000000000000000, 0.8660254037844387076, 1.000000000000000000, 0.8660254037844387076, 1.000000000000000000, 0.8660254037844387076, 1.000000000000000000, 0.8660254037844387076, 1.000000000000000000, 0.8660254037844387076, 1.000000000000000000, 0.8660254037844387076, 1.000000000000000000, 0.8660254037844387076, 1.000000000000000000, 0.8660254037844387076, 1.000000000000000000, 0.8660254037844387076, 1.000000000000000000, 0.8660254037844387076, 1.000000000000000000, 0.8660254037844387076, 1.000000000000000000, 0.8660254037844387076, 1.000000000000000000, 0.8660254037844387076, 1.000000000000000000, 0.8660254037844387076, 1.000000000000000000, 0.8660254037844387076, 1.000000000000000000, 0.8660254037844387076, 1.000000000000000000, 0.8660254037844387076, 1.000000000000000000, 0.8660254037844387076, 1.000000000000000000, 0.8660254037844387076, 1.000000000000000000, 0.8660254037844387076, 1.000000000000000000, 0.8660254037844387076, 1.000000000000000000, 0.8660254037844387076, 1.000000000000000000, 0.8660254037844387076, 1.000000000000000000, 0.8660254037844387076, 1.000000000000000000, 0.8660254037844387076, 1.000000000000000000, 0.8660254037844387076, 1.000000000000000000, 0.8660254037844387076, 1.000000000000000000, 0.8660254037844387076, 1.000000000000000000, 0.8660254037844387076, 1.000000000000000000, 0.8660254037844387076, 1.000000000000000000, 0.8660254037844387076, 1.000000000000000000, 0.8660254037844387076, 1.000000000000000000, 0.8660254037844387076, 1.000000000000000000, 0.8660254037844387076, 1.000000000000000000) ) ) 
 REPRESENTATION_ITEM ( '' )  SURFACE ( )  );
#33314 = CARTESIAN_POINT ( 'NONE',  ( -5.572037945536512105, 9.444535336527177805, 0.000000000000000000 ) ) ;
#33315 = AXIS2_PLACEMENT_3D ( 'NONE', #194564, #178340, #96034 ) ;
#33316 = CARTESIAN_POINT ( 'NONE',  ( 4.741601036477289810, 6.554953847355395880, 1.599625672291267398 ) ) ;
#33317 = CARTESIAN_POINT ( 'NONE',  ( 1.112081256596690437, 1.967444819121874744, -0.09107992038001262725 ) ) ;
#33318 = CARTESIAN_POINT ( 'NONE',  ( 1.845327587665198443, 0.3419125196015109225, -1.987051676161588620 ) ) ;
#33319 = CARTESIAN_POINT ( 'NONE',  ( -9.104463846776669200, 10.58062822844965645, -1.199719254218441611 ) ) ;
#33320 = CARTESIAN_POINT ( 'NONE',  ( 5.936491157937257235, 8.019268665717216749, 1.599625672291268286 ) ) ;
#33321 = CARTESIAN_POINT ( 'NONE',  ( 6.727182134110200273, 0.5640974741700152117, 2.241195997201197443 ) ) ;
#33322 = CARTESIAN_POINT ( 'NONE',  ( 2.818527994553555516, 2.063739945100159900, 0.7375456357434084786 ) ) ;
#33323 = CARTESIAN_POINT ( 'NONE',  ( 5.936143289257818978, 0.8957264799932495025, -1.590785280889392528 ) ) ;
#33324 = CARTESIAN_POINT ( 'NONE',  ( -10.48453286206953727, 11.12637651536962125, 0.7998128361456462443 ) ) ;
#33325 = DIRECTION ( 'NONE',  ( 0.000000000000000000, 0.000000000000000000, -1.000000000000000000 ) ) ;
#33326 = CARTESIAN_POINT ( 'NONE',  ( 4.204437034013637664, 6.958908068774287692, -1.082531754730548412 ) ) ;
#33327 = CARTESIAN_POINT ( 'NONE',  ( 8.585337585951586803, 11.03931315507545108, -1.599625672291255185 ) ) ;
#33328 = CARTESIAN_POINT ( 'NONE',  ( 4.390142812726693045, 4.016254791136236513, 1.214306433183764966E-14 ) ) ;
#33329 = CARTESIAN_POINT ( 'NONE',  ( 7.078765600110826561, 8.391552967285011988, -1.082531754730548412 ) ) ;
#33330 = ORIENTED_EDGE ( 'NONE', *, *, #199925, .F. ) ;
#33332 = CARTESIAN_POINT ( 'NONE',  ( 0.9439945835589347300, -1.278642754803262171, -1.554848376591860815 ) ) ;
#33331 = CARTESIAN_POINT ( 'NONE',  ( 4.774869596704574448, 1.716175909155163382, -0.6674964387535023969 ) ) ;
#33333 = CARTESIAN_POINT ( 'NONE',  ( 2.952824900933643804, 1.623659768481898302, 1.626969957801235989 ) ) ;
#33335 = CARTESIAN_POINT ( 'NONE',  ( 1.059155247252058896, 1.517088508067988117, 1.077460967357747990 ) ) ;
#33334 = DIRECTION ( 'NONE',  ( -0.6507913734559642727, 0.7592566023653003482, 2.775557561562893816E-17 ) ) ;
#33336 = CARTESIAN_POINT ( 'NONE',  ( 3.285556943750000514, -3.113541666188709645, 1.896917185911906500 ) ) ;
#33337 = CARTESIAN_POINT ( 'NONE',  ( -3.469997250093771246, 6.135748327496311383, -1.199719254218452935 ) ) ;
#33338 = CARTESIAN_POINT ( 'NONE',  ( 4.207966135563082410, 7.175396087857926375, -2.420000000000000373 ) ) ;
#33339 = CARTESIAN_POINT ( 'NONE',  ( 4.605663860560767375, 1.420894170025093439, 1.280184534114735095 ) ) ;
#33340 = CARTESIAN_POINT ( 'NONE',  ( -8.727698198895085469, 11.20540053684285553, -1.599625672291263179 ) ) ;
#33341 = CARTESIAN_POINT ( 'NONE',  ( -5.628043163448566588, 9.580151100749725757, 0.000000000000000000 ) ) ;
#33343 = CARTESIAN_POINT ( 'NONE',  ( 2.307302758404996545, -0.4121581357655336175, 1.824517092411604979 ) ) ;
#33342 = CARTESIAN_POINT ( 'NONE',  ( 3.228152448572230160, 2.040302950407224536, 0.4557642060307572907 ) ) ;
#33344 = CARTESIAN_POINT ( 'NONE',  ( 5.992340707560141588, 9.934888558888093968, 0.7216878364870438212 ) ) ;
#33345 = CARTESIAN_POINT ( 'NONE',  ( -0.6823417656250212460, 5.113541667008086655, 1.181850606188767472 ) ) ;
#33346 = CARTESIAN_POINT ( 'NONE',  ( 6.128435733830499998, 0.1874100934057248424, 1.831705376836203936 ) ) ;
#33347 = CARTESIAN_POINT ( 'NONE',  ( 3.195971524519376494, 4.751719416737803847, -1.599625672291262513 ) ) ;
#33349 = CARTESIAN_POINT ( 'NONE',  ( 4.976006071415387311, 5.764094157194782575, 1.199719254218462483 ) ) ;
#33348 = CARTESIAN_POINT ( 'NONE',  ( 5.843238758086321205, 6.086642049024201917, 0.6823498365625046969 ) ) ;
#33350 = CARTESIAN_POINT ( 'NONE',  ( 4.705503516419368815, -0.4560151319670002756, 1.663429522189649790 ) ) ;
#33351 = CARTESIAN_POINT ( 'NONE',  ( -5.930802130974132780, 9.006687355190106103, -1.199719254218440723 ) ) ;
#33352 = CARTESIAN_POINT ( 'NONE',  ( 0.5626190647941519130, -0.9651924803987484980, 1.440457774218842690 ) ) ;
#33353 =( LENGTH_UNIT ( ) NAMED_UNIT ( * ) SI_UNIT ( .MILLI., .METRE. ) );
#33354 = CARTESIAN_POINT ( 'NONE',  ( -10.33433454857960321, 4.766519530047388820, -5.444264161973041638 ) ) ;
#33355 = CIRCLE ( 'NONE', #16014, 0.7500000000000011102 ) ;
#33356 = CARTESIAN_POINT ( 'NONE',  ( 4.557605255626766549, 1.740051450181074877, 1.298158460866901454 ) ) ;
#33357 = CARTESIAN_POINT ( 'NONE',  ( 3.791466046568803705, 1.323482414808102137, 1.257835202898072380 ) ) ;
#33358 = CARTESIAN_POINT ( 'NONE',  ( 1.498799732657706718, 0.3773721054241683248, 1.924948185394937283 ) ) ;
#33359 = CARTESIAN_POINT ( 'NONE',  ( 5.823477710672365859, -1.535350753823118586, -1.458276433397849514 ) ) ;
#33361 = CARTESIAN_POINT ( 'NONE',  ( 0.6823417656249899377, 4.488541667008086655, -1.181850606188754593 ) ) ;
#33360 = CARTESIAN_POINT ( 'NONE',  ( 6.146038201015474378, 0.7148980135479511278, 2.178090959246486324 ) ) ;
#33362 = CARTESIAN_POINT ( 'NONE',  ( 7.703003830858588863, 12.13858823597705872, -0.7998128361456291469 ) ) ;
#33363 = VECTOR ( 'NONE', #147215, 1000.000000000000000 ) ;
#33364 = CARTESIAN_POINT ( 'NONE',  ( 1.717596852896427606, 1.764750374324057347, 1.175337852406685757 ) ) ;
#33365 = CARTESIAN_POINT ( 'NONE',  ( -4.284013352238250860, 7.941839977679187257, -0.7216878364870267237 ) ) ;
#33366 = CARTESIAN_POINT ( 'NONE',  ( -3.960390268523300339, 7.634556056670224855, 1.214306433183764966E-14 ) ) ;
#33367 = CARTESIAN_POINT ( 'NONE',  ( -5.721177634842498527, 5.777054783512106440, 0.000000000000000000 ) ) ;
#33368 = CARTESIAN_POINT ( 'NONE',  ( 6.280164127638760085, -1.199209930833704085, -1.809645864181265384 ) ) ;
#33370 = CARTESIAN_POINT ( 'NONE',  ( 1.500000000000001332, 12.65625000068279427, 0.000000000000000000 ) ) ;
#33369 = CARTESIAN_POINT ( 'NONE',  ( 6.883263157960362477, -0.004191378316371896506, 2.053658919477070910 ) ) ;
#33372 = ORIENTED_EDGE ( 'NONE', *, *, #130785, .T. ) ;
#33371 = CARTESIAN_POINT ( 'NONE',  ( 1.840792944257110042, 1.275724102719773434, -1.818268329069183897 ) ) ;
#33373 = CARTESIAN_POINT ( 'NONE',  ( 6.258435431136967431, 1.928752767684217106, -0.5880170417187426946 ) ) ;
#33375 = CARTESIAN_POINT ( 'NONE',  ( 4.293840196874755044, -1.418639180022958080, -1.497458912744116022 ) ) ;
#33374 = CARTESIAN_POINT ( 'NONE',  ( 3.714044015139744914, 6.420469553383295391, 1.199719254218462483 ) ) ;
#33377 = CARTESIAN_POINT ( 'NONE',  ( -0.2409995289980003397, 4.087843961663322645, -2.555282842491034323 ) ) ;
#33376 = CARTESIAN_POINT ( 'NONE',  ( 4.692003678781083487, 7.631698837623355658, -1.199719254218450271 ) ) ;
#33378 = CARTESIAN_POINT ( 'NONE',  ( 4.864343252252968597, 8.897093904262280972, 0.000000000000000000 ) ) ;
#33379 = CARTESIAN_POINT ( 'NONE',  ( -3.285556943749998737, -4.017708332855375986, 1.896917185911908499 ) ) ;
#33380 = CARTESIAN_POINT ( 'NONE',  ( -0.7500000000000006661, 12.70833333333333570, -1.299038105676657340 ) ) ;
#33381 = CARTESIAN_POINT ( 'NONE',  ( 0.2168896333464042925, -0.1002974801882359490, 2.088354908755992945 ) ) ;
#33382 = CARTESIAN_POINT ( 'NONE',  ( 4.599059095968327071, -0.4863373063577690059, 1.775805238918099382 ) ) ;
#33383 = CIRCLE ( 'NONE', #154467, 0.08000000000000001554 ) ;
#33385 = VERTEX_POINT ( 'NONE', #186406 ) ;
#33384 = CARTESIAN_POINT ( 'NONE',  ( 6.003563092752934871, 5.898578451166879510, 0.7998128361456341429 ) ) ;
#33386 =( NAMED_UNIT ( * ) SI_UNIT ( $, .STERADIAN. ) SOLID_ANGLE_UNIT ( ) );
#33387 = CARTESIAN_POINT ( 'NONE',  ( 1.852176121455822777, 0.5370312411601232405, 1.639109186831126053 ) ) ;
#33388 = CARTESIAN_POINT ( 'NONE',  ( 0.4373225248172890045, -5.223431457505089526, 10.96785329849812385 ) ) ;
#33389 = CARTESIAN_POINT ( 'NONE',  ( 1.618275512070939115, 0.2312369868452644750, 2.287056861988717493 ) ) ;
#33390 = CARTESIAN_POINT ( 'NONE',  ( -1.364683531250010295, 4.592708333674755394, 0.7879004041258379498 ) ) ;
#33391 = CARTESIAN_POINT ( 'NONE',  ( 1.458695031449417590, 0.9167444482420561425, 2.068505399879524642 ) ) ;
#33392 = CARTESIAN_POINT ( 'NONE',  ( 4.617860632714274161, -2.065554989951523535, 0.4101935312739966588 ) ) ;
#33393 = CARTESIAN_POINT ( 'NONE',  ( -4.930325137224961907, 5.781076077297750970, -1.199719254218453823 ) ) ;
#33394 = CARTESIAN_POINT ( 'NONE',  ( 2.776313302798124383, -1.692206278411222176, -0.5179841425143881795 ) ) ;
#33395 = CARTESIAN_POINT ( 'NONE',  ( 7.233438648090761980, 8.397765496649418182, 1.199719254218462483 ) ) ;
#33396 = CARTESIAN_POINT ( 'NONE',  ( 5.194182247366869731, 7.153241603385088965, 1.443375672974064550 ) ) ;
#33397 = CARTESIAN_POINT ( 'NONE',  ( -4.713430959045263435, 8.650753218861462202, 0.7998128361456481317 ) ) ;
#33398 = CARTESIAN_POINT ( 'NONE',  ( 4.975479186090839612, 8.748550117173898855, 0.7216878364870438212 ) ) ;
#33399 = CARTESIAN_POINT ( 'NONE',  ( 1.499999999999987121, 1.754166666666691521, 0.8660254037844524744 ) ) ;
#33400 = CARTESIAN_POINT ( 'NONE',  ( -4.796887421136680985, 4.490790167614548523, 1.214306433183764966E-14 ) ) ;
#33401 = CARTESIAN_POINT ( 'NONE',  ( 4.904621534589208132, -2.204716393758818782, -0.2710871420372409912 ) ) ;
#33402 = CARTESIAN_POINT ( 'NONE',  ( 3.750093249908572623, 0.7883579158753216687, 2.044908353623323016 ) ) ;
#33403 = CARTESIAN_POINT ( 'NONE',  ( -4.238895582566952314, 8.097128612970093897, 1.040834085586084257E-14 ) ) ;
#33404 = CARTESIAN_POINT ( 'NONE',  ( -3.149236820124241110, 6.896136400112061970, -0.7998128361456481317 ) ) ;
#33405 = CARTESIAN_POINT ( 'NONE',  ( 5.619825546450978315, -0.5151785252428126016, 2.056841324599982368 ) ) ;
#33406 =( BOUNDED_CURVE ( )  B_SPLINE_CURVE ( 2, ( #168176, #2438, #116284, #1376, #67437 ),
 .UNSPECIFIED., .F., .T. ) 
 B_SPLINE_CURVE_WITH_KNOTS ( ( 3, 2, 3 ),
 ( 0.000000000000000000, 0.01041666666666666609, 0.01562500000000010061 ),
 .UNSPECIFIED. ) 
 CURVE ( )  GEOMETRIC_REPRESENTATION_ITEM ( )  RATIONAL_B_SPLINE_CURVE ( ( 1.000000000000000000, 0.8660254037844387076, 1.000000000000000000, 0.9330127018922180770, 0.9330127018922194093 ) ) 
 REPRESENTATION_ITEM ( '' )  );
#33407 = CARTESIAN_POINT ( 'NONE',  ( -1.364683531250012516, 3.280208333674756727, 0.7879004041258379498 ) ) ;
#33408 = CARTESIAN_POINT ( 'NONE',  ( 6.609999999999999432, 2.404169510734831761, 2.660384318335922149 ) ) ;
#33409 = CARTESIAN_POINT ( 'NONE',  ( -2.968872451712654126, 6.407508927065978632, 1.040834085586084257E-14 ) ) ;
#33410 = CARTESIAN_POINT ( 'NONE',  ( 5.308877466510794285, -0.5174029350529658622, -2.056363676157816123 ) ) ;
#33411 = CARTESIAN_POINT ( 'NONE',  ( -6.672020991700860826, 7.917017590806697314, 1.082531754730549078 ) ) ;
#33412 = ORIENTED_EDGE ( 'NONE', *, *, #101217, .T. ) ;
#33414 = CARTESIAN_POINT ( 'NONE',  ( 6.579002408576895000, -0.1006694238701970334, -2.159482418181729813 ) ) ;
#33413 = CARTESIAN_POINT ( 'NONE',  ( -4.665414256878301025, 6.536345614481700927, -1.443375672974066548 ) ) ;
#33415 = CARTESIAN_POINT ( 'NONE',  ( 4.843287188579786573, 6.673587691474970107, -1.599625672291256295 ) ) ;
#33416 = CARTESIAN_POINT ( 'NONE',  ( 6.058133912487986272, -1.297239342979487509, 1.306937132449899508 ) ) ;
#33417 = UNCERTAINTY_MEASURE_WITH_UNIT (LENGTH_MEASURE( 1.000000000000000082E-05 ), #37663, 'distance_accuracy_value', 'NONE');
#33418 = FILL_AREA_STYLE_COLOUR ( '', #151805 ) ;
#33419 = CARTESIAN_POINT ( 'NONE',  ( -0.6823417656250212460, 2.863541667008084879, 1.181850606188767472 ) ) ;
#33420 = CARTESIAN_POINT ( 'NONE',  ( 1.434671803396998291, -1.260233744827907953, -1.200652698350104686 ) ) ;
#33421 = CARTESIAN_POINT ( 'NONE',  ( 2.184835310096557404, 5.700724961754617404, 1.040834085586084257E-14 ) ) ;
#33422 = CARTESIAN_POINT ( 'NONE',  ( -1.500000000000001110, 11.30208333401612997, 0.8660254037844418162 ) ) ;
#33423 = CARTESIAN_POINT ( 'NONE',  ( -1.402160292154681736E-14, -0.6156249996585817508, 1.575800808251672791 ) ) ;
#33424 = DIRECTION ( 'NONE',  ( -1.000000000000000000, 5.578564026256504688E-16, -1.232595164407830946E-31 ) ) ;
#33425 = ADVANCED_FACE ( 'NONE', ( #166984 ), #196687, .T. ) ;
#33426 = CARTESIAN_POINT ( 'NONE',  ( 5.102478102407745908, -0.7247817745383768884, -2.036717088958202471 ) ) ;
#33427 = CARTESIAN_POINT ( 'NONE',  ( -2.300079615812729905, 5.835176651756807331, -0.7998128361456281477 ) ) ;
#33428 = CARTESIAN_POINT ( 'NONE',  ( -7.497295758232736418, 7.849192594134070333, -0.7216878364870267237 ) ) ;
#33429 = CARTESIAN_POINT ( 'NONE',  ( 4.540002997438313592, 0.9271085556134452954, -1.952944755896801610 ) ) ;
#33431 = ORIENTED_EDGE ( 'NONE', *, *, #105631, .T. ) ;
#33430 = CARTESIAN_POINT ( 'NONE',  ( -5.334207092333882017, 5.187939460669764635, 0.7998128361456281477 ) ) ;
#33432 = CARTESIAN_POINT ( 'NONE',  ( 1.364683531249988535, 3.613541667008086211, 0.7879004041258500513 ) ) ;
#33433 = CARTESIAN_POINT ( 'NONE',  ( 5.483651708025924165, 1.321867191758316462, 1.462689542499737039 ) ) ;
#33434 = CARTESIAN_POINT ( 'NONE',  ( 5.413366682498521598, 0.5056653987138818307, 1.658472451074376242 ) ) ;
#33436 = CARTESIAN_POINT ( 'NONE',  ( 1.663894474538109236, 1.130263417742288112, 1.877492182091732076 ) ) ;
#33435 = CARTESIAN_POINT ( 'NONE',  ( 0.6801582343749692505, -0.5260416663252707181, 1.178068619123786132 ) ) ;
#33437 = CARTESIAN_POINT ( 'NONE',  ( 1.993646994336109257, 2.007229749184535450, -1.138263614794749801 ) ) ;
#33438 = CARTESIAN_POINT ( 'NONE',  ( 4.516905262009872857, 1.882569317753344240, 0.8387543118332175807 ) ) ;
#33439 = CARTESIAN_POINT ( 'NONE',  ( 6.614805133705309537, -0.1285734799129842065, 1.912263277720785970 ) ) ;
#33440 = CARTESIAN_POINT ( 'NONE',  ( -7.171900071504748730, 8.429933507252760805, -1.082531754730549078 ) ) ;
#33441 = CARTESIAN_POINT ( 'NONE',  ( -4.359828915246279024, 7.244161613499399799, -1.199719254218455378 ) ) ;
#33442 = LINE ( 'NONE', #195955, #5662 ) ;
#33443 = CARTESIAN_POINT ( 'NONE',  ( 4.394861267144759331, -2.057662932662501110, -0.5123870273424437904 ) ) ;
#33444 = CARTESIAN_POINT ( 'NONE',  ( 1.108046318188542489, -0.04667474159409169127, 2.016033875899234662 ) ) ;
#33445 = CARTESIAN_POINT ( 'NONE',  ( -7.836249598574384301, 8.244638741199329601, 1.040834085586084257E-14 ) ) ;
#33446 = CARTESIAN_POINT ( 'NONE',  ( 4.717920652503574175, -2.164970738276258189, 0.4266498443898231185 ) ) ;
#33447 = CARTESIAN_POINT ( 'NONE',  ( -1.642778471874998480, -1.188541666188709600, 2.845375778867863303 ) ) ;
#33448 = CARTESIAN_POINT ( 'NONE',  ( 1.408744241983818757, 3.463408486559384603, -0.5205678189275573242 ) ) ;
#33449 = DIRECTION ( 'NONE',  ( 0.000000000000000000, 0.000000000000000000, 1.000000000000000000 ) ) ;
#33450 = CARTESIAN_POINT ( 'NONE',  ( 3.627755783104286813, 3.517448670773187125, -2.500000000000000444 ) ) ;
#33453 = AXIS2_PLACEMENT_3D ( 'NONE', #171538, #72961, #23130 ) ;
#33452 = CARTESIAN_POINT ( 'NONE',  ( -0.008622031262367491067, 15.44736672593548299, 11.95585889282746450 ) ) ;
#33451 = CARTESIAN_POINT ( 'NONE',  ( -5.203215198707511036, 7.836405505866204102, -1.276579466623083858 ) ) ;
#33454 = VERTEX_POINT ( 'NONE', #3376 ) ;
#33455 = CARTESIAN_POINT ( 'NONE',  ( 3.432544477427549534, 2.010279954523132240, 0.4531449079418439774 ) ) ;
#33456 = CARTESIAN_POINT ( 'NONE',  ( -5.358255402162534516E-14, 1.328125000341440431, -1.570758158831820239 ) ) ;
#33457 = UNCERTAINTY_MEASURE_WITH_UNIT (LENGTH_MEASURE( 1.000000000000000082E-05 ), #151033, 'distance_accuracy_value', 'NONE');
#33458 = CARTESIAN_POINT ( 'NONE',  ( -4.530395885260773525, 8.437212299446219532, 0.7998128361456481317 ) ) ;
#33459 = CARTESIAN_POINT ( 'NONE',  ( 3.018227828326583762, -2.017275923677069205, 0.1012127129823153504 ) ) ;
#33460 = CARTESIAN_POINT ( 'NONE',  ( -1.402160292154681736E-14, -0.9124999999999769962, -1.732050807568870754 ) ) ;
#33461 = CARTESIAN_POINT ( 'NONE',  ( 2.361091307074211887, 5.906356958228550447, 0.7998128361456462443 ) ) ;
#33462 = CARTESIAN_POINT ( 'NONE',  ( 1.797801859905317823, -0.6954313725856995365, 1.940136720205553278 ) ) ;
#33463 = DIRECTION ( 'NONE',  ( 8.638326563840814399E-31, 0.000000000000000000, 1.000000000000000000 ) ) ;
#33464 = CARTESIAN_POINT ( 'NONE',  ( 6.518772930072240790, 6.499656594706071822, -0.7998128361456281477 ) ) ;
#33466 = ORIENTED_EDGE ( 'NONE', *, *, #53547, .T. ) ;
#33465 = CARTESIAN_POINT ( 'NONE',  ( -0.2408018239684642792, 0.2331886253038339407, -2.134526469895109635 ) ) ;
#33467 = CARTESIAN_POINT ( 'NONE',  ( 1.798526679444776954, 1.530131497970032450, 1.023642133485637595 ) ) ;
#33468 = EDGE_CURVE ( 'NONE', #180652, #213748, #140991, .T. ) ;
#33469 = CARTESIAN_POINT ( 'NONE',  ( 0.2062968637084483525, -0.6088960595307371104, 2.225859948526871079 ) ) ;
#33470 = CARTESIAN_POINT ( 'NONE',  ( 7.198453214212898743, 7.362893269528701268, 0.7998128361456291469 ) ) ;
#33471 = CARTESIAN_POINT ( 'NONE',  ( 1.968271169257681752, 1.109365460190291586, 1.855047589327807778 ) ) ;
#33472 = CARTESIAN_POINT ( 'NONE',  ( -4.311129659465605002, 4.131998812239033647, 0.7216878364870317197 ) ) ;
#33473 = CARTESIAN_POINT ( 'NONE',  ( 2.360564879530482330, -1.931125380751706810, -0.5807522007576990664 ) ) ;
#33474 = CARTESIAN_POINT ( 'NONE',  ( 2.196985159075715011, -1.500492831465898513, -1.741107174271120384 ) ) ;
#33475 = AXIS2_PLACEMENT_3D ( 'NONE', #83487, #118197, #151715 ) ;
#33476 = DIRECTION ( 'NONE',  ( 2.439454888092378666E-14, 0.000000000000000000, 1.000000000000000000 ) ) ;
#33477 = CARTESIAN_POINT ( 'NONE',  ( 0.1099206271272800961, -0.7955684105149689600, -1.691499381818922343 ) ) ;
#33478 = CARTESIAN_POINT ( 'NONE',  ( 11.41108574530281672, 11.25836855377622392, 3.405883542057599911 ) ) ;
#33479 = CARTESIAN_POINT ( 'NONE',  ( 4.276219423538512032, -1.135946514926335915, 1.611120745738093385 ) ) ;
#33480 = CARTESIAN_POINT ( 'NONE',  ( 3.098842478760281516, 1.825076540557273974, 0.8578426345753201732 ) ) ;
#33483 = EDGE_CURVE ( 'NONE', #22427, #19657, #213960, .T. ) ;
#33482 = CARTESIAN_POINT ( 'NONE',  ( 9.205623113554615600, 11.76297960394566466, 1.443375672974076540 ) ) ;
#33481 = CARTESIAN_POINT ( 'NONE',  ( 1.364683531249990311, 2.634375000341422801, 1.214306433183764966E-14 ) ) ;
#33485 = CARTESIAN_POINT ( 'NONE',  ( 6.305314546112477103, 1.749969596565099650, 1.171488565500600654 ) ) ;
#33484 = CARTESIAN_POINT ( 'NONE',  ( -6.581593504430098385, 9.765943957555402122, -1.199719254218440723 ) ) ;
#33486 = CARTESIAN_POINT ( 'NONE',  ( 4.809070886388271404, -1.664838503569150419, 1.230558894880565246 ) ) ;
#33487 = CARTESIAN_POINT ( 'NONE',  ( 7.470706336329915764, 8.674577799595093452, -1.199719254218441611 ) ) ;
#33488 = CARTESIAN_POINT ( 'NONE',  ( -7.088215381846223906, 7.164006121775713609, 0.7998128361456341429 ) ) ;
#33489 = CARTESIAN_POINT ( 'NONE',  ( -1.452308200714708342, 8.721976639181708180, 2.576600914284036037 ) ) ;
#33490 = CARTESIAN_POINT ( 'NONE',  ( 4.939715878566554252, -1.916525930768823383, 0.6376727893300809802 ) ) ;
#33491 = CARTESIAN_POINT ( 'NONE',  ( -0.6823417656249969321, 5.717708333674756283, -1.181850606188749264 ) ) ;
#33492 = CARTESIAN_POINT ( 'NONE',  ( 3.580997583313150212, -2.223846063185720645, -0.6162045312432282707 ) ) ;
#33493 = CARTESIAN_POINT ( 'NONE',  ( 1.094667215044333952, 2.031392189445472063, 0.3564975109212295545 ) ) ;
#33494 = CARTESIAN_POINT ( 'NONE',  ( 6.805829924380097040, 10.88395931184472154, 0.7216878364870438212 ) ) ;
#33495 = CARTESIAN_POINT ( 'NONE',  ( 7.126746022638799971, 8.343567110280638133, 1.199719254218452047 ) ) ;
#33496 = CARTESIAN_POINT ( 'NONE',  ( 4.929271367020211514, 7.908511140569038922, 1.199719254218452047 ) ) ;
#33497 = CARTESIAN_POINT ( 'NONE',  ( 1.364683531249988757, 0.9468750003414211358, 0.000000000000000000 ) ) ;
#33498 = CARTESIAN_POINT ( 'NONE',  ( 6.215487077222150880, 6.216099443039444949, 0.000000000000000000 ) ) ;
#33499 = CARTESIAN_POINT ( 'NONE',  ( 7.429504990164394584, 7.770103364721017591, 1.040834085586084257E-14 ) ) ;
#33501 = DIRECTION ( 'NONE',  ( -0.5994789404140901112, 2.055006554627987857E-15, 0.8003905296791060664 ) ) ;
#33500 = CARTESIAN_POINT ( 'NONE',  ( 3.578747896202236323, 1.379726198893852729, -1.676393335895840497 ) ) ;
#33502 = CARTESIAN_POINT ( 'NONE',  ( 0.000000000000000000, 0.000000000000000000, 0.000000000000000000 ) ) ;
#33504 = CARTESIAN_POINT ( 'NONE',  ( 2.770863647982471534, 1.747605724785822767, -0.5798694457997202178 ) ) ;
#33503 = CARTESIAN_POINT ( 'NONE',  ( -3.456965981804629884, 6.976951378839947537, 1.040834085586084257E-14 ) ) ;
#33505 = CARTESIAN_POINT ( 'NONE',  ( -1.364683531250010295, 4.530208333674754506, 0.7879004041258379498 ) ) ;
#33506 = CARTESIAN_POINT ( 'NONE',  ( 4.546525781634036534, -1.759932548463913671, 1.305750774140898685 ) ) ;
#33507 = DIRECTION ( 'NONE',  ( 0.000000000000000000, 1.000000000000000000, 0.000000000000000000 ) ) ;
#33508 = CARTESIAN_POINT ( 'NONE',  ( 5.049841537476964959, 0.7145653451936549994, -2.146778123354900814 ) ) ;
#33509 = CARTESIAN_POINT ( 'NONE',  ( -5.594971466091354095, 6.350553869658721595, -1.210626573312810761 ) ) ;
#33510 = CARTESIAN_POINT ( 'NONE',  ( 5.504185490526544378, 7.460110003252303557, -1.249659907641489820 ) ) ;
#33511 = CARTESIAN_POINT ( 'NONE',  ( -6.251718229232867685, 6.466295153626015590, -0.7216878364870338292 ) ) ;
#33512 = CARTESIAN_POINT ( 'NONE',  ( 5.411112705629925301, 5.485588709422586362, 0.000000000000000000 ) ) ;
#33513 = CARTESIAN_POINT ( 'NONE',  ( 6.257089712715798058, -1.519072588978742200, -0.9077291607378096261 ) ) ;
#33514 = AXIS2_PLACEMENT_3D ( 'NONE', #139362, #53829, #187014 ) ;
#33515 = CARTESIAN_POINT ( 'NONE',  ( 4.477201648280199286, -1.799136850145161892, -0.9032412251695760563 ) ) ;
#33516 = CARTESIAN_POINT ( 'NONE',  ( 6.662942426112080874, 9.860851032851066122, 1.199719254218460707 ) ) ;
#33517 = CARTESIAN_POINT ( 'NONE',  ( 2.784315802839703036, -1.083654668052931536, 1.805616322045165312 ) ) ;
#33518 = CARTESIAN_POINT ( 'NONE',  ( 0.5267775621587212909, -1.642505510697172655, 0.9855279480080190169 ) ) ;
#33519 = CARTESIAN_POINT ( 'NONE',  ( 4.546061579283848353, 4.198160018786257552, -0.7998128361456211532 ) ) ;
#33520 = CARTESIAN_POINT ( 'NONE',  ( 2.207411625193840266, -1.579985490969371575, -1.175680343436244391 ) ) ;
#33521 = CARTESIAN_POINT ( 'NONE',  ( 0.7076149179639171782, -1.862046558926268913, 0.1791945732521060819 ) ) ;
#33522 = CARTESIAN_POINT ( 'NONE',  ( 1.012071980069819910, 1.959787197952606252, -0.09269708818125664551 ) ) ;
#33524 = VERTEX_POINT ( 'NONE', #85715 ) ;
#33523 = CARTESIAN_POINT ( 'NONE',  ( 0.05278957052760185897, 0.3289079202175131389, 1.883742972368242174 ) ) ;
#33525 = CARTESIAN_POINT ( 'NONE',  ( 5.341549334104188418, 7.254893527920112994, 1.443375672974062551 ) ) ;
#33526 = AXIS2_PLACEMENT_3D ( 'NONE', #63822, #16112, #117973 ) ;
#33527 = CARTESIAN_POINT ( 'NONE',  ( -1.364683531250000748, 0.3218750003414205807, 0.000000000000000000 ) ) ;
#33528 = CARTESIAN_POINT ( 'NONE',  ( 6.403191318657627029, 1.556466930477506505, 1.037356966126230517 ) ) ;
#33529 = DIRECTION ( 'NONE',  ( -5.551115123125765446E-17, 0.000000000000000000, 1.000000000000000000 ) ) ;
#33530 = CARTESIAN_POINT ( 'NONE',  ( 6.930528400284448054, -1.278709912597691511, 1.628784411136071197 ) ) ;
#33531 = CARTESIAN_POINT ( 'NONE',  ( -7.346809171966454777, -6.836568542494980250, -8.002408263930250953 ) ) ;
#33532 = CARTESIAN_POINT ( 'NONE',  ( 1.328672132201724532, -1.314895749051579132, 1.599177317581280455 ) ) ;
#33533 = CARTESIAN_POINT ( 'NONE',  ( 1.499999999999985123, 0.2958333333333566517, -0.8660254037844323793 ) ) ;
#33534 = CARTESIAN_POINT ( 'NONE',  ( 7.311924916471702396, 7.425000578838787391, -0.7998128361456281477 ) ) ;
#33535 = CARTESIAN_POINT ( 'NONE',  ( -6.828502922777144768, 11.11833717654868892, 0.7998128361456481317 ) ) ;
#33536 = CARTESIAN_POINT ( 'NONE',  ( 5.662465432362883355, 6.635239754958710989, 1.199719254218451159 ) ) ;
#33537 = CARTESIAN_POINT ( 'NONE',  ( 5.918629486560170960, -0.7630358368452618834, -1.978611909900826582 ) ) ;
#33538 = CARTESIAN_POINT ( 'NONE',  ( 4.923546060418115822, 5.773167154356443120, -1.199719254218452047 ) ) ;
#33539 = CARTESIAN_POINT ( 'NONE',  ( -1.364683531250000748, 1.009375000341421247, 0.000000000000000000 ) ) ;
#33540 = CARTESIAN_POINT ( 'NONE',  ( -1.201851678989727383E-14, 2.962500000000025224, 1.732050807568877637 ) ) ;
#33542 = CARTESIAN_POINT ( 'NONE',  ( 5.118366684358879759, 5.930181538962194132, 1.199719254218462483 ) ) ;
#33541 = CARTESIAN_POINT ( 'NONE',  ( 6.408651779211167465, 0.6141799454031526828, 1.863335524608072502 ) ) ;
#33543 = CARTESIAN_POINT ( 'NONE',  ( 2.829453700430568652, -1.392333688140505510, 1.458332250898628057 ) ) ;
#33544 = CARTESIAN_POINT ( 'NONE',  ( 3.450306162294475065, -1.282734793626014280, 1.423081227541162841 ) ) ;
#33545 = CARTESIAN_POINT ( 'NONE',  ( 11.86239285000045918, 9.799999999999997158, -1.812080536912752837 ) ) ;
#33546 = CARTESIAN_POINT ( 'NONE',  ( 1.189316404147572337, 1.662717542896676504, 1.427817766309902314 ) ) ;
#33547 = CARTESIAN_POINT ( 'NONE',  ( 0.2335667940003048615, 5.721530573166598188, -2.747389403444942868 ) ) ;
#33548 = CARTESIAN_POINT ( 'NONE',  ( 3.092876253348992410, 1.606159189733218140, -0.9584765265276545820 ) ) ;
#33549 = CARTESIAN_POINT ( 'NONE',  ( 0.7499999999999867883, -1.152083332650516434, -1.299038105676652011 ) ) ;
#33550 = CARTESIAN_POINT ( 'NONE',  ( -8.019811557683421910, 9.315200557840817908, 1.199719254218462483 ) ) ;
#33552 = CARTESIAN_POINT ( 'NONE',  ( 5.325823331840044084, 0.8572517883133590200, -1.936080889991494747 ) ) ;
#33551 = CARTESIAN_POINT ( 'NONE',  ( -3.958617665510279160, 5.641473247893851628, -1.443375672974053447 ) ) ;
#33554 = EDGE_CURVE ( 'NONE', #184431, #18108, #61717, .T. ) ;
#33553 = CARTESIAN_POINT ( 'NONE',  ( 1.364683531250000303, 8.817708333674731946, -0.7879004041258355073 ) ) ;
#33555 = CARTESIAN_POINT ( 'NONE',  ( 6.777786256569462431, -2.009253640576996514, 0.4989836931604470505 ) ) ;
#33557 = DIRECTION ( 'NONE',  ( -0.000000000000000000, -1.000000000000000000, -0.000000000000000000 ) ) ;
#33556 = CARTESIAN_POINT ( 'NONE',  ( 2.612926333352751929, -0.2020284733853395243, 2.080942194061443651 ) ) ;
#33559 = ORIENTED_EDGE ( 'NONE', *, *, #37862, .F. ) ;
#33558 = CARTESIAN_POINT ( 'NONE',  ( 1.131409910074301806, -1.089654060068695252, -1.336973495911207843 ) ) ;
#33560 = CARTESIAN_POINT ( 'NONE',  ( 5.829115978871627135, 8.888053511070525659, 1.199719254218462483 ) ) ;
#33561 = CARTESIAN_POINT ( 'NONE',  ( 9.242769546185929386, 14.19339224059835658, 7.653689390903365641 ) ) ;
#33562 = CARTESIAN_POINT ( 'NONE',  ( 0.1216811705908975721, 2.536982183874236352, -1.996294991408742003 ) ) ;
#33563 = CARTESIAN_POINT ( 'NONE',  ( -9.857181934075960328, 5.275265258315555705, 6.218892358987248237 ) ) ;
#33564 = CARTESIAN_POINT ( 'NONE',  ( 5.924549939047454750, 9.855799328956630134, -0.7216878364870267237 ) ) ;
#33565 = CARTESIAN_POINT ( 'NONE',  ( 8.917737905728804648, 3.038492715500545227, 8.029567276306215362 ) ) ;
#33567 = CARTESIAN_POINT ( 'NONE',  ( 0.9260600326868747567, -0.8135480099433598511, -1.618595788997332363 ) ) ;
#33566 = CARTESIAN_POINT ( 'NONE',  ( 6.530187263637528439, 7.647581891445782709, -1.199719254218452047 ) ) ;
#33568 = CARTESIAN_POINT ( 'NONE',  ( -7.694415870955439551, 8.935572256658169010, 1.199719254218462483 ) ) ;
#33569 = CARTESIAN_POINT ( 'NONE',  ( 3.842846474469570062, 6.570739089268092137, -1.199719254218452047 ) ) ;
#33570 = CARTESIAN_POINT ( 'NONE',  ( -5.984664909832329904, 7.106694798503815136, 1.079546468792412783 ) ) ;
#33571 = CARTESIAN_POINT ( 'NONE',  ( 5.027041095616958444, 9.086908054853605421, 0.000000000000000000 ) ) ;
#33572 = CARTESIAN_POINT ( 'NONE',  ( 6.539320575229274901, 7.053161517996441532, 2.494893549996656912 ) ) ;
#33573 = DIRECTION ( 'NONE',  ( 0.000000000000000000, 0.000000000000000000, -1.000000000000000000 ) ) ;
#33574 = CARTESIAN_POINT ( 'NONE',  ( 9.499668754385625746, -7.215597533182398493, 0.07933194154557826616 ) ) ;
#33575 = CARTESIAN_POINT ( 'NONE',  ( 9.083599731475983319, 11.62061899152058686, 1.443375672974076540 ) ) ;
#33576 = CARTESIAN_POINT ( 'NONE',  ( 2.629178708315405455, 0.09452080204645990635, -1.858793618116144186 ) ) ;
#33577 = CARTESIAN_POINT ( 'NONE',  ( 0.6146668332816725977, 0.1418531279011990553, 1.910429497406636479 ) ) ;
#33578 = CARTESIAN_POINT ( 'NONE',  ( 6.352563997503644977, 0.6048113787208497794, 1.829064924511276002 ) ) ;
#33579 = CARTESIAN_POINT ( 'NONE',  ( -1.843739406749240750, 8.923774302061360686, 0.7750000000000013545 ) ) ;
#33580 = CARTESIAN_POINT ( 'NONE',  ( 4.607663176575717223, 8.357619647684677133, 0.2284409323990380658 ) ) ;
#33581 = DIRECTION ( 'NONE',  ( 4.440892098500630106E-16, 3.330669073875473073E-16, 1.000000000000000000 ) ) ;
#33582 = CARTESIAN_POINT ( 'NONE',  ( -3.470524135418300737, 6.032400010421219427, -1.082531754730549967 ) ) ;
#33583 = CARTESIAN_POINT ( 'NONE',  ( 8.432808358020015049, 11.82173160345663376, 1.082531754730546636 ) ) ;
#33584 = CARTESIAN_POINT ( 'NONE',  ( 5.137539950512164388, 1.839066438578255136, -0.7051811603524612559 ) ) ;
#33586 = CARTESIAN_POINT ( 'NONE',  ( 1.225412164737609055, 1.871785320780447792, 0.9964087003688710809 ) ) ;
#33585 = B_SPLINE_CURVE_WITH_KNOTS ( 'NONE', 3,
 ( #97028, #116500, #51449, #118636, #200856, #81811, #134850, #101247 ),
 .UNSPECIFIED., .F., .F.,
 ( 4, 2, 2, 4 ),
 ( 1.951563910473858677E-18, 0.0002925934901276177539, 0.0005851869802552335563, 0.001170373960510464294 ),
 .UNSPECIFIED. ) ;
#33587 = CARTESIAN_POINT ( 'NONE',  ( -5.880485940025243607, 7.883652901494672349, 1.599625672291269396 ) ) ;
#33588 = CARTESIAN_POINT ( 'NONE',  ( -11.29661021673627097, 7.648989264017080458, 3.919569178588850455 ) ) ;
#33589 = CARTESIAN_POINT ( 'NONE',  ( -1.347971487989957070E-14, -2.712500000000000355, 3.475000000000000089 ) ) ;
#33590 = CARTESIAN_POINT ( 'NONE',  ( 5.947271710577298087, 0.6394180277670692414, -2.096098967930816848 ) ) ;
#33591 = DIRECTION ( 'NONE',  ( 0.000000000000000000, 0.000000000000000000, 1.000000000000000000 ) ) ;
#33592 = CARTESIAN_POINT ( 'NONE',  ( 4.014609399936463596, 1.362939121162042078, -1.361637018764590534 ) ) ;
#33593 = CARTESIAN_POINT ( 'NONE',  ( -6.989391883044787868, 8.113044270762433285, -1.199719254218446718 ) ) ;
#33594 = CARTESIAN_POINT ( 'NONE',  ( -0.3282377607281426468, 2.261164550367422255, -1.225000000000034062 ) ) ;
#33595 = CARTESIAN_POINT ( 'NONE',  ( 1.102499568101540817, -2.207063161980229005, 0.003256074490760872773 ) ) ;
#33596 = DIRECTION ( 'NONE',  ( 0.000000000000000000, -0.000000000000000000, 1.000000000000000000 ) ) ;
#33597 =( BOUNDED_SURFACE ( )  B_SPLINE_SURFACE ( 3, 2, ( 
 ( #76946, #209064, #210137 ),
 ( #26064, #78020, #60701 ),
 ( #92177, #143071, #58579 ),
 ( #175543, #107396, #158227 ) ),
 .UNSPECIFIED., .F., .F., .T. ) 
 B_SPLINE_SURFACE_WITH_KNOTS ( ( 4, 4 ),
 ( 3, 3 ),
 ( 0.01127358803094578865, 0.01374177962974961961 ),
 ( 0.000000000000000000, 1.000000000000000000 ),
 .UNSPECIFIED. ) 
 GEOMETRIC_REPRESENTATION_ITEM ( )  RATIONAL_B_SPLINE_SURFACE ( (
 ( 1.000000000000000000, 0.6947640035331666963, 1.000000000000000000),
 ( 1.000000000000000000, 0.6955505939615598265, 1.000000000000000000),
 ( 1.000000000000000000, 0.6961913616428399010, 1.000000000000000000),
 ( 1.000000000000000000, 0.6967468848049991337, 1.000000000000000000) ) ) 
 REPRESENTATION_ITEM ( '' )  SURFACE ( )  );
#33598 = ORIENTED_EDGE ( 'NONE', *, *, #144618, .T. ) ;
#33599 = CYLINDRICAL_SURFACE ( 'NONE', #37536, 0.08000000000000020983 ) ;
#33600 = ORIENTED_EDGE ( 'NONE', *, *, #132620, .T. ) ;
#33601 = CARTESIAN_POINT ( 'NONE',  ( 5.893399327195629311, -1.782088370946652622, 0.8386133760364660183 ) ) ;
#33602 = CARTESIAN_POINT ( 'NONE',  ( 1.768985407559420020, 1.857901784229658793, -0.5654475766003872472 ) ) ;
#33603 = AXIS2_PLACEMENT_3D ( 'NONE', #210829, #31042, #97118 ) ;
#33604 = CARTESIAN_POINT ( 'NONE',  ( 0.2278875137335881207, -1.799627942332830965, -0.9090566646320766830 ) ) ;
#33606 = CARTESIAN_POINT ( 'NONE',  ( 4.891365455385704664, -1.702569429429393599, 0.7516348641289184451 ) ) ;
#33605 = CARTESIAN_POINT ( 'NONE',  ( -7.065734331377342414, 8.272386803808890576, -1.199719254218452047 ) ) ;
#33607 = CARTESIAN_POINT ( 'NONE',  ( 5.338878628731272613, 9.450718510153643948, -0.7998128361456481317 ) ) ;
#33608 = FILL_AREA_STYLE_COLOUR ( '', #181507 ) ;
#33609 = CARTESIAN_POINT ( 'NONE',  ( 3.757017964762656703, 7.397288368949487491, -1.734723475976807094E-15 ) ) ;
#33610 = CARTESIAN_POINT ( 'NONE',  ( -6.392833124043511894, 7.417059051927569868, 1.199719254218450271 ) ) ;
#33611 = CARTESIAN_POINT ( 'NONE',  ( -3.358905459982799879, -0.9385608918593922878, 0.07968368524804914088 ) ) ;
#33612 = CARTESIAN_POINT ( 'NONE',  ( 0.5389544483674936215, -1.876709678404146153, 1.131566444868239874 ) ) ;
#33613 = CARTESIAN_POINT ( 'NONE',  ( 5.016153647376212277, 5.914896012436124728, 1.082531754730558626 ) ) ;
#33614 = ORIENTED_EDGE ( 'NONE', *, *, #46133, .F. ) ;
#33615 = DIRECTION ( 'NONE',  ( -1.000000000000000000, 0.000000000000000000, 1.465138070926357285E-17 ) ) ;
#33616 = CARTESIAN_POINT ( 'NONE',  ( -2.927345865710862366E-15, -5.221050908132846224, -10.98765602437502764 ) ) ;
#33617 = CARTESIAN_POINT ( 'NONE',  ( 1.365546509989667534, 1.798985258052044900, -0.3101867277976525505 ) ) ;
#33618 = CARTESIAN_POINT ( 'NONE',  ( -4.436542580169821726, 6.199052314996659874, 1.599625672291267398 ) ) ;
#33619 = CARTESIAN_POINT ( 'NONE',  ( 3.269848819717678712, 1.566352396371019973, -0.7445194440909275180 ) ) ;
#33620 = CARTESIAN_POINT ( 'NONE',  ( -6.041797769283476782, 7.151762567314746022, -1.181783516275588752 ) ) ;
#33621 = CARTESIAN_POINT ( 'NONE',  ( 6.609000000000036401, 1.265604115953523845, 2.115306440354140172 ) ) ;
#33622 = CARTESIAN_POINT ( 'NONE',  ( 9.622536337397022521, 12.24937836509514710, 1.599625672291281386 ) ) ;
#33623 = CARTESIAN_POINT ( 'NONE',  ( 6.568987803155795113, -1.671525225137669102, -0.7347104647430282576 ) ) ;
#33624 = CARTESIAN_POINT ( 'NONE',  ( 4.328923052438288899, -1.828919189252835142, -0.7100325158947775606 ) ) ;
#33625 = CARTESIAN_POINT ( 'NONE',  ( -8.799405390469187793, 10.22472669609091689, -1.199719254218446718 ) ) ;
#33626 = CARTESIAN_POINT ( 'NONE',  ( 5.449487677688982679, 8.445153826357429949, -1.199719254218446718 ) ) ;
#33627 = CARTESIAN_POINT ( 'NONE',  ( 4.617906949270495609, -0.5647423089508787353, 2.043846993246847710 ) ) ;
#33628 = CARTESIAN_POINT ( 'NONE',  ( -6.984421689334302741, 11.30024240419870374, 0.000000000000000000 ) ) ;
#33629 = CARTESIAN_POINT ( 'NONE',  ( 6.609000000000020414, 4.695354556932705314, 2.562644781943985706 ) ) ;
#33630 = CARTESIAN_POINT ( 'NONE',  ( 2.571216573722459486, 1.847313327574741315, 0.9347662400437593000 ) ) ;
#33631 = CARTESIAN_POINT ( 'NONE',  ( 1.364683531249986537, -0.03229166632525094088, -0.7879004041258309554 ) ) ;
#33632 = ORIENTED_EDGE ( 'NONE', *, *, #25909, .F. ) ;
#33633 = CARTESIAN_POINT ( 'NONE',  ( 2.444286548701213757, -2.001697433659669567, -1.129998469374261072 ) ) ;
#33634 = CARTESIAN_POINT ( 'NONE',  ( 8.270110514656034084, 9.711179024262627024, 1.082531754730558626 ) ) ;
#33636 = CARTESIAN_POINT ( 'NONE',  ( -1.642778471874998480, -3.201041666188710000, 2.845375778867863303 ) ) ;
#33635 = CARTESIAN_POINT ( 'NONE',  ( 6.699137298928153683, 7.948653282571920720, 1.082531754730549967 ) ) ;
#33637 = CYLINDRICAL_SURFACE ( 'NONE', #54652, 11.99999999999999112 ) ;
#33638 = ORIENTED_EDGE ( 'NONE', *, *, #130663, .T. ) ;
#33639 = CARTESIAN_POINT ( 'NONE',  ( -5.593146208820614973, 6.196971745715879720, -0.8885217884838312319 ) ) ;
#33640 = CARTESIAN_POINT ( 'NONE',  ( 4.113462262696740979, 1.539102623358613586, 1.134910093507961237 ) ) ;
#33641 = DIRECTION ( 'NONE',  ( -2.345077562848777574E-16, 0.000000000000000000, -1.000000000000000000 ) ) ;
#33642 = CARTESIAN_POINT ( 'NONE',  ( 5.596639136713698726, -0.4230586844520961010, -1.671955901692462998 ) ) ;
#33643 = CARTESIAN_POINT ( 'NONE',  ( 3.749232653202066778, 0.2420323627391370025, -2.001857840249580800 ) ) ;
#33644 = CARTESIAN_POINT ( 'NONE',  ( 5.291695567192507887, 1.742433043099327561, -1.499359156687163575 ) ) ;
#33645 = CARTESIAN_POINT ( 'NONE',  ( -11.33772465723282785, 12.59131699265171989, -3.600000000000076472 ) ) ;
#33646 = CARTESIAN_POINT ( 'NONE',  ( 0.9794701899953797142, -0.05759512415488829418, -2.206297691287119722 ) ) ;
#33647 = CARTESIAN_POINT ( 'NONE',  ( -3.336715202739028552, 6.906935146588564223, 0.7216878364870338292 ) ) ;
#33648 = CARTESIAN_POINT ( 'NONE',  ( 5.465970981792784400, 0.8728298736929670509, 1.539401198699318352 ) ) ;
#33650 = CARTESIAN_POINT ( 'NONE',  ( 2.010137459244505820, -1.083026110817113086, -2.020279618534262855 ) ) ;
#33649 = CARTESIAN_POINT ( 'NONE',  ( 4.525389411911321602, 8.501647757197021704, -0.7998128361456381397 ) ) ;
#33651 = CARTESIAN_POINT ( 'NONE',  ( 6.580030785786400216, -1.806642183828395920, -0.3538341520857649081 ) ) ;
#33652 = CARTESIAN_POINT ( 'NONE',  ( -6.084577077482911101, 10.32070003369722144, 0.000000000000000000 ) ) ;
#33653 =( NAMED_UNIT ( * ) SI_UNIT ( $, .STERADIAN. ) SOLID_ANGLE_UNIT ( ) );
#33654 = CARTESIAN_POINT ( 'NONE',  ( -4.411198876399886615, 6.239761003923544713, -1.599625672291271394 ) ) ;
#33655 = DIRECTION ( 'NONE',  ( 0.000000000000000000, -1.000000000000000000, 0.000000000000000000 ) ) ;
#33656 = CARTESIAN_POINT ( 'NONE',  ( 0.6081839208269465002, 0.6806018353129331677, -2.061787349250172596 ) ) ;
#33657 = CARTESIAN_POINT ( 'NONE',  ( 2.571500236035813902, 1.429449181443824823, 1.422607194786096541 ) ) ;
#33658 = AXIS2_PLACEMENT_3D ( 'NONE', #7889, #21984, #25214 ) ;
#33659 = CARTESIAN_POINT ( 'NONE',  ( -1.500000000000015099, 0.1604166673494879791, -0.8660254037844383745 ) ) ;
#33660 = CARTESIAN_POINT ( 'NONE',  ( 5.180268977979770817, -1.068588414017849653, 1.602784418908353548 ) ) ;
#33661 = CARTESIAN_POINT ( 'NONE',  ( -0.6823417656250039265, 12.06770833367473017, -1.181850606188755259 ) ) ;
#33662 = CARTESIAN_POINT ( 'NONE',  ( 2.812952309885875746, -0.6487812942810657901, -2.124531788647378239 ) ) ;
#33663 = VERTEX_POINT ( 'NONE', #151801 ) ;
#33664 = CARTESIAN_POINT ( 'NONE',  ( 1.286956418854607431, 3.652345658002486672, 0.4592741676706121323 ) ) ;
#33665 = DIRECTION ( 'NONE',  ( 0.000000000000000000, 1.000000000000000000, 0.000000000000000000 ) ) ;
#33666 = CARTESIAN_POINT ( 'NONE',  ( 7.567422294721922960, 11.98040977715095323, 0.7998128361456462443 ) ) ;
#33667 = EDGE_CURVE ( 'NONE', #90832, #169159, #179693, .T. ) ;
#33668 = CARTESIAN_POINT ( 'NONE',  ( 0.000000000000000000, -4.500000000000003553, 0.000000000000000000 ) ) ;
#33669 = CARTESIAN_POINT ( 'NONE',  ( 4.054071295385909934, -1.286197829845928675, 1.172710138673456415 ) ) ;
#33671 = CARTESIAN_POINT ( 'NONE',  ( 3.350005920730843911, -0.7974703105717847462, 1.792663495558038056 ) ) ;
#33670 = VECTOR ( 'NONE', #155016, 1000.000000000000000 ) ;
#33673 = CARTESIAN_POINT ( 'NONE',  ( -5.585596099150174965, 9.460353182409786399, -0.7216878364870207285 ) ) ;
#33672 = CARTESIAN_POINT ( 'NONE',  ( 5.172599298813543633, 5.993452922492633839, -1.199719254218452047 ) ) ;
#33674 = EDGE_CURVE ( 'NONE', #76748, #157260, #29686, .T. ) ;
#33675 = CARTESIAN_POINT ( 'NONE',  ( -5.892944143475336460, 6.011535633345318708, 0.2346759862181871381 ) ) ;
#33676 = CARTESIAN_POINT ( 'NONE',  ( -11.37385970535894231, 1.000000000000000888, 3.825613075418397457 ) ) ;
#33677 = CARTESIAN_POINT ( 'NONE',  ( 1.029816311724339961, 1.988459969548944439, -0.5481627708354539497 ) ) ;
#33678 = CARTESIAN_POINT ( 'NONE',  ( -8.019811557683421910, 9.315200557840817908, 1.199719254218462483 ) ) ;
#33679 = CARTESIAN_POINT ( 'NONE',  ( -4.758548728272219641, 4.653987725846768342, 0.7216878364870317197 ) ) ;
#33680 = CARTESIAN_POINT ( 'NONE',  ( 0.6732104281652334654, -2.131434628316424273, -0.7592435237872022791 ) ) ;
#33681 = ORIENTED_EDGE ( 'NONE', *, *, #38690, .F. ) ;
#33682 = CARTESIAN_POINT ( 'NONE',  ( -0.7500000000000006661, 0.1395833340161536928, -1.299038105676652011 ) ) ;
#33683 = CARTESIAN_POINT ( 'NONE',  ( 2.512791842090915218, 1.668957736969980621, 0.8448945032545759348 ) ) ;
#33684 = CARTESIAN_POINT ( 'NONE',  ( 1.037308000539336694, -1.367553460919969543, 1.066146521862390673 ) ) ;
#33685 = CARTESIAN_POINT ( 'NONE',  ( 5.161759341795384870, 1.079763445194487970, 1.907048802792680631 ) ) ;
#33686 = CARTESIAN_POINT ( 'NONE',  ( 6.317414003067519879, -0.2912348092876380079, 2.289091032272353221 ) ) ;
#33687 = CARTESIAN_POINT ( 'NONE',  ( 1.217730312517154800, -2.010830008989676898, 0.4507304159913956831 ) ) ;
#33688 = CARTESIAN_POINT ( 'NONE',  ( 2.906119529042447969, 1.406244311732379293, -1.339499261486200465 ) ) ;
#33689 = MECHANICAL_DESIGN_GEOMETRIC_PRESENTATION_REPRESENTATION (  '', ( #168516 ), #147821 ) ;
#33690 = CARTESIAN_POINT ( 'NONE',  ( -5.558479791478509568, 5.587240632920778438, 0.000000000000000000 ) ) ;
#33691 = EDGE_CURVE ( 'NONE', #179865, #133314, #105193, .T. ) ;
#33692 = CARTESIAN_POINT ( 'NONE',  ( 6.063714619507535097, 1.842885348237649490, -0.3194776537047139264 ) ) ;
#33693 = CARTESIAN_POINT ( 'NONE',  ( 1.218750000000000888, -0.7852924748299231483, 1.895863743164115656 ) ) ;
#33694 = CARTESIAN_POINT ( 'NONE',  ( -1.119339255005453736E-13, 13.28612805825129151, 1.454322456996997470 ) ) ;
#33695 = CARTESIAN_POINT ( 'NONE',  ( 6.468125021464292246, 1.674632898861495134, 1.122323893169609565 ) ) ;
#33696 = CARTESIAN_POINT ( 'NONE',  ( -1.360316468750006669, 1.119791667008071423, -0.7853790794158921340 ) ) ;
#33697 = CARTESIAN_POINT ( 'NONE',  ( 4.588517629802620235, -0.5350896943857390564, 1.944070981013111155 ) ) ;
#33698 = CARTESIAN_POINT ( 'NONE',  ( -8.130085669689073313, 12.63685038127928806, 0.7998128361456481317 ) ) ;
#33699 = CARTESIAN_POINT ( 'NONE',  ( 9.271078113646423091, 9.710679308875986848, 1.040834085586084257E-14 ) ) ;
#33700 = CARTESIAN_POINT ( 'NONE',  ( 4.903208829997618423, 5.749440385532527564, -1.199719254218450271 ) ) ;
#33702 = DIRECTION ( 'NONE',  ( 0.000000000000000000, 1.000000000000000000, 0.000000000000000000 ) ) ;
#33701 = CARTESIAN_POINT ( 'NONE',  ( 2.648829494986388422, -1.517897411861212076, 1.014145048410304284 ) ) ;
#33703 = CARTESIAN_POINT ( 'NONE',  ( -11.48243876534946217, 11.29999999999998117, 3.199999999999997957 ) ) ;
#33704 = CARTESIAN_POINT ( 'NONE',  ( -10.56511880488638333, 9.841134764184808148, -3.405056808716381944 ) ) ;
#33705 = VERTEX_POINT ( 'NONE', #204772 ) ;
#33706 = CARTESIAN_POINT ( 'NONE',  ( -6.414416072596857532, 6.656109304217339151, -0.7216878364870338292 ) ) ;
#33707 = CARTESIAN_POINT ( 'NONE',  ( -1.608462485350629301, 8.735270501766756013, 2.463594439587650342 ) ) ;
#33708 = CARTESIAN_POINT ( 'NONE',  ( -8.646349277213090545, 11.11049346154719508, 1.599625672291269396 ) ) ;
#33709 = CARTESIAN_POINT ( 'NONE',  ( -0.2106725631050176961, -0.004273297132588448587, -2.003483006309704439 ) ) ;
#33710 = CARTESIAN_POINT ( 'NONE',  ( 0.5574859923395922845, -1.816599148028580579, 1.093606109393664427 ) ) ;
#33711 = VERTEX_POINT ( 'NONE', #56427 ) ;
#33712 = CARTESIAN_POINT ( 'NONE',  ( -7.598418745816086783, 7.829519723065708092, 0.000000000000000000 ) ) ;
#33713 = CARTESIAN_POINT ( 'NONE',  ( 3.994848817520957773, 7.812407387083109001, 1.040834085586084257E-14 ) ) ;
#33714 = CARTESIAN_POINT ( 'NONE',  ( 6.420785563114608685, 1.921975812937461781, 0.7442927364858693551 ) ) ;
#33715 = CARTESIAN_POINT ( 'NONE',  ( 5.309220276109914316, 1.198862193007979471, -1.621181151826488254 ) ) ;
#33716 = EDGE_LOOP ( 'NONE', ( #196977, #98721, #198718, #150334 ) ) ;
#33717 = ORIENTED_EDGE ( 'NONE', *, *, #155760, .T. ) ;
#33718 = CARTESIAN_POINT ( 'NONE',  ( -3.619250341049077946, 3.172667246362661064, 2.500000000000011102 ) ) ;
#33719 = DIRECTION ( 'NONE',  ( 0.7978120914393174168, 0.6029061840396252592, -6.536721945407052908E-15 ) ) ;
#33722 = ORIENTED_EDGE ( 'NONE', *, *, #93445, .F. ) ;
#33721 = DIRECTION ( 'NONE',  ( 1.000000000000000000, 0.000000000000000000, -1.224646799147353207E-16 ) ) ;
#33720 = CARTESIAN_POINT ( 'NONE',  ( -4.606738333593328072, 8.596554832492683929, 0.7998128361456281477 ) ) ;
#33723 = CARTESIAN_POINT ( 'NONE',  ( 4.595841027163160675, 8.489102040997540399, 0.04885061651019838302 ) ) ;
#33724 = CARTESIAN_POINT ( 'NONE',  ( 5.466172646012215530, 1.646588110366095314, 1.163089216160061001 ) ) ;
#33725 = CARTESIAN_POINT ( 'NONE',  ( 5.208873985248447802, -0.2666229848188906848, 1.821608446441948193 ) ) ;
#33726 = CARTESIAN_POINT ( 'NONE',  ( 0.07661050522435489119, 2.064768137775649048, -2.128874817076317871 ) ) ;
#33727 = CARTESIAN_POINT ( 'NONE',  ( 3.651255599878608926, -1.887205614810626209, 1.327874790813722949 ) ) ;
#33728 = CARTESIAN_POINT ( 'NONE',  ( 7.180978637093494044, 8.406838493811077839, -1.199719254218452047 ) ) ;
#33729 = CARTESIAN_POINT ( 'NONE',  ( 4.903692054014650026, -0.5817465652163296141, 2.081756923971528117 ) ) ;
#33731 = CARTESIAN_POINT ( 'NONE',  ( 7.527801604085637699, 9.805521176231838609, 1.599625672291281386 ) ) ;
#33730 = CARTESIAN_POINT ( 'NONE',  ( 3.362517798112668821, -1.944730434982215650, -0.5331690889110105580 ) ) ;
#33732 = CARTESIAN_POINT ( 'NONE',  ( 0.7845916355662507780, 1.712027273464492350, -0.9168598982515554496 ) ) ;
#33733 = CARTESIAN_POINT ( 'NONE',  ( -4.436542580169821726, 6.199052314996659874, 1.599625672291267398 ) ) ;
#33734 = CARTESIAN_POINT ( 'NONE',  ( 2.678032581596942130, 0.4534618882029567422, -0.1088563323523697446 ) ) ;
#33735 = CARTESIAN_POINT ( 'NONE',  ( -5.991777542596674166, 5.955104985976372944, 0.000000000000000000 ) ) ;
#33736 = CARTESIAN_POINT ( 'NONE',  ( 3.696050037196423332, -1.868490534004090931, -0.09263902202472777681 ) ) ;
#33740 = EDGE_CURVE ( 'NONE', #184334, #88263, #110330, .T. ) ;
#33739 = CARTESIAN_POINT ( 'NONE',  ( -6.774234028683526532, 7.932303117332766718, 1.199719254218452047 ) ) ;
#33738 = CARTESIAN_POINT ( 'NONE',  ( -1.500000000000015099, -0.5895833326505155458, -0.8660254037844383745 ) ) ;
#33737 = CARTESIAN_POINT ( 'NONE',  ( 0.8965662283535699162, -1.866366896104875162, -0.4163465257057268332 ) ) ;
#33741 = CARTESIAN_POINT ( 'NONE',  ( 3.282038605231399231, 1.400092287458438722, 1.705885466304429166 ) ) ;
#33742 = CARTESIAN_POINT ( 'NONE',  ( 0.000000000000000000, 8.920000000000001705, 0.000000000000000000 ) ) ;
#33743 = CARTESIAN_POINT ( 'NONE',  ( 5.352771719296971042, 5.139321848801576387, 0.7998128361456341429 ) ) ;
#33744 = CARTESIAN_POINT ( 'NONE',  ( 4.868786560638878491, 8.694351730805124134, 0.7216878364870317197 ) ) ;
#33745 = CARTESIAN_POINT ( 'NONE',  ( -2.950870989268691957, 6.594433254122103349, -0.7998128361456281477 ) ) ;
#33746 = CARTESIAN_POINT ( 'NONE',  ( -6.414416072596837104, 9.537216947121368804, -1.082531754730549967 ) ) ;
#33747 = CARTESIAN_POINT ( 'NONE',  ( 0.6320224300673723539, 1.017306711037075262, -1.688479424803266404 ) ) ;
#33748 = ADVANCED_FACE ( 'NONE', ( #52158 ), #184271, .F. ) ;
#33749 = CARTESIAN_POINT ( 'NONE',  ( 0.1656154469977044186, -2.063490973871735967, -1.033197247175041467 ) ) ;
#33750 = CARTESIAN_POINT ( 'NONE',  ( 1.627322669196319849, 0.1476378700930695564, -1.956383933670035713 ) ) ;
#33751 = CARTESIAN_POINT ( 'NONE',  ( 4.592669665391247769, 2.021776019120101520, 0.4074096221951555297 ) ) ;
#33752 = CARTESIAN_POINT ( 'NONE',  ( 6.005898861173831094, 6.109229547565340646, 1.040834085586084257E-14 ) ) ;
#33753 = CARTESIAN_POINT ( 'NONE',  ( 5.006703865196457492, 9.063181286029688977, 0.000000000000000000 ) ) ;
#33754 = EDGE_LOOP ( 'NONE', ( #9452, #132370, #58261, #112498 ) ) ;
#33755 = CARTESIAN_POINT ( 'NONE',  ( 7.076992996209058973, 11.20031622897851165, 1.040834085586084257E-14 ) ) ;
#33756 = CARTESIAN_POINT ( 'NONE',  ( -0.6823417656249969321, 4.780208333674755394, -1.181850606188749264 ) ) ;
#33757 = CARTESIAN_POINT ( 'NONE',  ( 11.78331023100045627, 12.30000000000000071, -1.800000000000001155 ) ) ;
#33758 = CARTESIAN_POINT ( 'NONE',  ( 3.673896439178918172, 6.269667698141953238, 1.082531754730558626 ) ) ;
#33759 = CARTESIAN_POINT ( 'NONE',  ( 1.200314488179974326, 0.8819602860624680130, -1.984045050410755406 ) ) ;
#33761 = CARTESIAN_POINT ( 'NONE',  ( 6.146043377905669125, 0.5841948715668408010, 1.746183665442810007 ) ) ;
#33760 = CARTESIAN_POINT ( 'NONE',  ( 10.96785329849812562, -5.223431457505089526, -0.4373225248172959434 ) ) ;
#33762 = CARTESIAN_POINT ( 'NONE',  ( -4.505605203626008581, 6.920276886661140381, 1.305342265584524375 ) ) ;
#33763 = CARTESIAN_POINT ( 'NONE',  ( 4.529832720297257254, 8.298905583739861314, 0.000000000000000000 ) ) ;
#33764 = CARTESIAN_POINT ( 'NONE',  ( 1.879943753831798015, -1.004885234286160722, 1.577526331995420472 ) ) ;
#33765 = CARTESIAN_POINT ( 'NONE',  ( 5.378265110509337532, -1.205767192478784500, 1.793856531414832256 ) ) ;
#33766 = CARTESIAN_POINT ( 'NONE',  ( -5.641245921709659328, 6.318796091258308323, 1.170641968482153850 ) ) ;
#33767 = CARTESIAN_POINT ( 'NONE',  ( -0.02264175331115856477, 0.2280268304470518537, -2.122276614016995744 ) ) ;
#33768 = CARTESIAN_POINT ( 'NONE',  ( 6.463557619869761517, 6.860074278669063830, -0.6545079704341187909 ) ) ;
#33769 = CARTESIAN_POINT ( 'NONE',  ( -0.6823417656250212460, 5.113541667008086655, 1.181850606188767472 ) ) ;
#33770 = CARTESIAN_POINT ( 'NONE',  ( 0.9965660710522584731, -1.865815080690262917, -0.4182784585613218420 ) ) ;
#33771 = CARTESIAN_POINT ( 'NONE',  ( 2.518099203671141595, 1.158133694123581359, -1.338384833553945663 ) ) ;
#33773 = CARTESIAN_POINT ( 'NONE',  ( 0.6274217273865910771, -0.2802014979648696502, 1.891502685196179812 ) ) ;
#33772 = AXIS2_PLACEMENT_3D ( 'NONE', #172718, #24296, #125112 ) ;
#33775 = CARTESIAN_POINT ( 'NONE',  ( 5.941025102908992217, -1.645668167864361431, -0.9802026474072849105 ) ) ;
#33774 = CARTESIAN_POINT ( 'NONE',  ( 3.327047314414037338, -3.194760604760761957, 0.08430543425245248801 ) ) ;
#33776 = CARTESIAN_POINT ( 'NONE',  ( 6.795365950078042339, -1.759944107108902367, 0.8842400836535941888 ) ) ;
#33777 = CARTESIAN_POINT ( 'NONE',  ( 0.8441712343106638761, -1.349783269286155774, -1.635521010841307410 ) ) ;
#33778 = CARTESIAN_POINT ( 'NONE',  ( 1.806654366501771136, 2.518449987798942136, 2.499999999999998668 ) ) ;
#33779 = CARTESIAN_POINT ( 'NONE',  ( 3.854256360616271415, 0.6726810918341770140, 1.745705178215435582 ) ) ;
#33781 = EDGE_LOOP ( 'NONE', ( #139352, #100708, #70596, #94875 ) ) ;
#33780 = CARTESIAN_POINT ( 'NONE',  ( 0.6623940301842005107, -1.324425631624454036, 1.256838194884236204 ) ) ;
#33783 = CARTESIAN_POINT ( 'NONE',  ( 10.20626665084801843, 3.700502905159948508, 5.921468070729023481 ) ) ;
#33782 = CARTESIAN_POINT ( 'NONE',  ( 3.475398437264758833, 0.05438942809191970457, -2.206374867412825402 ) ) ;
#33784 = CARTESIAN_POINT ( 'NONE',  ( -1.201851678989727383E-14, 4.259375000341417028, -1.575800808251660134 ) ) ;
#33785 = CARTESIAN_POINT ( 'NONE',  ( 1.486864572717770283, 1.987365476997263292, 0.5519934122387574194 ) ) ;
#33786 = CARTESIAN_POINT ( 'NONE',  ( 7.311924916471702396, 7.425000578838787391, -0.7998128361456281477 ) ) ;
#33787 = CARTESIAN_POINT ( 'NONE',  ( -8.910733272679575379, 11.41894145625809820, -1.599625672291263179 ) ) ;
#33788 = CARTESIAN_POINT ( 'NONE',  ( -2.224029779570270815, 15.44821792883578127, -11.75514780501742962 ) ) ;
#33789 = CARTESIAN_POINT ( 'NONE',  ( -3.430537540284197995, -0.01791083384793297137, -0.4075187568799509830 ) ) ;
#33790 = CARTESIAN_POINT ( 'NONE',  ( 6.433860211133586304, -1.853236450885078712, 0.4715264990977630077 ) ) ;
#33791 = STYLED_ITEM ( 'NONE', ( #146031 ), #200496 ) ;
#33792 = ORIENTED_EDGE ( 'NONE', *, *, #28655, .T. ) ;
#33793 = CARTESIAN_POINT ( 'NONE',  ( 4.404779037558821386, 0.5491149005726041477, 1.996164414091922135 ) ) ;
#33794 = CARTESIAN_POINT ( 'NONE',  ( 1.499999999999989120, 5.795833333333350268, -0.8660254037844323793 ) ) ;
#33795 = CARTESIAN_POINT ( 'NONE',  ( 1.370646902836635261, -1.372427557409527488, 1.669970663979184256 ) ) ;
#33796 = CARTESIAN_POINT ( 'NONE',  ( -5.811016664379555330, 7.234075022110222797, -1.179019473189359068 ) ) ;
#33797 = CARTESIAN_POINT ( 'NONE',  ( 1.594405160661801490, -1.078473704070359140, 1.707419690039575499 ) ) ;
#33798 = DIRECTION ( 'NONE',  ( 0.000000000000000000, 0.000000000000000000, 1.000000000000000000 ) ) ;
#33799 = ORIENTED_EDGE ( 'NONE', *, *, #442, .F. ) ;
#33801 = CARTESIAN_POINT ( 'NONE',  ( 7.944714827928039291, 11.25228915168265864, 1.082531754730557072 ) ) ;
#33800 = CARTESIAN_POINT ( 'NONE',  ( 1.737500000000001155, -2.683333333333332682, 3.009438278150922130 ) ) ;
#33802 = CARTESIAN_POINT ( 'NONE',  ( 6.714220164357198151, -1.617572894677368422, -1.203167480739217421 ) ) ;
#33803 = CARTESIAN_POINT ( 'NONE',  ( 6.503150280507321135, -0.1381757461387123076, 1.884094533524976578 ) ) ;
#33804 = CARTESIAN_POINT ( 'NONE',  ( 7.334597915313080918, 9.580116872663850813, 1.040834085586084257E-14 ) ) ;
#33805 = CARTESIAN_POINT ( 'NONE',  ( 4.810206850810132551, 1.511280187219691928, -1.587364365194674276 ) ) ;
#33806 = CARTESIAN_POINT ( 'NONE',  ( -1.201851678989727383E-14, 3.743750000682817269, 1.732050807568877637 ) ) ;
#33807 = CARTESIAN_POINT ( 'NONE',  ( 3.340010735810138520, -1.142844047782382466, -1.533173144288489276 ) ) ;
#33808 = CARTESIAN_POINT ( 'NONE',  ( -4.822949958159302497, 6.649860922651058992, -1.599625672291256295 ) ) ;
#33809 = CARTESIAN_POINT ( 'NONE',  ( 3.999292125906905859, 5.688926785023260102, 1.443375672974062551 ) ) ;
#33811 = CARTESIAN_POINT ( 'NONE',  ( 1.651970485933237143, 1.039013645561959853, 1.727991324714774013 ) ) ;
#33810 = DIRECTION ( 'NONE',  ( 0.000000000000000000, 0.000000000000000000, -1.000000000000000000 ) ) ;
#33812 = CARTESIAN_POINT ( 'NONE',  ( 1.364683531249997417, 12.79687500034139980, 2.602085213965210642E-15 ) ) ;
#33813 = B_SPLINE_CURVE_WITH_KNOTS ( 'NONE', 3,
 ( #11858, #73670, #77936, #172253, #127860, #23840, #25977, #92083, #158140, #207926 ),
 .UNSPECIFIED., .F., .F.,
 ( 4, 3, 3, 4 ),
 ( 4.665953388357896293E-15, 8.735091161667903135E-05, 0.0001705277764939987001, 0.0002537626642914739207 ),
 .UNSPECIFIED. ) ;
#33815 = CARTESIAN_POINT ( 'NONE',  ( -4.793689830883590020, 7.750332681742931662, 1.199719254218452935 ) ) ;
#33814 = CARTESIAN_POINT ( 'NONE',  ( 0.6094042559229868594, -0.3290114652876909296, 2.268531362689259812 ) ) ;
#33816 = CARTESIAN_POINT ( 'NONE',  ( 4.242953580973901850, -1.500179917044243139, 0.8508681493539415053 ) ) ;
#33817 = CARTESIAN_POINT ( 'NONE',  ( 7.095713291905693332, 9.371694488680407886, 1.599625672291268286 ) ) ;
#33818 = CARTESIAN_POINT ( 'NONE',  ( 2.849184837166184536, 6.475799410002530898, 0.7998128361456362523 ) ) ;
#33819 = CARTESIAN_POINT ( 'NONE',  ( 4.327421600515347855, 8.660439283198849481, -0.7750000000000001332 ) ) ;
#33820 = CARTESIAN_POINT ( 'NONE',  ( 1.205434515183744226, -1.544416933936803904, -1.209700862059132964 ) ) ;
#33821 = CARTESIAN_POINT ( 'NONE',  ( -9.367496997601305608, 14.48154074412967596, 7.499999999995371702 ) ) ;
#33822 = CARTESIAN_POINT ( 'NONE',  ( 0.07536363704233395300, 5.720741966631408104, -2.738263776839637398 ) ) ;
#33823 = VERTEX_POINT ( 'NONE', #193874 ) ;
#33824 = VECTOR ( 'NONE', #11366, 1000.000000000000000 ) ;
#33825 = DIRECTION ( 'NONE',  ( -0.6507913734559640506, -0.7592566023653004592, 0.000000000000000000 ) ) ;
#33826 = ORIENTED_EDGE ( 'NONE', *, *, #67738, .T. ) ;
#33827 = CARTESIAN_POINT ( 'NONE',  ( 4.811091142047322577, 1.503129720864199381, -1.010622461758519552 ) ) ;
#33828 = ORIENTED_EDGE ( 'NONE', *, *, #212430, .T. ) ;
#33829 = CARTESIAN_POINT ( 'NONE',  ( 5.885121196783658526, 9.023669275293071834, 1.199719254218452047 ) ) ;
#33830 = CARTESIAN_POINT ( 'NONE',  ( 6.234996492879100849, 1.692908850720629799, 0.6451080659017217611 ) ) ;
#33831 = CARTESIAN_POINT ( 'NONE',  ( 6.007671464186823407, 9.062681570643055906, 1.082531754730549967 ) ) ;
#33832 = CARTESIAN_POINT ( 'NONE',  ( 0.000000000000000000, 0.000000000000000000, 0.000000000000000000 ) ) ;
#33833 = CARTESIAN_POINT ( 'NONE',  ( 5.206864636422387171, 6.427350532134703087, -1.171562478298654231 ) ) ;
#33834 = VECTOR ( 'NONE', #121567, 1000.000000000000000 ) ;
#33836 = CARTESIAN_POINT ( 'NONE',  ( 10.70146331988817323, 11.37946204949139251, 0.7998128361456341429 ) ) ;
#33835 = CARTESIAN_POINT ( 'NONE',  ( 5.828513650932020340, -1.180329482691832244, 1.438830759754748723 ) ) ;
#33837 = CARTESIAN_POINT ( 'NONE',  ( 3.462411278976515128, -1.846996576941996482, -0.5078680121572733963 ) ) ;
#33838 = CARTESIAN_POINT ( 'NONE',  ( 1.500000000000039524, 7.128742170989512239, 10.89107411574799400 ) ) ;
#33839 = CARTESIAN_POINT ( 'NONE',  ( -1.364683531250014514, -1.011458332991911568, -0.7879004041258359514 ) ) ;
#33840 = CARTESIAN_POINT ( 'NONE',  ( 6.155038550924150087, 7.243595066575396757, 1.082531754730558626 ) ) ;
#33842 = CARTESIAN_POINT ( 'NONE',  ( 6.034383107294147841, 0.6662506799693500570, 2.009816206752083723 ) ) ;
#33841 = CARTESIAN_POINT ( 'NONE',  ( -2.117044542028253318, 5.621635732341564662, -0.7998128361456281477 ) ) ;
#33843 = CARTESIAN_POINT ( 'NONE',  ( 1.165152350680317195, -1.954565670758709128, -0.9236901323337529668 ) ) ;
#33844 = CARTESIAN_POINT ( 'NONE',  ( -5.971440312176176768, 5.931378217152456500, 0.000000000000000000 ) ) ;
#33845 = CARTESIAN_POINT ( 'NONE',  ( 5.065906673361608270, 5.939254536123854677, -1.199719254218450271 ) ) ;
#33846 = CARTESIAN_POINT ( 'NONE',  ( 0.5338675855391886715, 0.9430634504648884864, -1.562995807167219642 ) ) ;
#33847 = CARTESIAN_POINT ( 'NONE',  ( -3.228813138348844536, 6.918699094715619502, 0.7998128361456341429 ) ) ;
#33848 = CARTESIAN_POINT ( 'NONE',  ( 3.662960631648714216, -1.609669772967847079, -0.8612380056681954166 ) ) ;
#33849 = CARTESIAN_POINT ( 'NONE',  ( 10.16268612673838234, 10.86226847457346167, 8.132478767492923311 ) ) ;
#33850 = CARTESIAN_POINT ( 'NONE',  ( 2.689602200614676697, 1.814610489020528350, -0.6038049036062518304 ) ) ;
#33851 = VERTEX_POINT ( 'NONE', #93214 ) ;
#33852 = CARTESIAN_POINT ( 'NONE',  ( 2.383201438719654064, -0.002954665228930426248, 1.969739564733210324 ) ) ;
#33853 = CARTESIAN_POINT ( 'NONE',  ( 4.370608360784649093, -0.003437861098648780072, -1.942234966449083000 ) ) ;
#33854 = CARTESIAN_POINT ( 'NONE',  ( -7.425025402139490360, 8.691559719698066289, 1.199719254218452047 ) ) ;
#33856 = CARTESIAN_POINT ( 'NONE',  ( 5.097945154717048233, 1.425953928781589886, 1.569717048080176314 ) ) ;
#33855 = CARTESIAN_POINT ( 'NONE',  ( 7.693325821111733021, 7.940244644243982464, -0.7998128361456341429 ) ) ;
#33857 = CARTESIAN_POINT ( 'NONE',  ( 0.005973655272069301574, -7.189371949516782934, 9.500370076773188899 ) ) ;
#33858 = CARTESIAN_POINT ( 'NONE',  ( 2.455592584850064153, -1.418247937500687561, -1.282927761235647335 ) ) ;
#33859 = CARTESIAN_POINT ( 'NONE',  ( 5.904500254309781759, 6.149185751451256898, 0.8064407133735688182 ) ) ;
#33860 = CARTESIAN_POINT ( 'NONE',  ( -1.420000000000001039, 6.200000000000045475, -2.899999999999995470 ) ) ;
#33861 = ORIENTED_EDGE ( 'NONE', *, *, #25909, .T. ) ;
#33862 = CARTESIAN_POINT ( 'NONE',  ( -7.119749541375154145, 14.48019291653405105, 9.669933605396591858 ) ) ;
#33863 = CARTESIAN_POINT ( 'NONE',  ( 3.932747076415766596, 6.745899468197171345, 1.199719254218451159 ) ) ;
#33864 = CARTESIAN_POINT ( 'NONE',  ( 3.822509244049070887, 6.547012320444182798, -1.199719254218452047 ) ) ;
#33865 = CARTESIAN_POINT ( 'NONE',  ( 0.09053139919706915117, -9.918143888366140359, 9.499568811299539561 ) ) ;
#33867 = CARTESIAN_POINT ( 'NONE',  ( 6.192592252150040721, 1.490973663936447258, -1.357864438797616868 ) ) ;
#33866 = CARTESIAN_POINT ( 'NONE',  ( 4.758326833623739205, 0.7015320795021735556, 1.685726030614169924 ) ) ;
#33868 = DIRECTION ( 'NONE',  ( 0.000000000000000000, -1.000000000000000000, 0.000000000000000000 ) ) ;
#33869 = CARTESIAN_POINT ( 'NONE',  ( -9.164948653157999559, 10.75515685251491504, -1.082531754730539753 ) ) ;
#33870 = CARTESIAN_POINT ( 'NONE',  ( -6.480235040494578769, 6.771487114559836762, -0.2501488059577141598 ) ) ;
#33871 = FACE_OUTER_BOUND ( 'NONE', #143798, .T. ) ;
#33872 = CARTESIAN_POINT ( 'NONE',  ( 5.119927267529915227, -1.001353885182048931, -1.579878405157906673 ) ) ;
#33873 = CARTESIAN_POINT ( 'NONE',  ( 8.423693512792301163, 8.722063941212843119, 0.7998128361456481317 ) ) ;
#33874 = CARTESIAN_POINT ( 'NONE',  ( -5.436983294280064882, 6.301900917203534291, 1.199719254218450271 ) ) ;
#33875 = AXIS2_PLACEMENT_3D ( 'NONE', #39104, #207982, #139825 ) ;
#33876 = CARTESIAN_POINT ( 'NONE',  ( 1.364683531250000303, 10.56770833367473195, -0.7879004041258355073 ) ) ;
#33877 = CARTESIAN_POINT ( 'NONE',  ( -4.225337428953291230, 8.081310767087481750, 0.7998128361456341429 ) ) ;
#33878 =( NAMED_UNIT ( * ) PLANE_ANGLE_UNIT ( ) SI_UNIT ( $, .RADIAN. ) );
#33879 = EDGE_CURVE ( 'NONE', #83886, #163739, #41012, .T. ) ;
#33880 = CARTESIAN_POINT ( 'NONE',  ( -7.957709816578236506, 8.248692638954882028, 0.7998128361456341429 ) ) ;
#33881 = CARTESIAN_POINT ( 'NONE',  ( -4.717347382551060342, 7.590990148696470818, 1.199719254218464037 ) ) ;
#33882 = CARTESIAN_POINT ( 'NONE',  ( 6.807499178464245126, -1.738453852359397978, -1.300317965242798968 ) ) ;
#33883 = CARTESIAN_POINT ( 'NONE',  ( 2.144302737913783119, 0.9084621246772636161, 1.912570996397492618 ) ) ;
#33884 = CARTESIAN_POINT ( 'NONE',  ( 7.865701674222579598, 12.32840238656838139, -0.7998128361456352531 ) ) ;
#33885 = CARTESIAN_POINT ( 'NONE',  ( 0.5337978311145309407, 6.541559214916611076, 3.355412286555431667 ) ) ;
#33886 = CARTESIAN_POINT ( 'NONE',  ( 5.805552407531882508, -1.628464769346991581, -1.278160613847306504 ) ) ;
#33887 = CARTESIAN_POINT ( 'NONE',  ( 3.999262108721039155, 7.828827674157968985, 0.07552679838754294828 ) ) ;
#33888 = CARTESIAN_POINT ( 'NONE',  ( 6.670248388243460447, 6.884303995813253252, -0.7216878364870257245 ) ) ;
#33890 = SURFACE_SIDE_STYLE ('',( #136744 ) ) ;
#33889 = CARTESIAN_POINT ( 'NONE',  ( -3.475000000000000533, -3.879166666666665986, -2.006292185433948827 ) ) ;
#33891 = CARTESIAN_POINT ( 'NONE',  ( 2.080407636089614432, -2.248563537884174846, -0.4446712507181517782 ) ) ;
#33893 = DIRECTION ( 'NONE',  ( -1.000000000000000000, 0.000000000000000000, 1.478457507935137263E-17 ) ) ;
#33892 = DIRECTION ( 'NONE',  ( -0.000000000000000000, -8.546850786086437571E-32, -1.000000000000000000 ) ) ;
#33894 = CARTESIAN_POINT ( 'NONE',  ( 2.074333847954575205, 0.8209984392052707136, 1.727357542596375861 ) ) ;
#33895 = ORIENTED_EDGE ( 'NONE', *, *, #131734, .T. ) ;
#33896 = CARTESIAN_POINT ( 'NONE',  ( 7.009202228140744673, 9.200488570962775725, -1.443375672974058777 ) ) ;
#33897 = CARTESIAN_POINT ( 'NONE',  ( 1.107682593029035711, 1.527310012579755183, 1.311747809748030846 ) ) ;
#33898 = CARTESIAN_POINT ( 'NONE',  ( 0.6726124357511429341, 1.356994209013298036, -1.416925378234991095 ) ) ;
#33899 = CARTESIAN_POINT ( 'NONE',  ( 5.974412749747233242, 4.760129193867229880, -2.438793960827100094 ) ) ;
#33900 = CARTESIAN_POINT ( 'NONE',  ( -9.027031348600448979, 9.425958082989001952, 1.040834085586084257E-14 ) ) ;
#33901 = CARTESIAN_POINT ( 'NONE',  ( -9.410012541129075814, 4.000000000000001776, 6.919867902370715917 ) ) ;
#33903 = CARTESIAN_POINT ( 'NONE',  ( 1.990718100289643244, 1.541686266772484437, -0.8690610084590517648 ) ) ;
#33902 = CARTESIAN_POINT ( 'NONE',  ( 3.609396000958647210, -2.059664220577660743, 0.3575658041875314219 ) ) ;
#33904 = CARTESIAN_POINT ( 'NONE',  ( -2.549999999999999378, -7.105553651663779391, 1.849324200890692271 ) ) ;
#33906 = CARTESIAN_POINT ( 'NONE',  ( 5.666080500323320557, -1.458056995643598475, 1.768786637700834108 ) ) ;
#33905 = CARTESIAN_POINT ( 'NONE',  ( 0.000000000000000000, 12.22000000000000064, 0.000000000000000000 ) ) ;
#33907 = CARTESIAN_POINT ( 'NONE',  ( 3.450842174108187610, 0.4214097805228322891, -1.688396943527884053 ) ) ;
#33908 = EDGE_CURVE ( 'NONE', #67360, #94475, #40040, .T. ) ;
#33909 = CARTESIAN_POINT ( 'NONE',  ( 2.367870383881045981, 5.914265881169853856, 0.000000000000000000 ) ) ;
#33910 = EDGE_CURVE ( 'NONE', #169582, #16492, #162069, .T. ) ;
#33911 = CARTESIAN_POINT ( 'NONE',  ( 4.064412189046650248, 7.963840997188265547, 0.7998128361456271485 ) ) ;
#33912 = CARTESIAN_POINT ( 'NONE',  ( 3.848775019297555389, -0.8554209813324518130, 1.508043379464953260 ) ) ;
#33913 = CARTESIAN_POINT ( 'NONE',  ( 3.525983582677540085, 2.118976886349494659, -0.4726038967238275212 ) ) ;
#33914 = CARTESIAN_POINT ( 'NONE',  ( 5.508690485854129903, 5.321227076451600091, 1.040834085586084257E-14 ) ) ;
#33915 = CARTESIAN_POINT ( 'NONE',  ( 5.665250009225348826, 1.861346387706263261, -0.7762253298396750711 ) ) ;
#33916 = CARTESIAN_POINT ( 'NONE',  ( 0.8437500000000005551, 1.895863743164106774, 0.7852924748299443536 ) ) ;
#33917 = CIRCLE ( 'NONE', #213707, 9.636568542494918788 ) ;
#33918 = CARTESIAN_POINT ( 'NONE',  ( 1.499999999999987121, 4.077083334016147198, -0.8660254037844323793 ) ) ;
#33919 = CARTESIAN_POINT ( 'NONE',  ( 2.502848596126582059, 1.548454276800725449, -1.145803370841493418 ) ) ;
#33920 = CARTESIAN_POINT ( 'NONE',  ( 0.7500000000000006661, 8.364583334016128191, 1.299038105676657340 ) ) ;
#33921 = CARTESIAN_POINT ( 'NONE',  ( 5.730790430626864662, 1.492114905813126446, -1.645873056973495618 ) ) ;
#33922 = ORIENTED_EDGE ( 'NONE', *, *, #125247, .T. ) ;
#33923 = CARTESIAN_POINT ( 'NONE',  ( 6.983263157960361234, 3.701227967198342128, 2.360532479264612071 ) ) ;
#33924 = B_SPLINE_CURVE_WITH_KNOTS ( 'NONE', 3,
 ( #108060, #174085, #141601, #109129 ),
 .UNSPECIFIED., .F., .F.,
 ( 4, 4 ),
 ( 0.001582017824277145253, 0.002341702326271046831 ),
 .UNSPECIFIED. ) ;
#33925 = CARTESIAN_POINT ( 'NONE',  ( 1.499999999999989120, 2.025000000000019895, 1.214306433183764966E-14 ) ) ;
#33926 = CARTESIAN_POINT ( 'NONE',  ( 6.317209508963599340, 9.457495962844502557, 1.199719254218462483 ) ) ;
#33927 = CARTESIAN_POINT ( 'NONE',  ( 3.646780131951580461, 7.198401220678078971, -0.7216878364870267237 ) ) ;
#33928 = CARTESIAN_POINT ( 'NONE',  ( 1.998975601324129769, -2.179183720934555701, -0.4297205562568666148 ) ) ;
#33929 = CARTESIAN_POINT ( 'NONE',  ( 6.742638286788313451, -1.923764577213080029, -0.3838556375530403630 ) ) ;
#33930 = CARTESIAN_POINT ( 'NONE',  ( 8.785320351975350661, 9.351887953500479966, -0.7216878364870197293 ) ) ;
#33931 = DIRECTION ( 'NONE',  ( 0.000000000000000000, 1.000000000000000000, 0.000000000000000000 ) ) ;
#33932 = CARTESIAN_POINT ( 'NONE',  ( 5.903649544107831382, 5.852288987739402870, -0.7998128361456481317 ) ) ;
#33934 = AXIS2_PLACEMENT_3D ( 'NONE', #124618, #174369, #92055 ) ;
#33933 =( GEOMETRIC_REPRESENTATION_CONTEXT ( 3 ) GLOBAL_UNCERTAINTY_ASSIGNED_CONTEXT ( ( #184986 ) ) GLOBAL_UNIT_ASSIGNED_CONTEXT ( ( #182006, #53086, #82385 ) ) REPRESENTATION_CONTEXT ( 'NONE', 'WORKASPACE' ) );
#33935 = CARTESIAN_POINT ( 'NONE',  ( -4.340018570150322219, 5.196348098997705556, -1.082531754730551743 ) ) ;
#33936 = CARTESIAN_POINT ( 'NONE',  ( 4.070800801938780467, 1.460776800910084994, -1.456535598646004237 ) ) ;
#33937 = CARTESIAN_POINT ( 'NONE',  ( -4.985647801523292344, 6.839675073242382553, -1.599625672291256295 ) ) ;
#33938 = CARTESIAN_POINT ( 'NONE',  ( 1.499999999999987121, 3.327083334016150751, -0.8660254037844262731 ) ) ;
#33939 = CARTESIAN_POINT ( 'NONE',  ( -1.364683531250014514, -0.4697916663252449943, 0.7879004041258379498 ) ) ;
#33940 = CARTESIAN_POINT ( 'NONE',  ( 6.063714619507535097, 1.842885348237649490, -0.3194776537047139264 ) ) ;
#33941 = CARTESIAN_POINT ( 'NONE',  ( 4.746542152430166972, 1.714266118827989516, -0.2609391866443058206 ) ) ;
#33942 = CARTESIAN_POINT ( 'NONE',  ( 4.985792865680892305, -1.728136641771714777, -0.2059490554011476626 ) ) ;
#33943 = CARTESIAN_POINT ( 'NONE',  ( 3.714044015139744914, 6.420469553383295391, 1.199719254218462483 ) ) ;
#33944 = CARTESIAN_POINT ( 'NONE',  ( 1.927642574099263983, -1.500803908722462499, -1.732858182149794812 ) ) ;
#33945 = CARTESIAN_POINT ( 'NONE',  ( 0.6823417656249899377, 5.738541667008087543, -1.181850606188754593 ) ) ;
#33946 = CARTESIAN_POINT ( 'NONE',  ( 5.565992953457829628, -1.325659382304938960, 1.616758296502271097 ) ) ;
#33947 = CARTESIAN_POINT ( 'NONE',  ( 0.8668490835730925381, 1.774987751554598869, -0.4888055736953432207 ) ) ;
#33948 = EDGE_CURVE ( 'NONE', #160372, #70814, #89409, .T. ) ;
#33949 = CARTESIAN_POINT ( 'NONE',  ( 3.469446951953614189E-15, 6.400000000000023448, 1.214306433183764966E-14 ) ) ;
#33950 = CARTESIAN_POINT ( 'NONE',  ( 1.125625214514534900, 0.3961039030971893471, 1.976955501819408711 ) ) ;
#33951 = CARTESIAN_POINT ( 'NONE',  ( 4.858757509019037357, 5.629766575900002401, 2.499999999999999556 ) ) ;
#33952 = CARTESIAN_POINT ( 'NONE',  ( 9.215575659530927055, 13.21669868873661358, -9.027657081567449282 ) ) ;
#33953 = CARTESIAN_POINT ( 'NONE',  ( -7.725448601688521322, 7.907444878258402809, 1.040834085586084257E-14 ) ) ;
#33954 = CARTESIAN_POINT ( 'NONE',  ( 4.819033534653518025, 7.709623992816043270, -1.199719254218452047 ) ) ;
#33955 = CARTESIAN_POINT ( 'NONE',  ( -3.755786496842897795E-14, 1.703125000341434214, 1.570758158831776052 ) ) ;
#33956 = CARTESIAN_POINT ( 'NONE',  ( 3.703867829435038672, 1.536975034498413661, 1.461131120854219700 ) ) ;
#33957 = CARTESIAN_POINT ( 'NONE',  ( 1.364683531249988757, -0.3656249996585800299, 0.000000000000000000 ) ) ;
#33958 = CARTESIAN_POINT ( 'NONE',  ( 5.338443970399977978, 1.799313579390570128, 0.3082849261525285600 ) ) ;
#33959 = ORIENTED_EDGE ( 'NONE', *, *, #156113, .F. ) ;
#33960 = CARTESIAN_POINT ( 'NONE',  ( -7.228432174741334038, 8.462200954400218578, -1.199719254218452047 ) ) ;
#33961 = DIRECTION ( 'NONE',  ( 0.000000000000000000, -1.000000000000000000, 0.000000000000000000 ) ) ;
#33962 = CARTESIAN_POINT ( 'NONE',  ( 3.475000000000000533, -2.960416665710750905, 2.006292185433948827 ) ) ;
#33963 = CARTESIAN_POINT ( 'NONE',  ( -6.878064000834399394, 6.918829510595249310, -0.7998128361456291469 ) ) ;
#33964 = CARTESIAN_POINT ( 'NONE',  ( 2.970967976831692781, -1.526577591334898454, 1.322595846222093030 ) ) ;
#33965 = CARTESIAN_POINT ( 'NONE',  ( 0.4640741377587159211, 2.083006155408675397, -0.3091503547662070583 ) ) ;
#33966 = CARTESIAN_POINT ( 'NONE',  ( 9.890836756369282057, 11.49806328964105617, -1.199719254218440723 ) ) ;
#33967 = CARTESIAN_POINT ( 'NONE',  ( 3.783913598179854176, -1.105313619694109795, -1.496993097346049462 ) ) ;
#33968 = CARTESIAN_POINT ( 'NONE',  ( 9.077347539549325717, 10.54899253668443393, -1.199719254218446718 ) ) ;
#33969 = EDGE_CURVE ( 'NONE', #213712, #139878, #127519, .T. ) ;
#33970 = CARTESIAN_POINT ( 'NONE',  ( -5.570361349191150779, 5.866663122702686195, 0.5491554309224304653 ) ) ;
#33972 = CARTESIAN_POINT ( 'NONE',  ( -3.090368948911150770, 5.692848642783215674, 1.199719254218462483 ) ) ;
#33971 = COLOUR_RGB ( '', 0.31764706, 0.68627451, 0.89019608) ;
#33973 = CARTESIAN_POINT ( 'NONE',  ( -6.320072162264675164, 10.52516795595079557, 0.7998128361456481317 ) ) ;
#33974 = CARTESIAN_POINT ( 'NONE',  ( 6.772340629568521564, -1.270048932776141726, 1.623522132280514896 ) ) ;
#33976 = CARTESIAN_POINT ( 'NONE',  ( -4.144643181316929770, 7.629267798522465505, 0.8581763667485035052 ) ) ;
#33975 = CARTESIAN_POINT ( 'NONE',  ( -7.747558435566414659, 8.003516027774422170, -0.7998128361456362523 ) ) ;
#33977 = CARTESIAN_POINT ( 'NONE',  ( -0.6823417656250212460, 1.051041667008083325, 1.181850606188755259 ) ) ;
#33978 = CARTESIAN_POINT ( 'NONE',  ( 2.248989396041571887, -1.699371294898213369, -0.3429280648484279714 ) ) ;
#33979 = CARTESIAN_POINT ( 'NONE',  ( 1.710509606392306647, -0.2150479285965025134, 1.726905287013901225 ) ) ;
#33981 = CARTESIAN_POINT ( 'NONE',  ( 8.487040972474689582, 9.964264558384387627, -1.082531754730543083 ) ) ;
#33980 = CARTESIAN_POINT ( 'NONE',  ( 0.4293363604773897113, 2.209526777583595170, 0.6654907822973181730 ) ) ;
#33982 = CARTESIAN_POINT ( 'NONE',  ( 1.036483977676525114, 2.029821650745375905, 0.3549538351500410305 ) ) ;
#33983 = CARTESIAN_POINT ( 'NONE',  ( 5.168682875307768931, 7.053215992657626110, -1.599625672291256295 ) ) ;
#33984 =( GEOMETRIC_REPRESENTATION_CONTEXT ( 3 ) GLOBAL_UNCERTAINTY_ASSIGNED_CONTEXT ( ( #926 ) ) GLOBAL_UNIT_ASSIGNED_CONTEXT ( ( #6639, #40240, #152914 ) ) REPRESENTATION_CONTEXT ( 'NONE', 'WORKASPACE' ) );
#33985 = CARTESIAN_POINT ( 'NONE',  ( 0.2454708137151571101, -1.954895187565863779, -0.4925657318226167591 ) ) ;
#33986 = CARTESIAN_POINT ( 'NONE',  ( 3.475000000000000533, -1.545833333333334503, -2.006292185433951047 ) ) ;
#33987 = CARTESIAN_POINT ( 'NONE',  ( -4.586401103172829785, 8.572828063668767484, 0.7998128361456281477 ) ) ;
#33988 = CARTESIAN_POINT ( 'NONE',  ( 6.350466393003619814, 0.5888352225367661230, 1.775644890098279749 ) ) ;
#33991 = EDGE_CURVE ( 'NONE', #47282, #75373, #166636, .T. ) ;
#33990 = CARTESIAN_POINT ( 'NONE',  ( -6.780486220610186798, 8.043560357867583832, -1.082531754730549967 ) ) ;
#33989 = CARTESIAN_POINT ( 'NONE',  ( 4.588094604188536429, 1.105678411722615051, 1.560157546714964871 ) ) ;
#33992 = CARTESIAN_POINT ( 'NONE',  ( 6.551417122825020201, -1.769646310455678995, -1.318412661681533260 ) ) ;
#33993 = CARTESIAN_POINT ( 'NONE',  ( -6.956180625286119579, -6.372104534813793464, -6.956180625285381502 ) ) ;
#33994 = CARTESIAN_POINT ( 'NONE',  ( 6.016786309414542622, 10.24161080428416426, 0.7998128361456341429 ) ) ;
#33995 = CARTESIAN_POINT ( 'NONE',  ( -3.309598895067336510, 6.875299454304925284, 0.000000000000000000 ) ) ;
#33996 = CARTESIAN_POINT ( 'NONE',  ( 0.06511101446048017660, -1.620675302784078786, 1.204964419619258376 ) ) ;
#33997 = ADVANCED_FACE ( 'NONE', ( #127922 ), #210114, .F. ) ;
#33998 = CARTESIAN_POINT ( 'NONE',  ( 2.977863636430440941, 2.191611430486348766, -0.7225824955255434334 ) ) ;
#33999 = CARTESIAN_POINT ( 'NONE',  ( 4.668382477721988444, -0.8370036265390871089, -1.774476930476886594 ) ) ;
#34000 = CARTESIAN_POINT ( 'NONE',  ( 1.340592890135338555, -1.912720961655197893, -0.4351338972534216087 ) ) ;
#34001 = CARTESIAN_POINT ( 'NONE',  ( 10.09812548408005384, 10.67556790771522124, -0.7998128361456281477 ) ) ;
#34002 = CARTESIAN_POINT ( 'NONE',  ( -9.372156330296117943, 15.41898192430145365, 7.405769077363409281 ) ) ;
#34003 = ORIENTED_EDGE ( 'NONE', *, *, #106606, .T. ) ;
#34004 = CARTESIAN_POINT ( 'NONE',  ( 0.3920140705387532010, -2.106502388992930630, 0.2143382252216985973 ) ) ;
#34006 = CARTESIAN_POINT ( 'NONE',  ( -9.169391961543940539, 9.592045464756413509, 1.040834085586084257E-14 ) ) ;
#34005 = CARTESIAN_POINT ( 'NONE',  ( -3.425406365747000859, 7.148057860013469877, 1.040834085586084257E-14 ) ) ;
#34007 = CARTESIAN_POINT ( 'NONE',  ( 1.359045109759978498, 1.814150759811587355, -0.3131490413979670651 ) ) ;
#34008 = CARTESIAN_POINT ( 'NONE',  ( 4.487298306821032590, 0.1004956810540975631, 2.168842786202809680 ) ) ;
#34009 = CARTESIAN_POINT ( 'NONE',  ( -0.3380487832185405384, 2.650106715013329950, 1.972192952016705636 ) ) ;
#34010 = CARTESIAN_POINT ( 'NONE',  ( 1.793382672576701919, -0.1090974814243403090, -2.117938670719583527 ) ) ;
#34011 = CARTESIAN_POINT ( 'NONE',  ( 1.499999999999989120, 2.785416667349484676, 0.8660254037844524744 ) ) ;
#34012 = CARTESIAN_POINT ( 'NONE',  ( 8.866142388332804103, 12.43125098877526113, -1.199719254218446718 ) ) ;
#34013 = CARTESIAN_POINT ( 'NONE',  ( 11.92619526913699524, 13.52780024161489969, -1.328859060402685976 ) ) ;
#34014 = CARTESIAN_POINT ( 'NONE',  ( 6.304162555737000240, 6.968127521147626346, -0.9177210060461529206 ) ) ;
#34015 = VECTOR ( 'NONE', #7111, 1000.000000000000000 ) ;
#34016 = CARTESIAN_POINT ( 'NONE',  ( 2.091158219120598183, 1.794587730539594972, -1.012862355382545765 ) ) ;
#34018 = CARTESIAN_POINT ( 'NONE',  ( 2.449293598294706414E-16, -4.500000000000003553, -2.000000000000000000 ) ) ;
#34017 = CARTESIAN_POINT ( 'NONE',  ( -7.479294296233107708, 11.87759377891399204, 0.7998128361456481317 ) ) ;
#34019 = CARTESIAN_POINT ( 'NONE',  ( 0.6823417656249882723, 1.926041667008083991, -1.181850606188749264 ) ) ;
#34020 = CARTESIAN_POINT ( 'NONE',  ( -0.7500000000000006661, 9.208333333333332149, -1.299038105676657340 ) ) ;
#34021 =( BOUNDED_SURFACE ( )  B_SPLINE_SURFACE ( 3, 2, ( 
 ( #139609, #137469, #203483 ),
 ( #103892, #169940, #205631 ),
 ( #8505, #171010, #22607 ),
 ( #155840, #55136, #7425 ),
 ( #121281, #88715, #24750 ),
 ( #90852, #72427, #138529 ) ),
 .UNSPECIFIED., .F., .F., .T. ) 
 B_SPLINE_SURFACE_WITH_KNOTS ( ( 4, 2, 4 ),
 ( 3, 3 ),
 ( 0.000000000000000000, 0.0003766405729503175871, 0.0007532811459006351741 ),
 ( 0.000000000000000000, 1.000000000000000000 ),
 .UNSPECIFIED. ) 
 GEOMETRIC_REPRESENTATION_ITEM ( )  RATIONAL_B_SPLINE_SURFACE ( (
 ( 1.000000000000000000, 0.7071067811865551223, 1.000000000000000000),
 ( 1.000000000000000000, 0.7211294902953088171, 1.000000000000000000),
 ( 1.000000000000000000, 0.7311181975231312302, 1.000000000000000000),
 ( 1.000000000000000000, 0.7429553055060466038, 1.000000000000000000),
 ( 1.000000000000000000, 0.7451698531058997821, 1.000000000000000000),
 ( 1.000000000000000000, 0.7452309222763021657, 1.000000000000000000) ) ) 
 REPRESENTATION_ITEM ( '' )  SURFACE ( )  );
#34022 = CARTESIAN_POINT ( 'NONE',  ( 1.430889623655247744, 4.024647178788855584, -0.4691377289697504227 ) ) ;
#34023 = VERTEX_POINT ( 'NONE', #159246 ) ;
#34024 = CARTESIAN_POINT ( 'NONE',  ( 4.863870654145381778, 0.5962773724161560818, -1.817021391602849034 ) ) ;
#34025 = CARTESIAN_POINT ( 'NONE',  ( 11.91826848676359596, 12.59166292761250538, -1.400000051401918855 ) ) ;
#34026 = CARTESIAN_POINT ( 'NONE',  ( 1.212636322461498217, -1.017548795778918214, -2.020700439389290892 ) ) ;
#34027 = CARTESIAN_POINT ( 'NONE',  ( -10.46653140006992899, 11.31330084294416771, -0.7216878364870267237 ) ) ;
#34028 = CARTESIAN_POINT ( 'NONE',  ( 1.318313199092124188, -0.6538357601561273214, -1.689641652304620045 ) ) ;
#34029 = CARTESIAN_POINT ( 'NONE',  ( 1.428765994036251818, -1.616370030362016985, 1.027966131488191381 ) ) ;
#34030 = CIRCLE ( 'NONE', #124121, 0.7500000000000011102 ) ;
#34031 = CARTESIAN_POINT ( 'NONE',  ( 2.980987059868035693, 1.948563265827065960, 0.6999735360200682877 ) ) ;
#34032 = CARTESIAN_POINT ( 'NONE',  ( 1.364683531249986537, 1.717708333674749399, -0.7879004041258239610 ) ) ;
#34033 = CARTESIAN_POINT ( 'NONE',  ( 0.6374961883623613268, -1.392493025731633027, -1.395827840033945000 ) ) ;
#34034 = CARTESIAN_POINT ( 'NONE',  ( 5.197847267195914611, -0.6914886683457229788, 1.798296804713859220 ) ) ;
#34036 = CARTESIAN_POINT ( 'NONE',  ( 6.011645680221167076, 7.072102904328817274, -1.053258377668888857 ) ) ;
#34035 = CARTESIAN_POINT ( 'NONE',  ( 1.436587813502993249, 1.134030013130071346, -2.009770128656597876 ) ) ;
#34037 = CARTESIAN_POINT ( 'NONE',  ( 0.6823417656249899377, 1.592708333674752730, 1.181850606188755259 ) ) ;
#34038 = CARTESIAN_POINT ( 'NONE',  ( 5.283662074727401681, -1.959763400824132251, 0.6436608119341418188 ) ) ;
#34039 = CARTESIAN_POINT ( 'NONE',  ( -5.551173829791513192, 8.563787670477010394, 1.199719254218452047 ) ) ;
#34040 = CARTESIAN_POINT ( 'NONE',  ( 8.925345196497941558, 9.307324238869423283, 1.040834085586084257E-14 ) ) ;
#34041 = CARTESIAN_POINT ( 'NONE',  ( 4.111146893441827821, 5.819424013814004759, 1.599625672291267175 ) ) ;
#34043 = CARTESIAN_POINT ( 'NONE',  ( -1.499999999999997780, 4.400000000000021672, 1.214306433183764966E-14 ) ) ;
#34042 = CARTESIAN_POINT ( 'NONE',  ( 5.368238606676455582, 1.035150450411811640, 1.833903993397972387 ) ) ;
#34044 = CARTESIAN_POINT ( 'NONE',  ( 0.6433370543819162402, -0.2662039958584628829, -2.154713702345659510 ) ) ;
#34045 = CARTESIAN_POINT ( 'NONE',  ( 0.6823417656249899377, 3.238541667008085323, -1.181850606188754593 ) ) ;
#34046 = CARTESIAN_POINT ( 'NONE',  ( 4.622454487542247747, 1.333869025858843482, -1.700861402727947169 ) ) ;
#34047 = CARTESIAN_POINT ( 'NONE',  ( 5.760417579480547445, 2.017467016246987210, 0.09685271086026786547 ) ) ;
#34048 = CARTESIAN_POINT ( 'NONE',  ( -0.1399997263889836974, 2.022132088033218533, -2.415689637818136948 ) ) ;
#34051 = CARTESIAN_POINT ( 'NONE',  ( 6.656690234629796699, 6.868486149930637552, 1.040834085586084257E-14 ) ) ;
#34050 = CARTESIAN_POINT ( 'NONE',  ( -3.285556943750000070, -2.559374999522041172, 0.000000000000000000 ) ) ;
#34049 = CARTESIAN_POINT ( 'NONE',  ( -0.8947579783427154210, 14.55305220401379174, -11.95586206112747085 ) ) ;
#34052 = CARTESIAN_POINT ( 'NONE',  ( -6.038177310039794854, 8.137902509836795417, -1.599625672291271394 ) ) ;
#34053 = CARTESIAN_POINT ( 'NONE',  ( 3.116422982138194353, 1.968445132739887748, 0.4370783100892047801 ) ) ;
#34054 = CARTESIAN_POINT ( 'NONE',  ( -8.528242318195895066, 9.908369778438709474, 1.199719254218462483 ) ) ;
#34056 = CARTESIAN_POINT ( 'NONE',  ( -10.99948089704804843, -5.389012432655393425, 0.1178541238725522855 ) ) ;
#34055 = CARTESIAN_POINT ( 'NONE',  ( -10.48008955368359629, 11.32911868882677986, 1.040834085586084257E-14 ) ) ;
#34057 = CARTESIAN_POINT ( 'NONE',  ( 0.6823417656249917140, 4.842708333674755394, 1.181850606188765695 ) ) ;
#34059 = DIRECTION ( 'NONE',  ( 0.000000000000000000, -1.000000000000000000, 0.000000000000000000 ) ) ;
#34058 = CARTESIAN_POINT ( 'NONE',  ( 5.436455051933180016, 2.129025116502227810, 0.3735886874452337691 ) ) ;
#34060 = CARTESIAN_POINT ( 'NONE',  ( -0.4000000000000131783, 3.049942316455299451, 0.4288785890452472271 ) ) ;
#34061 = CARTESIAN_POINT ( 'NONE',  ( 1.387358672525639269, 7.251968950354889643, 4.302625267139791987 ) ) ;
#34063 = CARTESIAN_POINT ( 'NONE',  ( 5.255482535091188012, 1.942537579172060047, -0.5405093616211650298 ) ) ;
#34062 = CARTESIAN_POINT ( 'NONE',  ( -6.792271770322117597, 9.907772251142352715, 1.082531754730549967 ) ) ;
#34064 = CARTESIAN_POINT ( 'NONE',  ( -1.201851678989727383E-14, 5.837500000000023448, -1.732050807568863648 ) ) ;
#34065 = CARTESIAN_POINT ( 'NONE',  ( 1.136830759877343722, -1.561040526032995590, 0.7340551814495520633 ) ) ;
#34066 = CARTESIAN_POINT ( 'NONE',  ( 3.725458348705031231, 7.568394850123006279, -1.734723475976807094E-15 ) ) ;
#34068 = CARTESIAN_POINT ( 'NONE',  ( 6.855582950365507244, 8.027210192628430718, -1.199719254218452047 ) ) ;
#34067 = CARTESIAN_POINT ( 'NONE',  ( 8.432808358020029260, 8.940623960552603222, 0.7216878364870438212 ) ) ;
#34069 = CARTESIAN_POINT ( 'NONE',  ( 1.836970198721030181E-16, 13.49999999999999822, 1.500000000000000222 ) ) ;
#34070 = CARTESIAN_POINT ( 'NONE',  ( 6.204356031920277736, -0.6731288877953770511, -1.745422550748019441 ) ) ;
#34071 = CARTESIAN_POINT ( 'NONE',  ( 6.363545146358847937, -1.619577101098391925, -1.195656717203520403 ) ) ;
#34072 = CARTESIAN_POINT ( 'NONE',  ( -1.500000000000038636, 8.500000000000000000, -10.64483442802187874 ) ) ;
#34073 =( BOUNDED_SURFACE ( )  B_SPLINE_SURFACE ( 3, 2, ( 
 ( #177589, #212189, #77941 ),
 ( #147231, #12923, #211125 ),
 ( #11864, #144062, #46528 ),
 ( #96355, #176516, #159192 ),
 ( #110516, #30269, #60622 ),
 ( #64886, #93154, #81146 ),
 ( #131032, #114775, #162410 ),
 ( #63827, #129985, #27046 ) ),
 .UNSPECIFIED., .F., .F., .T. ) 
 B_SPLINE_SURFACE_WITH_KNOTS ( ( 4, 2, 2, 4 ),
 ( 3, 3 ),
 ( 0.000000000000000000, 0.0005123566476021777739, 0.0007685349714032666067, 0.001024713295204355548 ),
 ( 0.000000000000000000, 1.000000000000000000 ),
 .UNSPECIFIED. ) 
 GEOMETRIC_REPRESENTATION_ITEM ( )  RATIONAL_B_SPLINE_SURFACE ( (
 ( 1.000000000000000000, 0.7100530722026825448, 1.000000000000000000),
 ( 1.000000000000000000, 0.7667719522827929346, 1.000000000000000000),
 ( 1.000000000000000000, 0.8160440554222314624, 1.000000000000000000),
 ( 1.000000000000000000, 0.8737249316770007157, 1.000000000000000000),
 ( 1.000000000000000000, 0.8903164784319989034, 1.000000000000000000),
 ( 1.000000000000000000, 0.9150853305241244406, 1.000000000000000000),
 ( 1.000000000000000000, 0.9227739504732713760, 1.000000000000000000),
 ( 1.000000000000000000, 0.9238795325112854062, 1.000000000000000000) ) ) 
 REPRESENTATION_ITEM ( '' )  SURFACE ( )  );
#34074 = CIRCLE ( 'NONE', #141278, 0.07999999999999961309 ) ;
#34075 = CARTESIAN_POINT ( 'NONE',  ( -7.553300976144794454, 7.984808358356614733, -0.7216878364870338292 ) ) ;
#34076 = ORIENTED_EDGE ( 'NONE', *, *, #25609, .T. ) ;
#34077 = CARTESIAN_POINT ( 'NONE',  ( 9.042925270190632858, 10.61279623905300085, 1.082531754730549967 ) ) ;
#34079 = CARTESIAN_POINT ( 'NONE',  ( 2.144157856786413241, 0.8647422840215597262, 1.821734841475818101 ) ) ;
#34078 = CARTESIAN_POINT ( 'NONE',  ( 2.473420802178166067, -1.846219560914775570, -1.042883725575906029 ) ) ;
#34080 = CARTESIAN_POINT ( 'NONE',  ( 2.337905319157699502, -1.045887089798164915, -1.478944033197209462 ) ) ;
#34081 = CARTESIAN_POINT ( 'NONE',  ( 4.882344714252594642, 4.868692719482363707, 0.000000000000000000 ) ) ;
#34082 = CARTESIAN_POINT ( 'NONE',  ( 6.579002408576895000, -0.1006694238701970334, -2.159482418181729813 ) ) ;
#34083 = ORIENTED_EDGE ( 'NONE', *, *, #167754, .T. ) ;
#34084 = CARTESIAN_POINT ( 'NONE',  ( 7.935599982700328958, 8.152621489438862667, 0.7998128361456481317 ) ) ;
#34086 = CARTESIAN_POINT ( 'NONE',  ( 0.1806861152609346710, 1.591142543434557632, -1.066548322639774504 ) ) ;
#34085 = CARTESIAN_POINT ( 'NONE',  ( -5.392392409933270514, 7.314210449720692786, 1.599625672291269396 ) ) ;
#34087 = AXIS2_PLACEMENT_3D ( 'NONE', #4046, #136227, #150343 ) ;
#34088 = SURFACE_STYLE_FILL_AREA ( #136940 ) ;
#34089 = CARTESIAN_POINT ( 'NONE',  ( 1.464175926609780964E-14, -2.493749999044085452, -3.475000000000000533 ) ) ;
#34090 = CARTESIAN_POINT ( 'NONE',  ( 6.114364089638798738, 6.235772314107808079, 0.7216878364870317197 ) ) ;
#34091 = CARTESIAN_POINT ( 'NONE',  ( -1.364683531250014514, 0.05104166700808546175, -0.7879004041258359514 ) ) ;
#34092 = CARTESIAN_POINT ( 'NONE',  ( 3.470524135418292300, 5.072030796119872953, -1.443375672974057666 ) ) ;
#34093 = CARTESIAN_POINT ( 'NONE',  ( -9.646789991323334590, 11.21334206375407305, 1.199719254218462483 ) ) ;
#34094 = CARTESIAN_POINT ( 'NONE',  ( 4.206063578812153203, -2.156103337031569200, 0.1562769059922017589 ) ) ;
#34095 = CARTESIAN_POINT ( 'NONE',  ( -6.509323148336870091, 7.727203440215372865, 1.082531754730549078 ) ) ;
#34096 = CARTESIAN_POINT ( 'NONE',  ( 6.061904079085887354, 6.244845311787889486, 0.000000000000000000 ) ) ;
#34097 = CARTESIAN_POINT ( 'NONE',  ( 2.355864820516640812, -1.574449018071517825, -1.420800595792824028 ) ) ;
#34098 = DIRECTION ( 'NONE',  ( -1.000000000000000000, -0.000000000000000000, -2.168404344971003504E-14 ) ) ;
#34099 = CARTESIAN_POINT ( 'NONE',  ( 3.497303454036035930, 1.552041748764835249, 1.215357900914854516 ) ) ;
#34100 = CARTESIAN_POINT ( 'NONE',  ( 5.467032840998240495, -1.503656711810175350, 1.181500457595338505 ) ) ;
#34101 = ORIENTED_EDGE ( 'NONE', *, *, #127328, .T. ) ;
#34102 = CARTESIAN_POINT ( 'NONE',  ( 4.353576723319602770, 8.093273587265924718, -0.7216878364870386031 ) ) ;
#34103 = CARTESIAN_POINT ( 'NONE',  ( 5.723099352235532677, -1.779878778038428200, -0.8436364978330126441 ) ) ;
#34104 = CARTESIAN_POINT ( 'NONE',  ( 1.992034801999421623, -0.5177828490160235608, -1.871580480717034645 ) ) ;
#34105 = CARTESIAN_POINT ( 'NONE',  ( -3.284818356260900796, 7.054314858938165678, 0.7998128361456352531 ) ) ;
#34107 = CARTESIAN_POINT ( 'NONE',  ( 6.556249800660121529, 9.806652646482286073, 1.199719254218452047 ) ) ;
#34106 = CARTESIAN_POINT ( 'NONE',  ( -5.804299160426229953, 8.825413882922319431, -1.082531754730549967 ) ) ;
#34108 = CARTESIAN_POINT ( 'NONE',  ( 5.947222937888848371, 10.09017719417900416, 1.040834085586084257E-14 ) ) ;
#34110 = CARTESIAN_POINT ( 'NONE',  ( 5.872089928050205465, 6.023395468912922546, -0.7216878364870458196 ) ) ;
#34109 = CARTESIAN_POINT ( 'NONE',  ( 5.296431564432884542, 9.330920591813708143, 1.040834085586084257E-14 ) ) ;
#34112 = EDGE_LOOP ( 'NONE', ( #54891, #14267, #203242, #137159, #153887, #182733, #201335, #50629, #122930, #129270, #193938, #152659, #206365, #100989, #191491, #83168, #90606, #160927, #184296, #196475, #98774 ) ) ;
#34111 = CARTESIAN_POINT ( 'NONE',  ( 5.690081826675051246, 1.142623417513729089, 1.533212917768103534 ) ) ;
#34113 = CARTESIAN_POINT ( 'NONE',  ( 2.789901687333019797, 1.561178712900921584, 1.560079944692857046 ) ) ;
#34114 = CARTESIAN_POINT ( 'NONE',  ( 2.239569982544288518, -1.971322999760493300, 0.9919465654871155724 ) ) ;
#34115 = AXIS2_PLACEMENT_3D ( 'NONE', #179989, #33721, #147496 ) ;
#34116 = CARTESIAN_POINT ( 'NONE',  ( 0.3728825314828371762, 3.227879828479794710, -0.5317689764002981878 ) ) ;
#34117 = CARTESIAN_POINT ( 'NONE',  ( 1.066890508724306130, -1.507026839618429426, 1.177014404800474479 ) ) ;
#34118 = DIRECTION ( 'NONE',  ( 0.000000000000000000, 0.000000000000000000, 1.000000000000000000 ) ) ;
#34119 = CARTESIAN_POINT ( 'NONE',  ( 10.07387183015377197, 11.71160420905630062, -1.199719254218440723 ) ) ;
#34120 = CARTESIAN_POINT ( 'NONE',  ( 4.633297751427937428, 0.003287558298453730800, -2.070544812459538253 ) ) ;
#34121 = CARTESIAN_POINT ( 'NONE',  ( -4.303823697334223652, 7.108545849276850959, -1.199719254218452047 ) ) ;
#34123 = CARTESIAN_POINT ( 'NONE',  ( 1.903414394802248166, 1.797162532295241366, 1.201017911493490020 ) ) ;
#34122 = CARTESIAN_POINT ( 'NONE',  ( -2.930533758848195447, 6.570706485298192234, -0.7998128361456281477 ) ) ;
#34124 = CARTESIAN_POINT ( 'NONE',  ( 3.456733517523991051, -1.933646301634945885, -1.031433503814835007 ) ) ;
#34125 = CARTESIAN_POINT ( 'NONE',  ( -0.02069724287496089998, 3.480000000000000426, -2.000000000000000000 ) ) ;
#34126 = EDGE_CURVE ( 'NONE', #86318, #128668, #165443, .T. ) ;
#34127 = FILL_AREA_STYLE ('',( #203005 ) ) ;
#34128 = CARTESIAN_POINT ( 'NONE',  ( 1.451998047839293315, 7.315968950356647404, 4.301760722583980900 ) ) ;
#34129 = CARTESIAN_POINT ( 'NONE',  ( -1.402160292154681736E-14, 14.48437500034139980, 1.575800808251682339 ) ) ;
#34130 = CARTESIAN_POINT ( 'NONE',  ( -6.493429226302317225, 6.540365283632955773, 0.7998128361456341429 ) ) ;
#34131 = EDGE_CURVE ( 'NONE', #30345, #160120, #96375, .T. ) ;
#34132 = CARTESIAN_POINT ( 'NONE',  ( 5.537694164425770005, -1.361542515911953855, 1.073868356900798959 ) ) ;
#34133 = CARTESIAN_POINT ( 'NONE',  ( -4.288456660624211381, 3.897620947016656956, 1.214306433183764966E-14 ) ) ;
#34134 = CARTESIAN_POINT ( 'NONE',  ( 3.045825399726838079, 1.460771095745692527, 1.467265538693182991 ) ) ;
#34135 = CARTESIAN_POINT ( 'NONE',  ( 5.396159345875370938, -0.9528639288615829983, -1.890782970011774422 ) ) ;
#34136 = CARTESIAN_POINT ( 'NONE',  ( 6.986529229743720926, 7.045372277656132276, -0.7998128361456281477 ) ) ;
#34137 = CARTESIAN_POINT ( 'NONE',  ( -1.364683531250012516, 3.988541667008088432, -0.7879004041258300672 ) ) ;
#34138 = CARTESIAN_POINT ( 'NONE',  ( 2.992966325197043531, 0.2361965902525232364, 1.955129705961492270 ) ) ;
#34139 = CARTESIAN_POINT ( 'NONE',  ( 0.6328886395040033142, 1.767934563615305432, 0.7296191750566642931 ) ) ;
#34140 = CARTESIAN_POINT ( 'NONE',  ( 5.736350775408121550, 0.4420370857395071740, 2.249087507758650517 ) ) ;
#34141 = CARTESIAN_POINT ( 'NONE',  ( 2.402731849113007190, 1.466575434288765800, -1.087121784572639527 ) ) ;
#34142 = CARTESIAN_POINT ( 'NONE',  ( 4.848976215542928792, 5.686169002002086970, 1.199719254218452047 ) ) ;
#34143 = CARTESIAN_POINT ( 'NONE',  ( 3.836594282542902246, 7.419851063034623273, 0.7216878364870317197 ) ) ;
#34144 = CARTESIAN_POINT ( 'NONE',  ( -5.682838942422375084, 9.781729199468104596, 0.000000000000000000 ) ) ;
#34145 = ORIENTED_EDGE ( 'NONE', *, *, #73487, .F. ) ;
#34146 = VERTEX_POINT ( 'NONE', #205859 ) ;
#34147 = CARTESIAN_POINT ( 'NONE',  ( 4.078389064453043389, 0.9529185939490876223, 1.773430079992607045 ) ) ;
#34148 = CARTESIAN_POINT ( 'NONE',  ( 4.258614474744500278, -0.6113484564182982695, -1.864166799412938502 ) ) ;
#34149 = CARTESIAN_POINT ( 'NONE',  ( -7.507464373665155399, 9.781794407407920389, 1.599625672291295375 ) ) ;
#34150 = CARTESIAN_POINT ( 'NONE',  ( -5.274285450916075035, 6.112086766612214284, 1.199719254218450271 ) ) ;
#34151 = FACE_OUTER_BOUND ( 'NONE', #195204, .T. ) ;
#34153 = CARTESIAN_POINT ( 'NONE',  ( 6.227411129102443432, -1.664988906758845921, 0.6005623136680103835 ) ) ;
#34152 = CARTESIAN_POINT ( 'NONE',  ( -0.07645973585807680495, -1.289725328510348934, -1.646077999003342729 ) ) ;
#34154 = CARTESIAN_POINT ( 'NONE',  ( 10.99462479582585317, -5.166863022246526604, -0.3540227772641220683 ) ) ;
#34155 = CARTESIAN_POINT ( 'NONE',  ( 1.992365796559266267, -0.5863786240636535974, -2.111471653062434672 ) ) ;
#34156 = CARTESIAN_POINT ( 'NONE',  ( -0.09478571475088257148, -0.7418789811804274992, -1.573373712294885207 ) ) ;
#34157 = AXIS2_PLACEMENT_3D ( 'NONE', #164852, #99857, #34832 ) ;
#34158 = CARTESIAN_POINT ( 'NONE',  ( 8.111855979677986994, 8.358253485912799263, 1.040834085586084257E-14 ) ) ;
#34159 = CARTESIAN_POINT ( 'NONE',  ( 0.5742808809356505506, -1.622453496466894407, -0.5859570326207633739 ) ) ;
#34160 = CARTESIAN_POINT ( 'NONE',  ( 0.2577194443907256383, 2.166829308800602316, -0.3276212646995610989 ) ) ;
#34161 = CARTESIAN_POINT ( 'NONE',  ( 6.186827581914116081, -0.9662774195124073096, -1.439361474112188954 ) ) ;
#34162 = CARTESIAN_POINT ( 'NONE',  ( 2.930518499080053907, 1.225513248159842083, -1.835134156090315605 ) ) ;
#34163 = CARTESIAN_POINT ( 'NONE',  ( 6.848074921520021618, -0.9335981340678388696, 1.958013476854936652 ) ) ;
#34164 = CARTESIAN_POINT ( 'NONE',  ( -1.217323170181719538, 2.986755683774202197, 0.7750000000000152323 ) ) ;
#34165 = CARTESIAN_POINT ( 'NONE',  ( 1.815762809344774187, -1.387149605378830586, -1.599721994570136197 ) ) ;
#34166 = CARTESIAN_POINT ( 'NONE',  ( 6.827182134110196365, 7.629137130509086262, 2.889055895399252005 ) ) ;
#34167 = CARTESIAN_POINT ( 'NONE',  ( 5.508790920392054424, 1.458765576344657866, -1.258282468310659707 ) ) ;
#34169 = CARTESIAN_POINT ( 'NONE',  ( -1.500000000000011324, 5.379166666666692187, -0.8660254037844313801 ) ) ;
#34168 = CARTESIAN_POINT ( 'NONE',  ( 3.087719631786550956, -0.9270648334414759439, 2.096714421332421807 ) ) ;
#34170 = CARTESIAN_POINT ( 'NONE',  ( 3.063252641683779753, 5.661212951017999373, 1.199719254218450271 ) ) ;
#34171 = CARTESIAN_POINT ( 'NONE',  ( 4.157546660884947620, 8.002221537674429896, 1.040834085586084257E-14 ) ) ;
#34172 = CARTESIAN_POINT ( 'NONE',  ( 5.039773670486915158, -2.109617592216144644, 0.6956167390435584741 ) ) ;
#34173 = CARTESIAN_POINT ( 'NONE',  ( -8.351459436338048548, 8.845716885256940998, -0.7216878364870278340 ) ) ;
#34174 = CARTESIAN_POINT ( 'NONE',  ( -5.914749137557818059, 6.074338953224275528, -0.6118981238392419142 ) ) ;
#34175 = CARTESIAN_POINT ( 'NONE',  ( 5.287316719649520991, 8.151991358691011769, -1.082531754730549078 ) ) ;
#34176 = CARTESIAN_POINT ( 'NONE',  ( -9.314088342463968218, 9.968783942403868892, 0.7216878364870438212 ) ) ;
#34177 = CARTESIAN_POINT ( 'NONE',  ( 6.712695452541852070, 7.004101914153185504, 0.000000000000000000 ) ) ;
#34178 = EDGE_LOOP ( 'NONE', ( #104709, #183409, #164864, #163847 ) ) ;
#34179 = CARTESIAN_POINT ( 'NONE',  ( 2.584611472894111195, -0.6298744119781033435, 1.915600275669691488 ) ) ;
#34181 = CARTESIAN_POINT ( 'NONE',  ( 0.6024794235527919373, 2.056786662827071233, 0.1555941968269194953 ) ) ;
#34180 = CARTESIAN_POINT ( 'NONE',  ( 6.588372581236919601, 9.773852880496709972, -1.199719254218440723 ) ) ;
#34182 = CARTESIAN_POINT ( 'NONE',  ( 6.170369307550815030, 8.292126506933040986, 1.443375672974064550 ) ) ;
#34183 = CARTESIAN_POINT ( 'NONE',  ( -2.301756715112211360, 5.497064121812672788, -0.7511966642406193717 ) ) ;
#34184 = CARTESIAN_POINT ( 'NONE',  ( 1.364683531249988535, 3.155208333674756283, -0.7879004041258239610 ) ) ;
#34185 = CARTESIAN_POINT ( 'NONE',  ( 3.644632398932126094, -1.791719913761843364, 1.261548167004488130 ) ) ;
#34186 = CARTESIAN_POINT ( 'NONE',  ( 1.617814789376757156, 0.2004366740697149929, 2.006445999502483257 ) ) ;
#34187 = CARTESIAN_POINT ( 'NONE',  ( 1.382094229771430705, -0.2707140722739818650, -1.821126350552772610 ) ) ;
#34188 = CARTESIAN_POINT ( 'NONE',  ( 5.355124402800013783, 0.4497703203518633175, -2.247661708361737620 ) ) ;
#34189 = CARTESIAN_POINT ( 'NONE',  ( 4.031074566243696644, -1.271087849624694233, -1.332192834049110486 ) ) ;
#34190 = ADVANCED_FACE ( 'NONE', ( #206924 ), #61754, .T. ) ;
#34191 = CARTESIAN_POINT ( 'NONE',  ( 6.760712154708803823, 11.03924794713562818, 1.040834085586084257E-14 ) ) ;
#34192 = CARTESIAN_POINT ( 'NONE',  ( 4.524309061075334704, 1.122661849025725189, -1.439470297551891154 ) ) ;
#34193 = CARTESIAN_POINT ( 'NONE',  ( 4.465470312728934132, -1.956561007648183192, -0.4872041746135646889 ) ) ;
#34194 = CARTESIAN_POINT ( 'NONE',  ( -8.636707547105197946, 10.03491254549959777, -1.199719254218446718 ) ) ;
#34196 = CARTESIAN_POINT ( 'NONE',  ( -5.824109505522200081, 8.952488968821326054, -1.199719254218452047 ) ) ;
#34195 = CARTESIAN_POINT ( 'NONE',  ( 5.084992976345711568, -0.2718087151927280343, -2.246069130642995404 ) ) ;
#34197 = CARTESIAN_POINT ( 'NONE',  ( 6.247117736759643769, -1.781108002423707592, 1.123397916191863244 ) ) ;
#34198 = SURFACE_STYLE_FILL_AREA ( #198816 ) ;
#34199 = CARTESIAN_POINT ( 'NONE',  ( 4.773920332862017446, -2.031068740936771366, 0.4005940302675218834 ) ) ;
#34200 = CARTESIAN_POINT ( 'NONE',  ( 10.07778825365955733, 10.65184113889131012, -0.7998128361456281477 ) ) ;
#34201 = CARTESIAN_POINT ( 'NONE',  ( -1.580000000000001625, -1.099999999999982991, -2.579999999999989413 ) ) ;
#34202 = APPLICATION_PROTOCOL_DEFINITION ( 'draft international standard', 'automotive_design', 1998, #97515 ) ;
#34204 = CARTESIAN_POINT ( 'NONE',  ( 2.561056213344356181, -1.676160556340213992, -0.9495491084439124929 ) ) ;
#34203 = CARTESIAN_POINT ( 'NONE',  ( -9.040589502214116280, 9.441775928871617651, 0.7998128361456462443 ) ) ;
#34205 = UNCERTAINTY_MEASURE_WITH_UNIT (LENGTH_MEASURE( 1.000000000000000082E-05 ), #105597, 'distance_accuracy_value', 'NONE');
#34206 = SURFACE_STYLE_FILL_AREA ( #64591 ) ;
#34207 = CARTESIAN_POINT ( 'NONE',  ( 6.578958714233388072, 1.836342173298356917, 0.7121609383471518839 ) ) ;
#34208 = CARTESIAN_POINT ( 'NONE',  ( 5.515134625708930649, 9.656350506627580543, 0.000000000000000000 ) ) ;
#34209 = CARTESIAN_POINT ( 'NONE',  ( 4.739561450132447007, 6.795411536013346243, -1.240012687728889951 ) ) ;
#34210 = CARTESIAN_POINT ( 'NONE',  ( -3.765413976293358278, 5.416068943807445635, 1.599625672291267398 ) ) ;
#34212 = CARTESIAN_POINT ( 'NONE',  ( 1.758359454726521998, 0.8447074013377148249, -2.054735579953733904 ) ) ;
#34211 = CARTESIAN_POINT ( 'NONE',  ( 1.019968326173793960, -0.5097545255977399270, 2.058319881341897695 ) ) ;
#34213 = CARTESIAN_POINT ( 'NONE',  ( 3.522586592847714471, 1.337535325648725459, -1.626654721158872885 ) ) ;
#34214 = CARTESIAN_POINT ( 'NONE',  ( -7.099629715411508890, 8.311931418515415615, 1.199719254218452047 ) ) ;
#34215 = CARTESIAN_POINT ( 'NONE',  ( 6.938021921891177612, 9.117444880338284818, -1.599625672291262513 ) ) ;
#34216 = CARTESIAN_POINT ( 'NONE',  ( 2.699599903323801620, -1.451799986561516764, -1.319707477925702310 ) ) ;
#34217 = CARTESIAN_POINT ( 'NONE',  ( 4.299907273828439180, 8.168308919441841454, 1.040834085586084257E-14 ) ) ;
#34218 = CARTESIAN_POINT ( 'NONE',  ( -4.124570878694319376, 7.473888947179561981, -0.6522657496016289747 ) ) ;
#34219 = CARTESIAN_POINT ( 'NONE',  ( 5.657830175604453338, 5.495223381160312393, 0.7998128361456341429 ) ) ;
#34220 = CARTESIAN_POINT ( 'NONE',  ( -5.153507786970267013, 8.066157280557016307, -1.082531754730549967 ) ) ;
#34221 = CARTESIAN_POINT ( 'NONE',  ( -6.832946231607472498, 9.955225789308602913, 1.082531754730549967 ) ) ;
#34223 = CARTESIAN_POINT ( 'NONE',  ( 1.459403507577087700, -1.788631592985808538, 1.138920039206146928 ) ) ;
#34222 = AXIS2_PLACEMENT_3D ( 'NONE', #210784, #192392, #146890 ) ;
#34224 = CARTESIAN_POINT ( 'NONE',  ( -5.152980901645737077, 8.169505597632108262, -1.199719254218453823 ) ) ;
#34226 = CARTESIAN_POINT ( 'NONE',  ( 4.879329150013382410, -0.09822140645733207220, 1.959542894978071992 ) ) ;
#34225 = CARTESIAN_POINT ( 'NONE',  ( -1.225000000000028066, 1.229166666666677843, -0.7072540797573076965 ) ) ;
#34227 = CARTESIAN_POINT ( 'NONE',  ( 3.450221060135277629, 2.161883445724331665, 0.001893877739161941697 ) ) ;
#34228 = CARTESIAN_POINT ( 'NONE',  ( 2.436835438956724165, -1.365703447793526149, -1.235134912642745553 ) ) ;
#34229 = CARTESIAN_POINT ( 'NONE',  ( -4.236586233130071655, 7.334480220043515075, -0.8772045297030308664 ) ) ;
#34230 = CARTESIAN_POINT ( 'NONE',  ( -1.402160292154681736E-14, -1.115624999658584082, 1.575800808251672791 ) ) ;
#34231 = CARTESIAN_POINT ( 'NONE',  ( 4.523245630038312370, -1.073764689188366317, -1.369494959904279829 ) ) ;
#34232 = CARTESIAN_POINT ( 'NONE',  ( -1.419999999999997708, 6.280000000000035776, -3.469446951953614189E-15 ) ) ;
#34233 = CARTESIAN_POINT ( 'NONE',  ( 6.019457014787495730, 6.125047393447951016, -0.7216878364870257245 ) ) ;
#34234 = CARTESIAN_POINT ( 'NONE',  ( -10.16827420574893814, 6.288608293322982767, 5.589418380748610637 ) ) ;
#34235 = CARTESIAN_POINT ( 'NONE',  ( 1.956163130892615731, 2.155914767609674598, -0.1587918856347721730 ) ) ;
#34236 = CARTESIAN_POINT ( 'NONE',  ( 5.061874962716293780, 1.677747168027879709, -1.117663061872615771 ) ) ;
#34237 = CARTESIAN_POINT ( 'NONE',  ( -10.58855478214856660, 11.45566145536924552, -0.7216878364870217277 ) ) ;
#34238 = AXIS2_PLACEMENT_3D ( 'NONE', #177445, #176382, #195821 ) ;
#34239 = CARTESIAN_POINT ( 'NONE',  ( 1.622176833581047806, -1.201014165160016356, -1.797165035535647659 ) ) ;
#34240 = CARTESIAN_POINT ( 'NONE',  ( 3.573081558413326864, 0.04979752193529430465, -1.971001165494235652 ) ) ;
#34241 = B_SPLINE_CURVE_WITH_KNOTS ( 'NONE', 3,
 ( #112670, #180793, #178679, #47628, #144085, #45489 ),
 .UNSPECIFIED., .F., .F.,
 ( 4, 2, 4 ),
 ( 0.000000000000000000, 0.0003155923098472858596, 0.0006311846196945720446 ),
 .UNSPECIFIED. ) ;
#34242 = CARTESIAN_POINT ( 'NONE',  ( 0.000000000000000000, -5.166862915010159263, 0.000000000000000000 ) ) ;
#34243 = CARTESIAN_POINT ( 'NONE',  ( 3.052217916795424202, -1.468930141372110088, 1.270444820450331358 ) ) ;
#34247 = ORIENTED_EDGE ( 'NONE', *, *, #24409, .F. ) ;
#34246 = EDGE_CURVE ( 'NONE', #202349, #152273, #34030, .T. ) ;
#34245 = CARTESIAN_POINT ( 'NONE',  ( -4.502716413514313842, 5.386162249589033557, -1.082531754730549967 ) ) ;
#34244 = CARTESIAN_POINT ( 'NONE',  ( -10.12757755928392456, 10.91785469536048758, 0.7216878364870438212 ) ) ;
#34248 = CARTESIAN_POINT ( 'NONE',  ( -4.963693635934603776, 4.963599794778024155, 0.000000000000000000 ) ) ;
#34249 = CARTESIAN_POINT ( 'NONE',  ( -4.782994330570982555, 8.802186828966616972, 0.000000000000000000 ) ) ;
#34250 = CARTESIAN_POINT ( 'NONE',  ( -8.310784975052671442, 11.67937098999472667, -1.082531754730543083 ) ) ;
#34251 = EDGE_CURVE ( 'NONE', #7055, #26620, #51361, .T. ) ;
#34252 = CARTESIAN_POINT ( 'NONE',  ( 0.3587983166186413109, 0.8468606107991830667, 2.038007455039527294 ) ) ;
#34253 = CARTESIAN_POINT ( 'NONE',  ( -3.285556943750000070, -3.609374999522043659, 0.000000000000000000 ) ) ;
#34254 = CARTESIAN_POINT ( 'NONE',  ( 5.629730433169950921, 1.891637868780412068, -0.5196590155819302836 ) ) ;
#34255 = CARTESIAN_POINT ( 'NONE',  ( 1.424454163599726320, -1.462446849824734274, -1.388484543128357229 ) ) ;
#34256 = ORIENTED_EDGE ( 'NONE', *, *, #20771, .T. ) ;
#34257 = CARTESIAN_POINT ( 'NONE',  ( 3.643865571896960809, 2.100859469783818323, -0.2634356371126170826 ) ) ;
#34258 = CARTESIAN_POINT ( 'NONE',  ( 1.499999999999989120, 2.285416667349482012, 0.8660254037844524744 ) ) ;
#34260 = CARTESIAN_POINT ( 'NONE',  ( -6.043183783389232566, 8.073467052085995022, 1.599625672291269396 ) ) ;
#34259 = CARTESIAN_POINT ( 'NONE',  ( 9.579665964947855272, -7.246166700193438892, -1.544988095791843818E-15 ) ) ;
#34261 = CARTESIAN_POINT ( 'NONE',  ( 4.259580805731934205, 0.8699401392010926992, 1.622648742527862620 ) ) ;
#34262 = VERTEX_POINT ( 'NONE', #158204 ) ;
#34263 = CARTESIAN_POINT ( 'NONE',  ( -9.671043645249580933, 10.17730576241299900, 0.7998128361456462443 ) ) ;
#34264 = CARTESIAN_POINT ( 'NONE',  ( 4.746395313581045272, 1.087821826000658909, -1.820160695957805608 ) ) ;
#34265 = CARTESIAN_POINT ( 'NONE',  ( -1.499999999999990896, 4.410416667349482900, -0.8660254037844429265 ) ) ;
#34266 = CARTESIAN_POINT ( 'NONE',  ( 5.666418135507635512, 8.698239360479199433, 1.199719254218462483 ) ) ;
#34267 = ORIENTED_EDGE ( 'NONE', *, *, #63494, .T. ) ;
#34268 = CARTESIAN_POINT ( 'NONE',  ( 5.835248319207797074, -1.864956875241881251, 0.8770506743334179900 ) ) ;
#34269 = CIRCLE ( 'NONE', #155339, 0.08000000000000041800 ) ;
#34272 = CARTESIAN_POINT ( 'NONE',  ( 2.682954136603598272, 1.303717545168959990, 1.300458928786947688 ) ) ;
#34271 = CARTESIAN_POINT ( 'NONE',  ( 1.170091191536073660, -0.8321358839059491697, -1.664716676500255010 ) ) ;
#34270 = CARTESIAN_POINT ( 'NONE',  ( -4.450808633097269151, 7.987047222781179734, -2.500000000000000444 ) ) ;
#34273 = CARTESIAN_POINT ( 'NONE',  ( 7.587759525142423911, 12.00413654597487501, 0.7998128361456462443 ) ) ;
#34274 = CARTESIAN_POINT ( 'NONE',  ( -15.75000000000000000, 9.799999999999998934, 0.6999999999999992895 ) ) ;
#34275 = CARTESIAN_POINT ( 'NONE',  ( 0.000000000000000000, 11.29999999999999893, 0.000000000000000000 ) ) ;
#34276 = CARTESIAN_POINT ( 'NONE',  ( 2.631697372267821855, -2.058793095894187353, 0.7952504953367269813 ) ) ;
#34277 = CARTESIAN_POINT ( 'NONE',  ( 5.343176995970949861, -1.944282970029135083, 1.156607043288411019 ) ) ;
#34278 = CARTESIAN_POINT ( 'NONE',  ( -5.897433632264490910, 9.824163637709826702, 0.000000000000000000 ) ) ;
#34279 = CARTESIAN_POINT ( 'NONE',  ( 4.535318187750695174, -0.08185482751379420663, 1.809849901470663491 ) ) ;
#34280 = CARTESIAN_POINT ( 'NONE',  ( 5.841025094292755071, -1.646784362596087625, -0.9785371348113005574 ) ) ;
#34281 = CARTESIAN_POINT ( 'NONE',  ( -1.001543065824772872E-14, 5.134375000341421469, 1.575800808251672791 ) ) ;
#34282 = CARTESIAN_POINT ( 'NONE',  ( 5.084763247618332649, -0.2297073032716222263, -1.856415652357709778 ) ) ;
#34283 = AXIS2_PLACEMENT_3D ( 'NONE', #17516, #164862, #66258 ) ;
#34284 = CARTESIAN_POINT ( 'NONE',  ( 4.703460533163725366, -1.437978410778781857, -1.181371033526560144 ) ) ;
#34285 = CARTESIAN_POINT ( 'NONE',  ( 0.6823417656249917140, 5.092708333674749177, 1.181850606188765695 ) ) ;
#34286 = ADVANCED_FACE ( 'NONE', ( #123652 ), #107370, .F. ) ;
#34287 = CARTESIAN_POINT ( 'NONE',  ( 6.825078400183545391, 0.005516643811322509937, 1.755566376062764222 ) ) ;
#34288 = CARTESIAN_POINT ( 'NONE',  ( 0.1632964843477149597, 1.879801964727344732, -0.7303121171872913875 ) ) ;
#34290 = CARTESIAN_POINT ( 'NONE',  ( 1.365998295032941900, 2.074639164447332540, -0.3615360007043573187 ) ) ;
#34289 = CARTESIAN_POINT ( 'NONE',  ( -2.277406616971334508, 5.600798786534425311, 1.040834085586084257E-14 ) ) ;
#34291 = CARTESIAN_POINT ( 'NONE',  ( 9.911173986789782120, 11.52179005846497972, -1.199719254218440723 ) ) ;
#34293 = DIRECTION ( 'NONE',  ( -1.000000000000000000, 5.459311322609750190E-16, -1.776356839400250465E-15 ) ) ;
#34292 = FACE_OUTER_BOUND ( 'NONE', #179164, .T. ) ;
#34294 = CARTESIAN_POINT ( 'NONE',  ( -10.23541933785880431, 1.000000000000000888, -6.134053304049098543 ) ) ;
#34295 = CARTESIAN_POINT ( 'NONE',  ( 1.828384590600404591, -0.9557513975326953348, -1.779375440769872752 ) ) ;
#34296 = CARTESIAN_POINT ( 'NONE',  ( -1.364683531250012516, 2.280208333674751842, 0.7879004041258379498 ) ) ;
#34297 = CARTESIAN_POINT ( 'NONE',  ( 6.620655732516643965, 2.083750514537034970, 2.135603474206409835 ) ) ;
#34298 = CARTESIAN_POINT ( 'NONE',  ( 5.007038802148489509, 4.735966778795008381, 0.7998128361456341429 ) ) ;
#34299 = ORIENTED_EDGE ( 'NONE', *, *, #142583, .F. ) ;
#34300 = CARTESIAN_POINT ( 'NONE',  ( 2.688937055384226671, -0.3666181952855402382, -2.130111032054008646 ) ) ;
#34301 = CARTESIAN_POINT ( 'NONE',  ( 6.610000000000006537, 2.052567036419289614, 2.306714106643445561 ) ) ;
#34303 = CARTESIAN_POINT ( 'NONE',  ( 1.499999999999993117, 13.13541666734946567, 0.8660254037844408170 ) ) ;
#34302 = CARTESIAN_POINT ( 'NONE',  ( 4.706615602599436343, 5.520081620234675412, 1.199719254218452935 ) ) ;
#34304 = CARTESIAN_POINT ( 'NONE',  ( 8.229436053370667636, 11.58446391469906267, 1.082531754730558626 ) ) ;
#34305 = CARTESIAN_POINT ( 'NONE',  ( -7.266807147244793263, 8.540658428949452485, 1.082531754730549967 ) ) ;
#34306 = CARTESIAN_POINT ( 'NONE',  ( 0.5213437761196970666, -2.079166062760181788, 0.6930039600180630810 ) ) ;
#34307 = CARTESIAN_POINT ( 'NONE',  ( 0.04711431077958990604, 7.150937050890798119, 2.000088718513667541 ) ) ;
#34308 = CARTESIAN_POINT ( 'NONE',  ( 1.938691616020698172, 2.238021082172815479, 0.3313278802117639033 ) ) ;
#34309 = CARTESIAN_POINT ( 'NONE',  ( -7.965578943228732278, 9.251929174310385307, -1.199719254218446718 ) ) ;
#34310 = CARTESIAN_POINT ( 'NONE',  ( -5.382223794500852421, 5.381608636446842731, -0.7216878364870197293 ) ) ;
#34312 = STYLED_ITEM ( 'NONE', ( #25228 ), #44250 ) ;
#34311 = CARTESIAN_POINT ( 'NONE',  ( -1.201851678989727383E-14, 3.134375000341420137, 1.575800808251672791 ) ) ;
#34313 = CARTESIAN_POINT ( 'NONE',  ( 4.651083699394226834, 8.303454393088664176, 0.4639335724816190942 ) ) ;
#34314 = CARTESIAN_POINT ( 'NONE',  ( -1.500000000000015099, 10.47916666666666607, -0.8660254037844309360 ) ) ;
#34315 = CARTESIAN_POINT ( 'NONE',  ( 3.607351389687783794, 6.366271167014519783, 1.199719254218451159 ) ) ;
#34316 = CARTESIAN_POINT ( 'NONE',  ( 2.635733503900684838, 0.8381847041133619891, -1.558674532600109686 ) ) ;
#34317 = ADVANCED_FACE ( 'NONE', ( #706 ), #102363, .T. ) ;
#34318 = CARTESIAN_POINT ( 'NONE',  ( 6.827182134110222123, -0.006956174471953178659, 2.188967759425272330 ) ) ;
#34319 = CARTESIAN_POINT ( 'NONE',  ( 0.6823417656249969321, 14.83854166700806410, -1.181850606188757036 ) ) ;
#34320 = ORIENTED_EDGE ( 'NONE', *, *, #49219, .F. ) ;
#34321 = VECTOR ( 'NONE', #10711, 1000.000000000000000 ) ;
#34322 = CARTESIAN_POINT ( 'NONE',  ( -4.450819567036169211, 8.414649604842665553, -0.7998128361456362523 ) ) ;
#34323 = CARTESIAN_POINT ( 'NONE',  ( 5.659779856126235131, 1.203369751103126717, 1.617807692209996207 ) ) ;
#34325 = VERTEX_POINT ( 'NONE', #35366 ) ;
#34324 = CARTESIAN_POINT ( 'NONE',  ( 4.781432078664868079, 0.1701398743050798745, -1.803555781593807250 ) ) ;
#34326 = CARTESIAN_POINT ( 'NONE',  ( 2.254581950620972997, -1.447608085528677480, 1.184820545849271767 ) ) ;
#34327 = CARTESIAN_POINT ( 'NONE',  ( 2.289971195246335078, -1.349064171463711936, -1.570471239911851669 ) ) ;
#34328 = CARTESIAN_POINT ( 'NONE',  ( -6.414416072596837104, 9.537216947121368804, -1.082531754730549967 ) ) ;
#34329 = CARTESIAN_POINT ( 'NONE',  ( 2.021601768330282045, -0.4154675118966509317, 1.866563793090275203 ) ) ;
#34330 = CARTESIAN_POINT ( 'NONE',  ( -6.287978406667054543, 6.558588919770907744, 0.3271801204444577671 ) ) ;
#34331 = CARTESIAN_POINT ( 'NONE',  ( -11.60136562008509387, 4.149718911762417584, -5.313756115068398067 ) ) ;
#34332 = DIRECTION ( 'NONE',  ( -0.000000000000000000, 1.000000000000000000, 0.000000000000000000 ) ) ;
#34333 = CARTESIAN_POINT ( 'NONE',  ( -1.364683531249997417, 3.821875000341416584, 1.214306433183764966E-14 ) ) ;
#34334 = CARTESIAN_POINT ( 'NONE',  ( 0.2285749388857594433, 1.317234250586714284, -1.386657971642536014 ) ) ;
#34335 = CARTESIAN_POINT ( 'NONE',  ( 4.909461021924240498, 7.781436054670031410, 1.082531754730549078 ) ) ;
#34336 = CARTESIAN_POINT ( 'NONE',  ( 1.486689167417578394, 1.889818972856545987, 0.5264814339432166701 ) ) ;
#34337 = CARTESIAN_POINT ( 'NONE',  ( 1.607015867998833336, -0.9165151389911481150, 1.199999999999999734 ) ) ;
#34338 = CARTESIAN_POINT ( 'NONE',  ( -5.581116510680924847, 6.540332679663050541, -1.199719254218453823 ) ) ;
#34339 = CARTESIAN_POINT ( 'NONE',  ( 5.027636390373715791, -0.3086946445357249824, 2.097867224209007730 ) ) ;
#34340 = EDGE_CURVE ( 'NONE', #19108, #190224, #197883, .T. ) ;
#34342 = CARTESIAN_POINT ( 'NONE',  ( -10.71030397718323890, 6.055815897892919075, -4.668189396100475008 ) ) ;
#34341 = CARTESIAN_POINT ( 'NONE',  ( 8.238550898598388628, 12.76339314834017102, 0.7998128361456462443 ) ) ;
#34343 = CARTESIAN_POINT ( 'NONE',  ( 0.4209003391736841349, -0.09842406703440903515, 1.868101828653282226 ) ) ;
#34344 = CARTESIAN_POINT ( 'NONE',  ( -0.6823417656250003738, 2.717708333674753618, -1.181850606188749264 ) ) ;
#34345 = CARTESIAN_POINT ( 'NONE',  ( 1.916272853804147136, -2.012662139290276819, 0.05368196500972129831 ) ) ;
#34347 = CARTESIAN_POINT ( 'NONE',  ( 0.7380959315415897004, 2.114583753240849795, -0.1084930780173159887 ) ) ;
#34346 = CARTESIAN_POINT ( 'NONE',  ( -6.073689629242158716, 9.069426419882418600, -1.082531754730538864 ) ) ;
#34348 = CARTESIAN_POINT ( 'NONE',  ( 9.469529551615751828, 11.05767297274606342, 7.376832519613734540 ) ) ;
#34349 = CARTESIAN_POINT ( 'NONE',  ( 2.418496320782090869, 0.8830982243829659240, 1.872697815963566992 ) ) ;
#34350 = CARTESIAN_POINT ( 'NONE',  ( 4.553559489343365740, 6.405848385690952718, -1.599625672291269396 ) ) ;
#34351 = CARTESIAN_POINT ( 'NONE',  ( 4.817943484809818600, 6.714296380401858499, 1.599625672291269396 ) ) ;
#34352 = ORIENTED_EDGE ( 'NONE', *, *, #102667, .T. ) ;
#34354 = CARTESIAN_POINT ( 'NONE',  ( 3.018661757337009810, 6.673522483535157868, 0.000000000000000000 ) ) ;
#34353 = CARTESIAN_POINT ( 'NONE',  ( 5.841762345275034463, 2.088193589346263312, 0.1035180442379990684 ) ) ;
#34357 = ORIENTED_EDGE ( 'NONE', *, *, #41033, .F. ) ;
#34356 = CARTESIAN_POINT ( 'NONE',  ( 2.894932696777189118, -0.1353093493836102779, -1.806485987321084341 ) ) ;
#34355 = CARTESIAN_POINT ( 'NONE',  ( 4.647361241834577328, -1.411646026218037253, -1.157555111390089264 ) ) ;
#34358 = CARTESIAN_POINT ( 'NONE',  ( 9.752392566931574081, 10.27221283770866300, -0.7998128361456281477 ) ) ;
#34359 = CARTESIAN_POINT ( 'NONE',  ( -2.889872605471121236, 6.605953636083950364, 2.420000000000000373 ) ) ;
#34360 = CARTESIAN_POINT ( 'NONE',  ( 10.28154365687120908, 8.975950743582902902, -4.140073266697262611 ) ) ;
#34361 = CARTESIAN_POINT ( 'NONE',  ( 5.702238492974306183, -2.206952906645575307, -0.005361432510411765114 ) ) ;
#34362 = CARTESIAN_POINT ( 'NONE',  ( 1.364683531250000748, 11.06770833367473372, -0.7879004041258355073 ) ) ;
#34363 = ORIENTED_EDGE ( 'NONE', *, *, #74644, .F. ) ;
#34364 = CARTESIAN_POINT ( 'NONE',  ( 3.861887077619485797, 0.6414691495152945455, -1.801623935260010079 ) ) ;
#34365 = CARTESIAN_POINT ( 'NONE',  ( -3.164938793786285842, 5.779846795137578930, -1.199719254218452935 ) ) ;
#34366 = CARTESIAN_POINT ( 'NONE',  ( 6.096362627639171805, 10.26417349888772179, -0.7998128361456291469 ) ) ;
#34367 = CARTESIAN_POINT ( 'NONE',  ( 1.360316468749987573, 1.817708333674738608, -0.7853790794158981292 ) ) ;
#34368 = CARTESIAN_POINT ( 'NONE',  ( 5.490689023410166847, 5.508151403507724808, -0.7216878364870207285 ) ) ;
#34369 = CARTESIAN_POINT ( 'NONE',  ( 4.495411241332118557, 8.048790631822491548, -2.444653990452267944 ) ) ;
#34370 = CARTESIAN_POINT ( 'NONE',  ( 8.200258344473377647, 14.21219199450433202, -8.700760588951361285 ) ) ;
#34371 = CARTESIAN_POINT ( 'NONE',  ( 0.09881949811249221560, -0.4921898920670075839, 1.774194203830472993 ) ) ;
#34372 = EDGE_LOOP ( 'NONE', ( #209373, #178150, #31079 ) ) ;
#34373 = ADVANCED_FACE ( 'NONE', ( #2846 ), #56819, .T. ) ;
#34374 = CARTESIAN_POINT ( 'NONE',  ( 3.796049943699483453, -1.868292110373217740, -0.09463876624429126694 ) ) ;
#34375 = CARTESIAN_POINT ( 'NONE',  ( 6.210516883511641772, 9.403297576475722508, 1.199719254218452047 ) ) ;
#34376 = CARTESIAN_POINT ( 'NONE',  ( 0.01291932979524827718, 14.54879296676368128, 11.96434918891997157 ) ) ;
#34377 = CARTESIAN_POINT ( 'NONE',  ( -6.046573322014817897, 9.998159942418544333, 0.7216878364870458196 ) ) ;
#34378 = CARTESIAN_POINT ( 'NONE',  ( 3.499976210622149253, 7.235056012367825140, 0.7998128361456321445 ) ) ;
#34379 = CARTESIAN_POINT ( 'NONE',  ( 6.491088764554701740, 0.1969099459505334604, 2.060843999385448821 ) ) ;
#34380 = CARTESIAN_POINT ( 'NONE',  ( 2.161732667986946410, 1.242745142284812365, 1.587824664567152766 ) ) ;
#34381 = CARTESIAN_POINT ( 'NONE',  ( -8.320953590485107298, 10.73086516036454618, 1.599625672291269396 ) ) ;
#34382 = CARTESIAN_POINT ( 'NONE',  ( 5.318541398310776103, 9.426991741329731056, -0.7998128361456481317 ) ) ;
#34383 = CARTESIAN_POINT ( 'NONE',  ( -0.5000000000000247580, 3.172938907704287104, 0.3999999999999698241 ) ) ;
#34384 = CARTESIAN_POINT ( 'NONE',  ( 2.361504994916805877, 2.148894721571582789, -0.4289216190115978100 ) ) ;
#34385 = CARTESIAN_POINT ( 'NONE',  ( 6.481070005604858686, -0.09514881109910081070, -1.823337098959529001 ) ) ;
#34386 = CARTESIAN_POINT ( 'NONE',  ( -4.959585264500673496, 4.680604318205876524, 1.214306433183764966E-14 ) ) ;
#34387 = CARTESIAN_POINT ( 'NONE',  ( 1.292128843000387883, 8.373613470998947150, 10.90074592850030122 ) ) ;
#34388 = CARTESIAN_POINT ( 'NONE',  ( 5.899206235721897507, 6.055031161196562373, 0.000000000000000000 ) ) ;
#34389 = CARTESIAN_POINT ( 'NONE',  ( 9.121938423896107651, 9.536683004167278099, -0.7998128361456221525 ) ) ;
#34390 = EDGE_CURVE ( 'NONE', #11745, #81936, #27223, .T. ) ;
#34391 = CARTESIAN_POINT ( 'NONE',  ( 2.381428537494710618, 5.930083727052461562, 0.7998128361456462443 ) ) ;
#34392 = CARTESIAN_POINT ( 'NONE',  ( 4.895902868310594513, 8.725987423088758632, 0.000000000000000000 ) ) ;
#34393 = VERTEX_POINT ( 'NONE', #170708 ) ;
#34395 = CARTESIAN_POINT ( 'NONE',  ( 0.6627443117090633384, 0.5862905632768620201, 1.925809981296212170 ) ) ;
#34394 = CARTESIAN_POINT ( 'NONE',  ( 4.001369526190221571, -1.836035423186295201, 0.1395379388276704880 ) ) ;
#34396 = CARTESIAN_POINT ( 'NONE',  ( 2.671599042396528123, -0.8780164823973014565, -2.124237947079451683 ) ) ;
#34398 = CARTESIAN_POINT ( 'NONE',  ( 1.006444858994318681, 0.5332790290331288485, 1.782932314864177137 ) ) ;
#34397 = CARTESIAN_POINT ( 'NONE',  ( 3.307826292054301121, 4.882216645528547616, -1.443375672974057666 ) ) ;
#34399 = CARTESIAN_POINT ( 'NONE',  ( 2.520459450608881991, -4.091624429771669291, -2.338646429533238535 ) ) ;
#34400 = CARTESIAN_POINT ( 'NONE',  ( -5.579343907223557331, 6.467988298970945849, 1.199719254218450271 ) ) ;
#34401 = FACE_OUTER_BOUND ( 'NONE', #31712, .T. ) ;
#34402 = CARTESIAN_POINT ( 'NONE',  ( 4.728717205193702533, 1.314622909153417174, -1.389140896021365368 ) ) ;
#34403 = CARTESIAN_POINT ( 'NONE',  ( -6.970863535720637216, 11.28442455831609337, 0.7998128361456481317 ) ) ;
#34404 = CARTESIAN_POINT ( 'NONE',  ( 6.297309100973213170, 6.875137029808006339, 0.7249047842670247599 ) ) ;
#34405 = CARTESIAN_POINT ( 'NONE',  ( -6.943184063974186415, 7.273005294157565359, -0.7216878364870338292 ) ) ;
#34407 = CARTESIAN_POINT ( 'NONE',  ( 2.043623373375623942, 0.7184291972081280342, -1.727395513401897453 ) ) ;
#34406 = CARTESIAN_POINT ( 'NONE',  ( 3.931257944464498166, -1.443263031577642463, -1.512909484191153897 ) ) ;
#34408 = CARTESIAN_POINT ( 'NONE',  ( 7.510853912290742507, 8.825379654836435606, -1.082531754730537976 ) ) ;
#34409 = CARTESIAN_POINT ( 'NONE',  ( -1.201851678989727383E-14, 5.009375000341421469, -1.575800808251660134 ) ) ;
#34410 = CARTESIAN_POINT ( 'NONE',  ( 6.198766299729112639, 1.534709720371667308, 1.016988835930050739 ) ) ;
#34411 = AXIS2_PLACEMENT_3D ( 'NONE', #199703, #200761, #52411 ) ;
#34412 = CARTESIAN_POINT ( 'NONE',  ( 4.383363735919856730, 4.008345868194933104, -0.7998128361456211532 ) ) ;
#34414 = CARTESIAN_POINT ( 'NONE',  ( 3.506755287428983792, 7.242964935309132990, 1.040834085586084257E-14 ) ) ;
#34413 = CARTESIAN_POINT ( 'NONE',  ( 0.6125000000000001554, 1.166666666666656083, -1.060881119635941339 ) ) ;
#34415 = CARTESIAN_POINT ( 'NONE',  ( 3.738627921261325149, 0.2550716744767547728, 1.705777993037333129 ) ) ;
#34416 = CARTESIAN_POINT ( 'NONE',  ( -6.418895661066105873, 9.576129806964074120, -1.199719254218440723 ) ) ;
#34417 = CARTESIAN_POINT ( 'NONE',  ( 6.604147088760183415, -2.206502607372296421, 0.04933187264975073122 ) ) ;
#34418 = DIRECTION ( 'NONE',  ( 0.000000000000000000, 0.000000000000000000, -1.000000000000000000 ) ) ;
#34419 = CARTESIAN_POINT ( 'NONE',  ( -1.225000000000044276, 0.7916666673494797690, -0.7072540797572998139 ) ) ;
#34420 = CARTESIAN_POINT ( 'NONE',  ( 5.225502712144541206, 0.2199120275673121516, -2.159938666613583802 ) ) ;
#34421 = CARTESIAN_POINT ( 'NONE',  ( 3.176193443437186126, -1.086901434622984830, 1.466744820640853098 ) ) ;
#34422 = CARTESIAN_POINT ( 'NONE',  ( 1.340592890135338555, -1.912720961655197893, -0.4351338972534216087 ) ) ;
#34423 = CARTESIAN_POINT ( 'NONE',  ( 5.964083501069187498, -1.130735325014235793, 1.789944102876602328 ) ) ;
#34424 = ORIENTED_EDGE ( 'NONE', *, *, #59430, .F. ) ;
#34426 = CARTESIAN_POINT ( 'NONE',  ( -1.364683531249997417, 3.321875000341423245, 1.214306433183764966E-14 ) ) ;
#34425 = CARTESIAN_POINT ( 'NONE',  ( 5.478174288590652807, -2.235914823156583964, -0.5050262530511948622 ) ) ;
#34427 = CARTESIAN_POINT ( 'NONE',  ( 9.589694723567584234, 10.08239868711733855, -0.7998128361456281477 ) ) ;
#34428 = CARTESIAN_POINT ( 'NONE',  ( 1.418772191123615078, -0.7664089246972278779, -1.977313068770427229 ) ) ;
#34429 = CARTESIAN_POINT ( 'NONE',  ( -3.958617665510266725, 7.562211676496538360, -0.7216878364870267237 ) ) ;
#34430 = VECTOR ( 'NONE', #188585, 1000.000000000000000 ) ;
#34431 = FACE_OUTER_BOUND ( 'NONE', #41439, .T. ) ;
#34432 = CARTESIAN_POINT ( 'NONE',  ( -5.246642258364192735, 5.223430177620739023, 0.7216878364870317197 ) ) ;
#34433 = CARTESIAN_POINT ( 'NONE',  ( 6.297752264732417338, -1.566808387090750765, -1.503110733841714675 ) ) ;
#34435 = CARTESIAN_POINT ( 'NONE',  ( 1.499999999999997113, 13.17708333401613174, -0.8660254037844378194 ) ) ;
#34434 = CARTESIAN_POINT ( 'NONE',  ( 6.883263157960357148, 2.018753856957363535, 2.456789959645651500 ) ) ;
#34437 = ORIENTED_EDGE ( 'NONE', *, *, #150934, .F. ) ;
#34436 = CARTESIAN_POINT ( 'NONE',  ( 1.331071098547026654, 1.488246241617418697, -1.649206797639357180 ) ) ;
#34438 = CARTESIAN_POINT ( 'NONE',  ( 5.994767569012836361, -2.000857541758268354, 0.2496038112331094849 ) ) ;
#34440 = CARTESIAN_POINT ( 'NONE',  ( 4.364169495198770399, -2.057374995403418172, 0.1468088122822813202 ) ) ;
#34439 = CARTESIAN_POINT ( 'NONE',  ( 2.984766373302843778, 6.633977868828633717, -0.7998128361456291469 ) ) ;
#34441 = CARTESIAN_POINT ( 'NONE',  ( 5.155843554946782703, 9.237177590738404831, -0.7998128361456481317 ) ) ;
#34442 = CARTESIAN_POINT ( 'NONE',  ( 5.352436782344940802, 9.466536356036257871, 0.000000000000000000 ) ) ;
#34443 = CARTESIAN_POINT ( 'NONE',  ( 0.000000000000000000, -3.434374999522041616, -3.793834371823813001 ) ) ;
#34444 = CARTESIAN_POINT ( 'NONE',  ( 1.230728480726492879, 2.976239941806479550, 0.7750000000000100142 ) ) ;
#34445 = CARTESIAN_POINT ( 'NONE',  ( -0.01160896700787457207, -0.4585933848370716270, -2.046879979534850236 ) ) ;
#34446 = CARTESIAN_POINT ( 'NONE',  ( 5.133435478496918947, 0.5880181904946503169, 1.928752423557971829 ) ) ;
#34447 = CARTESIAN_POINT ( 'NONE',  ( 4.106863108761789505, -0.3106082297497716471, 1.814695527881895476 ) ) ;
#34448 = EDGE_CURVE ( 'NONE', #48080, #83910, #107231, .T. ) ;
#34450 = ORIENTED_EDGE ( 'NONE', *, *, #80889, .T. ) ;
#34449 = CARTESIAN_POINT ( 'NONE',  ( 4.059776932288224671, 6.823824623389866950, 1.199719254218462483 ) ) ;
#34451 = PRESENTATION_STYLE_ASSIGNMENT (( #67989 ) ) ;
#34452 = CARTESIAN_POINT ( 'NONE',  ( 2.291662735322400835, -0.7404417586454847822, 1.557896076775511451 ) ) ;
#34453 = CARTESIAN_POINT ( 'NONE',  ( 7.720982897393566802, -6.134628647623485698, -7.834948825496929281 ) ) ;
#34454 = CARTESIAN_POINT ( 'NONE',  ( 2.409158461118418693, -1.326566255432750197, -1.877132621748223373 ) ) ;
#34455 = CARTESIAN_POINT ( 'NONE',  ( -6.521635583373313061, 7.567328587812373719, -1.199719254218446718 ) ) ;
#34456 = CARTESIAN_POINT ( 'NONE',  ( 0.9489188801723142941, 0.6573868573102136237, 2.164820675142268058 ) ) ;
#34457 = CARTESIAN_POINT ( 'NONE',  ( 2.526118869349633034, -1.213293402057673775, -1.721263080769465992 ) ) ;
#34458 = CARTESIAN_POINT ( 'NONE',  ( -3.949167883330528372, 7.829389307186077396, 1.214306433183764966E-14 ) ) ;
#34459 = TRIMMED_CURVE ( 'NONE', #166111, ( PARAMETER_VALUE ( 2.245927859731927878 ), #113145 ), ( PARAMETER_VALUE ( 3.141592653589793116 ), #179151 ), .T., .PARAMETER. ) ;
#34460 = CARTESIAN_POINT ( 'NONE',  ( 6.419949431270806528, 7.448694743692793274, 1.199719254218462483 ) ) ;
#34461 = CARTESIAN_POINT ( 'NONE',  ( 4.041739190205284160, 7.729463131965888856, 0.000000000000000000 ) ) ;
#34462 = CARTESIAN_POINT ( 'NONE',  ( 6.750000000000005329, 3.748112931134527976E-13, 1.999999999999984901 ) ) ;
#34463 = CARTESIAN_POINT ( 'NONE',  ( -4.574986769607567894, 7.424902766929059261, 1.199719254218464037 ) ) ;
#34464 = UNCERTAINTY_MEASURE_WITH_UNIT (LENGTH_MEASURE( 1.000000000000000082E-05 ), #22875, 'distance_accuracy_value', 'NONE');
#34465 = CARTESIAN_POINT ( 'NONE',  ( -1.499999999999997780, 1.650000000000019451, 0.000000000000000000 ) ) ;
#34466 = CARTESIAN_POINT ( 'NONE',  ( -3.110706179331648169, 5.716575411607132118, 1.199719254218462483 ) ) ;
#34467 = CARTESIAN_POINT ( 'NONE',  ( 4.553117645631366450, 0.3812515705259692522, 2.188315991368384505 ) ) ;
#34468 = CARTESIAN_POINT ( 'NONE',  ( 3.802820697025221630, 1.879323313303274734, 1.126966401794778250 ) ) ;
#34469 = CARTESIAN_POINT ( 'NONE',  ( -5.708146366553361162, 6.618257834855742594, -1.199719254218446718 ) ) ;
#34470 = CARTESIAN_POINT ( 'NONE',  ( -11.95359438121989548, 9.995781002913005864, 1.059536798430472437 ) ) ;
#34471 = CARTESIAN_POINT ( 'NONE',  ( 1.364683531249988535, 2.863541667008082658, 0.7879004041258500513 ) ) ;
#34472 = CARTESIAN_POINT ( 'NONE',  ( 6.610000000000009202, 1.996100381701769289, 2.581056663040970811 ) ) ;
#34473 = CARTESIAN_POINT ( 'NONE',  ( -5.314433026876900001, 6.262888621853549331, 1.082531754730548412 ) ) ;
#34474 = CARTESIAN_POINT ( 'NONE',  ( 5.185831674374465905, 2.043064739972153543, -0.5678235988075125418 ) ) ;
#34475 = CARTESIAN_POINT ( 'NONE',  ( -5.628043163448566588, 9.580151100749725757, 0.000000000000000000 ) ) ;
#34476 = EDGE_LOOP ( 'NONE', ( #163636, #29606, #89777, #64062 ) ) ;
#34478 = CARTESIAN_POINT ( 'NONE',  ( 0.000000000000000000, -8.233137084989836652, 0.000000000000000000 ) ) ;
#34477 = CARTESIAN_POINT ( 'NONE',  ( -6.292392690518223475, 6.513748691792265788, -0.7216878364870338292 ) ) ;
#34479 = CARTESIAN_POINT ( 'NONE',  ( 3.994848817520957773, 7.812407387083109001, 1.040834085586084257E-14 ) ) ;
#34480 = CARTESIAN_POINT ( 'NONE',  ( 5.794452930745782382, 1.501506822132542718, -1.065412412061928160 ) ) ;
#34481 = CARTESIAN_POINT ( 'NONE',  ( 0.6823417656249899377, 2.155208333674753174, 1.181850606188767472 ) ) ;
#34482 = CARTESIAN_POINT ( 'NONE',  ( 0.6436349260668382533, 0.5032331446216579129, 1.666064694988089512 ) ) ;
#34483 = CARTESIAN_POINT ( 'NONE',  ( 4.142179624174931796, 4.791296635414242111, 1.199719254218464037 ) ) ;
#34484 = CARTESIAN_POINT ( 'NONE',  ( -9.498884434226665618, -9.954196546781716393, 0.1657939142878951944 ) ) ;
#34485 = CARTESIAN_POINT ( 'NONE',  ( 0.6823417656249882723, 0.4885416670080827695, -1.181850606188749264 ) ) ;
#34486 = CARTESIAN_POINT ( 'NONE',  ( -0.6124999999999967137, 1.708333333333339477, -1.060881119635938008 ) ) ;
#34487 = CARTESIAN_POINT ( 'NONE',  ( 4.944278945467968533, 2.155654431248493985, 0.1625706239713892443 ) ) ;
#34488 = CARTESIAN_POINT ( 'NONE',  ( -2.774614992291035698, 6.388801257648172971, 1.040834085586084257E-14 ) ) ;
#34489 = CARTESIAN_POINT ( 'NONE',  ( -5.843201017365469596, 9.760892253660966134, 0.7216878364870458196 ) ) ;
#34490 = CARTESIAN_POINT ( 'NONE',  ( 5.137646372127643524, -1.526005641499485810, -1.531359247741073570 ) ) ;
#34491 = ORIENTED_EDGE ( 'NONE', *, *, #128141, .T. ) ;
#34492 = CARTESIAN_POINT ( 'NONE',  ( 0.6823417656249899377, 2.592708333674753618, 1.181850606188767472 ) ) ;
#34493 = CARTESIAN_POINT ( 'NONE',  ( 6.028588005634209601, 1.899229357904350879, 0.5280594692760686160 ) ) ;
#34494 = CARTESIAN_POINT ( 'NONE',  ( 5.009033543107539899, 1.729337909971711662, 0.1259922892337256017 ) ) ;
#34496 = CARTESIAN_POINT ( 'NONE',  ( 2.156058135970494227, 0.9403143569667195001, 1.979733194660021622 ) ) ;
#34495 = CARTESIAN_POINT ( 'NONE',  ( -0.6801582343750161019, -0.9010416663252431846, -1.178068619123869398 ) ) ;
#34497 = CARTESIAN_POINT ( 'NONE',  ( 2.380262917520099553, 1.419673959206497527, 1.819133949716137844 ) ) ;
#34498 = CARTESIAN_POINT ( 'NONE',  ( 5.167286647625595641, 0.2060095241231186813, -2.050478191761321956 ) ) ;
#34499 = CARTESIAN_POINT ( 'NONE',  ( 0.1990292396216531146, -0.5187523925454742280, 1.871322268447791703 ) ) ;
#34501 = EDGE_CURVE ( 'NONE', #34978, #165933, #47990, .T. ) ;
#34500 = CARTESIAN_POINT ( 'NONE',  ( -7.009202228140755331, 8.240119356661432803, -1.082531754730543083 ) ) ;
#34502 = CARTESIAN_POINT ( 'NONE',  ( -3.305155586681401303, 7.078041627762083898, 0.7998128361456352531 ) ) ;
#34503 = DIRECTION ( 'NONE',  ( 0.000000000000000000, 0.000000000000000000, -1.000000000000000000 ) ) ;
#34504 = CARTESIAN_POINT ( 'NONE',  ( 3.392942708002244068, -2.044739723715986113, -0.5619712599038150236 ) ) ;
#34505 = CARTESIAN_POINT ( 'NONE',  ( 1.734723475976807094E-15, 0.7598076211376200151, -10.89999999999920632 ) ) ;
#34506 = CARTESIAN_POINT ( 'NONE',  ( 1.371720446232262081, -0.2986288616722633793, -1.994071132515719658 ) ) ;
#34507 = CARTESIAN_POINT ( 'NONE',  ( -7.171900071504748730, 8.429933507252760805, -1.082531754730549078 ) ) ;
#34508 = CARTESIAN_POINT ( 'NONE',  ( 4.260898339918250066, -1.637375743694971408, 1.479669880875638999 ) ) ;
#34509 = CARTESIAN_POINT ( 'NONE',  ( -3.285556943749998737, -2.967708332855377051, 1.896917185911908499 ) ) ;
#34510 = CARTESIAN_POINT ( 'NONE',  ( 1.586513592238134374, 1.791619466816740003, 0.5028711289422735931 ) ) ;
#34511 = CARTESIAN_POINT ( 'NONE',  ( -0.1290005225502918740, 6.946858002156244716, -2.769053915224591211 ) ) ;
#34512 = DIRECTION ( 'NONE',  ( -0.000000000000000000, 1.000000000000000000, -0.000000000000000000 ) ) ;
#34513 = CARTESIAN_POINT ( 'NONE',  ( 0.000000000000000000, 0.000000000000000000, -0.5000000000000004441 ) ) ;
#34515 = CARTESIAN_POINT ( 'NONE',  ( 6.825078400183551608, 4.689370880799383912, 2.706890346843467299 ) ) ;
#34514 = CARTESIAN_POINT ( 'NONE',  ( -5.847422642759834588, 7.296647196851402839, -1.286413008881746256 ) ) ;
#34516 = ORIENTED_EDGE ( 'NONE', *, *, #106606, .F. ) ;
#34517 = CARTESIAN_POINT ( 'NONE',  ( 3.098563410164618226, -0.5969507786072983935, -1.972546241584592241 ) ) ;
#34518 = CARTESIAN_POINT ( 'NONE',  ( -0.6801582343750282034, 1.432291667008027458, 1.178068619123810334 ) ) ;
#34519 = EDGE_CURVE ( 'NONE', #45181, #40348, #116353, .T. ) ;
#34520 = CARTESIAN_POINT ( 'NONE',  ( -4.882907879216086933, 8.848476292394087395, -0.7998128361456281477 ) ) ;
#34521 = CARTESIAN_POINT ( 'NONE',  ( 2.315108654539797861, 1.620709295712051246, -1.204917113890991320 ) ) ;
#34522 = CARTESIAN_POINT ( 'NONE',  ( 0.7499999999999867883, -0.6833333333333135862, -1.299038105676652899 ) ) ;
#34523 = CARTESIAN_POINT ( 'NONE',  ( 4.546061579283848353, 4.198160018786257552, -0.7998128361456211532 ) ) ;
#34524 = CARTESIAN_POINT ( 'NONE',  ( 1.973578683463860672, 1.972434364383905292, -0.5973212362519930707 ) ) ;
#34526 = CARTESIAN_POINT ( 'NONE',  ( -1.364683531250014514, 12.83854166700806232, -0.7879004041258335089 ) ) ;
#34525 = CARTESIAN_POINT ( 'NONE',  ( -9.406910906341037659, 15.38274361496693210, -7.349368793364722485 ) ) ;
#34527 = CARTESIAN_POINT ( 'NONE',  ( 5.575427483717746213, 7.527751369135936343, 1.599625672291267398 ) ) ;
#34528 =( GEOMETRIC_REPRESENTATION_CONTEXT ( 3 ) GLOBAL_UNCERTAINTY_ASSIGNED_CONTEXT ( ( #105395 ) ) GLOBAL_UNIT_ASSIGNED_CONTEXT ( ( #20061, #181509, #82943 ) ) REPRESENTATION_CONTEXT ( 'NONE', 'WORKASPACE' ) );
#34529 = CARTESIAN_POINT ( 'NONE',  ( -0.1409997244346088419, 5.722143553014046979, -2.594341442600463843 ) ) ;
#34530 = CARTESIAN_POINT ( 'NONE',  ( 1.025062291269123405, -1.166378923895025510, -1.424538887614942739 ) ) ;
#34531 = CARTESIAN_POINT ( 'NONE',  ( 5.901041445831936016, 1.806360628843254768, -1.267562117129708232 ) ) ;
#34532 = CARTESIAN_POINT ( 'NONE',  ( 6.008198349511364000, 7.038594824965278995, 1.199719254218453823 ) ) ;
#34533 = CARTESIAN_POINT ( 'NONE',  ( 1.405796033167512116, -0.5266655099175953092, 2.096309153942426562 ) ) ;
#34534 = CARTESIAN_POINT ( 'NONE',  ( -4.948362879307902418, 4.875437568721725512, 1.214306433183764966E-14 ) ) ;
#34535 = CARTESIAN_POINT ( 'NONE',  ( 2.096888995370162156, 1.803417055948232761, 0.9023429676050932491 ) ) ;
#34536 = CARTESIAN_POINT ( 'NONE',  ( -1.138412281109779656E-15, -6.465328379374292389, -10.58872653680446696 ) ) ;
#34537 = CARTESIAN_POINT ( 'NONE',  ( -0.4612990374432109908, 6.901512110099052855, 3.726810127985829446 ) ) ;
#34538 = CARTESIAN_POINT ( 'NONE',  ( 3.176271558300056697, 6.436868453234527720, -0.7638679071477995075 ) ) ;
#34539 = EDGE_CURVE ( 'NONE', #158833, #65494, #24438, .T. ) ;
#34540 = CARTESIAN_POINT ( 'NONE',  ( 4.416843060293515144, 1.802029179758830812, 0.8000101564944164245 ) ) ;
#34541 = CARTESIAN_POINT ( 'NONE',  ( 3.608611488583326032, 1.916353073142588403, 0.6279913346786819561 ) ) ;
#34543 = CARTESIAN_POINT ( 'NONE',  ( 9.042925270190625753, 11.57316545335434199, 1.443375672974076540 ) ) ;
#34542 = CARTESIAN_POINT ( 'NONE',  ( -1.364683531249997417, 2.509375000341422357, 1.214306433183764966E-14 ) ) ;
#34545 = CARTESIAN_POINT ( 'NONE',  ( -0.01666059994226073634, -0.1612322585618740090, -2.171656592459796808 ) ) ;
#34544 = CARTESIAN_POINT ( 'NONE',  ( -6.527360889975461156, 9.702672574024962415, 1.199719254218452047 ) ) ;
#34546 = CARTESIAN_POINT ( 'NONE',  ( 5.758279222819879806, -2.070544812512797428, -0.003756845764937844813 ) ) ;
#34547 = CARTESIAN_POINT ( 'NONE',  ( 5.472687561410540802, 9.536552588287639409, 0.7998128361456462443 ) ) ;
#34548 = CARTESIAN_POINT ( 'NONE',  ( -6.744291347794091784, 9.955758108146730123, -1.199719254218440723 ) ) ;
#34549 = CARTESIAN_POINT ( 'NONE',  ( 6.539320575229258914, 2.958022083381315337, 2.556018433155104574 ) ) ;
#34550 = CARTESIAN_POINT ( 'NONE',  ( 5.396742217995451618, -1.971451684502657287, -0.4385051361721309937 ) ) ;
#34551 = CARTESIAN_POINT ( 'NONE',  ( 0.7499999999999867883, -0.9020833326505162120, -1.299038105676652011 ) ) ;
#34552 = CARTESIAN_POINT ( 'NONE',  ( 1.217717225187223473, 0.4062273103370617755, -2.022011198395957887 ) ) ;
#34553 = CARTESIAN_POINT ( 'NONE',  ( 7.280365300858406385, 11.43758391773608984, 1.040834085586084257E-14 ) ) ;
#34554 = CARTESIAN_POINT ( 'NONE',  ( 5.332099551924443404, 9.442809587212341427, 0.000000000000000000 ) ) ;
#34555 = CARTESIAN_POINT ( 'NONE',  ( 6.412080304620304538, 6.445458208337293549, -0.7998128361456481317 ) ) ;
#34556 = CARTESIAN_POINT ( 'NONE',  ( 0.6823417656249882723, 1.238541667008083547, -1.181850606188749264 ) ) ;
#34558 = CARTESIAN_POINT ( 'NONE',  ( -4.787437654953777155, 6.678706214094487947, -1.250000000000001110 ) ) ;
#34557 = CARTESIAN_POINT ( 'NONE',  ( 6.066347387471824781, 6.042103138330730872, -0.7998128361456481317 ) ) ;
#34559 = CARTESIAN_POINT ( 'NONE',  ( 6.602457619730760285, 8.725953194484466380, 1.443375672974076540 ) ) ;
#34561 = SURFACE_STYLE_FILL_AREA ( #54023 ) ;
#34560 = CARTESIAN_POINT ( 'NONE',  ( 2.893231026729268685, 0.2635377995367886861, 2.155045766152231757 ) ) ;
#34563 = CARTESIAN_POINT ( 'NONE',  ( 2.946635061770470632, -1.506786691049965432, -1.057933238436038925 ) ) ;
#34562 = CARTESIAN_POINT ( 'NONE',  ( -3.958617665510266725, 7.562211676496538360, -0.7216878364870267237 ) ) ;
#34564 = CARTESIAN_POINT ( 'NONE',  ( -1.201851678989727383E-14, 4.696875000341419693, -1.575800808251660134 ) ) ;
#34565 = CARTESIAN_POINT ( 'NONE',  ( 4.775033345069852331, 2.044829088842615494, -0.7888500489584143738 ) ) ;
#34566 = CARTESIAN_POINT ( 'NONE',  ( 7.128288838256305660, 14.48195940547645044, 9.656477080921417766 ) ) ;
#34567 = CARTESIAN_POINT ( 'NONE',  ( 4.874029165478985348, 1.298689969358796770, 1.852503425883561095 ) ) ;
#34568 = CARTESIAN_POINT ( 'NONE',  ( -5.766295404513795297, 5.621766148221195358, 0.7998128361456341429 ) ) ;
#34569 = CARTESIAN_POINT ( 'NONE',  ( 11.33772463945037146, 19.00000000000000000, 3.679999999999999272 ) ) ;
#34570 = CARTESIAN_POINT ( 'NONE',  ( 4.771426152247889796, 8.279957873513081879, -0.8122977234717634332 ) ) ;
#34571 = CARTESIAN_POINT ( 'NONE',  ( -6.441532379824190357, 6.687744995982559892, 0.7216878364870257245 ) ) ;
#34572 = CARTESIAN_POINT ( 'NONE',  ( 4.584065335196260804, 6.441438539186039591, 1.443375672974065660 ) ) ;
#34573 = CARTESIAN_POINT ( 'NONE',  ( 0.1096998152198442600, -0.7512755041745984297, -1.601369504124000587 ) ) ;
#34574 = CARTESIAN_POINT ( 'NONE',  ( 3.756497301808682465, 2.003587623774540472, 0.1952383342433745284 ) ) ;
#34575 = CARTESIAN_POINT ( 'NONE',  ( 5.608269097547198712, 9.694731047113750222, -0.7998128361456281477 ) ) ;
#34576 = CARTESIAN_POINT ( 'NONE',  ( 3.047987177024631844, 0.7594498649067694673, -1.964434322149722245 ) ) ;
#34577 = CARTESIAN_POINT ( 'NONE',  ( 1.405720392582618938, -1.065544983005232371, -1.591680324291492310 ) ) ;
#34579 = CARTESIAN_POINT ( 'NONE',  ( 0.7499999999999902300, 2.983333333333351600, 1.299038105676669330 ) ) ;
#34578 = CARTESIAN_POINT ( 'NONE',  ( 1.364683531250000303, 11.75520833367473017, -0.7879004041258355073 ) ) ;
#34580 = CARTESIAN_POINT ( 'NONE',  ( 1.838274926946784182, -1.056231965017372598, 1.662188548998255078 ) ) ;
#34581 = CARTESIAN_POINT ( 'NONE',  ( 0.2329894512427649333, -1.712236961970284632, 0.7538099095961707796 ) ) ;
#34582 = CARTESIAN_POINT ( 'NONE',  ( 1.469116868872882620, 1.728625619535430369, 0.9278086228877155950 ) ) ;
#34584 = ORIENTED_EDGE ( 'NONE', *, *, #184415, .F. ) ;
#34583 = CARTESIAN_POINT ( 'NONE',  ( 6.486573133654839118, -1.106559166176981579, 1.434805384617921842 ) ) ;
#34585 = CARTESIAN_POINT ( 'NONE',  ( 5.992340707560160240, 7.053780915984068756, 1.082531754730558626 ) ) ;
#34586 = CARTESIAN_POINT ( 'NONE',  ( 1.364683531249988757, 1.196875000341421469, 0.000000000000000000 ) ) ;
#34587 = CIRCLE ( 'NONE', #86395, 4.000000000000000000 ) ;
#34588 = CARTESIAN_POINT ( 'NONE',  ( 5.576977133510579776, -0.04717937999037385977, -1.870219006134994588 ) ) ;
#34589 = CARTESIAN_POINT ( 'NONE',  ( 10.55232363013785246, 11.20546574478267132, 0.000000000000000000 ) ) ;
#34590 = DIRECTION ( 'NONE',  ( 8.659560562354940254E-17, 0.7071067811865469066, -0.7071067811865481278 ) ) ;
#34591 = VERTEX_POINT ( 'NONE', #8203 ) ;
#34592 = CARTESIAN_POINT ( 'NONE',  ( 5.014543041041934046, 0.7873211189074662553, 1.914903133430221116 ) ) ;
#34593 = DIRECTION ( 'NONE',  ( -1.000000000000000000, -0.000000000000000000, -0.000000000000000000 ) ) ;
#34594 =( BOUNDED_CURVE ( )  B_SPLINE_CURVE ( 2, ( #113648, #198012, #98396, #82130, #61626 ),
 .UNSPECIFIED., .F., .T. ) 
 B_SPLINE_CURVE_WITH_KNOTS ( ( 3, 2, 3 ),
 ( 0.1116300932268876750, 0.1125000000000000028, 0.1135379806157290616 ),
 .UNSPECIFIED. ) 
 CURVE ( )  GEOMETRIC_REPRESENTATION_ITEM ( )  RATIONAL_B_SPLINE_CURVE ( ( 0.9557375992087471239, 0.9720291019185025583, 1.000000000000000000, 0.9666248718707487475, 0.9498782570434030070 ) ) 
 REPRESENTATION_ITEM ( '' )  );
#34595 = CARTESIAN_POINT ( 'NONE',  ( -4.516274566683622815, 5.401980094953223066, 1.082531754730549078 ) ) ;
#34596 = CARTESIAN_POINT ( 'NONE',  ( 0.1861046438572169504, -1.272802160389638892, -1.633586439835111648 ) ) ;
#34597 = CARTESIAN_POINT ( 'NONE',  ( 1.499999999999987121, 1.045833333333352266, -0.8660254037844253849 ) ) ;
#34598 = CARTESIAN_POINT ( 'NONE',  ( 6.262976894508937242, 9.394224579314053969, -1.199719254218440723 ) ) ;
#34599 = CARTESIAN_POINT ( 'NONE',  ( -8.538937818508475885, 8.856515631215026829, 1.040834085586084257E-14 ) ) ;
#34600 = CARTESIAN_POINT ( 'NONE',  ( 5.155843554946782703, 9.237177590738404831, -0.7998128361456481317 ) ) ;
#34601 = CARTESIAN_POINT ( 'NONE',  ( -1.364683531250014514, 0.7385416670080887647, -0.7879004041258289570 ) ) ;
#34602 = CARTESIAN_POINT ( 'NONE',  ( -1.500000000000013101, 2.129166666666693519, -0.8660254037844313801 ) ) ;
#34604 = CARTESIAN_POINT ( 'NONE',  ( 3.161022370280501814, 6.839609865302569425, 0.000000000000000000 ) ) ;
#34603 = CARTESIAN_POINT ( 'NONE',  ( 5.705508943770692731, -1.545575431542939970, -1.208212526538715137 ) ) ;
#34605 = CARTESIAN_POINT ( 'NONE',  ( 3.673203737196802710, -0.8145011343782401214, -1.844427810980188820 ) ) ;
#34606 = CARTESIAN_POINT ( 'NONE',  ( 3.520622370129117940, 0.2863239327370070697, 1.894091974173327531 ) ) ;
#34607 = CARTESIAN_POINT ( 'NONE',  ( 11.91826848676359241, 10.09166292761251071, -1.400000051401918855 ) ) ;
#34608 = CARTESIAN_POINT ( 'NONE',  ( 0.9959476074029066650, -2.191739723303193887, 0.005169097091584087637 ) ) ;
#34609 = CARTESIAN_POINT ( 'NONE',  ( 0.2331713839410758660, 6.947498546895825022, -2.548426565200106353 ) ) ;
#34610 = CARTESIAN_POINT ( 'NONE',  ( 3.338976900156843453, -1.651226333174139693, 0.8788041501476551165 ) ) ;
#34611 = CARTESIAN_POINT ( 'NONE',  ( 1.499999999999987566, -1.193749999317185395, 0.000000000000000000 ) ) ;
#34612 = CARTESIAN_POINT ( 'NONE',  ( -8.206763054973658100, 8.468978407091068306, 0.7998128361456602331 ) ) ;
#34614 = CARTESIAN_POINT ( 'NONE',  ( 4.886377882447483501, -0.7144107685513987338, -1.993165935382594789 ) ) ;
#34613 = CARTESIAN_POINT ( 'NONE',  ( -4.365362273920257330, 6.116008624372160973, 1.443375672974064550 ) ) ;
#34615 = CARTESIAN_POINT ( 'NONE',  ( -1.123270288250342919, 3.096052654332833054, 0.7749999999993751887 ) ) ;
#34616 = CARTESIAN_POINT ( 'NONE',  ( 5.969205681473694902, 1.824102622056431811, 0.9793482939001868504 ) ) ;
#34618 = CARTESIAN_POINT ( 'NONE',  ( -4.395760127892912372, 7.709923763356872684, -0.8030953006082339751 ) ) ;
#34617 = CARTESIAN_POINT ( 'NONE',  ( 2.507466893629331395, -2.067604658949507179, 0.3094350269009105703 ) ) ;
#34620 = EDGE_LOOP ( 'NONE', ( #27788, #93409, #67636, #153809 ) ) ;
#34619 = CARTESIAN_POINT ( 'NONE',  ( 0.9907087679515521605, 1.524132375323374200, -0.8073730212512005844 ) ) ;
#34621 = B_SPLINE_CURVE_WITH_KNOTS ( 'NONE', 3,
 ( #91126, #27162, #109567, #158258, #74863, #93267, #75922, #76974, #209094, #156118, #159300, #124761, #143101, #138804, #123702, #188600, #26093, #140966, #42383, #108493, #73783, #126892, #110626, #7700, #192850, #44509, #176627, #88991, #155044, #6630, #72709, #122637, #40231, #174517, #106342, #189663, #139879, #205910, #57545, #41315, #112757, #66807, #178769, #198954, #1819, #99362, #116721, #145229, #28238, #211234, #165413, #132949, #11975, #85226, #83085, #151315, #79111, #67877, #200030, #167552, #46634, #13034, #161454, #33277, #118863, #94331, #134023, #52729, #29308, #51682, #100414, #183795, #19153, #2883, #117803, #68954, #135075, #201088, #741, #182721, #129024, #166484, #149164, #160373, #144173, #17009, #50596, #34339, #18076, #35404, #84163, #150251, #62859, #78049, #195000, #101482, #210165, #61806, #127975, #193927, #45574, #111690, #177697, #95402, #3951, #22339, #169682, #139342, #6094, #189138, #55942, #155581, #58072, #74331, #40777, #136134, #38626, #20215, #8247, #154513, #186995, #73235, #72162, #140433, #171823, #121028, #138271, #57007, #204285, #172909, #203230, #88453, #188059, #205372, #54875, #122095, #105799, #184849, #39688, #5017, #156654, #119940, #23417, #123179, #70018, #206445, #104702, #36477, #89528, #7165, #37550, #90595, #106883, #24483, #87375, #152373, #170753, #53811, #202150, #102550, #168613, #185916, #103630, #86303, #21270, #153445, #71091, #137208, #94864, #107963, #45051, #127437, #13583, #126361, #110097, #192320, #9322, #190195, #157727, #10375, #128504, #210716, #173991, #158779, #75396, #61275, #76452, #124235, #41853, #77520, #25563, #62344, #160918, #194472, #92734, #208566, #46114, #177163, #193407, #43978, #28781, #141508, #91674, #207517, #142560, #112232, #27708, #209635, #143641, #176108, #11445, #12512, #42918, #93803, #211774, #59136, #78583, #145773, #125295, #144705, #111163, #178241, #191253, #79656, #109028, #60200, #159843, #29857, #95937, #161993, #175047, #26632, #181413, #151071, #179308, #65510, #99118, #213888, #16762, #34097, #131656, #129563, #132705, #149996, #100168, #98064, #115421, #197659, #17823, #18895, #167308, #48251, #30929, #80732, #97005, #33040, #114366, #83906, #165167, #67629, #148922, #166233, #133774, #82846, #14638, #84979, #130620, #66563, #182468, #164120, #163058, #1567, #199782, #146822, #64479, #51428, #31986, #35149, #195550, #180360, #49305, #495, #198711, #117548, #147872, #50356, #116478, #63412, #183542, #15703, #101225, #196612, #212842, #47188, #113301, #81789, #154262, #139086, #205113, #155322, #56756, #122921, #55679, #120765, #119681, #184600, #136951, #86049, #36217, #187806, #121835, #2633, #134828, #170493, #118612, #89273, #39434, #6906, #185668, #87114, #72983, #106623, #4758, #202976, #70834, #102296, #68706, #168370, #103370, #188879, #186743, #88189, #22077, #54617, #104444, #105527, #135878, #38365, #90329, #200832, #171561, #19965, #5836, #40520, #152125, #71907, #52483, #172652, #3695, #21016, #153184, #138016, #204031, #24227, #23159, #69772, #201898, #53550, #37297, #169432, #192065, #75142, #208319, #141251, #127182, #7984, #11187, #28526, #193150, #190999, #59949, #76199, #110905, #111985, #45864, #207260, #57817, #173733, #189947, #126105, #58889, #10124, #128256, #93544, #144456, #44800, #12257 ),
 .UNSPECIFIED., .F., .F.,
 ( 4, 1, 1, 1, 1, 1, 1, 1, 1, 1, 1, 1, 1, 1, 1, 1, 1, 1, 1, 1, 1, 1, 1, 1, 1, 1, 1, 1, 1, 1, 1, 1, 1, 1, 1, 1, 1, 1, 1, 1, 1, 1, 1, 1, 1, 1, 1, 1, 1, 1, 1, 1, 1, 1, 1, 1, 1, 1, 1, 1, 1, 1, 1, 1, 1, 1, 1, 1, 1, 1, 1, 1, 1, 1, 1, 1, 1, 1, 1, 1, 1, 1, 1, 1, 1, 1, 1, 1, 1, 1, 1, 1, 1, 1, 1, 1, 1, 1, 1, 1, 1, 1, 1, 1, 1, 1, 1, 1, 1, 1, 1, 1, 1, 1, 1, 1, 1, 1, 1, 1, 1, 1, 1, 1, 1, 1, 1, 1, 1, 1, 1, 1, 1, 1, 1, 1, 1, 1, 1, 1, 1, 1, 1, 1, 1, 1, 1, 1, 1, 1, 1, 1, 1, 1, 1, 1, 1, 1, 1, 1, 1, 1, 1, 1, 1, 1, 1, 1, 1, 1, 1, 1, 1, 1, 1, 1, 1, 1, 1, 1, 1, 1, 1, 1, 1, 1, 1, 1, 1, 1, 1, 1, 1, 1, 1, 1, 1, 1, 1, 1, 1, 1, 1, 1, 1, 1, 1, 1, 1, 1, 1, 1, 1, 1, 1, 1, 1, 1, 1, 1, 1, 1, 1, 1, 1, 1, 1, 1, 1, 1, 1, 1, 1, 1, 1, 1, 1, 1, 1, 1, 1, 1, 1, 1, 1, 1, 1, 1, 1, 1, 1, 1, 1, 1, 1, 1, 1, 1, 1, 1, 1, 1, 1, 1, 1, 1, 1, 1, 1, 1, 1, 1, 1, 1, 1, 1, 1, 1, 1, 1, 1, 1, 1, 1, 1, 1, 1, 1, 1, 1, 1, 1, 1, 1, 1, 1, 1, 1, 1, 1, 1, 1, 1, 1, 1, 1, 1, 1, 1, 1, 1, 1, 1, 1, 1, 1, 1, 1, 1, 1, 1, 1, 1, 1, 1, 1, 1, 1, 1, 1, 1, 1, 1, 1, 1, 1, 1, 1, 1, 1, 1, 1, 1, 1, 1, 1, 1, 1, 1, 1, 1, 1, 1, 1, 1, 1, 1, 1, 1, 1, 1, 1, 1, 1, 1, 1, 1, 1, 1, 1, 1, 1, 1, 1, 1, 1, 1, 1, 1, 1, 1, 1, 1, 1, 4 ),
 ( 0.000000000000000000, 0.002599942752653872004, 0.005208763852970823248, 0.007813103504395044890, 0.01041666580238601383, 0.01302040446826325734, 0.01562503794709516405, 0.01822898659850798186, 0.02083325479626091381, 0.02343751936515397344, 0.02604147156932860516, 0.02864593660736421826, 0.03124971754428982826, 0.03385421962853985695, 0.03645805019290717514, 0.03906245553539786086, 0.04166655880408994678, 0.04427067902208449424, 0.04687506736766395427, 0.04947890482860387018, 0.05208340383233839299, 0.05468718329397467132, 0.05729165635893663372, 0.05989559287350183087, 0.06249988401580178210, 0.06510415622071820396, 0.06770810475871495704, 0.07031256650665723695, 0.07291634835701975292, 0.07552085129243907291, 0.07812468146351797538, 0.08072908640827750060, 0.08333318980393969455, 0.08593730989448074287, 0.08854169822802662737, 0.09114553558425014801, 0.09375003453682481669, 0.09635381396055957282, 0.09895828689139142542, 0.1015622234206122604, 0.1041665143989399522, 0.1067707866525781646, 0.1093747350801187734, 0.1119791968332524285, 0.1145829786367304204, 0.1171874814968899975, 0.1197913116783300008, 0.1223957164865987768, 0.1249998199429257079, 0.1276039399106482508, 0.1302083283009266290, 0.1328121656006459317, 0.1354166645410730119, 0.1380204439687620910, 0.1406249168095159707, 0.1432288533966223909, 0.1458331442541831724, 0.1484374165996726891, 0.1510413649597071029, 0.1536458267615184170, 0.1562496085608837959, 0.1588541113892728840, 0.1614579416238982879, 0.1640623463390579739, 0.1666664498991252963, 0.1692705697871219883, 0.1718749582774928841, 0.1744787955635339893, 0.1770832945353020271, 0.1796870740097127606, 0.1822915468038420750, 0.1848954834917516388, 0.1874997742717963711, 0.1901040467523684718, 0.1927079950878241021, 0.1953124569817516476, 0.1979162388197689970, 0.2005207416598733527, 0.2031245719904950509, 0.2057289766559125821, 0.2083330803627857220, 0.2109372002141371993, 0.2135415888479497148, 0.2161454261631269858, 0.2187499252097131475, 0.2213537047736018060, 0.2239581775645482220, 0.2265621143961681627, 0.2291664051419355919, 0.2317706778008114532, 0.2343746261546043874, 0.2369790881840763974, 0.2395828701034999064, 0.2421873729987945312, 0.2447912034682135918, 0.2473956081272447038, 0.2499997120239797754, 0.2526038318817556694, 0.2552082207023498306, 0.2578120580894675551, 0.2604165572543392093, 0.2630203369504529598, 0.2656248097816475973, 0.2682287467998764607, 0.2708330375545950908, 0.2734373104349877015, 0.2760412588500244513, 0.2786457210584605826, 0.2812495031020356140, 0.2838540060959860445, 0.2864578367469951536, 0.2890622414429859233, 0.2916663455726313803, 0.2942704654798921071, 0.2968748545306000852, 0.2994786920324540302, 0.3020831913590704687, 0.3046869712301484290, 0.3072914441450140810, 0.3098953813927431966, 0.3124996721996327054, 0.3151039453447485039, 0.3177078938639273376, 0.3203123562947402525, 0.3229161385052047861, 0.3255206416412691484, 0.3281244725166545528, 0.3307288772929431464, 0.3333329816985414751, 0.3359371016983396796, 0.3385414910224879836, 0.3411453286818670882, 0.3437498282136811634, 0.3463536083024566503, 0.3489580813444087548, 0.3515620188645239841, 0.3541663097667969717, 0.3567705832198370119, 0.3593745318860498972, 0.3619789945826469846, 0.3645827770027332826, 0.3671872803243637073, 0.3697911114669067967, 0.3723955163668249413, 0.3749996210914142147, 0.3776037412267966853, 0.3802081308677072724, 0.3828119687273952576, 0.3854164685078552144, 0.3880202488570567709, 0.3906247220695055478, 0.3932286599048890885, 0.3958329509457525486, 0.3984372247499146091, 0.4010411736060487398, 0.4036456366118335581, 0.4062494192842699414, 0.4088539228349143406, 0.4114577542873927851, 0.4140621593542673784, 0.4166662644408827831, 0.4192703847548917562, 0.4218747747558840855, 0.4244786128586610641, 0.4270831129312115948, 0.4296868935835649328, 0.4322913670099168826, 0.4348953052034483235, 0.4374995964261053638, 0.4401038706245853915, 0.4427078197135246862, 0.4453122830718987402, 0.4479160660394111426, 0.4505205698625146526, 0.4531244016677045128, 0.4557288069448597878, 0.4583329124365353446, 0.4609370329722101700, 0.4635414233766025904, 0.4661452617652466213, 0.4687497621733308639, 0.4713535431715604185, 0.4739580168552197104, 0.4765619554497781962, 0.4791662468974299260, 0.4817705215334236457, 0.4843744708980504132, 0.4869789346524148743, 0.4895827179577280641, 0.4921872220967347111, 0.4947910542974118808, 0.4973954598281701278, 0.4999995657679404681, 0.5026036865683194410, 0.5052080774194306345, 0.5078119161367193879, 0.5104164169237808135, 0.5130201983106112973, 0.5156246722949818784, 0.5182286113334474420, 0.5208329030492938605, 0.5234371781659985512, 0.5260411278491948783, 0.5286455920429519173, 0.5312493757287917173, 0.5338538802271461936, 0.5364577128660878991, 0.5390621186937718523, 0.5416662251246735504, 0.5442703462327953545, 0.5468747375739465566, 0.5494785766626585355, 0.5520830778721422805, 0.5546868596903002935, 0.5572913340187868325, 0.5598952735440421158, 0.5624995655712847764, 0.5651038412119004928, 0.5677077912565504647, 0.5703122559331050834, 0.5729160400421993149, 0.5755205449433484777, 0.5781243780633351648, 0.5807287842312690573, 0.5833328911963423513, 0.5859370126552478908, 0.5885414045297637786, 0.5911452440326808722, 0.5937497457080352925, 0.5963535280002507655, 0.5989580027162609843, 0.6015619427711926814, 0.6041662351530351360, 0.6067705113607667622, 0.6093744618097575172, 0.6119789270125192138, 0.6145827115875999169, 0.6171872169349945647, 0.6197910505788110092, 0.6223954571303226269, 0.6249995646726131948, 0.6276036865253464825, 0.6302080789765573954, 0.6328119189364656005, 0.6354164211211439373, 0.6380202039301521300, 0.6406246790770983024, 0.6432286197045988807, 0.6458329124842493441, 0.6484371893023079814, 0.6510411401985315427, 0.6536456059709156996, 0.6562493910547204656, 0.6588538968918166150, 0.6614577311022542538, 0.6640621380806766005, 0.6666662462432366709, 0.6692703685328477148, 0.6718747616040910975, 0.6744786020637821844, 0.6770831048012443398, 0.6796868881697873954, 0.6822913637910873463, 0.6848953050340567117, 0.6874995982547292828, 0.6901038757263339152, 0.6927078271126885234, 0.6953122934981186276, 0.6979160791333920422, 0.7005205855036529261, 0.7031244203235108570, 0.7057288277721832648, 0.7083329365980738368, 0.7109370593676189731, 0.7135414531022405971, 0.7161452941045143294, 0.7187497974382286436, 0.7213535814090563658, 0.7239580575481356917, 0.7265619994494829648, 0.7291662931543987369, 0.7317705713227778963, 0.7343745232421703406, 0.7369789902840787610, 0.7395827765135741805, 0.7421872834604720248, 0.7447911189325585601, 0.7473955268948287989, 0.7499996364271210858, 0.7526037597196653106, 0.7552081541610216053, 0.7578119957486867397, 0.7604164997221309896, 0.7630202843380037292, 0.7656247610382975743, 0.7682287036409420899, 0.7708329978733315935, 0.7734372767817252470, 0.7760412292770711984, 0.7786456970189011839, 0.7812494838853828449, 0.7838539914523996455, 0.7864578276195345330, 0.7890622361387605865, 0.7916663464205372369, 0.7942704702791556493, 0.7968748654706151457, 0.7994787076864910969, 0.8020832123431549388, 0.8046869976468442598, 0.8072914749517984268, 0.8098954182986718431, 0.8124997131017763774, 0.8151039927934364826, 0.8177079459076636025, 0.8203124143928716139, 0.8229162019391148553, 0.8255207101697450423, 0.8281245470747605752, 0.8307289561943111966, 0.8333330672686687368, 0.8359371917364484261, 0.8385415877213925340, 0.8411454306083117061, 0.8437499359916976749, 0.8463537220259882421, 0.8489581999790609679, 0.8515621441131088210, 0.8541664395301816759, 0.8567707200483754004, 0.8593746738244238959, 0.8619791430964799384, 0.8645829313652741988, 0.8671874403030259693, 0.8697912779887684298, 0.8723956877520262498, 0.8749997996620757501, 0.8776039247821166844, 0.8802083216039426894, 0.8828121652047509205, 0.8854166713583762061, 0.8880204581660676721, 0.8906249368107317377, 0.8932288817749149956, 0.8958331778492237829, 0.8984374592372342816, 0.9010414137180589034, 0.9036458838204490807, 0.9062496728545991198, 0.9088541825429954368, 0.9114580210523274273, 0.9140624315026897317, 0.9166665442915585826, 0.9192706701069754960, 0.9218750678090992245, 0.9244789121666602272, 0.9270834191340497910, 0.9296872067579531329, 0.9322916861377325004, 0.9348956319750387767, 0.9374999287497546296, 0.9401042110508202043, 0.9427081662796877870, 0.9453126372565492375, 0.9479164270979697493, 0.9505209375757615042, 0.9531247769568838013, 0.9557291881641908349, 0.9583333018366511080, 0.9609374282806871781, 0.9635418271385329803, 0.9661456726567504427, 0.9687501794391485399, 0.9713539669241311181, 0.9739584505366999378, 0.9765624007674321705, 0.9791666904763859369, 0.9817709514985233366, 0.9843749191276834898, 0.9869795472165283634, 0.9895832986789295793, 0.9921868791097946394, 0.9947912178632822844, 0.9974000636350187632, 1.000000000000000000 ),
 .UNSPECIFIED. ) ;
#34622 = CARTESIAN_POINT ( 'NONE',  ( 7.637320603199683866, 7.804628880021436288, -0.7998128361456281477 ) ) ;
#34623 = FACE_OUTER_BOUND ( 'NONE', #87542, .T. ) ;
#34624 = CARTESIAN_POINT ( 'NONE',  ( -10.98545788874447915, 13.75743779547922863, 1.592267205258850460 ) ) ;
#34625 = CARTESIAN_POINT ( 'NONE',  ( -9.968679514594425584, 5.546356146656833630, 6.001058933476985935 ) ) ;
#34626 = CARTESIAN_POINT ( 'NONE',  ( 7.280365300414074703, 7.596107060012304402, -0.7216878364870257245 ) ) ;
#34627 = CARTESIAN_POINT ( 'NONE',  ( -2.830620210203090181, 6.524417021870718258, 0.000000000000000000 ) ) ;
#34629 = CARTESIAN_POINT ( 'NONE',  ( 0.3283783949157508819, 1.250606878306897984, -1.310747381600821049 ) ) ;
#34628 = CARTESIAN_POINT ( 'NONE',  ( 7.180978637093494044, 8.406838493811077839, -1.199719254218452047 ) ) ;
#34630 = CARTESIAN_POINT ( 'NONE',  ( -7.705111371268023923, 7.883718109434487253, 1.040834085586084257E-14 ) ) ;
#34631 = CARTESIAN_POINT ( 'NONE',  ( 3.167801447087334576, 6.847518788243868393, -0.7998128361456291469 ) ) ;
#34632 = CARTESIAN_POINT ( 'NONE',  ( -5.757633847399098670, 7.274473465504208036, 1.200491007486852002 ) ) ;
#34633 = CARTESIAN_POINT ( 'NONE',  ( 5.176180785367283654, 9.260904359562321275, -0.7998128361456481317 ) ) ;
#34634 = CARTESIAN_POINT ( 'NONE',  ( -6.764898216730284908, -7.628386336122852995, 6.764898216727350366 ) ) ;
#34635 = CARTESIAN_POINT ( 'NONE',  ( 4.025675347721991315, 7.559696154190033823, -0.3592088497781486534 ) ) ;
#34636 = CARTESIAN_POINT ( 'NONE',  ( 8.093854517678360949, 12.38665467069271386, 1.040834085586084257E-14 ) ) ;
#34637 = ORIENTED_EDGE ( 'NONE', *, *, #85583, .F. ) ;
#34638 = EDGE_CURVE ( 'NONE', #46524, #110107, #134577, .T. ) ;
#34639 = CARTESIAN_POINT ( 'NONE',  ( 3.437814515362676016, 1.178941034414218603, 1.440021488233768521 ) ) ;
#34640 = CARTESIAN_POINT ( 'NONE',  ( 0.8959254483255777446, -0.8623397379431455567, -1.710623486014851480 ) ) ;
#34641 = CARTESIAN_POINT ( 'NONE',  ( 0.7508259783030580836, 2.089789393294994468, 0.3585813216958123606 ) ) ;
#34642 = PRESENTATION_STYLE_ASSIGNMENT (( #117029 ) ) ;
#34643 = CARTESIAN_POINT ( 'NONE',  ( 0.3282377607281028453, 1.386164550367412929, 1.224999999999958566 ) ) ;
#34644 = CARTESIAN_POINT ( 'NONE',  ( -1.515977770626737664, 8.685538819012460721, -2.532029653471351338 ) ) ;
#34645 = CARTESIAN_POINT ( 'NONE',  ( -4.785665035943912571, 4.685623418130398399, 1.214306433183764966E-14 ) ) ;
#34646 = CARTESIAN_POINT ( 'NONE',  ( 9.585251415181632595, 10.28514086057449184, 0.000000000000000000 ) ) ;
#34647 = CARTESIAN_POINT ( 'NONE',  ( 4.539879430399799354, 1.283355579558099091, 1.494016145327778045 ) ) ;
#34648 = CARTESIAN_POINT ( 'NONE',  ( 1.032067064438058068, -2.067986175307830798, 0.4682213744369929098 ) ) ;
#34649 = CARTESIAN_POINT ( 'NONE',  ( -4.882907879216086933, 8.848476292394087395, -0.7998128361456281477 ) ) ;
#34650 = CARTESIAN_POINT ( 'NONE',  ( -10.79642412263275908, 6.372378903489562596, 5.136797334115418501 ) ) ;
#34651 = CARTESIAN_POINT ( 'NONE',  ( 10.39230484541330313, 3.447199233515649386, 5.999999999999906741 ) ) ;
#34652 = CARTESIAN_POINT ( 'NONE',  ( 6.386699327874667986, 1.908680410311427655, -1.076638258889956345 ) ) ;
#34653 = DIRECTION ( 'NONE',  ( 0.000000000000000000, -1.000000000000000000, 0.000000000000000000 ) ) ;
#34654 = CARTESIAN_POINT ( 'NONE',  ( 4.102502470231626397, -0.6033306519132185519, -1.829551733875626862 ) ) ;
#34655 = CARTESIAN_POINT ( 'NONE',  ( -6.659026002606323047, 10.92061410301605662, 0.000000000000000000 ) ) ;
#34656 = CARTESIAN_POINT ( 'NONE',  ( 0.2174332111963481196, -1.791455004416471430, 0.3504355335035569396 ) ) ;
#34657 = CARTESIAN_POINT ( 'NONE',  ( 0.8388348947251201837, 2.174866457552121268, 0.3736606161612308630 ) ) ;
#34658 = CARTESIAN_POINT ( 'NONE',  ( -0.2656570211550942084, 7.171539594011602681, 2.094714161149640042 ) ) ;
#34659 = ORIENTED_EDGE ( 'NONE', *, *, #178287, .T. ) ;
#34660 = EDGE_LOOP ( 'NONE', ( #102847, #30618, #4481 ) ) ;
#34661 = CARTESIAN_POINT ( 'NONE',  ( 6.262555971378708897, -0.7055598467285629782, -1.838920630280465041 ) ) ;
#34662 = CARTESIAN_POINT ( 'NONE',  ( 0.7318534483069280006, 1.913536139905326339, 0.3307262847246707493 ) ) ;
#34663 = CARTESIAN_POINT ( 'NONE',  ( 0.1399997263886003374, 0.002789056014650820314, -1.999853399661279063 ) ) ;
#34665 = CARTESIAN_POINT ( 'NONE',  ( 4.539814342829402882, 1.213294893355709503, 1.411164879910733472 ) ) ;
#34664 = CARTESIAN_POINT ( 'NONE',  ( -5.986807348886189040, 9.142303119412650503, -1.199719254218452047 ) ) ;
#34666 = CARTESIAN_POINT ( 'NONE',  ( 6.526270840131753737, 8.707344961610770540, -1.599625672291283607 ) ) ;
#34667 = DIRECTION ( 'NONE',  ( 1.276756478318932585E-15, -1.000000000000000000, 1.665334536937738262E-16 ) ) ;
#34668 = CARTESIAN_POINT ( 'NONE',  ( -4.394814349124112951, 8.279033840620114049, -0.7998128361456281477 ) ) ;
#34669 = CARTESIAN_POINT ( 'NONE',  ( -4.394251184604987870, 5.259619482528146150, 1.082531754730549078 ) ) ;
#34670 = CARTESIAN_POINT ( 'NONE',  ( 0.4159077360078728969, -1.177411712353953588, -1.848246096435968600 ) ) ;
#34671 = CARTESIAN_POINT ( 'NONE',  ( 4.934804725694211136, 6.780358151441803649, -1.443375672974051449 ) ) ;
#34672 = CARTESIAN_POINT ( 'NONE',  ( 10.99917004716958857, -6.764708007038256810, -0.1531059978909480312 ) ) ;
#34673 = DIRECTION ( 'NONE',  ( 0.6249999999999992228, 1.778438476333678106E-14, -0.7806247497998005658 ) ) ;
#34674 = CARTESIAN_POINT ( 'NONE',  ( 1.787459277025660542, 1.258035843444211155, 1.323286951131589895 ) ) ;
#34675 = CARTESIAN_POINT ( 'NONE',  ( -3.490334480514268645, 6.159475096320226939, -1.199719254218452935 ) ) ;
#34676 =( BOUNDED_SURFACE ( )  B_SPLINE_SURFACE ( 3, 2, ( 
 ( #189866, #64146, #30588 ),
 ( #13251, #29514, #128169 ),
 ( #95607, #177901, #44712 ),
 ( #12178, #15365, #196277 ) ),
 .UNSPECIFIED., .F., .F., .T. ) 
 B_SPLINE_SURFACE_WITH_KNOTS ( ( 4, 4 ),
 ( 3, 3 ),
 ( 0.005241070803109281785, 0.008267458746840847944 ),
 ( 0.000000000000000000, 1.000000000000000000 ),
 .UNSPECIFIED. ) 
 GEOMETRIC_REPRESENTATION_ITEM ( )  RATIONAL_B_SPLINE_SURFACE ( (
 ( 1.000000000000000000, 0.7184380228464080087, 1.000000000000000000),
 ( 1.000000000000000000, 0.7185467277397550312, 1.000000000000000000),
 ( 1.000000000000000000, 0.7186585579881030750, 1.000000000000000000),
 ( 1.000000000000000000, 0.7187737999613691420, 1.000000000000000000) ) ) 
 REPRESENTATION_ITEM ( '' )  SURFACE ( )  );
#34677 = CARTESIAN_POINT ( 'NONE',  ( 3.463219708433932009, -1.672243815576504700, -0.4589255088537134153 ) ) ;
#34678 = CARTESIAN_POINT ( 'NONE',  ( 1.224999999999969225, 1.937500000682795820, -2.081668171172168513E-14 ) ) ;
#34679 = CARTESIAN_POINT ( 'NONE',  ( 6.509000000000039421, 4.695815278351551214, 2.562658139094181386 ) ) ;
#34680 = CARTESIAN_POINT ( 'NONE',  ( -1.162044386198238935E-15, 0.3125000000000180411, 1.224999999999967004 ) ) ;
#34681 = CARTESIAN_POINT ( 'NONE',  ( 0.06489154195065281738, -1.720053269671377949, -0.8678208687467499072 ) ) ;
#34682 = CARTESIAN_POINT ( 'NONE',  ( 4.891432378139471737, -1.795214109662087942, 0.7913882323652280393 ) ) ;
#34683 = CARTESIAN_POINT ( 'NONE',  ( -9.027031348600448979, 9.425958082989001952, 1.040834085586084257E-14 ) ) ;
#34684 = CARTESIAN_POINT ( 'NONE',  ( 6.449928391799196525, 8.548002428564306143, -1.599625672291262513 ) ) ;
#34685 = CARTESIAN_POINT ( 'NONE',  ( 4.846395287928321416, 1.089488137594313510, -1.819044145143506208 ) ) ;
#34686 = CARTESIAN_POINT ( 'NONE',  ( 5.481239241674765950, 9.616805891921051952, -0.7998128361456481317 ) ) ;
#34687 = CARTESIAN_POINT ( 'NONE',  ( -8.459397779922852578, 11.95671561229694824, 1.199719254218453823 ) ) ;
#34688 = DIRECTION ( 'NONE',  ( 0.000000000000000000, 1.000000000000000000, 0.000000000000000000 ) ) ;
#34689 = CARTESIAN_POINT ( 'NONE',  ( 3.327070777303439364, -1.911029926764183040, -0.7966718667702379353 ) ) ;
#34691 = CARTESIAN_POINT ( 'NONE',  ( -1.402160292154681736E-14, 0.009375000341421267647, -1.575800808251665908 ) ) ;
#34690 = DIRECTION ( 'NONE',  ( 0.000000000000000000, 0.000000000000000000, 1.000000000000000000 ) ) ;
#34692 = ORIENTED_EDGE ( 'NONE', *, *, #126637, .F. ) ;
#34693 = CARTESIAN_POINT ( 'NONE',  ( 2.672825289193903942, 1.627854652907471777, 1.623211659370107363 ) ) ;
#34694 = CARTESIAN_POINT ( 'NONE',  ( 9.110716038703335684, 9.731516254683127087, -0.7216878364870197293 ) ) ;
#34696 = CARTESIAN_POINT ( 'NONE',  ( 3.285556943749998737, -1.655208332855374609, -1.896917185911906500 ) ) ;
#34695 = CARTESIAN_POINT ( 'NONE',  ( 7.838022202476093270, 8.316983122409855156, 0.7216878364870267237 ) ) ;
#34697 =( NAMED_UNIT ( * ) PLANE_ANGLE_UNIT ( ) SI_UNIT ( $, .RADIAN. ) );
#34698 = CARTESIAN_POINT ( 'NONE',  ( -10.30353590654652862, 3.711604710691488673, 6.155358625546677231 ) ) ;
#34699 = EDGE_LOOP ( 'NONE', ( #142438, #95917 ) ) ;
#34700 = LINE ( 'NONE', #183088, #163641 ) ;
#34701 = CARTESIAN_POINT ( 'NONE',  ( 4.552931727387078631, 0.3324577288378940954, 1.883125075537089854 ) ) ;
#34702 = CARTESIAN_POINT ( 'NONE',  ( 3.475000000000000533, -1.225000000000000311, 0.000000000000000000 ) ) ;
#34703 = CARTESIAN_POINT ( 'NONE',  ( 4.700069144524660736, -1.724479993061514449, -0.04023236952926077803 ) ) ;
#34704 = CARTESIAN_POINT ( 'NONE',  ( 3.467982673848205355, -0.9896861206786079501, 1.756853968756578066 ) ) ;
#34705 = CARTESIAN_POINT ( 'NONE',  ( 4.711759750379289180, 2.199509664246365848, 0.6680300025654511975 ) ) ;
#34706 = DIRECTION ( 'NONE',  ( 0.000000000000000000, -1.000000000000000000, 0.000000000000000000 ) ) ;
#34707 = CARTESIAN_POINT ( 'NONE',  ( 1.084930333755677045, -2.153824616689365978, -0.4803136671489223741 ) ) ;
#34708 = CARTESIAN_POINT ( 'NONE',  ( -4.584065335196305213, 6.441438539186039591, 1.443375672974058777 ) ) ;
#34709 = CARTESIAN_POINT ( 'NONE',  ( 6.186734212497608354, -0.2616995340462315300, -1.750118319643848119 ) ) ;
#34711 = CARTESIAN_POINT ( 'NONE',  ( 1.500361222516993331, -0.8285058210528316591, -2.137470567302256708 ) ) ;
#34710 = CARTESIAN_POINT ( 'NONE',  ( 6.062430963966053632, 7.101866208495718702, -1.199719254218452047 ) ) ;
#34712 = CARTESIAN_POINT ( 'NONE',  ( 0.3216633777232960067, 1.663872621647478622, 0.5102041932069888430 ) ) ;
#34713 = CARTESIAN_POINT ( 'NONE',  ( -2.300079615812729905, 5.835176651756807331, -0.7998128361456281477 ) ) ;
#34714 = CARTESIAN_POINT ( 'NONE',  ( -3.492107083971660586, 6.231819477012331632, 1.199719254218452935 ) ) ;
#34715 = CARTESIAN_POINT ( 'NONE',  ( -0.6801582343750074422, -0.1197916663252529546, -1.178068619123865846 ) ) ;
#34716 = CARTESIAN_POINT ( 'NONE',  ( 10.75000000000000000, 1.316495309083404618E-15, 0.000000000000000000 ) ) ;
#34717 = CARTESIAN_POINT ( 'NONE',  ( 0.5202908490967810273, 2.147468835798187037, -0.3191156193892603632 ) ) ;
#34718 = CARTESIAN_POINT ( 'NONE',  ( 1.341030165941111241, -1.731997234073547220, -1.032477317303444053 ) ) ;
#34719 = CARTESIAN_POINT ( 'NONE',  ( 1.499999999999989120, 0.8062500006828163812, 0.000000000000000000 ) ) ;
#34720 = CARTESIAN_POINT ( 'NONE',  ( 5.848256421918945236, 1.924412893870678820, 0.09223618542448899782 ) ) ;
#34721 = CARTESIAN_POINT ( 'NONE',  ( -0.6823417656250039265, 11.06770833367473550, -1.181850606188755259 ) ) ;
#34722 = CARTESIAN_POINT ( 'NONE',  ( 2.777807369331359411, 0.3217554308703252652, -2.197856884423950774 ) ) ;
#34723 = ORIENTED_EDGE ( 'NONE', *, *, #178034, .T. ) ;
#34724 = DIRECTION ( 'NONE',  ( 1.276756478318932585E-15, -1.000000000000000000, 1.665334536937738262E-16 ) ) ;
#34725 = FACE_OUTER_BOUND ( 'NONE', #129231, .T. ) ;
#34726 = CARTESIAN_POINT ( 'NONE',  ( 9.673906298550626559, 11.24497775551929557, 1.199719254218452047 ) ) ;
#34727 = PLANE ( 'NONE',  #201418 ) ;
#34728 = PRESENTATION_STYLE_ASSIGNMENT (( #37946 ) ) ;
#34729 = CARTESIAN_POINT ( 'NONE',  ( 4.159493969870859509, 0.8249727819007621754, 1.532509256507504025 ) ) ;
#34730 = CARTESIAN_POINT ( 'NONE',  ( 2.207404936347991065, -1.573848641742966459, -1.171066219227391070 ) ) ;
#34732 = CARTESIAN_POINT ( 'NONE',  ( -7.551528373131759508, 7.912463978182924684, 1.040834085586084257E-14 ) ) ;
#34731 = CARTESIAN_POINT ( 'NONE',  ( 3.310162060030825248, 7.013606170011280838, -0.7998128361456291469 ) ) ;
#34733 = FILL_AREA_STYLE_COLOUR ( '', #42214 ) ;
#34734 = CARTESIAN_POINT ( 'NONE',  ( 4.363950690066983107, 4.004001632660354915, -0.1812806842866887536 ) ) ;
#34735 = CARTESIAN_POINT ( 'NONE',  ( 0.5200786239168513347, 2.040466299037096309, -0.3010312105025755303 ) ) ;
#34736 = CARTESIAN_POINT ( 'NONE',  ( -7.212047647465563038, 10.50147379109678880, -1.199719254218446718 ) ) ;
#34737 = CARTESIAN_POINT ( 'NONE',  ( -3.511198595814942980, 5.119484333249288532, 1.443375672974064550 ) ) ;
#34738 = CARTESIAN_POINT ( 'NONE',  ( 0.9368240258568013568, 2.229511284875786536, 0.3842425355367936057 ) ) ;
#34739 = ORIENTED_EDGE ( 'NONE', *, *, #67181, .T. ) ;
#34740 = CARTESIAN_POINT ( 'NONE',  ( 0.7499999999999885647, 0.5145833340161540814, 1.299038105676657340 ) ) ;
#34741 = CARTESIAN_POINT ( 'NONE',  ( 2.881944908259078453, -0.9649329312324153030, 1.602325162460143559 ) ) ;
#34742 = CARTESIAN_POINT ( 'NONE',  ( 1.089978434334002433, -0.4226591196558672214, 1.681707840898168937 ) ) ;
#34743 = CARTESIAN_POINT ( 'NONE',  ( 5.847271748948593029, 0.6375361197438635941, -2.096799129279611762 ) ) ;
#34744 = CARTESIAN_POINT ( 'NONE',  ( 5.807753868445137080, -0.5680028841938968842, 2.236484270104825089 ) ) ;
#34745 = CARTESIAN_POINT ( 'NONE',  ( 1.147419824990800752, -1.624031055642958243, -1.268641727334917313 ) ) ;
#34746 = CARTESIAN_POINT ( 'NONE',  ( 3.204954726155031963, -0.3781314774268499379, 1.904617838069742275 ) ) ;
#34747 = CARTESIAN_POINT ( 'NONE',  ( -3.741687207247254676, 7.309126141856352454, 1.040834085586084257E-14 ) ) ;
#34748 = CARTESIAN_POINT ( 'NONE',  ( 5.641831084104285132, 0.7588036158820666843, -1.709917670604633066 ) ) ;
#34749 = CARTESIAN_POINT ( 'NONE',  ( 0.9375000000000007772, 1.451031289061083251, -1.451031289061159413 ) ) ;
#34750 = CARTESIAN_POINT ( 'NONE',  ( 1.415355422365517146, 13.32676603809294136, -0.06183170064162012147 ) ) ;
#34751 = CARTESIAN_POINT ( 'NONE',  ( 0.4909827745146425060, 1.656533638411663345, 0.5119339833263967243 ) ) ;
#34752 = CARTESIAN_POINT ( 'NONE',  ( 1.360316468749969365, 0.7447916670080855228, 0.7853790794158739264 ) ) ;
#34753 = CARTESIAN_POINT ( 'NONE',  ( 4.535779832184696936, -1.617819081767550182, 1.203352566194588746 ) ) ;
#34754 = CARTESIAN_POINT ( 'NONE',  ( -2.928197990427299668, 6.360055388899728435, 1.040834085586084257E-14 ) ) ;
#34755 = CARTESIAN_POINT ( 'NONE',  ( 7.964525173024008531, 11.37936423758166526, 1.199719254218460707 ) ) ;
#34756 = CARTESIAN_POINT ( 'NONE',  ( 4.203910148689107729, 7.062256385849379647, -1.199719254218448494 ) ) ;
#34758 = CARTESIAN_POINT ( 'NONE',  ( -15.75000000000000000, 10.19999999999999929, -0.7000000000000009548 ) ) ;
#34757 = CARTESIAN_POINT ( 'NONE',  ( 1.910518402784128433, 1.353611321597010253, -1.225282022559864625 ) ) ;
#34759 = CARTESIAN_POINT ( 'NONE',  ( -4.261005416444848315, 8.193199762486115034, 0.7998128361456352531 ) ) ;
#34760 = CARTESIAN_POINT ( 'NONE',  ( 6.689586359223958389, -7.817744194000435520, -6.745922712994591564 ) ) ;
#34761 = CARTESIAN_POINT ( 'NONE',  ( -10.50000000000000000, 10.19999999999999929, -3.600000000000000977 ) ) ;
#34762 = ORIENTED_EDGE ( 'NONE', *, *, #117585, .T. ) ;
#34763 = CARTESIAN_POINT ( 'NONE',  ( -5.682275777458886346, 7.722684055159061423, 1.443375672974058777 ) ) ;
#34764 = ADVANCED_FACE ( 'NONE', ( #56966 ), #154891, .F. ) ;
#34765 = CARTESIAN_POINT ( 'NONE',  ( -6.777912011469602760, -7.189630408300049069, 6.776323704810609527 ) ) ;
#34766 = CARTESIAN_POINT ( 'NONE',  ( -7.486073373039941359, 11.88550270185529278, -0.7998128361456291469 ) ) ;
#34767 = CARTESIAN_POINT ( 'NONE',  ( 0.1408863878445747453, 1.934039905153326799, 0.5823465565887532280 ) ) ;
#34769 = ORIENTED_EDGE ( 'NONE', *, *, #165987, .F. ) ;
#34768 = CARTESIAN_POINT ( 'NONE',  ( 0.06529689308308950224, -1.700389599856198863, 1.266735544122286283 ) ) ;
#34770 = CARTESIAN_POINT ( 'NONE',  ( -7.774674742793745708, 8.035151719539642912, 0.7998128361456341429 ) ) ;
#34771 = CARTESIAN_POINT ( 'NONE',  ( 4.330940004561544043, 7.140181541042074365, -1.199719254218452047 ) ) ;
#34772 = CIRCLE ( 'NONE', #211183, 0.08000000000000004330 ) ;
#34773 = CARTESIAN_POINT ( 'NONE',  ( 5.401267763076613271, 1.683455835520174526, 1.188505893847252581 ) ) ;
#34774 = CARTESIAN_POINT ( 'NONE',  ( 5.572888750952301073, -0.9041123360693378297, 1.802415994888312722 ) ) ;
#34775 = ORIENTED_EDGE ( 'NONE', *, *, #130557, .F. ) ;
#34776 = CARTESIAN_POINT ( 'NONE',  ( -1.115562610750309283E-14, 9.562500000000000000, 1.500000000000001554 ) ) ;
#34777 = CARTESIAN_POINT ( 'NONE',  ( 7.075376061485196821, 9.347967719856493218, 1.599625672291268286 ) ) ;
#34779 = ORIENTED_EDGE ( 'NONE', *, *, #87971, .F. ) ;
#34778 = CARTESIAN_POINT ( 'NONE',  ( -7.279802135894939852, 7.457800344824362604, -0.7998128361456362523 ) ) ;
#34780 = CARTESIAN_POINT ( 'NONE',  ( 4.672271667806711548, 8.395315985019093930, 0.5582388282892002396 ) ) ;
#34781 = CARTESIAN_POINT ( 'NONE',  ( 4.921249881687197458, 0.7690040753521177885, 1.863882819927860535 ) ) ;
#34782 = CARTESIAN_POINT ( 'NONE',  ( 4.716662652015527257, -0.08744826293657045890, 1.839185557975311358 ) ) ;
#34783 = CARTESIAN_POINT ( 'NONE',  ( -0.02319159430947542386, 5.725354828811364705, -2.405035539666657840 ) ) ;
#34784 = CARTESIAN_POINT ( 'NONE',  ( 3.000898454221593958, -0.6702494718498009929, -2.208213912191819617 ) ) ;
#34785 = CARTESIAN_POINT ( 'NONE',  ( 7.289443866002793371, 8.533381260871966134, 1.199719254218452047 ) ) ;
#34786 = CARTESIAN_POINT ( 'NONE',  ( 4.973979902034267653, 1.240098594129716458, 1.770319513135506062 ) ) ;
#34787 = CARTESIAN_POINT ( 'NONE',  ( 7.446452682403650769, 9.710614100936176385, -1.599625672291262513 ) ) ;
#34788 = CARTESIAN_POINT ( 'NONE',  ( 6.480030769895370746, -1.807141314969593848, -0.3518929191878711338 ) ) ;
#34789 = CARTESIAN_POINT ( 'NONE',  ( -4.623494077460110319, 5.352830164246910272, 1.199719254218462483 ) ) ;
#34790 = AXIS2_PLACEMENT_3D ( 'NONE', #207291, #113075, #76228 ) ;
#34791 = CARTESIAN_POINT ( 'NONE',  ( -9.453683584225196057, 15.47105875301949851, -7.391106286260058944 ) ) ;
#34792 = CARTESIAN_POINT ( 'NONE',  ( -6.140917232347002042, 6.129101290685087911, -0.7998128361456362523 ) ) ;
#34793 = CARTESIAN_POINT ( 'NONE',  ( 3.274138816734498025, -1.115311402298941656, 1.501645261301733481 ) ) ;
#34794 = ADVANCED_FACE ( 'NONE', ( #110048 ), #80243, .T. ) ;
#34797 = CARTESIAN_POINT ( 'NONE',  ( -6.947627372360122955, 7.070263120700404968, 0.000000000000000000 ) ) ;
#34796 = CARTESIAN_POINT ( 'NONE',  ( -0.6823417656249969321, 5.467708333674756283, -1.181850606188749264 ) ) ;
#34795 = CARTESIAN_POINT ( 'NONE',  ( 1.705181254219298115, 1.662258477346746588, -0.9455041445245655485 ) ) ;
#34798 = CARTESIAN_POINT ( 'NONE',  ( 2.807470779205251343, 1.864772411128329477, 1.179945617918669143 ) ) ;
#34799 = CARTESIAN_POINT ( 'NONE',  ( 4.517891501851804215, 6.293959390292322986, -1.599625672291255185 ) ) ;
#34800 = CARTESIAN_POINT ( 'NONE',  ( 6.658462837642791676, 8.861568958707010779, 1.443375672974063439 ) ) ;
#34801 = CARTESIAN_POINT ( 'NONE',  ( -3.113568832632681360, 6.784247404713427798, -0.7998128361456281477 ) ) ;
#34802 = CARTESIAN_POINT ( 'NONE',  ( -7.553300976144794454, 7.984808358356614733, -0.7216878364870338292 ) ) ;
#34803 = CARTESIAN_POINT ( 'NONE',  ( 0.1925371440497048448, -0.4299567264692584212, -1.931277891087788579 ) ) ;
#34804 = CARTESIAN_POINT ( 'NONE',  ( 0.4820102390354238375, 2.151571070674349606, -0.8345519191893053801 ) ) ;
#34805 = CARTESIAN_POINT ( 'NONE',  ( 1.223018651738450480, -1.772137153356953432, -0.8420139538000551704 ) ) ;
#34806 = CARTESIAN_POINT ( 'NONE',  ( 4.170800697546906299, 1.462118435030785646, -1.455038044888419702 ) ) ;
#34807 = CARTESIAN_POINT ( 'NONE',  ( 4.677199807034550183, 8.400557508274889784, 1.040834085586084257E-14 ) ) ;
#34808 = CARTESIAN_POINT ( 'NONE',  ( 5.332099551924443404, 9.442809587212341427, 0.000000000000000000 ) ) ;
#34809 = ORIENTED_EDGE ( 'NONE', *, *, #75894, .T. ) ;
#34810 = CARTESIAN_POINT ( 'NONE',  ( 7.199016378732056687, 10.38230762762066384, -1.082531754730537976 ) ) ;
#34811 = CARTESIAN_POINT ( 'NONE',  ( 1.364683531249988535, 4.217708333674752730, -0.7879004041258239610 ) ) ;
#34812 = DIRECTION ( 'NONE',  ( -0.000000000000000000, 1.000000000000000000, -0.000000000000000000 ) ) ;
#34813 = CARTESIAN_POINT ( 'NONE',  ( 4.650083499362875017, 5.487814173087225633, 1.082531754730560403 ) ) ;
#34814 = CARTESIAN_POINT ( 'NONE',  ( 6.215302479579098538, -1.858902078722439732, -1.121643639950772764 ) ) ;
#34816 = CARTESIAN_POINT ( 'NONE',  ( 6.532758020889952277, -1.641319963461195464, 0.8346263169811756200 ) ) ;
#34815 = FACE_OUTER_BOUND ( 'NONE', #134036, .T. ) ;
#34817 = CARTESIAN_POINT ( 'NONE',  ( -4.343764581222149701, 7.058997420150165070, 1.213430737042743957 ) ) ;
#34818 = CARTESIAN_POINT ( 'NONE',  ( 1.528351178377739927, 1.801267752838480840, 0.5040548479407629401 ) ) ;
#34819 = CARTESIAN_POINT ( 'NONE',  ( -6.138273485042783584, 5.995793210058552702, 0.01269068828805425264 ) ) ;
#34820 = CARTESIAN_POINT ( 'NONE',  ( -1.378728738066235859, 3.613591550242559070, -0.5908528300941767730 ) ) ;
#34821 = CARTESIAN_POINT ( 'NONE',  ( 6.265786130652515773, 6.994708711910199384, -0.9640221254198673151 ) ) ;
#34822 = CARTESIAN_POINT ( 'NONE',  ( -1.364683531249997417, 4.821875000341417916, 1.214306433183764966E-14 ) ) ;
#34823 = CARTESIAN_POINT ( 'NONE',  ( 1.066890508724306130, -1.507026839618429648, 1.177014404800474479 ) ) ;
#34824 = AXIS2_PLACEMENT_3D ( 'NONE', #156775, #8361, #140548 ) ;
#34825 = CARTESIAN_POINT ( 'NONE',  ( 3.520126680498508520, 1.123421168108656776, -1.367553765667248955 ) ) ;
#34826 = CARTESIAN_POINT ( 'NONE',  ( 0.5043727151736315806, -1.897847990334254886, -0.2338014693106793551 ) ) ;
#34828 = CARTESIAN_POINT ( 'NONE',  ( 3.814002402653454027, 1.021707883093534885, -1.620180217528136568 ) ) ;
#34827 = CARTESIAN_POINT ( 'NONE',  ( 9.579665964948885559, -7.473374494045003757, 0.07999999999999847511 ) ) ;
#34829 = CARTESIAN_POINT ( 'NONE',  ( -1.452583904633382383, 1.374772708486763806, 1.500000000000001332 ) ) ;
#34830 = CARTESIAN_POINT ( 'NONE',  ( 5.898876253247024692, 0.3825491175142159417, 1.931855958600266154 ) ) ;
#34831 = CARTESIAN_POINT ( 'NONE',  ( 0.9144942500491148873, -2.120778211678171488, 0.005759991200282587286 ) ) ;
#34832 = DIRECTION ( 'NONE',  ( 0.000000000000000000, 0.000000000000000000, -1.000000000000000000 ) ) ;
#34833 = CARTESIAN_POINT ( 'NONE',  ( 3.678450976403758066, -1.802590750232490491, -0.4997190347926713794 ) ) ;
#34835 = ORIENTED_EDGE ( 'NONE', *, *, #137674, .T. ) ;
#34834 = CARTESIAN_POINT ( 'NONE',  ( 1.084280211047653264, -1.780658692889337091, -0.4022698149812459212 ) ) ;
#34837 = CARTESIAN_POINT ( 'NONE',  ( -5.031484404002922517, 6.963427452793760963, 1.443375672974058777 ) ) ;
#34836 = CARTESIAN_POINT ( 'NONE',  ( 3.194164748978207680, -0.8942147705085048415, 2.017778291555922809 ) ) ;
#34838 = CARTESIAN_POINT ( 'NONE',  ( 1.364683531249990311, 5.196875000341417916, 1.214306433183764966E-14 ) ) ;
#34839 = CARTESIAN_POINT ( 'NONE',  ( 0.5728089798012192535, 1.423622861147020302, -1.492835154123072883 ) ) ;
#34840 = CARTESIAN_POINT ( 'NONE',  ( 7.623762449586013901, 7.788811034138823253, 1.040834085586084257E-14 ) ) ;
#34841 = CARTESIAN_POINT ( 'NONE',  ( -8.317037166979361018, 11.79062823052953668, 1.199719254218453823 ) ) ;
#34842 = CARTESIAN_POINT ( 'NONE',  ( -8.749942580429538097, 15.44732705574467779, -8.150331060152165463 ) ) ;
#34843 = CARTESIAN_POINT ( 'NONE',  ( -11.41381675112453564, 19.00000000000000000, 3.704697986577180746 ) ) ;
#34844 = CARTESIAN_POINT ( 'NONE',  ( 6.539320575229249144, 0.007148032025052972194, 1.896977914940492393 ) ) ;
#34845 = VERTEX_POINT ( 'NONE', #179012 ) ;
#34846 = CARTESIAN_POINT ( 'NONE',  ( 3.859880467719906783, -0.6038372105774907350, 1.980330894321411517 ) ) ;
#34847 = CARTESIAN_POINT ( 'NONE',  ( 0.7499999999999902300, 4.816666666666684193, -1.299038105676658228 ) ) ;
#34848 = CARTESIAN_POINT ( 'NONE',  ( 1.194844697948213463, -0.5240009448631496314, -2.097013730318515456 ) ) ;
#34849 = CARTESIAN_POINT ( 'NONE',  ( -5.043389779576542331, 7.890798448915884222, -1.099773784605091009 ) ) ;
#34850 = CARTESIAN_POINT ( 'NONE',  ( 1.471359524643547134, -1.733428207583002756, -1.036219422855472194 ) ) ;
#34851 = CARTESIAN_POINT ( 'NONE',  ( 7.058808231563191704, -6.527411821100059797, -6.446420058208622628 ) ) ;
#34853 = CARTESIAN_POINT ( 'NONE',  ( 9.110716038703335684, 9.731516254683127087, -0.7216878364870197293 ) ) ;
#34852 = CARTESIAN_POINT ( 'NONE',  ( 1.001543065824772753E-15, -3.412500000000000977, 4.012584370867899430 ) ) ;
#34854 = CARTESIAN_POINT ( 'NONE',  ( 6.731795954091533751, -1.842168972580451536, -0.8196458303668037182 ) ) ;
#34855 = CARTESIAN_POINT ( 'NONE',  ( -0.03006412033006514162, -0.9462945741195265548, 1.780671068589256834 ) ) ;
#34856 = CARTESIAN_POINT ( 'NONE',  ( 6.539320575229278454, 3.689604457162498630, 2.617406275049142916 ) ) ;
#34857 = CARTESIAN_POINT ( 'NONE',  ( 5.302338810847700756, 1.659911028786088760, -1.431018553749351829 ) ) ;
#34858 =( BOUNDED_SURFACE ( )  B_SPLINE_SURFACE ( 3, 2, ( 
 ( #105986, #172007, #155757 ),
 ( #139522, #7342, #73419 ),
 ( #189314, #174164, #141678 ),
 ( #46283, #195720, #77692 ),
 ( #177339, #75569, #9497 ),
 ( #191429, #157903, #76623 ) ),
 .UNSPECIFIED., .F., .F., .T. ) 
 B_SPLINE_SURFACE_WITH_KNOTS ( ( 4, 2, 4 ),
 ( 3, 3 ),
 ( 0.000000000000000000, 0.0003754691837024765901, 0.0007509383674049531802 ),
 ( 0.000000000000000000, 1.000000000000000000 ),
 .UNSPECIFIED. ) 
 GEOMETRIC_REPRESENTATION_ITEM ( )  RATIONAL_B_SPLINE_SURFACE ( (
 ( 1.000000000000000000, 0.6711954675835395401, 1.000000000000000000),
 ( 1.000000000000000000, 0.6709646295267452931, 1.000000000000000000),
 ( 1.000000000000000000, 0.6771840716659260906, 1.000000000000000000),
 ( 1.000000000000000000, 0.6927481755867372915, 1.000000000000000000),
 ( 1.000000000000000000, 0.7017972101309932764, 1.000000000000000000),
 ( 1.000000000000000000, 0.7071067811865475727, 1.000000000000000000) ) ) 
 REPRESENTATION_ITEM ( '' )  SURFACE ( )  );
#34859 = CARTESIAN_POINT ( 'NONE',  ( -1.201851678989727383E-14, 2.993750000682821266, 1.732050807568877637 ) ) ;
#34860 = CARTESIAN_POINT ( 'NONE',  ( 3.111475685156277038, 1.510342251817019532, 1.173009309769344588 ) ) ;
#34861 = CARTESIAN_POINT ( 'NONE',  ( -5.928993247877788697, 5.811580298812519807, 0.7998128361456341429 ) ) ;
#34862 = CARTESIAN_POINT ( 'NONE',  ( 4.406036734316882253, 6.163462161501577441, -1.443375672974051449 ) ) ;
#34864 = CARTESIAN_POINT ( 'NONE',  ( 1.107046246104196552, -0.04665650516593074226, 2.016035445577879504 ) ) ;
#34863 = CARTESIAN_POINT ( 'NONE',  ( -9.829298179783291900, 11.53023130024440768, 1.082531754730558626 ) ) ;
#34865 = CARTESIAN_POINT ( 'NONE',  ( 1.364683531250000303, 12.31770833367473195, -0.7879004041258355073 ) ) ;
#34867 = CARTESIAN_POINT ( 'NONE',  ( -4.142898457427624415, 6.991076079377632091, 1.199719254218452935 ) ) ;
#34866 = CARTESIAN_POINT ( 'NONE',  ( 0.3984806668858055789, -0.7796899918033869392, -2.155833124811225687 ) ) ;
#34868 = CARTESIAN_POINT ( 'NONE',  ( 3.680403716343355836, -1.662106674541915075, -0.4603510507015916020 ) ) ;
#34869 = CARTESIAN_POINT ( 'NONE',  ( -0.1405533004718703405, 5.725074605807632722, -2.314389626777931586 ) ) ;
#34870 = CARTESIAN_POINT ( 'NONE',  ( 5.345992642490140057, 5.131412925860272090, 1.040834085586084257E-14 ) ) ;
#34871 = CARTESIAN_POINT ( 'NONE',  ( 0.000000000000000000, 14.48154074412737202, -12.00000000000000178 ) ) ;
#34872 = CARTESIAN_POINT ( 'NONE',  ( 0.9241798626423223251, 0.9638202082158978667, 1.708698881219716137 ) ) ;
#34873 = CARTESIAN_POINT ( 'NONE',  ( -1.154700538379266339, -2.500000000000002220, 2.602085213965210642E-15 ) ) ;
#34874 = CARTESIAN_POINT ( 'NONE',  ( 5.515469562660962666, 5.329135999392899947, 0.7998128361456341429 ) ) ;
#34875 = CARTESIAN_POINT ( 'NONE',  ( 0.07536363704235479744, 6.947016338497881804, -2.739277465201896078 ) ) ;
#34876 = ORIENTED_EDGE ( 'NONE', *, *, #68027, .T. ) ;
#34877 = LINE ( 'NONE', #204833, #33834 ) ;
#34878 = ORIENTED_EDGE ( 'NONE', *, *, #181087, .T. ) ;
#34879 = CARTESIAN_POINT ( 'NONE',  ( 3.510248027248025426, -1.809562450863181127, -0.08562717191654131699 ) ) ;
#34880 = ORIENTED_EDGE ( 'NONE', *, *, #10566, .T. ) ;
#34881 = CARTESIAN_POINT ( 'NONE',  ( 6.964048179274811012, 8.153752959689313684, 1.199719254218452047 ) ) ;
#34882 = DIRECTION ( 'NONE',  ( -0.000000000000000000, -1.000000000000000000, -0.000000000000000000 ) ) ;
#34883 = CARTESIAN_POINT ( 'NONE',  ( 5.461500695664097904, -1.431772717462083566, -1.109608708211702099 ) ) ;
#34884 = CARTESIAN_POINT ( 'NONE',  ( 6.658462837642799670, 7.901199744405670522, 1.082531754730549967 ) ) ;
#34885 = SURFACE_STYLE_FILL_AREA ( #1308 ) ;
#34886 = CARTESIAN_POINT ( 'NONE',  ( 4.968100067739229075, 6.607231601306259527, -1.242533411653036879 ) ) ;
#34887 = ORIENTED_EDGE ( 'NONE', *, *, #201882, .T. ) ;
#34888 = ADVANCED_FACE ( 'NONE', ( #30628 ), #88478, .F. ) ;
#34890 = CARTESIAN_POINT ( 'NONE',  ( 9.028840231696797503, 12.62106513936658203, -1.199719254218446718 ) ) ;
#34889 = CARTESIAN_POINT ( 'NONE',  ( 5.934019871859393724, 1.109147300373466871, 1.494279092885692606 ) ) ;
#34891 = CARTESIAN_POINT ( 'NONE',  ( 4.323789496349770722, 0.8154102246901802076, -1.733521564635835732 ) ) ;
#34892 = CARTESIAN_POINT ( 'NONE',  ( -12.76460961864369814, 7.407083900356914441, 2.164514475593080078 ) ) ;
#34893 = CIRCLE ( 'NONE', #27947, 1.500000000000000222 ) ;
#34894 = DIRECTION ( 'NONE',  ( -0.2684563758389253985, 0.000000000000000000, 0.9632918427306595976 ) ) ;
#34895 = CARTESIAN_POINT ( 'NONE',  ( 0.6823417656249864960, -1.073958332991911568, -1.181850606188749264 ) ) ;
#34896 = CARTESIAN_POINT ( 'NONE',  ( 5.910991785878156435, 7.919243054989755670, -1.443375672974057666 ) ) ;
#34897 = CARTESIAN_POINT ( 'NONE',  ( -8.175203439360366531, 12.48156174598837787, 1.040834085586084257E-14 ) ) ;
#34898 = CARTESIAN_POINT ( 'NONE',  ( 0.6202742476981680797, -1.157488721396517040, -1.825510493854154426 ) ) ;
#34899 = CARTESIAN_POINT ( 'NONE',  ( -4.502189528189771472, 7.410248995266807803, -1.199719254218453823 ) ) ;
#34900 = EDGE_CURVE ( 'NONE', #61589, #142909, #162218, .T. ) ;
#34901 = CARTESIAN_POINT ( 'NONE',  ( 5.071631979963703962, 8.074598522336444262, 1.199719254218451159 ) ) ;
#34902 = CARTESIAN_POINT ( 'NONE',  ( 0.3229203692996869823, -0.09522068211164493035, 1.823229820405058099 ) ) ;
#34903 = CARTESIAN_POINT ( 'NONE',  ( -5.576481253922474401, 5.400316305864651056, -0.7998128361456221525 ) ) ;
#34904 = CARTESIAN_POINT ( 'NONE',  ( 2.994927033977520914, 1.566606242385214731, -0.9370212210159311050 ) ) ;
#34905 = CARTESIAN_POINT ( 'NONE',  ( -3.001048869802169783, 2.786623193720129343, 2.499999999999998668 ) ) ;
#34906 = CARTESIAN_POINT ( 'NONE',  ( 1.670022949053862948, 1.907054940702714863, -0.1439945843566131367 ) ) ;
#34907 = VERTEX_POINT ( 'NONE', #92190 ) ;
#34908 = CARTESIAN_POINT ( 'NONE',  ( 2.541402807867772840, 1.801932494976875576, -0.7955018757880153446 ) ) ;
#34909 = CARTESIAN_POINT ( 'NONE',  ( 5.267111086673036624, 1.870628123453799363, -0.5216035295831971119 ) ) ;
#34910 = CARTESIAN_POINT ( 'NONE',  ( -4.004454267989906668, 5.765225627445230927, 1.599625672291270506 ) ) ;
#34912 = CARTESIAN_POINT ( 'NONE',  ( 3.639029512587122372, 2.014767915268770082, 0.6618469929612482705 ) ) ;
#34911 = CARTESIAN_POINT ( 'NONE',  ( 4.543917759235442944, 5.330267469643351852, 1.199719254218452935 ) ) ;
#34913 = CARTESIAN_POINT ( 'NONE',  ( 9.596473800374404561, 10.09030761005864285, 0.000000000000000000 ) ) ;
#34914 = CARTESIAN_POINT ( 'NONE',  ( 6.095406204355903412, 6.027892130464396203, -0.2603320317973931153 ) ) ;
#34915 = CARTESIAN_POINT ( 'NONE',  ( -1.257518954445011827, 3.114770990628817682, -0.7749999999999918066 ) ) ;
#34916 = EDGE_LOOP ( 'NONE', ( #190349, #208983 ) ) ;
#34917 = CARTESIAN_POINT ( 'NONE',  ( -2.995508107964761191, 6.411541510041463887, -0.7147908198718248007 ) ) ;
#34918 = CARTESIAN_POINT ( 'NONE',  ( 4.258142763143749399, 7.125527769379820242, 1.199719254218451159 ) ) ;
#34919 = CIRCLE ( 'NONE', #90303, 11.00000000000000000 ) ;
#34920 = CARTESIAN_POINT ( 'NONE',  ( 4.688087255275310561, 8.691461907788344377, -0.7998128361456381397 ) ) ;
#34921 = CARTESIAN_POINT ( 'NONE',  ( 11.94650005372638013, 12.44897299662361867, -1.135399707157281890 ) ) ;
#34922 = CARTESIAN_POINT ( 'NONE',  ( 5.426323838365306074, 1.084245000580752238, -1.468710674947353967 ) ) ;
#34923 = FACE_BOUND ( 'NONE', #26175, .T. ) ;
#34924 = CARTESIAN_POINT ( 'NONE',  ( -9.327646496521989405, 10.94497100310623594, -1.082531754730539753 ) ) ;
#34925 = CARTESIAN_POINT ( 'NONE',  ( -6.510788175286835511, 6.826513026331759271, 0.5708727117093035375 ) ) ;
#34926 = CARTESIAN_POINT ( 'NONE',  ( 7.407835137441771245, -5.166862915010159263, 8.023115266309158500 ) ) ;
#34927 = CARTESIAN_POINT ( 'NONE',  ( 6.051601594667258333, 0.5412791183288803154, -1.790613848972313571 ) ) ;
#34928 = CARTESIAN_POINT ( 'NONE',  ( 6.103141704446003679, 10.27208242182903142, 0.7998128361456462443 ) ) ;
#34930 = ADVANCED_FACE ( 'NONE', ( #175554 ), #75904, .T. ) ;
#34929 = CARTESIAN_POINT ( 'NONE',  ( 3.650929903551769939, -1.574478333125122864, 1.109889904662264115 ) ) ;
#34931 = CARTESIAN_POINT ( 'NONE',  ( -4.199533704925234368, 7.510932310329544670, -0.9222493318717175370 ) ) ;
#34932 = AXIS2_PLACEMENT_3D ( 'NONE', #149730, #132453, #116218 ) ;
#34933 = CARTESIAN_POINT ( 'NONE',  ( 4.704842999142070603, 5.447737239542574272, -1.199719254218452047 ) ) ;
#34934 = CARTESIAN_POINT ( 'NONE',  ( 1.364683531249996529, 9.526041667008062319, 0.7879004041258405033 ) ) ;
#34935 = CARTESIAN_POINT ( 'NONE',  ( -6.749261541504576911, 6.768559974710451677, 1.040834085586084257E-14 ) ) ;
#34936 = CARTESIAN_POINT ( 'NONE',  ( 3.708318708537623021, 4.285125567170706695, -1.199719254218446718 ) ) ;
#34937 = CARTESIAN_POINT ( 'NONE',  ( -4.787437638956939523, 5.718337012605431369, -1.082531754730549967 ) ) ;
#34938 = CARTESIAN_POINT ( 'NONE',  ( 0.9489988177146626569, -1.915858558953801749, -0.9014485902382618487 ) ) ;
#34939 = CARTESIAN_POINT ( 'NONE',  ( 9.901532256681887745, 10.44620914241737530, 0.000000000000000000 ) ) ;
#34941 = EDGE_CURVE ( 'NONE', #139957, #91093, #93248, .T. ) ;
#34940 = CARTESIAN_POINT ( 'NONE',  ( -6.132223229318823243, 5.371873414713975947, 2.500000000000000444 ) ) ;
#34942 = CARTESIAN_POINT ( 'NONE',  ( 6.666853767972947153, 1.538155548931797956, -1.385880503156889487 ) ) ;
#34944 = CARTESIAN_POINT ( 'NONE',  ( 4.026147685736890303, 7.792003671190927960, 0.3652107146706294882 ) ) ;
#34943 = CARTESIAN_POINT ( 'NONE',  ( 1.927068723821170559, -1.203646435588998420, -1.393412863611859454 ) ) ;
#34945 = CARTESIAN_POINT ( 'NONE',  ( 5.748293942514166588, 7.729428904398431222, -1.443375672974057666 ) ) ;
#34946 = CARTESIAN_POINT ( 'NONE',  ( 4.312902262922978736, 5.164712407232485702, -1.082531754730548412 ) ) ;
#34947 = CARTESIAN_POINT ( 'NONE',  ( 0.9027369068667027152, 1.732534852245724233, -1.501034128341944607 ) ) ;
#34949 = DIRECTION ( 'NONE',  ( 1.561251128379126077E-17, 1.301042606982605475E-17, 1.000000000000000000 ) ) ;
#34948 = CARTESIAN_POINT ( 'NONE',  ( -1.352264364406415176, 3.300000000000026024, -0.2254051929223724882 ) ) ;
#34950 = EDGE_CURVE ( 'NONE', #82080, #119302, #20408, .T. ) ;
#34951 = ORIENTED_EDGE ( 'NONE', *, *, #71220, .F. ) ;
#34952 = CARTESIAN_POINT ( 'NONE',  ( 7.741342523278692767, 11.01502146292508044, 1.082531754730558626 ) ) ;
#34953 = CARTESIAN_POINT ( 'NONE',  ( 1.019790247428183472, -0.4849793317353002786, 1.953821064534920326 ) ) ;
#34954 = CARTESIAN_POINT ( 'NONE',  ( 0.6023038706522118035, 1.956103482322549825, 0.1501044349687257751 ) ) ;
#34955 = CARTESIAN_POINT ( 'NONE',  ( -10.13488352141530768, 11.78278451552804817, 1.199719254218462483 ) ) ;
#34957 = CARTESIAN_POINT ( 'NONE',  ( -9.420111044277531320, 2.999985932080179829, -6.906458289183190047 ) ) ;
#34956 = CARTESIAN_POINT ( 'NONE',  ( -6.828502922777144768, 11.11833717654868892, 0.7998128361456481317 ) ) ;
#34958 = CARTESIAN_POINT ( 'NONE',  ( 1.642778471875000035, -0.6635416661887084677, -2.845375778867859751 ) ) ;
#34961 = B_SPLINE_CURVE_WITH_KNOTS ( 'NONE', 3,
 ( #210890, #47364, #14816, #130791, #115590, #178419, #113478 ),
 .UNSPECIFIED., .F., .F.,
 ( 4, 3, 4 ),
 ( 8.673617379884028731E-19, 0.0008000000000005099386, 0.002977368225425562967 ),
 .UNSPECIFIED. ) ;
#34960 = CARTESIAN_POINT ( 'NONE',  ( 2.817004693338585941, -0.1753839976894235320, 1.761133515796961868 ) ) ;
#34959 = CARTESIAN_POINT ( 'NONE',  ( 3.908215892115148637, 1.478387765550030153, -1.478483494758761951 ) ) ;
#34962 = DIRECTION ( 'NONE',  ( 0.000000000000000000, 1.000000000000000000, 0.000000000000000000 ) ) ;
#34964 = CARTESIAN_POINT ( 'NONE',  ( 4.998102599042142380, -0.7687487195138610341, -2.159632177038037337 ) ) ;
#34963 = CARTESIAN_POINT ( 'NONE',  ( -11.86580791720155226, 7.723834678533566311, 1.807467791464186346 ) ) ;
#34965 = CARTESIAN_POINT ( 'NONE',  ( 3.714586447349605081, -0.1257948980903991487, 1.735838019273880928 ) ) ;
#34966 = CARTESIAN_POINT ( 'NONE',  ( 2.866659414285625651, 5.431854185720147221, -1.199719254218446718 ) ) ;
#34967 = CARTESIAN_POINT ( 'NONE',  ( 6.086684617892325733, 6.065829907154645539, -0.7998128361456481317 ) ) ;
#34968 = CARTESIAN_POINT ( 'NONE',  ( 2.776348759439921654, -1.715481723685903903, 0.2504971047874882117 ) ) ;
#34969 = CARTESIAN_POINT ( 'NONE',  ( 3.666621648402784484, -0.8769701800699877259, -1.986351817242467677 ) ) ;
#34970 = CARTESIAN_POINT ( 'NONE',  ( 5.834086172582112262, 5.700855377634248100, 1.040834085586084257E-14 ) ) ;
#34971 = CARTESIAN_POINT ( 'NONE',  ( 4.786342355033275986, -0.6839347017603314427, -1.897111394664739326 ) ) ;
#34972 = CARTESIAN_POINT ( 'NONE',  ( 1.125000000000000888, -2.052068128417952497, 6.471134675641443159E-14 ) ) ;
#34973 = AXIS2_PLACEMENT_3D ( 'NONE', #153626, #72347, #40955 ) ;
#34974 = CARTESIAN_POINT ( 'NONE',  ( -1.500000000000013101, 4.160416667349482900, -0.8660254037844313801 ) ) ;
#34975 = CARTESIAN_POINT ( 'NONE',  ( 1.957912498325198536, 1.921386756000037055, -0.1395382256239047214 ) ) ;
#34976 = CARTESIAN_POINT ( 'NONE',  ( -6.009258394948636914E-15, 9.218750000682799595, -1.732050807568875195 ) ) ;
#34977 = CARTESIAN_POINT ( 'NONE',  ( 5.133148801814766848, 2.052693810517117079, 0.8496366593433544168 ) ) ;
#34978 = VERTEX_POINT ( 'NONE', #192833 ) ;
#34980 = CIRCLE ( 'NONE', #156071, 0.07999999999999998779 ) ;
#34979 = CARTESIAN_POINT ( 'NONE',  ( -0.1110810684433142237, 6.948330828014858795, -2.391984312838004278 ) ) ;
#34981 = CARTESIAN_POINT ( 'NONE',  ( 1.499999999999989120, 1.275000000000019229, 0.000000000000000000 ) ) ;
#34982 = CARTESIAN_POINT ( 'NONE',  ( 5.452350330990040739, 9.512825819463730070, 0.7998128361456462443 ) ) ;
#34983 = CARTESIAN_POINT ( 'NONE',  ( 3.158686601859607368, 6.628958768904106513, -0.7216878364870267237 ) ) ;
#34984 = CARTESIAN_POINT ( 'NONE',  ( -3.285556943750000514, -1.188541666188710044, -1.896917185911906722 ) ) ;
#34985 = CARTESIAN_POINT ( 'NONE',  ( 1.840792944257110042, 1.275724102719773434, -1.818268329069183897 ) ) ;
#34986 = CARTESIAN_POINT ( 'NONE',  ( 6.303176765056641706, -1.658072099422291057, 1.048360225930293321 ) ) ;
#34987 = CARTESIAN_POINT ( 'NONE',  ( 7.592202833972727660, 11.80139437303613015, -0.7216878364870267237 ) ) ;
#34988 = CARTESIAN_POINT ( 'NONE',  ( 0.3965938887841921612, 3.117564169212590830, 1.962087417844435189 ) ) ;
#34989 = CARTESIAN_POINT ( 'NONE',  ( 6.872354139354274416, -1.400524804419982727, 1.777693731722047588 ) ) ;
#34990 = CARTESIAN_POINT ( 'NONE',  ( 4.634908411025333130, 6.500755460986618495, 1.599625672291268286 ) ) ;
#34991 = CARTESIAN_POINT ( 'NONE',  ( -3.960390268967665328, 6.674186842887300131, 1.082531754730549967 ) ) ;
#34992 = CARTESIAN_POINT ( 'NONE',  ( 4.316881300680885047, -1.530586319191833633, 1.382930202259499364 ) ) ;
#34993 = CARTESIAN_POINT ( 'NONE',  ( -4.741601036477307574, 6.554953847355395880, 1.599625672291267398 ) ) ;
#34994 = CARTESIAN_POINT ( 'NONE',  ( 1.499999999999990896, 3.806250000682819046, 1.214306433183764966E-14 ) ) ;
#34995 = CARTESIAN_POINT ( 'NONE',  ( -1.364683531250000748, -0.7406249996585803075, 0.000000000000000000 ) ) ;
#34996 = CARTESIAN_POINT ( 'NONE',  ( 6.397708313642382905, -0.6301307688901837123, 1.761319926792910495 ) ) ;
#34997 = CARTESIAN_POINT ( 'NONE',  ( 4.412597608232919022, -1.071937594435016683, -1.363045487976799475 ) ) ;
#34998 = CARTESIAN_POINT ( 'NONE',  ( 4.598987173745545221, -0.4583060902535853187, 1.678952109248931901 ) ) ;
#34999 = CARTESIAN_POINT ( 'NONE',  ( 4.009460741339333723, 5.700790169694431420, -1.599625672291256295 ) ) ;
#35000 = CARTESIAN_POINT ( 'NONE',  ( 2.437429393347473994, -1.701094670537067755, -1.536833775788006173 ) ) ;
#35001 = CARTESIAN_POINT ( 'NONE',  ( 1.364683531249988535, 3.676041667008087099, 0.7879004041258500513 ) ) ;
#35002 = CARTESIAN_POINT ( 'NONE',  ( 5.899963319545262763, -0.7533809947482277281, -1.950465142816688813 ) ) ;
#35003 = CARTESIAN_POINT ( 'NONE',  ( 6.580031058444741454, -1.904989947508778814, -0.3762313139713204801 ) ) ;
#35004 = CARTESIAN_POINT ( 'NONE',  ( 0.2834499351972658010, -6.554910260573309166, 9.477100694337659448 ) ) ;
#35005 = CARTESIAN_POINT ( 'NONE',  ( 1.354138928560550292, 0.1455316553338575902, -2.011204400906742240 ) ) ;
#35006 = CARTESIAN_POINT ( 'NONE',  ( -5.721177634842498527, 5.777054783512106440, 0.000000000000000000 ) ) ;
#35007 = CARTESIAN_POINT ( 'NONE',  ( 8.329933198152533080, 13.18708556817446009, -8.542943463288903416 ) ) ;
#35008 = CARTESIAN_POINT ( 'NONE',  ( -6.991200766141138168, 11.30815132714001159, 0.7998128361456481317 ) ) ;
#35009 = CARTESIAN_POINT ( 'NONE',  ( 5.198661835836162481, 8.152523677529138979, 1.199719254218462483 ) ) ;
#35010 = CARTESIAN_POINT ( 'NONE',  ( 3.053504691927158898, -1.869126254513186591, 1.001442229663196182 ) ) ;
#35011 = CARTESIAN_POINT ( 'NONE',  ( -1.364683531250014514, -0.9697916663252473812, 0.7879004041258379498 ) ) ;
#35012 = CARTESIAN_POINT ( 'NONE',  ( 5.250558533952181861, 0.5335417292645014964, 1.745990657226546894 ) ) ;
#35013 = ORIENTED_EDGE ( 'NONE', *, *, #161705, .F. ) ;
#35014 = CARTESIAN_POINT ( 'NONE',  ( -4.932134020321308654, 8.976183133675331050, 0.7998128361456291469 ) ) ;
#35015 = EDGE_CURVE ( 'NONE', #74053, #47282, #210605, .T. ) ;
#35016 = CARTESIAN_POINT ( 'NONE',  ( -0.5000000000000229816, 3.999999999999976019, 0.4999999999999553690 ) ) ;
#35017 = CARTESIAN_POINT ( 'NONE',  ( 1.001543065824772753E-15, -0.8093749995220410609, 3.793834371823811669 ) ) ;
#35018 = CARTESIAN_POINT ( 'NONE',  ( -6.826694039680798021, 7.923230120171105284, -1.199719254218446718 ) ) ;
#35019 = CARTESIAN_POINT ( 'NONE',  ( 3.129170305635332383, 1.827809467758968243, 0.8596994449004448091 ) ) ;
#35020 = CARTESIAN_POINT ( 'NONE',  ( 6.335036379411270957, 0.2100110484798515254, 2.196758413611602290 ) ) ;
#35021 = CARTESIAN_POINT ( 'NONE',  ( -3.984117037569407938, 5.741498858621315371, 1.599625672291270506 ) ) ;
#35022 = CARTESIAN_POINT ( 'NONE',  ( 3.959670595502752022, -0.5440038360976228171, 1.779617975935204655 ) ) ;
#35023 = CARTESIAN_POINT ( 'NONE',  ( 8.565000355531088516, 11.01558638625153286, -1.599625672291257406 ) ) ;
#35024 = CARTESIAN_POINT ( 'NONE',  ( 11.84668729035180590, 13.50518580017410564, -1.400000000000001688 ) ) ;
#35025 = CARTESIAN_POINT ( 'NONE',  ( -4.925689880466507908, 4.641059703499347044, -0.7998128361456221525 ) ) ;
#35026 = CARTESIAN_POINT ( 'NONE',  ( -6.832419346282942563, 10.05857410638369487, 1.199719254218453823 ) ) ;
#35028 = CARTESIAN_POINT ( 'NONE',  ( -5.229776604766065873, 6.614552831964506829, 1.409540066939333425 ) ) ;
#35027 = CARTESIAN_POINT ( 'NONE',  ( -6.720001414228860881, 7.869031733802326123, -1.199719254218452047 ) ) ;
#35029 = CARTESIAN_POINT ( 'NONE',  ( 0.6823417656249882723, -0.3239583329919110133, -1.181850606188749264 ) ) ;
#35030 = CARTESIAN_POINT ( 'NONE',  ( 1.862203476926355794, -0.5897614712949137417, 1.630587920151181924 ) ) ;
#35031 = CARTESIAN_POINT ( 'NONE',  ( 1.692878195147719422, -0.5885122380313506651, 1.637943671576999272 ) ) ;
#35033 = CARTESIAN_POINT ( 'NONE',  ( 7.863365906246055914, 10.19701286208565705, -1.443375672974057666 ) ) ;
#35032 = CARTESIAN_POINT ( 'NONE',  ( 0.4644773334415828736, 2.281836724062924038, -0.3429670027690605583 ) ) ;
#35034 = CARTESIAN_POINT ( 'NONE',  ( 5.252858170651868441, 5.093032385374103299, -0.7998128361456481317 ) ) ;
#35035 = CARTESIAN_POINT ( 'NONE',  ( 1.651711298185059684, 0.6011997390959940013, -1.971106496394055885 ) ) ;
#35036 = CARTESIAN_POINT ( 'NONE',  ( 5.464099601507359516, 6.333536608968757697, 1.199719254218462483 ) ) ;
#35037 = EDGE_CURVE ( 'NONE', #105457, #168364, #86454, .T. ) ;
#35038 = CARTESIAN_POINT ( 'NONE',  ( 0.3685172633814579601, -0.5404119286356176000, 1.942243004588292354 ) ) ;
#35039 = CARTESIAN_POINT ( 'NONE',  ( -1.225000000000026290, 1.020833333333308834, 0.7072540797572558491 ) ) ;
#35040 = CARTESIAN_POINT ( 'NONE',  ( -4.437261413422502798, 8.398831758960053406, 0.000000000000000000 ) ) ;
#35041 =( GEOMETRIC_REPRESENTATION_CONTEXT ( 3 ) GLOBAL_UNCERTAINTY_ASSIGNED_CONTEXT ( ( #62997 ) ) GLOBAL_UNIT_ASSIGNED_CONTEXT ( ( #177344, #196782, #21992 ) ) REPRESENTATION_CONTEXT ( 'NONE', 'WORKASPACE' ) );
#35042 = CARTESIAN_POINT ( 'NONE',  ( 0.5144491564793505223, 1.361202580669124584, -1.426332009298651116 ) ) ;
#35044 = CARTESIAN_POINT ( 'NONE',  ( -6.780486220610184134, 9.003929572168926754, -1.443375672974066548 ) ) ;
#35043 = CARTESIAN_POINT ( 'NONE',  ( 4.429883728109570207, -1.874397765517330061, 0.3784635845696313061 ) ) ;
#35045 = CARTESIAN_POINT ( 'NONE',  ( 6.428370569364434850, 1.274405893209800356, -1.801548588985131039 ) ) ;
#35046 = CARTESIAN_POINT ( 'NONE',  ( -1.752700365193352367E-14, 1.875000000682780943, 1.414508159514551444 ) ) ;
#35047 = CARTESIAN_POINT ( 'NONE',  ( -0.4499999999999833578, 4.000000000000003553, -0.9353126743251295450 ) ) ;
#35048 = CARTESIAN_POINT ( 'NONE',  ( 3.567203813726958828, 6.215469311773181182, 1.082531754730549078 ) ) ;
#35049 = CARTESIAN_POINT ( 'NONE',  ( -4.055297343818976330, 5.824542549245813383, 1.443375672974065660 ) ) ;
#35050 = CARTESIAN_POINT ( 'NONE',  ( 0.3112020186443940628, 1.677875239561373855, -1.123872588032665210 ) ) ;
#35051 = ORIENTED_EDGE ( 'NONE', *, *, #153089, .F. ) ;
#35052 = CARTESIAN_POINT ( 'NONE',  ( 2.907580275951544113, 1.948851909871853749, 1.235431545971882095 ) ) ;
#35053 = CARTESIAN_POINT ( 'NONE',  ( 4.545333077707183200, 1.753367681936630840, -0.8802267832125689750 ) ) ;
#35054 = CARTESIAN_POINT ( 'NONE',  ( 0.4616703453074429975, -0.5288386019042885522, 1.889040479230045255 ) ) ;
#35055 = CARTESIAN_POINT ( 'NONE',  ( 3.606105671554957759, 4.269840040644637291, -1.082531754730543083 ) ) ;
#35056 = FACE_OUTER_BOUND ( 'NONE', #184614, .T. ) ;
#35057 = ORIENTED_EDGE ( 'NONE', *, *, #106262, .F. ) ;
#35058 = CARTESIAN_POINT ( 'NONE',  ( 0.4447203898077173312, -1.529029696559053741, 1.464872618488068490 ) ) ;
#35060 = CARTESIAN_POINT ( 'NONE',  ( -6.835281999583978418, 11.12624609948998966, -0.7998128361456291469 ) ) ;
#35059 = CARTESIAN_POINT ( 'NONE',  ( -4.517891501851816649, 6.293959390292322986, -1.599625672291256295 ) ) ;
#35061 = CARTESIAN_POINT ( 'NONE',  ( 0.1636598862229492191, -1.205073137261414962, 1.392071761982638378 ) ) ;
#35062 = CARTESIAN_POINT ( 'NONE',  ( 3.538082186586584577, 1.373364251514897383, 1.681533162179976060 ) ) ;
#35063 = CARTESIAN_POINT ( 'NONE',  ( 0.1107184056071714995, 2.601508666554186444, 2.078650322257169503 ) ) ;
#35064 = CARTESIAN_POINT ( 'NONE',  ( 1.266058358664986949, 0.6103625328083387425, -2.030891291126469600 ) ) ;
#35065 = CARTESIAN_POINT ( 'NONE',  ( 0.7499999999999885647, 3.097916667349487341, -1.299038105676658228 ) ) ;
#35066 = CARTESIAN_POINT ( 'NONE',  ( 8.378048858240820351, 11.86180853700128601, -1.199719254218446718 ) ) ;
#35067 = CARTESIAN_POINT ( 'NONE',  ( 11.92619526913699879, 13.40000000000000036, -1.328859060402686199 ) ) ;
#35068 = CARTESIAN_POINT ( 'NONE',  ( 6.480989489388473856, 6.848452138476523565, -0.6157061703677743081 ) ) ;
#35069 = CARTESIAN_POINT ( 'NONE',  ( 2.337248977212981860, -1.842284197780035493, 0.9235709308827669828 ) ) ;
#35070 = CIRCLE ( 'NONE', #3972, 0.07999999999999933553 ) ;
#35072 = CARTESIAN_POINT ( 'NONE',  ( -9.367496997601300279, 15.00000000000599343, 7.499999999995378808 ) ) ;
#35071 = CARTESIAN_POINT ( 'NONE',  ( -8.371269781434001800, 11.85389961405997816, -1.199719254218446718 ) ) ;
#35073 = CARTESIAN_POINT ( 'NONE',  ( -1.364683531250012516, 2.530208333674753174, 0.7879004041258379498 ) ) ;
#35074 = CARTESIAN_POINT ( 'NONE',  ( 0.07755575628183573877, 1.996246338214379801, -2.602582295553407032 ) ) ;
#35075 = CARTESIAN_POINT ( 'NONE',  ( 1.378728738066228754, 4.086408449757453099, -0.5908528300941744416 ) ) ;
#35076 = ORIENTED_EDGE ( 'NONE', *, *, #4927, .T. ) ;
#35077 = CARTESIAN_POINT ( 'NONE',  ( 4.354103434560454566, 0.8146061972254794448, -1.730223316255767196 ) ) ;
#35078 = CARTESIAN_POINT ( 'NONE',  ( -0.9311234436981480345, -1.121869630441516996, -3.475000000000001421 ) ) ;
#35079 = CARTESIAN_POINT ( 'NONE',  ( 1.493865258296807275, 1.713033017868152763, 1.477889207592040455 ) ) ;
#35080 = CARTESIAN_POINT ( 'NONE',  ( -3.195971524519394702, 4.751719416737803847, -1.599625672291262513 ) ) ;
#35081 = CARTESIAN_POINT ( 'NONE',  ( 1.546807606353679754, 0.1796435140209233228, 1.802673299184972322 ) ) ;
#35082 = CARTESIAN_POINT ( 'NONE',  ( 0.8838324889288513564, -1.915903395820263366, 0.003361870754229472590 ) ) ;
#35083 = CARTESIAN_POINT ( 'NONE',  ( 2.242711981562468093, -2.029969483702593003, -0.4061203719310027549 ) ) ;
#35084 = CARTESIAN_POINT ( 'NONE',  ( 1.364683531249986537, 1.467708333674748289, -0.7879004041258239610 ) ) ;
#35085 = AXIS2_PLACEMENT_3D ( 'NONE', #112466, #86034, #193643 ) ;
#35086 = CARTESIAN_POINT ( 'NONE',  ( 0.07499057489264608634, 0.002531239327739977750, -1.955573237620360949 ) ) ;
#35087 = CARTESIAN_POINT ( 'NONE',  ( 5.285741052758629266, 1.295255816434317753, 1.426247342039884014 ) ) ;
#35088 = EDGE_CURVE ( 'NONE', #128985, #116165, #35956, .T. ) ;
#35090 = CARTESIAN_POINT ( 'NONE',  ( 6.292946923374557855, 6.878031543426355476, -0.7329977330566839200 ) ) ;
#35089 = CARTESIAN_POINT ( 'NONE',  ( 0.3468381721418262731, 2.301974930567828537, 0.1634500305177730706 ) ) ;
#35091 = CARTESIAN_POINT ( 'NONE',  ( 0.6823417656249899377, 2.092708333674753174, 1.181850606188767472 ) ) ;
#35092 = CARTESIAN_POINT ( 'NONE',  ( 4.703617135414410733, -1.592502274362836978, -1.310920101374695168 ) ) ;
#35093 = CARTESIAN_POINT ( 'NONE',  ( -5.900823170445743671, 7.907379670318584353, 1.599625672291269396 ) ) ;
#35094 = CARTESIAN_POINT ( 'NONE',  ( 8.776205506747620788, 9.133327934160710981, -0.7998128361456221525 ) ) ;
#35095 = DIRECTION ( 'NONE',  ( 0.000000000000000000, 0.000000000000000000, -1.000000000000000000 ) ) ;
#35096 = CARTESIAN_POINT ( 'NONE',  ( 5.412729640353754590, 7.337937218544611895, 1.599625672291267398 ) ) ;
#35098 = CARTESIAN_POINT ( 'NONE',  ( -0.7499999999999972244, 3.358333333333359150, -1.299038105676652011 ) ) ;
#35097 = CARTESIAN_POINT ( 'NONE',  ( 5.790091041381728587, -0.9498100376258570288, 1.879691625423451029 ) ) ;
#35099 = CARTESIAN_POINT ( 'NONE',  ( 0.5730174903513629570, 1.496870926018354364, -1.572904236412080436 ) ) ;
#35100 = CARTESIAN_POINT ( 'NONE',  ( -0.6823417656250212460, 1.863541667008083991, 1.181850606188755259 ) ) ;
#35101 = CARTESIAN_POINT ( 'NONE',  ( 5.272814564875167420, -2.033366364591123521, -0.7337546567489710014 ) ) ;
#35102 = CARTESIAN_POINT ( 'NONE',  ( 5.303380940763749329, 1.780254367526274972, -0.9538449857209270188 ) ) ;
#35103 = CARTESIAN_POINT ( 'NONE',  ( -1.015412733742047324, 2.800000000000017586, 0.9313266920541376503 ) ) ;
#35104 = VERTEX_POINT ( 'NONE', #94314 ) ;
#35107 = CARTESIAN_POINT ( 'NONE',  ( 5.666945020832170776, 7.634521829102760115, 1.443375672974062551 ) ) ;
#35106 = CARTESIAN_POINT ( 'NONE',  ( -3.285556943750000070, -2.209374999522041527, 0.000000000000000000 ) ) ;
#35105 = CARTESIAN_POINT ( 'NONE',  ( 8.025500584646550806, 8.327781868367935658, 0.000000000000000000 ) ) ;
#35108 = CARTESIAN_POINT ( 'NONE',  ( -6.089547271193396227, 7.133501900260939443, -1.199719254218453823 ) ) ;
#35109 = CARTESIAN_POINT ( 'NONE',  ( 3.784388871581423786, -0.6371526190629381858, -1.913262240507591416 ) ) ;
#35110 = CARTESIAN_POINT ( 'NONE',  ( -8.154339323615371171, 11.60081407993821045, 1.199719254218453823 ) ) ;
#35112 = CARTESIAN_POINT ( 'NONE',  ( 11.04536101718726293, 10.19999999999999929, -1.100000000000000311 ) ) ;
#35111 = CARTESIAN_POINT ( 'NONE',  ( -9.490344339885973923, 12.09515436799890331, -1.443375672974059665 ) ) ;
#35114 = CARTESIAN_POINT ( 'NONE',  ( 0.07933194154487524519, -7.473374494045017968, -9.499668754385622194 ) ) ;
#35113 = CARTESIAN_POINT ( 'NONE',  ( 5.172814640947125397, -2.034155943344346795, -0.7319064324283753864 ) ) ;
#35115 = CARTESIAN_POINT ( 'NONE',  ( -11.89197369110779867, 11.30000000000000071, 0.8056055387119849254 ) ) ;
#35116 = CARTESIAN_POINT ( 'NONE',  ( -7.097136523687877840, -8.233137084989836652, 6.434831245971847302 ) ) ;
#35118 = CARTESIAN_POINT ( 'NONE',  ( 6.028922772295511656, -1.701938481575874684, 1.081082441910637071 ) ) ;
#35117 = CARTESIAN_POINT ( 'NONE',  ( -8.175203438916030407, 8.640084888264587093, 0.7216878364870578100 ) ) ;
#35119 = CARTESIAN_POINT ( 'NONE',  ( -0.7499999999999972244, 5.858333333333353821, -1.299038105676652011 ) ) ;
#35120 = CARTESIAN_POINT ( 'NONE',  ( 0.9258787065367773961, 1.030881334376580805, -1.382772916119678897 ) ) ;
#35121 = CARTESIAN_POINT ( 'NONE',  ( 5.845500506147374153, 6.848780674373954547, 1.199719254218453823 ) ) ;
#35123 = CARTESIAN_POINT ( 'NONE',  ( 7.856023664475727308, 8.130058794835305136, -0.7998128361456341429 ) ) ;
#35122 = CARTESIAN_POINT ( 'NONE',  ( 7.104109303880752790, 11.23195192126214970, -0.7216878364870267237 ) ) ;
#35124 = CARTESIAN_POINT ( 'NONE',  ( -4.218512253981381299, 3.978430757497701364, -0.5307291018261834914 ) ) ;
#35125 = CARTESIAN_POINT ( 'NONE',  ( 5.290257391050456448, -1.856285702826396156, -0.2301478561287788605 ) ) ;
#35126 = CARTESIAN_POINT ( 'NONE',  ( 6.275645410888611941, 0.3399709936107355168, -1.984134265935801000 ) ) ;
#35127 = CARTESIAN_POINT ( 'NONE',  ( 6.539320575229256249, 2.979067782826944288, 2.350490835693247682 ) ) ;
#35128 = AXIS2_PLACEMENT_3D ( 'NONE', #208849, #107174, #158014 ) ;
#35129 = CARTESIAN_POINT ( 'NONE',  ( -7.255021596644144921, 7.636815748939187465, 0.7216878364870317197 ) ) ;
#35130 = VERTEX_POINT ( 'NONE', #108475 ) ;
#35131 = COLOUR_RGB ( '', 0.09019608, 0.27058824, 0.51372549) ;
#35133 = CARTESIAN_POINT ( 'NONE',  ( 2.319935610374638468, 0.9480221781073931986, -1.779637559903464394 ) ) ;
#35132 = CARTESIAN_POINT ( 'NONE',  ( 2.157031413788193852, 0.4673396547767159070, 2.068183735011968061 ) ) ;
#35134 = CARTESIAN_POINT ( 'NONE',  ( 5.905458427204159477, 9.047396044116986502, 1.199719254218452047 ) ) ;
#35135 = CARTESIAN_POINT ( 'NONE',  ( 6.086834708314957432, -0.3123483334277510348, -2.138898144987111838 ) ) ;
#35136 = CARTESIAN_POINT ( 'NONE',  ( 6.588372581236919601, 9.773852880496709972, -1.199719254218440723 ) ) ;
#35138 = CARTESIAN_POINT ( 'NONE',  ( 0.6553225869628921396, 1.845336034500634437, -0.5141059209906836402 ) ) ;
#35137 = CARTESIAN_POINT ( 'NONE',  ( -4.381256195510448315, 8.263215994737505454, 1.040834085586084257E-14 ) ) ;
#35139 = CARTESIAN_POINT ( 'NONE',  ( -1.420000000000021911, 6.280000000000042881, 2.580000000000011173 ) ) ;
#35140 = FACE_OUTER_BOUND ( 'NONE', #66571, .T. ) ;
#35141 = CARTESIAN_POINT ( 'NONE',  ( 6.941411460072420603, 7.200660912947041581, 1.040834085586084257E-14 ) ) ;
#35142 = CARTESIAN_POINT ( 'NONE',  ( -0.6823417656250246877, -0.3864583329919110688, 1.181850606188755259 ) ) ;
#35143 = CARTESIAN_POINT ( 'NONE',  ( 3.714570900464285064, 4.396382807705524698, 1.082531754730560403 ) ) ;
#35144 = CARTESIAN_POINT ( 'NONE',  ( -8.611400122974211868, 13.19838391011195888, 1.040834085586084257E-14 ) ) ;
#35145 = CARTESIAN_POINT ( 'NONE',  ( 4.065412822539622439, 0.2671453805177248508, -2.145074402785766665 ) ) ;
#35146 = CARTESIAN_POINT ( 'NONE',  ( -6.468648687495877958, 6.719380688266201496, 0.000000000000000000 ) ) ;
#35147 = EDGE_CURVE ( 'NONE', #197638, #75373, #158811, .T. ) ;
#35148 = CARTESIAN_POINT ( 'NONE',  ( 4.895902868310594513, 8.725987423088758632, 0.000000000000000000 ) ) ;
#35149 = CARTESIAN_POINT ( 'NONE',  ( 1.687894460584405731, 2.027760172737497424, -0.6205009303206151516 ) ) ;
#35150 = CARTESIAN_POINT ( 'NONE',  ( 6.827182134110198142, 0.003888933837258023996, 1.810856214465889069 ) ) ;
#35151 = CARTESIAN_POINT ( 'NONE',  ( 2.688696339244216915, -0.3334303690454739066, -1.942799078106532074 ) ) ;
#35152 = CARTESIAN_POINT ( 'NONE',  ( 4.552931727387078631, 0.3324577288378940954, 1.883125075537089854 ) ) ;
#35153 = VERTEX_POINT ( 'NONE', #27144 ) ;
#35154 = CARTESIAN_POINT ( 'NONE',  ( -5.653072611647089601E-16, -1.229881656804728163, -7.771561172376095783E-15 ) ) ;
#35155 = CARTESIAN_POINT ( 'NONE',  ( 6.039503384146654774, 1.820429283694004141, -0.7522724601281975954 ) ) ;
#35156 = CARTESIAN_POINT ( 'NONE',  ( 1.341630539043844106, 1.939701883965805562, 0.09577479888067677583 ) ) ;
#35157 = ORIENTED_EDGE ( 'NONE', *, *, #154124, .F. ) ;
#35158 = CARTESIAN_POINT ( 'NONE',  ( -5.632486471834530661, 5.535932070087196344, -0.7998128361456362523 ) ) ;
#35160 = LINE ( 'NONE', #39444, #186151 ) ;
#35159 = CARTESIAN_POINT ( 'NONE',  ( -4.981695098378565945, 4.776675467721892332, -0.7998128361456362523 ) ) ;
#35161 = CARTESIAN_POINT ( 'NONE',  ( 6.795661308947685164, 8.951357498570873261, -1.599625672291262513 ) ) ;
#35163 = CARTESIAN_POINT ( 'NONE',  ( 4.814553946184248368, 7.670711132973337065, -1.082531754730548412 ) ) ;
#35162 = CARTESIAN_POINT ( 'NONE',  ( 6.958359152311676787, 9.141171649162195934, -1.599625672291262513 ) ) ;
#35165 = EDGE_LOOP ( 'NONE', ( #60632, #106617, #172327, #38721 ) ) ;
#35164 = CARTESIAN_POINT ( 'NONE',  ( 5.883449979803576646, 0.1360998956825946737, -1.907488392096804874 ) ) ;
#35166 = CARTESIAN_POINT ( 'NONE',  ( 3.492985898914053866, -0.4302566696539159574, -2.164365734511737305 ) ) ;
#35167 = CARTESIAN_POINT ( 'NONE',  ( 1.641937377912294771, -1.598774535768614280, -1.521335986861327427 ) ) ;
#35168 = DIRECTION ( 'NONE',  ( 0.000000000000000000, 0.000000000000000000, 1.000000000000000000 ) ) ;
#35169 = CARTESIAN_POINT ( 'NONE',  ( 0.2406774923011632261, 1.829974501424940891, 0.5550298453492612527 ) ) ;
#35170 = DIRECTION ( 'NONE',  ( -0.000000000000000000, 1.000000000000000000, -0.000000000000000000 ) ) ;
#35171 = CARTESIAN_POINT ( 'NONE',  ( -0.4421172008954280530, 6.952755576498319989, 3.903674101997708146 ) ) ;
#35172 = CARTESIAN_POINT ( 'NONE',  ( 3.262232429473245432, -2.068111870375147987, 0.09887451149894616043 ) ) ;
#35173 = CARTESIAN_POINT ( 'NONE',  ( -5.575427483717760424, 7.527751369135936343, 1.599625672291269396 ) ) ;
#35174 = CARTESIAN_POINT ( 'NONE',  ( -5.911423380092099222, 7.159701334921778404, 1.127351979631958434 ) ) ;
#35176 = CARTESIAN_POINT ( 'NONE',  ( 1.411231610350563992, 1.906656261001705488, 1.018656936289302539 ) ) ;
#35175 = CARTESIAN_POINT ( 'NONE',  ( -3.632695093457760649, 6.325562478087638496, -1.199719254218452047 ) ) ;
#35177 = CARTESIAN_POINT ( 'NONE',  ( 3.861010967126535576, 0.2669419790740577558, -2.175157288012785184 ) ) ;
#35178 = CARTESIAN_POINT ( 'NONE',  ( -0.6125000000000089262, 0.7083333333333317050, -1.060881119635948444 ) ) ;
#35179 = CARTESIAN_POINT ( 'NONE',  ( 2.929970594329034395, 6.432399770110250437, -0.7216878364870338292 ) ) ;
#35180 = CARTESIAN_POINT ( 'NONE',  ( 1.387358672530662584, 7.251968950356647348, 4.302625267142138554 ) ) ;
#35181 = CARTESIAN_POINT ( 'NONE',  ( -1.364683531250010295, 14.94270833367472839, 0.7879004041258445001 ) ) ;
#35182 = CARTESIAN_POINT ( 'NONE',  ( -6.330731382938325602, 6.350551133041632212, 0.7998128361456281477 ) ) ;
#35183 = PRODUCT_DEFINITION_CONTEXT ( 'detailed design', #51947, 'design' ) ;
#35184 = CARTESIAN_POINT ( 'NONE',  ( 6.363864384548370445, -0.09514871459133207587, -1.731698918886691363 ) ) ;
#35185 = CARTESIAN_POINT ( 'NONE',  ( -2.764973262183167968, 5.313220341600567664, 1.199719254218462483 ) ) ;
#35186 = CARTESIAN_POINT ( 'NONE',  ( 3.959880360806608213, -0.6057208360459276353, 1.979630382156400303 ) ) ;
#35187 = CARTESIAN_POINT ( 'NONE',  ( 4.482099252480286289, -2.116778089722763045, -0.05043497882678028149 ) ) ;
#35188 = CARTESIAN_POINT ( 'NONE',  ( 7.149227073107712549, 7.235186428247455837, -0.7998128361456281477 ) ) ;
#35190 = EDGE_CURVE ( 'NONE', #140850, #37159, #13800, .T. ) ;
#35189 = CARTESIAN_POINT ( 'NONE',  ( 0.6823417656249917140, 4.592708333674755394, 1.181850606188765695 ) ) ;
#35191 = CARTESIAN_POINT ( 'NONE',  ( 2.975404341296074229, -0.1976578167360588389, 1.959527558586687146 ) ) ;
#35192 = CARTESIAN_POINT ( 'NONE',  ( 0.3692113334803036606, -1.616751421056546789, -1.021125667832627260 ) ) ;
#35193 = CARTESIAN_POINT ( 'NONE',  ( 4.277453538519633724, 1.495592673709666531, 1.737217383791799463 ) ) ;
#35194 = CARTESIAN_POINT ( 'NONE',  ( 2.842213963582499670, 1.811911227886909614, 0.2232855069103783507 ) ) ;
#35195 = EDGE_CURVE ( 'NONE', #201878, #212450, #109408, .T. ) ;
#35196 = CARTESIAN_POINT ( 'NONE',  ( 4.913904330310220558, 4.697586238308844919, 0.000000000000000000 ) ) ;
#35197 = CARTESIAN_POINT ( 'NONE',  ( 4.622967192135525316, 8.337286124226029216, -0.7216878364870207285 ) ) ;
#35198 = CARTESIAN_POINT ( 'NONE',  ( -6.008234629150358330, 10.16135750065076060, 0.000000000000000000 ) ) ;
#35199 = ORIENTED_EDGE ( 'NONE', *, *, #137619, .F. ) ;
#35200 = CARTESIAN_POINT ( 'NONE',  ( 3.480730050573742851, -1.348849006198136635, 1.494714382889005488 ) ) ;
#35201 = CARTESIAN_POINT ( 'NONE',  ( 4.012515129279304205, 0.7020173944642660313, 1.832041770129029468 ) ) ;
#35202 = CARTESIAN_POINT ( 'NONE',  ( -7.182068686937172153, 9.402166106225269715, 1.599625672291283607 ) ) ;
#35203 = CARTESIAN_POINT ( 'NONE',  ( -5.738125327081750271, 7.717565519727259904, 1.599625672291269396 ) ) ;
#35204 = CARTESIAN_POINT ( 'NONE',  ( 0.1755611466353446948, 4.081716065625639267, -2.798746370182193743 ) ) ;
#35206 = CARTESIAN_POINT ( 'NONE',  ( 5.910986595158141732, 1.562736066445655769, 0.8308124446602130897 ) ) ;
#35205 = CARTESIAN_POINT ( 'NONE',  ( 0.3629773032866591143, 0.2007434131479734207, -2.081070348792604108 ) ) ;
#35207 = DIRECTION ( 'NONE',  ( 0.000000000000000000, 0.000000000000000000, 1.000000000000000000 ) ) ;
#35208 = B_SPLINE_CURVE_WITH_KNOTS ( 'NONE', 3,
 ( #35150, #86050, #1568, #135879, #116479, #100169, #50357, #152127, #31987, #17824, #83907, #49306, #149997, #98065, #33041, #213889, #167309, #67630, #133775, #65511, #148923, #199783, #99119, #165168, #496, #84980, #151072, #2634, #23160, #122922, #25311, #39435, #189948, #204032, #138017, #21018, #205114, #202977, #206190, #54618, #56758, #41597, #188880, #72984, #136952, #169433, #9069, #55680, #6907, #121836, #105528, #88190, #22078, #40521, #104446, #107708, #139087, #87115, #170494, #103371, #70835, #89274, #53551, #155323, #156399, #187808, #171562, #106624, #119682, #154263, #7985, #153185, #5837, #157473, #201899, #71908, #24228, #91413, #172653, #90330, #4759, #75143, #120766, #185669, #74074, #37298, #140168, #57818, #123980, #173734, #186744, #38366, #128258, #127183, #195301, #158528, #46931, #161742, #210460, #194220, #129324, #143380, #160662, #77267, #44802, #27447, #175859, #62098, #43729, #113049, #12258, #108775, #109844, #42666, #10125, #45865, #110906, #174800, #13333, #162807, #93545, #209379, #207261, #159589, #79407, #26376, #11188, #96757, #141253, #61023, #177989, #30674, #193151, #176912, #92490, #14384, #58890, #76200, #125045, #28527, #179055, #208320, #59950, #145524, #142310, #191000, #29602, #126106, #95688, #192066, #144457, #63159, #94618, #78335, #111986, #211524, #98869, #168126, #134594, #165991, #65267, #114123, #102061, #18657, #80477, #50114, #17576, #149750, #48005, #196365, #167065, #163876, #130375, #49054, #116235, #180115, #132467, #146575, #184358, #68467, #251, #33848, #212594, #148683, #66323, #164921, #84737, #64232, #198469, #16514, #81540, #182225, #200595, #15452, #31739, #133528, #99929, #83660, #97812, #181169, #52242, #100976, #150825, #147622, #1327, #2388, #118370, #67388, #199536, #35980, #51178, #213641, #82597, #117301, #131413, #183298, #197413, #115174, #32795, #34904, #106377, #202729, #203793, #201658, #71661, #107460, #123737, #7736, #154015, #137775, #55439, #70590, #90091, #54381, #120519, #6667, #19727, #135637, #21833, #121591, #204857, #169186, #185426, #72743, #5581, #187564, #69530, #186497, #139917, #104202, #103128, #122673, #85806, #152941, #23989, #151887, #37044, #20779, #53307, #39190, #86874, #170248, #119439, #22911, #4517, #156155, #136705, #89027, #38128, #205947, #40266, #155080, #138841, #73822, #87941, #105279, #57579, #56513, #189698, #171316, #188636, #172401, #41351, #3460, #141004, #75957, #74895, #42419, #78085, #143137, #207011, #45610, #195038, #59700, #129066, #193962, #9882, #160408, #8820, #128009, #93302, #173486, #142060, #210205, #62896, #191819, #208074, #58642, #46672, #25063, #124795, #91165, #125862, #211273, #159338, #43484, #10934, #175608, #190756, #95441, #12011, #111725, #13070, #176661, #161491, #109602, #158291, #92242, #27196, #77010, #157221, #79149, #44545, #209132, #60770, #126930, #108524, #174553, #192887, #26129, #110660, #28274, #94366, #177733, #144209, #61841, #29346, #145265, #163619, #114914, #66063, #180912, #32536, #199275, #100726, #178804, #148431, #149485, #212332, #47751, #113866, #98610, #16254, #7289, #15199, #183040, #81290, #147367, #99666, #200338, #14125, #164671, #132206, #83403, #115977, #196114, #179861, #34656, #150565, #198214, #31485, #82339, #133266, #166805, #63970, #49849, #117044 ),
 .UNSPECIFIED., .F., .F.,
 ( 4, 1, 1, 1, 1, 1, 1, 1, 1, 1, 1, 1, 1, 1, 1, 1, 1, 1, 1, 1, 1, 1, 1, 1, 1, 1, 1, 1, 1, 1, 1, 1, 1, 1, 1, 1, 1, 1, 1, 1, 1, 1, 1, 1, 1, 1, 1, 1, 1, 1, 1, 1, 1, 1, 1, 1, 1, 1, 1, 1, 1, 1, 1, 1, 1, 1, 1, 1, 1, 1, 1, 1, 1, 1, 1, 1, 1, 1, 1, 1, 1, 1, 1, 1, 1, 1, 1, 1, 1, 1, 1, 1, 1, 1, 1, 1, 1, 1, 1, 1, 1, 1, 1, 1, 1, 1, 1, 1, 1, 1, 1, 1, 1, 1, 1, 1, 1, 1, 1, 1, 1, 1, 1, 1, 1, 1, 1, 1, 1, 1, 1, 1, 1, 1, 1, 1, 1, 1, 1, 1, 1, 1, 1, 1, 1, 1, 1, 1, 1, 1, 1, 1, 1, 1, 1, 1, 1, 1, 1, 1, 1, 1, 1, 1, 1, 1, 1, 1, 1, 1, 1, 1, 1, 1, 1, 1, 1, 1, 1, 1, 1, 1, 1, 1, 1, 1, 1, 1, 1, 1, 1, 1, 1, 1, 1, 1, 1, 1, 1, 1, 1, 1, 1, 1, 1, 1, 1, 1, 1, 1, 1, 1, 1, 1, 1, 1, 1, 1, 1, 1, 1, 1, 1, 1, 1, 1, 1, 1, 1, 1, 1, 1, 1, 1, 1, 1, 1, 1, 1, 1, 1, 1, 1, 1, 1, 1, 1, 1, 1, 1, 1, 1, 1, 1, 1, 1, 1, 1, 1, 1, 1, 1, 1, 1, 1, 1, 1, 1, 1, 1, 1, 1, 1, 1, 1, 1, 1, 1, 1, 1, 1, 1, 1, 1, 1, 1, 1, 1, 1, 1, 1, 1, 1, 1, 1, 1, 1, 1, 1, 1, 1, 1, 1, 1, 1, 1, 1, 1, 1, 1, 1, 1, 1, 1, 1, 1, 1, 1, 1, 1, 1, 1, 1, 1, 1, 1, 1, 1, 1, 1, 1, 1, 1, 1, 1, 1, 1, 1, 1, 1, 1, 1, 1, 1, 1, 1, 1, 1, 1, 1, 1, 1, 1, 1, 1, 1, 1, 1, 1, 1, 1, 1, 1, 1, 1, 1, 1, 1, 1, 1, 1, 1, 1, 1, 1, 1, 1, 1, 1, 1, 1, 1, 1, 1, 4 ),
 ( 0.000000000000000000, 0.002600214693118923798, 0.005208871813129847643, 0.007813341859462101871, 0.01041561011214237054, 0.01302159838915000617, 0.01562452542669844589, 0.01822945805747129902, 0.02083332260852943998, 0.02343713088342555886, 0.02604210653276634729, 0.02864513693292065552, 0.03125071383394792401, 0.03385356881896259273, 0.03645895053148855841, 0.03906228851054763251, 0.04166670673482164577, 0.04427111720854654681, 0.04687446234244373178, 0.04947983976256019323, 0.05208269766733494843, 0.05468827385445936690, 0.05729129101459448647, 0.05989628262864687969, 0.06250008845252298662, 0.06510390268380349121, 0.06770888856031336001, 0.07031191025079500112, 0.07291748459129859805, 0.07552033970978830335, 0.07812571920045624507, 0.08072905536012038585, 0.08333347174482363950, 0.08593788071299547637, 0.08854122383090638759, 0.09114659965375219997, 0.09374945576594469199, 0.09635503022752239799, 0.09895804583665256116, 0.1015630356028039000, 0.1041668400134527495, 0.1067706523020897913, 0.1093756367037285043, 0.1119786565701353653, 0.1145842293264338063, 0.1171870828570002881, 0.1197924606432616973, 0.1223957954228293843, 0.1250002099740243899, 0.1276046175975352470, 0.1302079588893767237, 0.1328133332639841735, 0.1354161877457908392, 0.1380217606440506395, 0.1406247748629219918, 0.1432297629411592166, 0.1458335661004374617, 0.1484373766077259071, 0.1510423596945167368, 0.1536453778991425101, 0.1562509492307036785, 0.1588538013357113088, 0.1614591775772540871, 0.1640625111385781432, 0.1666669240170048083, 0.1692713304565471311, 0.1718746700842041231, 0.1744800431702197008, 0.1770828961840006377, 0.1796884676783837009, 0.1822914806691622869, 0.1848964672195632097, 0.1875002692887918765, 0.1901040781760970355, 0.1927090601080766463, 0.1953120768130981733, 0.1979176468793322763, 0.2005204977210985895, 0.2031258725775486607, 0.2057292050824250096, 0.2083336164487647746, 0.2109380218649763994, 0.2135413599902747928, 0.2161467319472901716, 0.2187495836553486062, 0.2213551539052408534, 0.2239581658300387468, 0.2265631510126252801, 0.2291669521530730058, 0.2317707595817034838, 0.2343757405188569010, 0.2369787558863956922, 0.2395843248466610342, 0.2421871745874512594, 0.2447925482183819501, 0.2473958798285567084, 0.2500002898434375842, 0.2526046943969075254, 0.2552080311816201097, 0.2578134021691782518, 0.2604162527337665622, 0.2630218218985046486, 0.2656248329193858781, 0.2682298168941298910, 0.2708336172670197106, 0.2734374233982336255, 0.2760424035005001331, 0.2786454176926287940, 0.2812509857062375773, 0.2838538345082703418, 0.2864592070732082663, 0.2890625379503836689, 0.2916669467743862043, 0.2942713506256608436, 0.2968746862315132518, 0.2994800564091141259, 0.3020829059924399762, 0.3046884742313171190, 0.3072914845103039694, 0.3098964674371332273, 0.3125002672036480411, 0.3151040721986592130, 0.3177090516259382103, 0.3203120648046862140, 0.3229176320309106729, 0.3255204800563645251, 0.3281258517147956355, 0.3307291820206363919, 0.3333335898142997245, 0.3359379931238887229, 0.3385413277125659537, 0.3411466972396727249, 0.3437495460039050044, 0.3463551134761772565, 0.3489581231752558743, 0.3515631052140602009, 0.3541669045353489920, 0.3567707085553323276, 0.3593756874674896018, 0.3619786997948497009, 0.3645842663929277916, 0.3671871138039469185, 0.3697924847153226668, 0.3723958146114617063, 0.3750002215352895019, 0.3776046244636719340, 0.3802079581968237365, 0.3828133272328684833, 0.3854161753401436075, 0.3880217422050354359, 0.3906247514861621029, 0.3932297327967993472, 0.3958335318339832876, 0.3984373350400814418, 0.4010423135969549691, 0.4036453252348887744, 0.4062508913640303643, 0.4088537383227308641, 0.4114591086464738368, 0.4140624382945181647, 0.4166668445089845574, 0.4192712472166146842, 0.4218745802558619973, 0.4244799489602520959, 0.4270827965726798348, 0.4296883629893904488, 0.4322913720144979099, 0.4348963527567997200, 0.4375001516709778882, 0.4401039542243071478, 0.4427089325857130886, 0.4453119436961573974, 0.4479175095155500941, 0.4505203561840259718, 0.4531257260795358843, 0.4557290556410732441, 0.4583334613066292196, 0.4609378639539425948, 0.4635411964608836533, 0.4661465649930071620, 0.4687494122726767465, 0.4713549784003855381, 0.4739579873313886638, 0.4765629676651664814, 0.4791667666174222462, 0.4817705686790782482, 0.4843755470048167200, 0.4869785577496898998, 0.4895841234185048796, 0.4921869699588339309, 0.4947923395854939010, 0.4973956692220981579, 0.5000000744991768276, 0.5026044772465965149, 0.5052078093828125116, 0.5078131779020444991, 0.5104160250110306718, 0.5130215910089035436, 0.5156246000077054914, 0.5182295800927568807, 0.5208333792441637300, 0.5234371809752277338, 0.5260421594250891397, 0.5286451699662961801, 0.5312507356436946271, 0.5338535822179446555, 0.5364589517351265879, 0.5390622816083643354, 0.5416666866573878192, 0.5442710896653298880, 0.5468744215923915242, 0.5494797902580997873, 0.5520826373584690749, 0.5546882033856646022, 0.5572912126141627009, 0.5598961926102767883, 0.5624999921219043797, 0.5651037936834493181, 0.5677087724172201755, 0.5703117829166597375, 0.5729173487617980065, 0.5755201955320329299, 0.5781255650991041772, 0.5807288953705399548, 0.5833333003519244331, 0.5859377037808047861, 0.5885410356602774895, 0.5911464046318289922, 0.5937492518856454238, 0.5963548181013198501, 0.5989578277214122615, 0.6015628077883760083, 0.6041666078212959423, 0.6067704093743923055, 0.6093753885518610192, 0.6119783991714310423, 0.6145839653434672645, 0.6171868124717531101, 0.6197921822480817466, 0.6223955130792849788, 0.6249999181534476866, 0.6276043221636865566, 0.6302076541571374202, 0.6328130235939036785, 0.6354158711632348355, 0.6380214377265494008, 0.6406244479001403924, 0.6432294281977445349, 0.6458332289130368498, 0.6484370306187589028, 0.6510420103997216490, 0.6536450213013255128, 0.6562505879594253688, 0.6588534356078361576, 0.6614588057527972520, 0.6640621373053481324, 0.6666665426327121891, 0.6692709473847417989, 0.6718742796537453543, 0.6744796497151083203, 0.6770824977620315543, 0.6796880648321572682, 0.6822910757211636534, 0.6848960564092084757, 0.6874998579679674204, 0.6901036599873985322, 0.6927086405316660311, 0.6953116518772185506, 0.6979172191805607106, 0.7005200675111846742, 0.7031254381841663958, 0.7057287706196612165, 0.7083331763606625087, 0.7109375820149322900, 0.7135409147210758363, 0.7161462855664346705, 0.7187491342530435423, 0.7213547019891674017, 0.7239577137555243125, 0.7265626949938263079, 0.7291664975571658935, 0.7317703000514055311, 0.7343752815188082650, 0.7369782934702413524, 0.7395838615780243597, 0.7421867107529701579, 0.7447920821133793279, 0.7473954155934371402, 0.7499998219085300954, 0.7526042286255122393, 0.7552075619304030596, 0.7578129337191791270, 0.7604157832075884027, 0.7630213517689198310, 0.7656243645745874904, 0.7682293465229839136, 0.7708331502520449074, 0.7734369533822141873, 0.7760419359326080624, 0.7786449486518774998, 0.7812505177233250997, 0.7838533679047272607, 0.7864587401119955690, 0.7890620747982641792, 0.7916664818479275390, 0.7942708897881238794, 0.7968742238533942368, 0.7994795967450375462, 0.8020824471973901915, 0.8046880167431663677, 0.8072910307501349747, 0.8098960135684915018, 0.8124998186244467568, 0.8151036225516941069, 0.8177086063449673370, 0.8203116199940584385, 0.8229171901884252405, 0.8255200415384508217, 0.8281254147520410447, 0.8307287508062024539, 0.8333331587509454907, 0.8359375680748931670, 0.8385409030622068549, 0.8411462772162020540, 0.8437491287946751184, 0.8463546994841673055, 0.8489577148544642515, 0.8515626987026798655, 0.8541665052467400931, 0.8567703101322480252, 0.8593752953283267937, 0.8619783100692604005, 0.8645838815458386506, 0.8671867342266933454, 0.8697921086061042306, 0.8723954461898817403, 0.8749998551902504751, 0.8776042660585271493, 0.8802076021295854868, 0.8828129777054576355, 0.8854158305722678035, 0.8880214025647872322, 0.8906244194604823194, 0.8932294044984951942, 0.8958332126919159588, 0.8984370186969063976, 0.9010420054557602976, 0.9036450214505988843, 0.9062505943687239052, 0.9088534485426573717, 0.9114588242474312985, 0.9140621635225948394, 0.9166665737391771485, 0.9192709863124074454, 0.9218743236289563825, 0.9244797007862803895, 0.9270825551036790957, 0.9296881285585824051, 0.9322911471418501295, 0.9348961335295734587, 0.9374999435335269471, 0.9401037508197458425, 0.9427087393012421046, 0.9453117567106092967, 0.9479173312323898593, 0.9505201870615167525, 0.9531255642405720430, 0.9557289053967781278, 0.9583333169903581750, 0.9609377312744702415, 0.9635410702737328137, 0.9661464495301401723, 0.9687493035862174695, 0.9713548794777306927, 0.9739579066090123804, 0.9765628826531806972, 0.9791666865793459129, 0.9817705523293528413, 0.9843754818126480011, 0.9869784094881522973, 0.9895843956701340094, 0.9921866610829068733, 0.9947911313000845634, 0.9973997837621362272, 1.000000000000000000 ),
 .UNSPECIFIED. ) ;
#35209 = CARTESIAN_POINT ( 'NONE',  ( 1.869323357045350686, 2.096458975851514861, -0.6381942758529115522 ) ) ;
#35210 = CARTESIAN_POINT ( 'NONE',  ( 0.3095773630682343569, 1.202386210327820004, -1.258585571321766627 ) ) ;
#35211 = COLOUR_RGB ( '', 0.09019608, 0.27058824, 0.51372549) ;
#35212 = CARTESIAN_POINT ( 'NONE',  ( 6.262976894508937242, 9.394224579314053969, -1.199719254218440723 ) ) ;
#35213 = CARTESIAN_POINT ( 'NONE',  ( 0.2331713839410941569, 0.7381306520543399197, -2.038767774274966360 ) ) ;
#35214 = CARTESIAN_POINT ( 'NONE',  ( 0.2227383504175127205, -0.09031333296150539924, 1.722639462886750517 ) ) ;
#35215 = CARTESIAN_POINT ( 'NONE',  ( 1.195116192591906046, -1.458952948520657156, -1.775991855458454838 ) ) ;
#35216 = CARTESIAN_POINT ( 'NONE',  ( 0.4159077360078728969, -1.177411712353953588, -1.848246096435968600 ) ) ;
#35217 = CARTESIAN_POINT ( 'NONE',  ( 2.825073394047578734, 2.078234123670623212, 0.7428476018367863309 ) ) ;
#35218 = ADVANCED_FACE ( 'NONE', ( #144156 ), #51153, .T. ) ;
#35219 = CARTESIAN_POINT ( 'NONE',  ( 6.637192348400761333, -0.09982221633967082453, -2.168999452382541993 ) ) ;
#35220 = CARTESIAN_POINT ( 'NONE',  ( 0.000000000000000000, 3.900000000000000799, 0.000000000000000000 ) ) ;
#35221 = CARTESIAN_POINT ( 'NONE',  ( 2.290374991995058895, -0.8151648431981967091, -1.954327666539334762 ) ) ;
#35222 = CARTESIAN_POINT ( 'NONE',  ( 6.727182134110201162, 1.237345558575110083, 2.302850971298702198 ) ) ;
#35223 = CARTESIAN_POINT ( 'NONE',  ( 5.192375284248013756, -1.911820684568351192, -0.2360692857661383648 ) ) ;
#35224 = ORIENTED_EDGE ( 'NONE', *, *, #143273, .F. ) ;
#35226 = CARTESIAN_POINT ( 'NONE',  ( -1.364683531250000748, -1.178124999658580752, 0.000000000000000000 ) ) ;
#35225 = CARTESIAN_POINT ( 'NONE',  ( 2.788958495631514545, 1.964664059585927491, -1.180940832111162520 ) ) ;
#35227 = CARTESIAN_POINT ( 'NONE',  ( 3.388648328411762556, 6.040841252200647382, 1.199719254218462483 ) ) ;
#35228 = CARTESIAN_POINT ( 'NONE',  ( 5.331380718671758778, 7.243030143248949670, -1.599625672291256295 ) ) ;
#35229 = CIRCLE ( 'NONE', #59054, 0.08000000000000040412 ) ;
#35230 = CARTESIAN_POINT ( 'NONE',  ( 4.301594116137519741, 1.984124119141786657, -0.9988866673766303439 ) ) ;
#35231 = CARTESIAN_POINT ( 'NONE',  ( -8.527715433315703919, 9.051348881730875817, 1.040834085586084257E-14 ) ) ;
#35232 = CARTESIAN_POINT ( 'NONE',  ( 7.065207446497155708, 9.336104335703744539, 0.000000000000000000 ) ) ;
#35233 = CARTESIAN_POINT ( 'NONE',  ( 4.528060117284222308, 8.226561203566173930, 0.7216878364870438212 ) ) ;
#35234 = CARTESIAN_POINT ( 'NONE',  ( -6.656690234185426824, 10.70996300661758660, 0.7216878364870458196 ) ) ;
#35235 = CARTESIAN_POINT ( 'NONE',  ( 6.536439455564168277, 6.798469917679251573, 0.7216878364870328300 ) ) ;
#35236 = ORIENTED_EDGE ( 'NONE', *, *, #84119, .F. ) ;
#35237 = CARTESIAN_POINT ( 'NONE',  ( 3.041638857185970046, -1.525043868314728934, 1.319228477497782714 ) ) ;
#35239 = CARTESIAN_POINT ( 'NONE',  ( 0.7606827552629210620, -0.6912373536034731591, -1.943445369992405025 ) ) ;
#35238 = CARTESIAN_POINT ( 'NONE',  ( 6.252281394196331554, 10.44607872653774372, 1.040834085586084257E-14 ) ) ;
#35240 = CARTESIAN_POINT ( 'NONE',  ( -11.78331023100045449, 13.79999999999998295, 1.799999999999999600 ) ) ;
#35241 = CARTESIAN_POINT ( 'NONE',  ( 6.333067150914816423, 7.521571443223021625, 1.082531754730549967 ) ) ;
#35242 = CARTESIAN_POINT ( 'NONE',  ( -11.00595142344305444, 13.60990418661507739, -1.443824005414911182 ) ) ;
#35243 = CARTESIAN_POINT ( 'NONE',  ( -0.6823417656250212460, 3.051041667008084879, 1.181850606188767472 ) ) ;
#35244 = CARTESIAN_POINT ( 'NONE',  ( 4.101666331917613206, -2.185647184384610586, 0.1603006067264350909 ) ) ;
#35245 = CARTESIAN_POINT ( 'NONE',  ( 0.9322677863709986079, -1.591319861332978425, -1.238319039483272599 ) ) ;
#35246 = CARTESIAN_POINT ( 'NONE',  ( 1.171164436615620863, 1.096940724416964885, 1.478650282607060662 ) ) ;
#35247 = CARTESIAN_POINT ( 'NONE',  ( 4.739906352223059116, 2.286097037578460611, 0.1700548269078107355 ) ) ;
#35248 = CARTESIAN_POINT ( 'NONE',  ( 2.993917163610838816, -0.5349900852187582379, -1.761688665035024304 ) ) ;
#35249 = CARTESIAN_POINT ( 'NONE',  ( 8.503988664269582998, 10.94440607977979063, 1.599625672291281386 ) ) ;
#35250 = CARTESIAN_POINT ( 'NONE',  ( 3.891465932158610030, 1.322013910284997262, 1.259209046625270556 ) ) ;
#35251 = CARTESIAN_POINT ( 'NONE',  ( 5.361953999179126740, -0.05229508359532940298, -2.015913028294749942 ) ) ;
#35252 = CARTESIAN_POINT ( 'NONE',  ( -8.962103233833181193, 10.41454084668224489, -1.199719254218446718 ) ) ;
#35254 = DIRECTION ( 'NONE',  ( 0.000000000000000000, 0.000000000000000000, 1.000000000000000000 ) ) ;
#35253 = CARTESIAN_POINT ( 'NONE',  ( 4.891644337148946420, 1.673267685831375307, 1.523052275532793320 ) ) ;
#35255 = CARTESIAN_POINT ( 'NONE',  ( 6.211965580189116487, -2.090513352778848422, 0.2539706045930691380 ) ) ;
#35256 = CARTESIAN_POINT ( 'NONE',  ( -1.981451431469474223, 3.479816182765814059, -0.4617787996151642149 ) ) ;
#35257 = CARTESIAN_POINT ( 'NONE',  ( 4.000488093070094564, 2.060113009926473726, 0.2059288336104248551 ) ) ;
#35258 = CARTESIAN_POINT ( 'NONE',  ( 8.543609354905870035, 13.11929468069890525, 0.7998128361456462443 ) ) ;
#35259 = CARTESIAN_POINT ( 'NONE',  ( -1.360316468750048635, 1.942708333674827204, 0.7853790794158580502 ) ) ;
#35260 = SHAPE_DEFINITION_REPRESENTATION ( #145815, #99753 ) ;
#35262 = CARTESIAN_POINT ( 'NONE',  ( 1.822755070894378271, 1.797457900398396813, 0.6936678961073846628 ) ) ;
#35261 = CARTESIAN_POINT ( 'NONE',  ( -7.004758919754800139, 11.32396917302262018, 0.000000000000000000 ) ) ;
#35263 = CARTESIAN_POINT ( 'NONE',  ( -5.164730172163054966, 4.990216387137135889, -0.7998128361456362523 ) ) ;
#35264 = CARTESIAN_POINT ( 'NONE',  ( 6.666861335811934630, 1.461617314166022474, -1.320220550599479070 ) ) ;
#35265 = CARTESIAN_POINT ( 'NONE',  ( 5.695833931072550094, 5.817763472438987726, 0.000000000000000000 ) ) ;
#35266 = CARTESIAN_POINT ( 'NONE',  ( 5.790052644182137165, 6.039355072771209088, 0.5314338945540015846 ) ) ;
#35267 = CARTESIAN_POINT ( 'NONE',  ( -3.521367211247373508, 5.131347717920458962, -1.599625672291256295 ) ) ;
#35269 = CARTESIAN_POINT ( 'NONE',  ( 1.529832089473160517, -0.2657924667638748017, 2.205375646708715998 ) ) ;
#35268 = CARTESIAN_POINT ( 'NONE',  ( 0.5629301599625028407, 0.6213668382478373386, 2.027498709647377773 ) ) ;
#35270 = CARTESIAN_POINT ( 'NONE',  ( 2.977667800601135895, 2.000151994021987623, -0.6593727523046940542 ) ) ;
#35271 = CARTESIAN_POINT ( 'NONE',  ( -7.923814432544069142, 8.209148024248356990, 0.000000000000000000 ) ) ;
#35272 = CARTESIAN_POINT ( 'NONE',  ( 5.452350330990040739, 9.512825819463730070, 0.7998128361456462443 ) ) ;
#35273 = CARTESIAN_POINT ( 'NONE',  ( 0.3614606035443160836, -0.5022670859271642918, 1.791915111541013461 ) ) ;
#35274 = CARTESIAN_POINT ( 'NONE',  ( 6.775324078527185989, 8.927630729746953264, -1.599625672291262513 ) ) ;
#35276 =( BOUNDED_CURVE ( )  B_SPLINE_CURVE ( 3, ( #185094, #118054, #103878, #166742 ),
 .UNSPECIFIED., .F., .T. ) 
 B_SPLINE_CURVE_WITH_KNOTS ( ( 4, 4 ),
 ( 0.5000000000000005551, 1.000000000000000000 ),
 .UNSPECIFIED. ) 
 CURVE ( )  GEOMETRIC_REPRESENTATION_ITEM ( )  RATIONAL_B_SPLINE_CURVE ( ( 0.9999999999999994449, 0.3333333333333334259, 0.3333333333333341475, 1.000000000000000222 ) ) 
 REPRESENTATION_ITEM ( '' )  );
#35275 = CARTESIAN_POINT ( 'NONE',  ( -4.339127873110165901, 7.217636166161084610, -1.009937615098016606 ) ) ;
#35277 = CARTESIAN_POINT ( 'NONE',  ( 5.497994985541524215, 6.373081223675282736, -1.199719254218445830 ) ) ;
#35278 = CARTESIAN_POINT ( 'NONE',  ( -6.183927461608886844, 7.347575139032721303, 1.082531754730548412 ) ) ;
#35279 = CARTESIAN_POINT ( 'NONE',  ( -6.399085315970132193, 10.40942393536641397, -0.7216878364870278340 ) ) ;
#35280 = AXIS2_PLACEMENT_3D ( 'NONE', #64845, #62708, #28089 ) ;
#35281 = CARTESIAN_POINT ( 'NONE',  ( 1.529697670087664108, -0.2543295609688834835, 2.105205558366497698 ) ) ;
#35282 = CARTESIAN_POINT ( 'NONE',  ( -4.762657100150483380, 8.778460060142702304, 0.000000000000000000 ) ) ;
#35284 = CARTESIAN_POINT ( 'NONE',  ( 4.773855682050706761, -1.924389145058275963, 0.3807478752155256663 ) ) ;
#35283 = CARTESIAN_POINT ( 'NONE',  ( 0.6125000000000037081, 0.3333333333333590720, 1.060881119635903147 ) ) ;
#35285 = CARTESIAN_POINT ( 'NONE',  ( 2.975616057669258741, 2.053088362031017855, -0.6768339029224537118 ) ) ;
#35286 = CARTESIAN_POINT ( 'NONE',  ( 1.294213439101927321, 1.504999338701202394, -1.060447551955064016 ) ) ;
#35287 = COLOUR_RGB ( '', 0.09019608, 0.27058824, 0.51372549) ;
#35288 = CARTESIAN_POINT ( 'NONE',  ( -4.054949276293840832, 7.568305524423037056, 0.4105793130844727079 ) ) ;
#35289 = CARTESIAN_POINT ( 'NONE',  ( 4.232984923718338344, 7.533997312158466464, -0.9744250676351111640 ) ) ;
#35290 = CARTESIAN_POINT ( 'NONE',  ( 4.101278252482940978, -1.735469017763660027, 0.1308211784099410635 ) ) ;
#35291 = CARTESIAN_POINT ( 'NONE',  ( 4.001749955438753226, 7.811071542261023737, 0.1299566359906061952 ) ) ;
#35292 = CARTESIAN_POINT ( 'NONE',  ( 5.260200412422194383, 7.159986452624450770, -1.443375672974051449 ) ) ;
#35293 = CARTESIAN_POINT ( 'NONE',  ( -10.01593736600300311, 5.734280347462529015, 5.906528988732270058 ) ) ;
#35294 = CARTESIAN_POINT ( 'NONE',  ( 2.079201547314021070, -0.1057080177612122196, -2.159229931372666389 ) ) ;
#35295 = CARTESIAN_POINT ( 'NONE',  ( 3.005232341680406094, 2.000550758621592706, 0.2495690156183311137 ) ) ;
#35296 = CARTESIAN_POINT ( 'NONE',  ( -10.61567108937589765, 11.48729714713446803, 0.7216878364870438212 ) ) ;
#35297 = CARTESIAN_POINT ( 'NONE',  ( 1.780366757100563913, -1.156431984057613827, 1.826190802295484472 ) ) ;
#35298 = EDGE_LOOP ( 'NONE', ( #26267, #204045, #141329, #12018, #181001, #164791 ) ) ;
#35299 = CARTESIAN_POINT ( 'NONE',  ( 3.801606108737245471, -0.5733388152893458267, 1.886244881718708521 ) ) ;
#35300 = CARTESIAN_POINT ( 'NONE',  ( 6.509000000000010999, 0.004788705324892603143, 2.000274819378269786 ) ) ;
#35301 = CARTESIAN_POINT ( 'NONE',  ( 3.702622889756892022, 1.667158369460784106, 0.9958445826224509023 ) ) ;
#35304 = EDGE_LOOP ( 'NONE', ( #196519, #11011, #51581, #23412 ) ) ;
#35303 = LINE ( 'NONE', #16912, #84311 ) ;
#35302 = CARTESIAN_POINT ( 'NONE',  ( -8.622622508166983835, 13.00355065959610279, 1.040834085586084257E-14 ) ) ;
#35305 = CARTESIAN_POINT ( 'NONE',  ( -3.960390268523300339, 7.634556056670224855, 1.214306433183764966E-14 ) ) ;
#35306 = CARTESIAN_POINT ( 'NONE',  ( -0.1106856583841086261, 0.2435294909829844312, -2.031701206977332586 ) ) ;
#35307 = CARTESIAN_POINT ( 'NONE',  ( 3.888156192069020634, 7.758209000714329839, 1.040834085586084257E-14 ) ) ;
#35308 = CARTESIAN_POINT ( 'NONE',  ( -5.438755897737433287, 6.374245297895642537, -1.199719254218453823 ) ) ;
#35309 = CARTESIAN_POINT ( 'NONE',  ( -6.805266759416629618, 6.904175738932996964, 0.000000000000000000 ) ) ;
#35310 = CARTESIAN_POINT ( 'NONE',  ( -9.449669878600616357, 12.04770082983265844, -1.443375672974058777 ) ) ;
#35311 = CARTESIAN_POINT ( 'NONE',  ( 6.791963826450252206, -0.9943653912195188349, 2.080009744879149913 ) ) ;
#35312 = FACE_OUTER_BOUND ( 'NONE', #92827, .T. ) ;
#35313 = CARTESIAN_POINT ( 'NONE',  ( 4.276187414114787089, -1.004825795036960567, -1.684713053385626269 ) ) ;
#35314 = CARTESIAN_POINT ( 'NONE',  ( 1.301407962653992501, 1.352153127569672098, -1.496052916918483744 ) ) ;
#35315 = ORIENTED_EDGE ( 'NONE', *, *, #132876, .T. ) ;
#35316 = CARTESIAN_POINT ( 'NONE',  ( 3.907494643824228397, -2.025022917198250560, 0.6182885518764801303 ) ) ;
#35317 = CARTESIAN_POINT ( 'NONE',  ( 1.499999999999989120, 3.535416667349488229, 0.8660254037844524744 ) ) ;
#35318 = CARTESIAN_POINT ( 'NONE',  ( -6.175902666224832416, 7.163973517805802160, -1.199719254218446718 ) ) ;
#35319 = CARTESIAN_POINT ( 'NONE',  ( 2.677489186553199563, -0.9463553590365642032, 1.579155189138586213 ) ) ;
#35320 = ORIENTED_EDGE ( 'NONE', *, *, #64280, .F. ) ;
#35321 = UNCERTAINTY_MEASURE_WITH_UNIT (LENGTH_MEASURE( 1.000000000000000082E-05 ), #119191, 'distance_accuracy_value', 'NONE');
#35322 = CARTESIAN_POINT ( 'NONE',  ( -8.507905087775398556, 9.884643009614800135, 1.199719254218462483 ) ) ;
#35323 = CARTESIAN_POINT ( 'NONE',  ( 0.3868389748197148537, 3.100956225802592670, 0.4583768147622874212 ) ) ;
#35324 = CARTESIAN_POINT ( 'NONE',  ( 5.713165544288242970, 1.732532623411761286, -1.222520872474173848 ) ) ;
#35325 = CARTESIAN_POINT ( 'NONE',  ( -0.1399997263889597998, 7.629137130509076492, -2.600276787041354787 ) ) ;
#35326 = CARTESIAN_POINT ( 'NONE',  ( 7.450369105909416589, 8.650851030771185890, -1.199719254218441611 ) ) ;
#35327 = CARTESIAN_POINT ( 'NONE',  ( 5.852824474907069252, -1.627199953678662991, 1.264450640605979892 ) ) ;
#35328 = VECTOR ( 'NONE', #184060, 1000.000000000000000 ) ;
#35331 = CARTESIAN_POINT ( 'NONE',  ( 2.630204301513817455, 0.2276190002089127917, 1.827071974840013269 ) ) ;
#35330 = CARTESIAN_POINT ( 'NONE',  ( 0.5196754285911856508, 1.841638447829671899, -0.2671899778997516850 ) ) ;
#35329 = LINE ( 'NONE', #51607, #208061 ) ;
#35332 = CARTESIAN_POINT ( 'NONE',  ( 7.411503528164766763, 11.79850454950093841, 1.040834085586084257E-14 ) ) ;
#35333 = SURFACE_SIDE_STYLE ('',( #144884 ) ) ;
#35334 = CARTESIAN_POINT ( 'NONE',  ( 0.000000000000000000, 13.49999999999999822, -1.240450515248286534 ) ) ;
#35335 = CARTESIAN_POINT ( 'NONE',  ( 1.224999999999929257, 2.208333334016110427, -0.7072540797573095839 ) ) ;
#35336 = CARTESIAN_POINT ( 'NONE',  ( 2.737190076726934151, 0.2709513247245790013, 2.190122135706531914 ) ) ;
#35337 = CARTESIAN_POINT ( 'NONE',  ( 5.395900114300756556, -0.8213888976819706533, 2.108206106441696370 ) ) ;
#35338 = CARTESIAN_POINT ( 'NONE',  ( -8.053180056837398126, 8.497724275839514618, 0.7216878364870578100 ) ) ;
#35339 = CARTESIAN_POINT ( 'NONE',  ( 5.080233222017616512, 0.8995743074830947483, 1.572398339973365422 ) ) ;
#35340 = CARTESIAN_POINT ( 'NONE',  ( 4.803869215722607500, -1.030175745946705801, -1.614969243545740785 ) ) ;
#35341 = EDGE_CURVE ( 'NONE', #73414, #6089, #96532, .T. ) ;
#35342 = CARTESIAN_POINT ( 'NONE',  ( -0.6823417656249969321, 5.780208333674756283, -1.181850606188749264 ) ) ;
#35343 = CARTESIAN_POINT ( 'NONE',  ( 3.537922462266992252, 0.8877721971902104992, -1.760348037230663021 ) ) ;
#35344 = CARTESIAN_POINT ( 'NONE',  ( 4.785944050937030347, -0.8815013282119155136, 1.649949660215948688 ) ) ;
#35345 = EDGE_CURVE ( 'NONE', #40498, #19959, #197696, .T. ) ;
#35346 = CARTESIAN_POINT ( 'NONE',  ( 4.984723811273123140, 1.780707155018296239, 0.5408319247705763999 ) ) ;
#35347 = CARTESIAN_POINT ( 'NONE',  ( -0.6823417656250212460, 5.551041667008087543, 1.181850606188767472 ) ) ;
#35348 = CONICAL_SURFACE ( 'NONE', #204797, 8.368490868537556082, 0.7853981633974479459 ) ;
#35349 = TOROIDAL_SURFACE ( 'NONE', #212232, 11.92000000000000171, 0.08000000000000000167 ) ;
#35350 = CARTESIAN_POINT ( 'NONE',  ( 0.2160302486270138655, 1.032475520995678853, -1.731998313101141163 ) ) ;
#35352 = CARTESIAN_POINT ( 'NONE',  ( 1.260533433194007236, 0.8550034467163977192, 1.924895685913818655 ) ) ;
#35351 = CARTESIAN_POINT ( 'NONE',  ( -10.65400978224035811, 11.32409958890225710, 1.040834085586084257E-14 ) ) ;
#35353 = CARTESIAN_POINT ( 'NONE',  ( 8.536830278099042602, 13.11138575775759563, -0.7998128361456352531 ) ) ;
#35355 = CARTESIAN_POINT ( 'NONE',  ( -10.65400978224035811, 11.32409958890225710, 1.040834085586084257E-14 ) ) ;
#35354 = CARTESIAN_POINT ( 'NONE',  ( 1.483456582845025240, 7.293967155395495006, 4.258619948150350609 ) ) ;
#35356 = CARTESIAN_POINT ( 'NONE',  ( 3.463236921083117981, -1.731491641549892435, 1.224000437801611163 ) ) ;
#35357 = DIRECTION ( 'NONE',  ( 0.6507913734559627184, 0.7592566023653016805, 0.000000000000000000 ) ) ;
#35358 = CARTESIAN_POINT ( 'NONE',  ( 1.599874016572962798, 1.395964939349272349, 1.459955266877453806 ) ) ;
#35359 = CARTESIAN_POINT ( 'NONE',  ( -0.6823417656250212460, 1.801041667008083991, 1.181850606188755259 ) ) ;
#35360 = CARTESIAN_POINT ( 'NONE',  ( -2.765500147507697459, 5.209872024525476597, 1.082531754730560403 ) ) ;
#35361 = CARTESIAN_POINT ( 'NONE',  ( 3.334415713957098681, 5.977569868670206787, -1.199719254218446718 ) ) ;
#35362 = ORIENTED_EDGE ( 'NONE', *, *, #7000, .F. ) ;
#35363 = CARTESIAN_POINT ( 'NONE',  ( 1.704591423195594535, -0.7763021076895926242, -2.017573427605146907 ) ) ;
#35364 = CARTESIAN_POINT ( 'NONE',  ( 6.890000000000007674, 6.036127733823692054, 2.594896729422516923 ) ) ;
#35367 = CARTESIAN_POINT ( 'NONE',  ( 1.886825320689258012, 2.480000000000016858, -2.459652456995881753 ) ) ;
#35366 = CARTESIAN_POINT ( 'NONE',  ( -3.929058411375426108, 4.999999999999997335, 0.7499999999999988898 ) ) ;
#35365 = CARTESIAN_POINT ( 'NONE',  ( 4.543917759235442944, 5.330267469643351852, 1.199719254218452935 ) ) ;
#35368 = DIRECTION ( 'NONE',  ( 1.276756478318932585E-15, -1.000000000000000000, 1.665334536937738262E-16 ) ) ;
#35369 = CARTESIAN_POINT ( 'NONE',  ( 6.456263137377813877, -1.236968576560824040, 1.593241027169020052 ) ) ;
#35370 = CARTESIAN_POINT ( 'NONE',  ( -7.714226216495749355, 8.102278128774251797, 1.040834085586084257E-14 ) ) ;
#35372 = B_SPLINE_CURVE_WITH_KNOTS ( 'NONE', 3,
 ( #91559, #9212, #7047, #43873, #59026, #192211, #142452, #56896, #109989, #123071, #171706, #40666, #140317, #156545, #22222, #88335 ),
 .UNSPECIFIED., .F., .F.,
 ( 4, 3, 3, 3, 3, 4 ),
 ( 0.000000000000000000, 6.716675436053851645E-06, 1.344324725955300992E-05, 2.018532118335282307E-05, 2.694176617306668026E-05, 3.135538808400729303E-05 ),
 .UNSPECIFIED. ) ;
#35371 = CARTESIAN_POINT ( 'NONE',  ( 1.154151856878969928, 0.8927059368322427524, 2.001694687108931170 ) ) ;
#35373 = LINE ( 'NONE', #51649, #70580 ) ;
#35375 = CARTESIAN_POINT ( 'NONE',  ( -1.364683531250010740, 12.38020833367473195, 0.7879004041258445001 ) ) ;
#35374 = CARTESIAN_POINT ( 'NONE',  ( 1.130147970125170431, -1.436987675322987101, -1.747601730595295333 ) ) ;
#35376 = CARTESIAN_POINT ( 'NONE',  ( -7.645908563102897126, 11.00764485934031889, 1.199719254218453823 ) ) ;
#35377 = CARTESIAN_POINT ( 'NONE',  ( -5.111060722227552588, 6.025620933095978238, 1.082531754730546636 ) ) ;
#35378 = CARTESIAN_POINT ( 'NONE',  ( 1.364683531249990311, 2.696875000341415696, 1.214306433183764966E-14 ) ) ;
#35379 = CARTESIAN_POINT ( 'NONE',  ( 4.605417112443645600, 8.360468292628990383, 0.2083848827989076002 ) ) ;
#35380 = AXIS2_PLACEMENT_3D ( 'NONE', #167942, #40083, #123555 ) ;
#35381 = CARTESIAN_POINT ( 'NONE',  ( -1.500000000000001110, 9.270833333333332149, 0.8660254037844419273 ) ) ;
#35382 = CARTESIAN_POINT ( 'NONE',  ( 3.967213729759576868, 0.2084270747255561884, -1.712163910207653128 ) ) ;
#35383 = CARTESIAN_POINT ( 'NONE',  ( 3.054329744828568227, 6.785411478933790264, 0.000000000000000000 ) ) ;
#35384 = CARTESIAN_POINT ( 'NONE',  ( 1.651228947852514173, 0.5200303365089484764, -1.691588852159523704 ) ) ;
#35385 = CARTESIAN_POINT ( 'NONE',  ( 3.035794076406534536, -1.939542403429166395, 0.5389024948808174287 ) ) ;
#35386 = CARTESIAN_POINT ( 'NONE',  ( 5.842855468016632692, 0.4250294216477692455, 2.165293060021292515 ) ) ;
#35387 = ORIENTED_EDGE ( 'NONE', *, *, #192096, .T. ) ;
#35388 = CARTESIAN_POINT ( 'NONE',  ( -4.938913097128142304, 8.984092056616635347, -0.7998128361456362523 ) ) ;
#35389 = CARTESIAN_POINT ( 'NONE',  ( 4.991814629660241920, -2.006445540622634915, 0.2004526995145126111 ) ) ;
#35390 = VERTEX_POINT ( 'NONE', #108496 ) ;
#35391 = CARTESIAN_POINT ( 'NONE',  ( 2.746779440450992649, -1.556306552617524597, 1.037596984913228937 ) ) ;
#35392 = CARTESIAN_POINT ( 'NONE',  ( 6.721331454403435934, -0.1262074967819451221, 1.796610827203233063 ) ) ;
#35393 = CARTESIAN_POINT ( 'NONE',  ( 1.722773492080275748, 1.414811824084385661, -1.286832238068566392 ) ) ;
#35394 = CARTESIAN_POINT ( 'NONE',  ( -6.309289698153002668, 6.533461890506125691, 0.1636223065131766075 ) ) ;
#35395 = CARTESIAN_POINT ( 'NONE',  ( -11.16206481669071415, 4.728763190537430994, -6.013947724923736082 ) ) ;
#35396 = CARTESIAN_POINT ( 'NONE',  ( -3.621833129746846680, 4.096114899008192367, 2.500000000000011102 ) ) ;
#35397 = CARTESIAN_POINT ( 'NONE',  ( -1.364683531249997417, 4.071875000341417028, 1.214306433183764966E-14 ) ) ;
#35398 = CARTESIAN_POINT ( 'NONE',  ( -0.1054227091227821350, -1.855472971956134920, -0.4628026090111520552 ) ) ;
#35399 = CARTESIAN_POINT ( 'NONE',  ( 6.427974226654860956, 7.632296364919712417, -1.082531754730548412 ) ) ;
#35400 = CARTESIAN_POINT ( 'NONE',  ( 1.732786548908150870, -1.861864252656076912, -0.6185235971247133868 ) ) ;
#35401 = CARTESIAN_POINT ( 'NONE',  ( -4.322341018716196359, 3.567520274870279007, -2.444429072473030651 ) ) ;
#35402 = EDGE_CURVE ( 'NONE', #35390, #170914, #94174, .T. ) ;
#35403 = CARTESIAN_POINT ( 'NONE',  ( -3.474632506852224356, 7.275764701294714420, -0.7998128361456481317 ) ) ;
#35404 = CARTESIAN_POINT ( 'NONE',  ( 4.992489932941453823, -1.175987964647656536, 1.764448611491518548 ) ) ;
#35406 = DIRECTION ( 'NONE',  ( 0.000000000000000000, 0.000000000000000000, -1.000000000000000000 ) ) ;
#35405 = CARTESIAN_POINT ( 'NONE',  ( 9.759171643738394408, 10.28012176064996197, 0.000000000000000000 ) ) ;
#35407 = CARTESIAN_POINT ( 'NONE',  ( 0.2450992160058732550, -1.441561472518913867, -1.191725768352129622 ) ) ;
#35408 = CARTESIAN_POINT ( 'NONE',  ( -1.201851678989727383E-14, 1.821875000341421691, 1.575800808251672791 ) ) ;
#35409 = CARTESIAN_POINT ( 'NONE',  ( 2.232683648988046610, 1.311727534961094177, -1.527327462066043084 ) ) ;
#35410 = ORIENTED_EDGE ( 'NONE', *, *, #182811, .T. ) ;
#35412 = CARTESIAN_POINT ( 'NONE',  ( 0.5798918133415768006, -0.7576680531077238934, 1.977200763303339714 ) ) ;
#35411 = CARTESIAN_POINT ( 'NONE',  ( -7.863365906246068349, 9.236643647784308797, -1.082531754730543971 ) ) ;
#35413 = CARTESIAN_POINT ( 'NONE',  ( 9.443127104094640956, 11.07005408922290002, 7.334139569562794669 ) ) ;
#35414 = CARTESIAN_POINT ( 'NONE',  ( 2.945825538390862697, 1.462269270728074222, 1.465923284304726737 ) ) ;
#35415 = CARTESIAN_POINT ( 'NONE',  ( 5.740951700743842423, 5.662474837148078421, -0.7998128361456481317 ) ) ;
#35416 = CARTESIAN_POINT ( 'NONE',  ( 3.400062661977048428, 7.188766548940353829, -1.734723475976807094E-15 ) ) ;
#35417 = EDGE_LOOP ( 'NONE', ( #16033, #128581, #169667 ) ) ;
#35419 = CARTESIAN_POINT ( 'NONE',  ( 4.379447312414087357, 5.068108938359919158, -1.199719254218452047 ) ) ;
#35418 = CARTESIAN_POINT ( 'NONE',  ( 4.681631697639319079, -0.9857103537862299536, 1.843662662672640007 ) ) ;
#35422 = ORIENTED_EDGE ( 'NONE', *, *, #38065, .T. ) ;
#35421 = CARTESIAN_POINT ( 'NONE',  ( 3.000440247697288676, -1.785030861869114638, -0.3072999389705335926 ) ) ;
#35420 = CARTESIAN_POINT ( 'NONE',  ( 3.487140482124751362, 1.650829432287181264, -0.7796944959364560113 ) ) ;
#35423 = CARTESIAN_POINT ( 'NONE',  ( 6.270183524512255246, 1.130759168108757873, 1.895055401287759178 ) ) ;
#35424 = CARTESIAN_POINT ( 'NONE',  ( 1.843739406749228538, 8.499999999999996447, -0.7750000000000013545 ) ) ;
#35425 = CARTESIAN_POINT ( 'NONE',  ( 10.74389548477261691, 10.91622383494151549, 5.684367872889470874 ) ) ;
#35426 = CARTESIAN_POINT ( 'NONE',  ( 5.122202071631626552, -1.176711583861598243, -1.866687997650509301 ) ) ;
#35427 = CARTESIAN_POINT ( 'NONE',  ( -0.6823417656250039265, 9.880208333674728394, -1.181850606188755259 ) ) ;
#35428 = ADVANCED_FACE ( 'NONE', ( #22879, #107425 ), #173450, .F. ) ;
#35429 = ORIENTED_EDGE ( 'NONE', *, *, #180435, .T. ) ;
#35430 = CARTESIAN_POINT ( 'NONE',  ( 4.178302048780179412, 0.9043031410675538284, 1.684961085834511874 ) ) ;
#35431 = CARTESIAN_POINT ( 'NONE',  ( -4.135400547368138113, 4.783387712472935149, 1.199719254218462483 ) ) ;
#35432 = CIRCLE ( 'NONE', #204881, 6.249999999999995559 ) ;
#35433 = VECTOR ( 'NONE', #193073, 1000.000000000000000 ) ;
#35434 = CARTESIAN_POINT ( 'NONE',  ( 0.5101186646354113341, -1.387778780781445676E-14, 1.261047121698059215 ) ) ;
#35435 = CARTESIAN_POINT ( 'NONE',  ( 4.487385655998873624, 7.218738451098584363, 1.082531754730558626 ) ) ;
#35436 = CARTESIAN_POINT ( 'NONE',  ( 10.99970480893080627, -6.134628647623513231, 0.08058608058608522640 ) ) ;
#35437 = CARTESIAN_POINT ( 'NONE',  ( 7.958945746774230834, 14.27980018522660188, -8.981532223576218499 ) ) ;
#35438 = CARTESIAN_POINT ( 'NONE',  ( -7.116813477139661615, 15.47012847482234221, -9.672254489698197233 ) ) ;
#35439 = CARTESIAN_POINT ( 'NONE',  ( 4.059713336928523653, 1.856696190431494475, -0.2264497139414511362 ) ) ;
#35440 = CARTESIAN_POINT ( 'NONE',  ( 0.7500000000000006661, 10.91666666666666430, -1.299038105676657340 ) ) ;
#35441 = CARTESIAN_POINT ( 'NONE',  ( -0.2409995289980246813, 5.721856934700204178, -2.594540323675114113 ) ) ;
#35442 = CARTESIAN_POINT ( 'NONE',  ( -7.537970219518091319, 7.896646132300314314, -0.7216878364870278340 ) ) ;
#35443 = CARTESIAN_POINT ( 'NONE',  ( 0.2988868148526523938, -0.2362956723594503705, -1.897694653714178781 ) ) ;
#35444 = CARTESIAN_POINT ( 'NONE',  ( 5.495132332240461714, 5.305409230568988832, 0.7998128361456341429 ) ) ;
#35445 = CARTESIAN_POINT ( 'NONE',  ( 0.4968415868889561882, 0.3310222599195339899, 1.941247527895247904 ) ) ;
#35446 = CARTESIAN_POINT ( 'NONE',  ( 1.230092461119953517, 2.014234866427236259, 0.09611455020034495589 ) ) ;
#35447 = CARTESIAN_POINT ( 'NONE',  ( -7.160677686311960777, 11.50587440067263678, -0.7998128361456291469 ) ) ;
#35448 = CARTESIAN_POINT ( 'NONE',  ( 5.855142236255289845, 7.924361590421551860, -1.599625672291281386 ) ) ;
#35450 = ADVANCED_FACE ( 'NONE', ( #8783 ), #206119, .T. ) ;
#35449 = CARTESIAN_POINT ( 'NONE',  ( 2.295757763869426871, 5.519548059767960702, 0.4031905389056070765 ) ) ;
#35451 = CARTESIAN_POINT ( 'NONE',  ( 1.640847625397081622, -1.850035366842089024, 1.174371965539475093 ) ) ;
#35452 = DIRECTION ( 'NONE',  ( 1.000000000000000000, -0.000000000000000000, -0.000000000000000000 ) ) ;
#35453 = CARTESIAN_POINT ( 'NONE',  ( -2.286521462199063492, 5.819358805874190743, 1.040834085586084257E-14 ) ) ;
#35454 = EDGE_CURVE ( 'NONE', #43310, #95302, #110682, .T. ) ;
#35455 = CARTESIAN_POINT ( 'NONE',  ( 4.367134877377630175, 7.148722219365612141, -1.082531754730548412 ) ) ;
#35456 = CARTESIAN_POINT ( 'NONE',  ( 7.397945374551106568, 11.78268670361832093, -0.7998128361456291469 ) ) ;
#35457 =( BOUNDED_SURFACE ( )  B_SPLINE_SURFACE ( 3, 2, ( 
 ( #101447, #122059, #69985 ),
 ( #167520, #188023, #54840 ),
 ( #89493, #136097, #37516 ),
 ( #67846, #2852, #199999 ) ),
 .UNSPECIFIED., .F., .F., .T. ) 
 B_SPLINE_SURFACE_WITH_KNOTS ( ( 4, 4 ),
 ( 3, 3 ),
 ( 0.01090155471707268328, 0.01336979040894267431 ),
 ( 0.000000000000000000, 1.000000000000000000 ),
 .UNSPECIFIED. ) 
 GEOMETRIC_REPRESENTATION_ITEM ( )  RATIONAL_B_SPLINE_SURFACE ( (
 ( 1.000000000000000000, 0.6967468848055766717, 1.000000000000000000),
 ( 1.000000000000000000, 0.6961913616436843366, 1.000000000000000000),
 ( 1.000000000000000000, 0.6955505937926286242, 1.000000000000000000),
 ( 1.000000000000000000, 0.6947640035364027744, 1.000000000000000000) ) ) 
 REPRESENTATION_ITEM ( '' )  SURFACE ( )  );
#35458 = CARTESIAN_POINT ( 'NONE',  ( 2.530568227245037605, 6.104080031761181857, 0.000000000000000000 ) ) ;
#35459 = CARTESIAN_POINT ( 'NONE',  ( 6.780486220610169035, 9.003929572168926754, -1.443375672974078761 ) ) ;
#35460 = VERTEX_POINT ( 'NONE', #13036 ) ;
#35462 = CARTESIAN_POINT ( 'NONE',  ( 0.3814940398445298420, 0.1953205766255173559, -2.003579427208526553 ) ) ;
#35461 = CARTESIAN_POINT ( 'NONE',  ( 3.403688466941825475, -0.7492148395099357261, -1.682118234477212537 ) ) ;
#35463 = CARTESIAN_POINT ( 'NONE',  ( 3.269240723250285363, -2.295843464198448203, 0.1100516299901241751 ) ) ;
#35465 = CARTESIAN_POINT ( 'NONE',  ( 0.5142147075538996415, 0.7048593813003102282, 1.722512033545370080 ) ) ;
#35464 = CARTESIAN_POINT ( 'NONE',  ( 3.389175213736297820, 4.977123720824209840, 1.443375672974062551 ) ) ;
#35466 = CARTESIAN_POINT ( 'NONE',  ( -3.474999999999998312, -0.3208333333333319715, 2.006292185433951047 ) ) ;
#35467 = CARTESIAN_POINT ( 'NONE',  ( -3.879604511804807032, 7.677955697080923514, 0.7998128361456341429 ) ) ;
#35468 = DIRECTION ( 'NONE',  ( 1.276756478318932585E-15, -1.000000000000000000, 1.665334536937738262E-16 ) ) ;
#35469 = CARTESIAN_POINT ( 'NONE',  ( 4.447458312869024155, -1.746245811230532130, 0.7801085911468002010 ) ) ;
#35470 = CARTESIAN_POINT ( 'NONE',  ( -8.971744963941075568, 11.49012176272984931, 1.599625672291269396 ) ) ;
#35471 = CARTESIAN_POINT ( 'NONE',  ( 6.093313910611117379, 7.014445836765536235, -0.9825430356366869900 ) ) ;
#35472 = CARTESIAN_POINT ( 'NONE',  ( -6.346625304972878467, 7.537389289624049304, 1.082531754730548412 ) ) ;
#35474 = CARTESIAN_POINT ( 'NONE',  ( 2.623731232481395725, -1.075365945362505293, -1.530472918023266571 ) ) ;
#35473 = CARTESIAN_POINT ( 'NONE',  ( 3.878531184313998015, -0.2068018975109634505, -2.080507369234054771 ) ) ;
#35475 = CARTESIAN_POINT ( 'NONE',  ( 7.131225611108088280, 9.342849184424693476, 1.443375672974076540 ) ) ;
#35476 = CARTESIAN_POINT ( 'NONE',  ( -6.745922712994596893, -7.817744194000435520, -6.689586359223953060 ) ) ;
#35477 = CARTESIAN_POINT ( 'NONE',  ( 3.280519990774858119, 1.572054556770419387, -0.7471684773981291938 ) ) ;
#35478 = AXIS2_PLACEMENT_3D ( 'NONE', #97284, #14918, #147100 ) ;
#35479 = CARTESIAN_POINT ( 'NONE',  ( 3.161022370280501814, 6.839609865302569425, 0.000000000000000000 ) ) ;
#35481 = CARTESIAN_POINT ( 'NONE',  ( 5.030238685870051185, 5.827365540725222282, -1.199719254218452047 ) ) ;
#35480 = FACE_OUTER_BOUND ( 'NONE', #91276, .T. ) ;
#35482 = CARTESIAN_POINT ( 'NONE',  ( 4.160587402808674007, -1.276020550970466516, 1.160787852381778062 ) ) ;
#35483 = CARTESIAN_POINT ( 'NONE',  ( -7.335124800193271177, 8.516399340768996851, -1.199719254218452935 ) ) ;
#35484 = CARTESIAN_POINT ( 'NONE',  ( 6.094375512030342001, -2.195847865938059140, -0.2203403561373064590 ) ) ;
#35485 = CARTESIAN_POINT ( 'NONE',  ( -0.6125000000000383471, 0.7708333340161397373, -1.060881119635972647 ) ) ;
#35486 = CARTESIAN_POINT ( 'NONE',  ( 3.924824802941798030, -1.462044496099848212, 1.605114832664520153 ) ) ;
#35487 = CARTESIAN_POINT ( 'NONE',  ( 2.051128252772801641, -1.465761996925791122, -1.088229512710245261 ) ) ;
#35488 = CARTESIAN_POINT ( 'NONE',  ( 0.4616703453074429975, -0.5288386019042885522, 1.889040479230045255 ) ) ;
#35489 = CARTESIAN_POINT ( 'NONE',  ( 5.999228916948370127, -0.2569761400621084491, 2.101594505611179109 ) ) ;
#35490 = ORIENTED_EDGE ( 'NONE', *, *, #172906, .T. ) ;
#35492 = CARTESIAN_POINT ( 'NONE',  ( -1.201851678989727383E-14, 2.884375000341418804, 1.575800808251672791 ) ) ;
#35491 = CARTESIAN_POINT ( 'NONE',  ( 6.163675082799745297, 1.174783243402954591, 1.968361872208840069 ) ) ;
#35493 = CARTESIAN_POINT ( 'NONE',  ( 8.380911511541880188, 12.92948053010758258, 0.7998128361456462443 ) ) ;
#35494 = CARTESIAN_POINT ( 'NONE',  ( 1.805496089173063812, 1.843435535509674317, -1.047849062051921853 ) ) ;
#35495 = CARTESIAN_POINT ( 'NONE',  ( -5.477130870240893401, 6.452702772444876445, 1.082531754730548412 ) ) ;
#35496 = CARTESIAN_POINT ( 'NONE',  ( 3.389175213736297820, 4.977123720824209840, 1.443375672974062551 ) ) ;
#35497 = CARTESIAN_POINT ( 'NONE',  ( -5.707619481228832115, 6.721606151930833661, -1.082531754730543971 ) ) ;
#35498 = AXIS2_PLACEMENT_3D ( 'NONE', #142902, #107229, #40039 ) ;
#35500 = CARTESIAN_POINT ( 'NONE',  ( 0.7500000000000006661, 12.11458333401613174, 1.299038105676657340 ) ) ;
#35499 = LINE ( 'NONE', #184939, #134482 ) ;
#35502 = VERTEX_POINT ( 'NONE', #144176 ) ;
#35501 = CARTESIAN_POINT ( 'NONE',  ( 1.084998894000373637, -1.405142754555653628, 1.720412613360406295 ) ) ;
#35503 = CARTESIAN_POINT ( 'NONE',  ( 6.416638760586134360, -1.319225726833603840, -1.525046029381103452 ) ) ;
#35505 = CARTESIAN_POINT ( 'NONE',  ( 3.942276525692486544, -1.021014944866809326, 1.792092113122957242 ) ) ;
#35504 = CARTESIAN_POINT ( 'NONE',  ( 5.508690485854129903, 5.321227076451600091, 1.040834085586084257E-14 ) ) ;
#35507 = CARTESIAN_POINT ( 'NONE',  ( 1.737500000000001155, -3.033333333333332327, 3.009438278150922130 ) ) ;
#35506 = CARTESIAN_POINT ( 'NONE',  ( 5.505492895601038938, 8.580769590579979678, -1.199719254218452047 ) ) ;
#35508 = CARTESIAN_POINT ( 'NONE',  ( 7.388267364804250725, 7.584343111885245570, -0.7998128361456341429 ) ) ;
#35509 = CARTESIAN_POINT ( 'NONE',  ( 1.642778471875001811, -1.742708332855374298, 2.845375778867859751 ) ) ;
#35510 = CARTESIAN_POINT ( 'NONE',  ( 0.4102503234837206469, 1.440240287209685111, -1.515647972008065780 ) ) ;
#35511 = CARTESIAN_POINT ( 'NONE',  ( 5.151017605526480025, 0.9962996879465220168, 1.753031629501592192 ) ) ;
#35512 = CARTESIAN_POINT ( 'NONE',  ( 4.142028884782995135, 0.4951553702221401232, 1.773339192993342639 ) ) ;
#35513 = CARTESIAN_POINT ( 'NONE',  ( 5.524057522564145728, 8.532151978711786100, 1.199719254218462483 ) ) ;
#35514 = CARTESIAN_POINT ( 'NONE',  ( 0.6215558277854142943, -0.9165932506310509043, -1.460862699585960822 ) ) ;
#35515 = AXIS2_PLACEMENT_3D ( 'NONE', #47107, #14559, #111083 ) ;
#35516 = CARTESIAN_POINT ( 'NONE',  ( 0.1749484593404549426, -5.350147675656140578, 10.96499746917716855 ) ) ;
#35517 = CARTESIAN_POINT ( 'NONE',  ( 0.4405775615070831042, -1.946229768708742647, -1.222969628347547966 ) ) ;
#35518 = CARTESIAN_POINT ( 'NONE',  ( -6.925517538482230506, 6.974191971184389160, 0.7998128361456341429 ) ) ;
#35519 = CARTESIAN_POINT ( 'NONE',  ( 1.775094195334154135, -2.148033089049032895, -0.7103491116851842202 ) ) ;
#35520 = CARTESIAN_POINT ( 'NONE',  ( 3.545630178961965751, -1.594748897588176950, -1.375714639268589279 ) ) ;
#35521 = CARTESIAN_POINT ( 'NONE',  ( -4.261005416444848315, 8.193199762486115034, 0.7998128361456352531 ) ) ;
#35522 = CARTESIAN_POINT ( 'NONE',  ( 7.447506452608354088, 7.583179037664891098, 0.7998128361456341429 ) ) ;
#35524 = ADVANCED_FACE ( 'NONE', ( #195003 ), #212299, .F. ) ;
#35523 = CARTESIAN_POINT ( 'NONE',  ( 5.167065940139554669, 9.042344340222555843, -0.7216878364870458196 ) ) ;
#35525 = CARTESIAN_POINT ( 'NONE',  ( 6.531249988543854634, -0.7852927567036558365, -1.895863743163934245 ) ) ;
#35526 = CARTESIAN_POINT ( 'NONE',  ( -4.401593425930945713, 8.286942763561420122, 1.040834085586084257E-14 ) ) ;
#35527 = CARTESIAN_POINT ( 'NONE',  ( 6.033015167956792268, 8.061603667414825480, -1.443375672974057666 ) ) ;
#35528 = CARTESIAN_POINT ( 'NONE',  ( 4.469394083494863779, 7.278994484577430590, 1.251062204184281379 ) ) ;
#35529 = STYLED_ITEM ( 'NONE', ( #141019 ), #177196 ) ;
#35530 = CARTESIAN_POINT ( 'NONE',  ( -4.946027110887008860, 4.664786472323266153, -0.7998128361456221525 ) ) ;
#35531 = CARTESIAN_POINT ( 'NONE',  ( 5.484718290073375080, -1.409174384840453653, 1.717275654355006509 ) ) ;
#35532 = CARTESIAN_POINT ( 'NONE',  ( 3.451304434523004172, 0.5324976444292061073, -2.125649318046138880 ) ) ;
#35533 = CARTESIAN_POINT ( 'NONE',  ( -4.843287188579803448, 6.673587691474970107, -1.599625672291256295 ) ) ;
#35534 = CARTESIAN_POINT ( 'NONE',  ( -11.97178994924802353, 9.720000062027946086, 0.8322011300497191844 ) ) ;
#35535 = CARTESIAN_POINT ( 'NONE',  ( 5.424254290899477304, 0.9654600744411747648, 1.707767180430696641 ) ) ;
#35536 = CARTESIAN_POINT ( 'NONE',  ( 1.364683531249986537, 2.155208333674751398, -0.7879004041258239610 ) ) ;
#35537 = CARTESIAN_POINT ( 'NONE',  ( 6.610000000000026965, 7.052677709320480659, 2.598153670447616470 ) ) ;
#35538 = CARTESIAN_POINT ( 'NONE',  ( -4.880572111239580124, 7.677455982212699759, 1.082531754730560403 ) ) ;
#35539 = CARTESIAN_POINT ( 'NONE',  ( 4.904590598983499916, -2.104870323260544129, -0.2570220051709286579 ) ) ;
#35540 = CARTESIAN_POINT ( 'NONE',  ( -6.943184063974175757, 9.193743722760251202, -1.443375672974066548 ) ) ;
#35541 = EDGE_LOOP ( 'NONE', ( #193946, #196270, #118097, #35422, #115470 ) ) ;
#35543 = CARTESIAN_POINT ( 'NONE',  ( 6.209879897626497502, -2.145988306206991325, 0.2596296833028768347 ) ) ;
#35542 = CARTESIAN_POINT ( 'NONE',  ( -6.780486220610195680, 7.083191143566240910, -0.7216878364870338292 ) ) ;
#35544 = CARTESIAN_POINT ( 'NONE',  ( 4.469384193999260901, 8.366031992974468423, -0.7998128361456231517 ) ) ;
#35545 = CARTESIAN_POINT ( 'NONE',  ( 4.933073973922719624, -1.305863698873997780, -1.298312775753200699 ) ) ;
#35546 = CARTESIAN_POINT ( 'NONE',  ( -1.201851678989727383E-14, 3.134375000341420137, 1.575800808251672791 ) ) ;
#35547 = CARTESIAN_POINT ( 'NONE',  ( 1.487455728203713745, -1.732000560005091616, -0.1708635279896036641 ) ) ;
#35548 = CARTESIAN_POINT ( 'NONE',  ( 11.45842088241076340, 12.50693529122958481, 3.566211699757793063 ) ) ;
#35549 = CARTESIAN_POINT ( 'NONE',  ( 1.364683531249986981, -1.053124999658580752, 0.000000000000000000 ) ) ;
#35550 = DIRECTION ( 'NONE',  ( 0.000000000000000000, 1.000000000000000000, 0.000000000000000000 ) ) ;
#35551 = CARTESIAN_POINT ( 'NONE',  ( 5.260679775997886054, -1.568431141927080219, 1.487858469166832176 ) ) ;
#35552 = CARTESIAN_POINT ( 'NONE',  ( -4.620631424159025613, 4.285158171140619032, -0.7998128361456221525 ) ) ;
#35553 = CARTESIAN_POINT ( 'NONE',  ( -7.388830529323428209, 8.683019041374528513, 1.082531754730549967 ) ) ;
#35554 = CARTESIAN_POINT ( 'NONE',  ( 4.645497774645744649, -1.668943667408796294, -1.373881373981879594 ) ) ;
#35555 = CARTESIAN_POINT ( 'NONE',  ( 1.364683531249990311, 3.134375000341423245, 1.214306433183764966E-14 ) ) ;
#35556 = CARTESIAN_POINT ( 'NONE',  ( 4.850830000233872674, -1.585153962374891812, 1.171817952366477344 ) ) ;
#35557 = CARTESIAN_POINT ( 'NONE',  ( 4.516742233720687949, 1.733484511791906879, -0.04249706786149141935 ) ) ;
#35558 = CARTESIAN_POINT ( 'NONE',  ( 0.9432342461353732110, -1.730868645791438842, -1.344178957308760802 ) ) ;
#35559 = CARTESIAN_POINT ( 'NONE',  ( 2.292384291596425427, -0.9864983578860975211, 2.086231237977907327 ) ) ;
#35560 = CARTESIAN_POINT ( 'NONE',  ( 5.079397637315079983, 1.924335792300538861, -0.7379084467255945246 ) ) ;
#35561 = CARTESIAN_POINT ( 'NONE',  ( 0.3044966626061855752, 1.689057509992748729, 0.9581197715371556622 ) ) ;
#35562 = CARTESIAN_POINT ( 'NONE',  ( -7.659993601596720936, 8.999375959026737704, -1.082531754730543083 ) ) ;
#35563 = CARTESIAN_POINT ( 'NONE',  ( -6.168033539574333979, 6.160736982450306876, 0.7998128361456281477 ) ) ;
#35564 = CARTESIAN_POINT ( 'NONE',  ( -0.2110808730067274541, 0.0005491059566040365795, -1.796958327270286704 ) ) ;
#35565 = SURFACE_STYLE_FILL_AREA ( #150412 ) ;
#35566 = CARTESIAN_POINT ( 'NONE',  ( 1.617814789376757156, 0.2004366740697149929, 2.006445999502483257 ) ) ;
#35567 = CARTESIAN_POINT ( 'NONE',  ( -6.683806541412776525, 7.860491055478785682, -1.082531754730543083 ) ) ;
#35568 = ADVANCED_FACE ( 'NONE', ( #145231 ), #63932, .F. ) ;
#35569 = CARTESIAN_POINT ( 'NONE',  ( 3.909358855915114006, 1.891329263188616938, 1.136761501516952766 ) ) ;
#35570 = CARTESIAN_POINT ( 'NONE',  ( 1.642778471875000035, -1.363541666188707646, -2.845375778867859751 ) ) ;
#35571 = CARTESIAN_POINT ( 'NONE',  ( 1.340418531419234505, -1.814007083311576451, -0.4145509422008378242 ) ) ;
#35572 = CARTESIAN_POINT ( 'NONE',  ( -0.02880301295725678015, 0.2243704974793322426, -2.307247863525173859 ) ) ;
#35573 = DIRECTION ( 'NONE',  ( 5.551115123125764213E-17, 0.000000000000000000, -1.000000000000000000 ) ) ;
#35574 = DIRECTION ( 'NONE',  ( 0.8660254037844411501, -0.4999999999999956146, -5.551115123125779621E-17 ) ) ;
#35576 = CARTESIAN_POINT ( 'NONE',  ( 6.925078400183534377, -0.01048729610059369148, 2.244148362790527429 ) ) ;
#35575 = CARTESIAN_POINT ( 'NONE',  ( -4.953783236630994402, 8.080086878320878796, -1.094444140625696837 ) ) ;
#35577 = CARTESIAN_POINT ( 'NONE',  ( 1.224999999999991651, 2.124999999999967137, -3.469446951953614189E-14 ) ) ;
#35578 = ORIENTED_EDGE ( 'NONE', *, *, #31325, .F. ) ;
#35579 = CARTESIAN_POINT ( 'NONE',  ( 3.045831416509756195, 0.7432089164593397301, -1.922393172558758634 ) ) ;
#35580 = CARTESIAN_POINT ( 'NONE',  ( -0.6801582343750004478, 2.348958333674739052, -1.178068619123869398 ) ) ;
#35581 = UNCERTAINTY_MEASURE_WITH_UNIT (LENGTH_MEASURE( 1.000000000000000082E-05 ), #45925, 'distance_accuracy_value', 'NONE');
#35582 = CARTESIAN_POINT ( 'NONE',  ( -5.045605722580076780, 9.038290442985410067, -0.7998128361456231517 ) ) ;
#35583 = CARTESIAN_POINT ( 'NONE',  ( 2.649087060217536926, 0.2492969965636695762, 2.004170148778378735 ) ) ;
#35584 = CARTESIAN_POINT ( 'NONE',  ( -1.500000000000001332, -1.099999999999976108, 0.000000000000000000 ) ) ;
#35585 = CARTESIAN_POINT ( 'NONE',  ( 5.196852952739813070, 4.957416621151553571, -0.7998128361456221525 ) ) ;
#35586 = CARTESIAN_POINT ( 'NONE',  ( 2.219669609025213930, -1.999274383190910775, 0.4996674803129513842 ) ) ;
#35588 = CARTESIAN_POINT ( 'NONE',  ( 1.364683531249996529, 13.21354166700806410, 0.7879004041258405033 ) ) ;
#35587 = FACE_BOUND ( 'NONE', #194547, .T. ) ;
#35589 = CARTESIAN_POINT ( 'NONE',  ( 5.147291874682557555, 9.156924287104992288, 0.7998128361456462443 ) ) ;
#35590 = CARTESIAN_POINT ( 'NONE',  ( -0.2411972340276386517, 4.090764154511560058, -2.455280512047691044 ) ) ;
#35591 = AXIS2_PLACEMENT_3D ( 'NONE', #3408, #120465, #102004 ) ;
#35592 = CARTESIAN_POINT ( 'NONE',  ( 6.024089167411393220, -1.222679950896175205, -1.837027303407394507 ) ) ;
#35593 = CARTESIAN_POINT ( 'NONE',  ( 6.387826650694035990, 7.481494509678370264, -1.199719254218452047 ) ) ;
#35594 = CARTESIAN_POINT ( 'NONE',  ( 1.177287030172860183, -0.05180490295666682898, -2.161124318685260004 ) ) ;
#35595 = CARTESIAN_POINT ( 'NONE',  ( -3.795919822146277767, 7.372397525905215687, -0.7216878364870267237 ) ) ;
#35596 = CARTESIAN_POINT ( 'NONE',  ( 2.167204200501818612, 1.841733140229084853, -0.8216742516050157263 ) ) ;
#35597 = EDGE_CURVE ( 'NONE', #170847, #100853, #55062, .T. ) ;
#35598 = CARTESIAN_POINT ( 'NONE',  ( 2.372814144171823791, -0.5044604469449982531, 2.242205522996820743 ) ) ;
#35599 = EDGE_CURVE ( 'NONE', #94234, #34907, #148623, .T. ) ;
#35600 = CARTESIAN_POINT ( 'NONE',  ( 0.1144128442461203460, 7.018241394329717942, 3.990988525772905859 ) ) ;
#35601 = CARTESIAN_POINT ( 'NONE',  ( 3.132295304332796348, 6.444579696763526933, -0.6078999513244928155 ) ) ;
#35602 = CARTESIAN_POINT ( 'NONE',  ( 2.184254540302111636, -1.834043650784190405, -0.3674020703766100460 ) ) ;
#35603 = CARTESIAN_POINT ( 'NONE',  ( 3.555875268649951959, 1.124244472066991518, 1.673854899288424347 ) ) ;
#35605 = CARTESIAN_POINT ( 'NONE',  ( 11.33772463945037146, 13.39999999999998259, 3.599999999999999201 ) ) ;
#35604 = CARTESIAN_POINT ( 'NONE',  ( 1.364683531249988535, 1.863541667008086211, 0.7879004041258500513 ) ) ;
#35607 = CARTESIAN_POINT ( 'NONE',  ( 5.514326386059018148, -0.9456761151771397866, -1.881892731060728519 ) ) ;
#35606 = CARTESIAN_POINT ( 'NONE',  ( -8.148614017013223076, 9.465470093725620870, -1.199719254218446718 ) ) ;
#35608 = CARTESIAN_POINT ( 'NONE',  ( 5.784525094524856748, 9.900363043587685041, 1.040834085586084257E-14 ) ) ;
#35609 = CARTESIAN_POINT ( 'NONE',  ( -8.064402442030170093, 8.302891025323665630, 0.7998128361456602331 ) ) ;
#35610 = CARTESIAN_POINT ( 'NONE',  ( 6.539320575229256249, 7.052319431262985105, 2.701414634427783845 ) ) ;
#35611 = CARTESIAN_POINT ( 'NONE',  ( 5.045178214694073127, 0.1526089617210572014, 2.014106518579480642 ) ) ;
#35612 = CARTESIAN_POINT ( 'NONE',  ( 0.6823417656249899377, 5.676041667008087543, -1.181850606188754593 ) ) ;
#35613 = CARTESIAN_POINT ( 'NONE',  ( 0.5321751443473606846, 1.184493745614173310, 1.688377367428809173 ) ) ;
#35614 = CARTESIAN_POINT ( 'NONE',  ( 8.785320351975350661, 9.351887953500479966, -0.7216878364870197293 ) ) ;
#35615 = EDGE_CURVE ( 'NONE', #12329, #167635, #126896, .T. ) ;
#35616 = CARTESIAN_POINT ( 'NONE',  ( 4.830447868218803897, 8.857549289555754157, -0.7998128361456481317 ) ) ;
#35617 = CARTESIAN_POINT ( 'NONE',  ( 6.710359684120930091, 6.793450817754725257, 0.7998128361456352531 ) ) ;
#35618 = CARTESIAN_POINT ( 'NONE',  ( -1.364683531250014514, 0.3010416670080866552, -0.7879004041258359514 ) ) ;
#35619 = CARTESIAN_POINT ( 'NONE',  ( 5.740951700743842423, 5.662474837148078421, -0.7998128361456481317 ) ) ;
#35620 = CARTESIAN_POINT ( 'NONE',  ( 7.009202228140744673, 9.200488570962775725, -1.443375672974058777 ) ) ;
#35622 = CARTESIAN_POINT ( 'NONE',  ( -1.378728738066235859, 3.613591550242559070, -0.5908528300941767730 ) ) ;
#35621 = CARTESIAN_POINT ( 'NONE',  ( 3.350208609569472529, -0.8826205156595956502, 1.983864470818137660 ) ) ;
#35624 = CARTESIAN_POINT ( 'NONE',  ( 2.173174093899932657, 1.133995793187540180, 1.450494936146892622 ) ) ;
#35623 = CARTESIAN_POINT ( 'NONE',  ( -5.450014563013544588, 5.460697866378308341, 0.7216878364870317197 ) ) ;
#35625 = CARTESIAN_POINT ( 'NONE',  ( -1.364683531249997417, 3.009375000341422801, 1.214306433183764966E-14 ) ) ;
#35626 = CARTESIAN_POINT ( 'NONE',  ( 3.931328349035985603, -1.512150646884598215, -1.586510368271301541 ) ) ;
#35627 = CARTESIAN_POINT ( 'NONE',  ( 6.883263157960357148, 2.018753856957363535, 2.456789959645651500 ) ) ;
#35628 = CARTESIAN_POINT ( 'NONE',  ( 4.399490234458226290, 1.814852776126129497, 1.350843829522253792 ) ) ;
#35629 = CARTESIAN_POINT ( 'NONE',  ( -5.693534442735004752, 8.729875052244421951, 1.199719254218452047 ) ) ;
#35630 = DIRECTION ( 'NONE',  ( 0.000000000000000000, 0.000000000000000000, -1.000000000000000000 ) ) ;
#35631 = CARTESIAN_POINT ( 'NONE',  ( 4.730098472736550264, 8.327237590489470875, -0.7222317683119976461 ) ) ;
#35632 = CIRCLE ( 'NONE', #115343, 0.05000000000000056483 ) ;
#35633 = CARTESIAN_POINT ( 'NONE',  ( -6.929625909916163451, 7.257187447756535903, 0.7216878364870317197 ) ) ;
#35634 = CARTESIAN_POINT ( 'NONE',  ( 4.421367491832270957, 6.251624388594711590, 1.443375672974058777 ) ) ;
#35635 = CARTESIAN_POINT ( 'NONE',  ( 0.1273423419134401269, -1.083036363347224418, -1.400124042496312615 ) ) ;
#35636 = CARTESIAN_POINT ( 'NONE',  ( 3.317044347720001785, 1.585670248135360838, -1.240117154037506886 ) ) ;
#35637 = CARTESIAN_POINT ( 'NONE',  ( 6.272618624616828953, 10.46980549536166016, 1.040834085586084257E-14 ) ) ;
#35638 = CARTESIAN_POINT ( 'NONE',  ( 1.958176110230916755, 2.100372442369624171, -0.1540336313638566157 ) ) ;
#35639 = CARTESIAN_POINT ( 'NONE',  ( 1.159628707424670280, 1.142309718407741093, 1.537566464135895261 ) ) ;
#35641 = CARTESIAN_POINT ( 'NONE',  ( 1.499999999999989120, 2.504166666666687302, 0.8660254037844524744 ) ) ;
#35640 = CARTESIAN_POINT ( 'NONE',  ( -8.012344526598182026E-15, 12.54687500034139624, -1.575800808251669460 ) ) ;
#35642 = CARTESIAN_POINT ( 'NONE',  ( 1.820693447614455618, -1.395048584331352703, 1.390583823087336857 ) ) ;
#35643 = CARTESIAN_POINT ( 'NONE',  ( 0.6548940681232479077, -1.578012236938080015, -1.004313744925364071 ) ) ;
#35644 = CARTESIAN_POINT ( 'NONE',  ( 0.6780837441340243910, -1.046368970337024473, -1.659334490400856454 ) ) ;
#35646 = ORIENTED_EDGE ( 'NONE', *, *, #197756, .T. ) ;
#35645 = CARTESIAN_POINT ( 'NONE',  ( 0.01762790050853849447, -0.5081247445114078776, 1.843608005305336528 ) ) ;
#35647 = CARTESIAN_POINT ( 'NONE',  ( 6.073689629242148058, 8.109057205581079231, -1.443375672974057666 ) ) ;
#35648 = CARTESIAN_POINT ( 'NONE',  ( -0.6823417656250003738, 0.7802083336747520637, -1.181850606188749264 ) ) ;
#35649 = CARTESIAN_POINT ( 'NONE',  ( 6.121928861531041655, -1.040746078065577063, -1.554202398018275755 ) ) ;
#35650 = CARTESIAN_POINT ( 'NONE',  ( -6.277139874739040337, -0.02379966007286238305, 0.000000000000000000 ) ) ;
#35651 = STYLED_ITEM ( 'NONE', ( #47325 ), #80971 ) ;
#35652 = CARTESIAN_POINT ( 'NONE',  ( 5.752806990244247132, -0.4974732019265227234, -2.009498513695342936 ) ) ;
#35653 = AXIS2_PLACEMENT_3D ( 'NONE', #50688, #202246, #153536 ) ;
#35654 = CARTESIAN_POINT ( 'NONE',  ( 1.347111479062088799E-15, -0.9200000000000041478, -11.00000000000000178 ) ) ;
#35655 = CARTESIAN_POINT ( 'NONE',  ( -5.600926855776901192, 5.707038551260711579, -0.7216878364870338292 ) ) ;
#35656 = CARTESIAN_POINT ( 'NONE',  ( 0.2209699231256057605, -0.9756392058242843168, 3.445770853192297256 ) ) ;
#35657 = CARTESIAN_POINT ( 'NONE',  ( -1.500000000000013101, 0.6708333333333583726, 0.8660254037844403729 ) ) ;
#35658 = CARTESIAN_POINT ( 'NONE',  ( 7.751511138711133064, 10.06651563329490529, -1.599625672291262513 ) ) ;
#35659 = CARTESIAN_POINT ( 'NONE',  ( -8.479735010343349089, 11.98044238112085758, 1.199719254218453823 ) ) ;
#35660 = CARTESIAN_POINT ( 'NONE',  ( 4.667750024854814050, 8.667735138964429709, -0.7998128361456381397 ) ) ;
#35661 = CARTESIAN_POINT ( 'NONE',  ( -1.201851678989727383E-14, 0.8218750003414171390, 1.575800808251672791 ) ) ;
#35662 = VERTEX_POINT ( 'NONE', #33562 ) ;
#35663 = CARTESIAN_POINT ( 'NONE',  ( -1.500000000000013101, 2.420833333333359150, 0.8660254037844403729 ) ) ;
#35665 = CARTESIAN_POINT ( 'NONE',  ( 4.039439701867726384, 6.800097854565950506, 1.199719254218462483 ) ) ;
#35664 = CARTESIAN_POINT ( 'NONE',  ( 5.353941776413853937, -0.7077614321437855072, 1.829919609802006741 ) ) ;
#35666 = CARTESIAN_POINT ( 'NONE',  ( 2.636092105226188309, 0.1017362925337349233, -2.013677536115268563 ) ) ;
#35667 = ADVANCED_FACE ( 'NONE', ( #1033 ), #82303, .T. ) ;
#35668 = CARTESIAN_POINT ( 'NONE',  ( 2.202218669689899322, 1.248139960717888908, -1.453441320886917243 ) ) ;
#35669 = CARTESIAN_POINT ( 'NONE',  ( -1.913843478179648727, 3.256154753185184880, -0.4414708703500292430 ) ) ;
#35670 = AXIS2_PLACEMENT_3D ( 'NONE', #156382, #76181, #192046 ) ;
#35671 = CARTESIAN_POINT ( 'NONE',  ( 0.8377433530848135135, 0.8832496248250313320, -2.005872107257236969 ) ) ;
#35672 = CARTESIAN_POINT ( 'NONE',  ( 0.1333692844072559558, 0.7140749627707367875, -2.136770008611441618 ) ) ;
#35673 = CARTESIAN_POINT ( 'NONE',  ( 3.567518508692040236, 1.825626599287116791, -0.4067673385957787380 ) ) ;
#35674 = CARTESIAN_POINT ( 'NONE',  ( 1.499999999999987566, -0.6937499993171849511, 0.000000000000000000 ) ) ;
#35675 = CARTESIAN_POINT ( 'NONE',  ( -8.182509401047415309, 9.505014708432145909, 1.199719254218462483 ) ) ;
#35677 = CARTESIAN_POINT ( 'NONE',  ( 4.710634317702605323, 2.026528413205666013, 0.6131292256000410168 ) ) ;
#35676 = CARTESIAN_POINT ( 'NONE',  ( -4.772106882330234612, 6.590544000850479200, -1.443375672974053447 ) ) ;
#35678 = CARTESIAN_POINT ( 'NONE',  ( -0.09999999999991612820, -10.00000000000009592, -9.579478065114042096 ) ) ;
#35679 = CARTESIAN_POINT ( 'NONE',  ( 5.670397268163976712, -0.9275489576153757021, -1.851018422006404096 ) ) ;
#35681 = CARTESIAN_POINT ( 'NONE',  ( -6.138551946455282682, 6.334268068046505107, -0.2462770601040304153 ) ) ;
#35680 = CARTESIAN_POINT ( 'NONE',  ( 0.9782033901477287241, -2.040585271250746846, -0.4545043172074214599 ) ) ;
#35683 = ORIENTED_EDGE ( 'NONE', *, *, #4802, .F. ) ;
#35682 = CARTESIAN_POINT ( 'NONE',  ( 0.4809449578498920519, 1.612012756419522352, -0.6139154093185476002 ) ) ;
#35684 = CARTESIAN_POINT ( 'NONE',  ( 7.558834334818744338, 8.777393797832065303, 1.199719254218462483 ) ) ;
#35685 = CIRCLE ( 'NONE', #184419, 0.07999999999999998779 ) ;
#35686 = CARTESIAN_POINT ( 'NONE',  ( 7.903135977162644821, 15.38542563725095746, 9.031658180448362216 ) ) ;
#35687 = CARTESIAN_POINT ( 'NONE',  ( -0.08044988649999126884, -9.906619926850268598, -9.499659352616909302 ) ) ;
#35688 = CARTESIAN_POINT ( 'NONE',  ( -9.505648412044632067, 5.017053549588888828, 6.783778555801666776 ) ) ;
#35689 = CARTESIAN_POINT ( 'NONE',  ( 7.307481607641395094, 8.588111966078864512, -1.082531754730537976 ) ) ;
#35690 = DIRECTION ( 'NONE',  ( -5.578564026256490882E-16, -1.000000000000000000, -9.066213480720158442E-32 ) ) ;
#35692 = CARTESIAN_POINT ( 'NONE',  ( 0.4163052458206939477, -0.6087807487058238820, -1.706225765549937545 ) ) ;
#35691 = CARTESIAN_POINT ( 'NONE',  ( 6.318982112420993502, 9.529840343536603697, -1.199719254218452047 ) ) ;
#35693 = CARTESIAN_POINT ( 'NONE',  ( -6.672584156219988571, 10.93643194889866521, -0.7998128361456291469 ) ) ;
#35694 = CARTESIAN_POINT ( 'NONE',  ( 4.059776932288224671, 6.823824623389866950, 1.199719254218462483 ) ) ;
#35695 = CARTESIAN_POINT ( 'NONE',  ( -5.200254360346833415, 7.740598053885397789, 1.191768289972208628 ) ) ;
#35696 = CARTESIAN_POINT ( 'NONE',  ( 5.905458427204159477, 9.047396044116986502, 1.199719254218452047 ) ) ;
#35697 = CARTESIAN_POINT ( 'NONE',  ( -7.055228938194283650, -8.176568542494891290, 6.396834479292372144 ) ) ;
#35698 = CARTESIAN_POINT ( 'NONE',  ( 9.499668754385636404, -7.246166700194470067, 0.07933194154488391880 ) ) ;
#35699 = CARTESIAN_POINT ( 'NONE',  ( 10.23604278863759909, 11.04439746293979496, 0.000000000000000000 ) ) ;
#35700 = VERTEX_POINT ( 'NONE', #165700 ) ;
#35701 = CARTESIAN_POINT ( 'NONE',  ( 6.011342256177334420, -1.897693555989588887, 0.6820111564242032909 ) ) ;
#35702 = CARTESIAN_POINT ( 'NONE',  ( 0.8387270772249322270, 1.259995426201226953, -1.705408266269872630 ) ) ;
#35703 = CARTESIAN_POINT ( 'NONE',  ( -3.009160446454586690, 6.366307309526169966, -0.7771143261618658205 ) ) ;
#35704 = PRODUCT_DEFINITION_CONTEXT ( 'detailed design', #63005, 'design' ) ;
#35705 = CARTESIAN_POINT ( 'NONE',  ( 2.274369412726469530, 5.658954245771043112, 0.5045856980266817393 ) ) ;
#35706 = CARTESIAN_POINT ( 'NONE',  ( -1.548913609767783806, 8.694120146927671655, -2.506286796689249030 ) ) ;
#35707 = CARTESIAN_POINT ( 'NONE',  ( -3.443407828190963915, 6.961133532957338943, 0.7216878364870317197 ) ) ;
#35708 = CARTESIAN_POINT ( 'NONE',  ( 8.080296364064698977, 12.37083682481011060, -0.7216878364870328300 ) ) ;
#35709 = CARTESIAN_POINT ( 'NONE',  ( 3.713681502677267154, 0.4829771288026918907, -1.909149233777557075 ) ) ;
#35710 = CARTESIAN_POINT ( 'NONE',  ( 1.418772191123615078, -0.7664089246972278779, -1.977313068770427451 ) ) ;
#35711 = CARTESIAN_POINT ( 'NONE',  ( -4.880045225915050189, 7.780804299287790826, 1.199719254218464037 ) ) ;
#35712 = CARTESIAN_POINT ( 'NONE',  ( -11.77172135380034490, 8.649151653032827625, -2.103707379449156978 ) ) ;
#35714 = EDGE_CURVE ( 'NONE', #99612, #192043, #172583, .T. ) ;
#35713 = CARTESIAN_POINT ( 'NONE',  ( 6.727182134110202938, 2.016807574165893513, 2.492494991173601182 ) ) ;
#35715 = CARTESIAN_POINT ( 'NONE',  ( 6.052700813158569559, -1.877759139263988297, -1.129571069393126459 ) ) ;
#35716 = DIRECTION ( 'NONE',  ( 0.000000000000000000, 1.000000000000000000, 0.000000000000000000 ) ) ;
#35717 = CARTESIAN_POINT ( 'NONE',  ( 3.979452554116496898, 1.814262220864255815, -0.6480193189529972475 ) ) ;
#35718 = CARTESIAN_POINT ( 'NONE',  ( -8.681298431451969222, 9.022603012982438386, 1.040834085586084257E-14 ) ) ;
#35719 = CARTESIAN_POINT ( 'NONE',  ( -0.1298852118744100725, 7.629137130509058728, -2.326516543997098729 ) ) ;
#35720 = CARTESIAN_POINT ( 'NONE',  ( 1.348561525465460820, 2.204488851003219896, 0.1053889787279923829 ) ) ;
#35721 = CARTESIAN_POINT ( 'NONE',  ( 5.508226607891452353, 6.381517327172165466, -1.198580242432255583 ) ) ;
#35722 = ORIENTED_EDGE ( 'NONE', *, *, #194119, .F. ) ;
#35723 = CARTESIAN_POINT ( 'NONE',  ( 4.014622883422321209, 5.777089012116397804, -1.443375672974068769 ) ) ;
#35724 = CARTESIAN_POINT ( 'NONE',  ( 6.561384255921438147, 1.635440365473137536, 1.096959908523033711 ) ) ;
#35725 = CARTESIAN_POINT ( 'NONE',  ( 0.5560688330792910028, -1.405822068596472407, 1.340092691751965770 ) ) ;
#35726 = CARTESIAN_POINT ( 'NONE',  ( 6.081499288503829703, 1.550124037452194958, -1.697122508851423905 ) ) ;
#35728 = CARTESIAN_POINT ( 'NONE',  ( 4.153051346612735450, 1.574026050290713963, -0.9924080308383613769 ) ) ;
#35727 = CARTESIAN_POINT ( 'NONE',  ( -6.577640801285370209, 7.702944352034914566, -1.199719254218452047 ) ) ;
#35729 = CARTESIAN_POINT ( 'NONE',  ( 6.038177310039780643, 8.137902509836795417, -1.599625672291283607 ) ) ;
#35731 = EDGE_CURVE ( 'NONE', #29554, #172976, #51500, .T. ) ;
#35730 = FACE_OUTER_BOUND ( 'NONE', #94145, .T. ) ;
#35732 = SURFACE_STYLE_USAGE ( .BOTH. , #119185 ) ;
#35733 = CARTESIAN_POINT ( 'NONE',  ( -4.880045225915050189, 7.780804299287790826, 1.199719254218464037 ) ) ;
#35734 = CARTESIAN_POINT ( 'NONE',  ( 6.720655732516647163, 3.705577233864749243, 2.340827588962008043 ) ) ;
#35735 = CARTESIAN_POINT ( 'NONE',  ( 6.567919234911265391, -1.285863816539883908, 1.649083965234589000 ) ) ;
#35736 = CARTESIAN_POINT ( 'NONE',  ( 4.853455804012216213, 6.685451076146141425, 1.443375672974062551 ) ) ;
#35737 = ORIENTED_EDGE ( 'NONE', *, *, #128001, .T. ) ;
#35738 = CARTESIAN_POINT ( 'NONE',  ( 10.14375151705082878, -9.181160345032706616, -0.1770598413457902254 ) ) ;
#35739 = DIRECTION ( 'NONE',  ( 0.3090169943749516146, 0.000000000000000000, 0.9510565162951523099 ) ) ;
#35740 = CARTESIAN_POINT ( 'NONE',  ( 0.5393321728033516615, -1.288848960320065462, -1.293324666950084190 ) ) ;
#35741 = CARTESIAN_POINT ( 'NONE',  ( -4.894657149733403045, 5.669187081899118574, -1.199719254218446718 ) ) ;
#35742 = VECTOR ( 'NONE', #149309, 1000.000000000000000 ) ;
#35743 = CARTESIAN_POINT ( 'NONE',  ( 2.496349097179047405, -1.714988558773246741, 0.2561001183170578677 ) ) ;
#35744 = CARTESIAN_POINT ( 'NONE',  ( 1.224999999999955014, 1.958333334016109095, -0.7072540797573237947 ) ) ;
#35745 = CARTESIAN_POINT ( 'NONE',  ( -11.04536101718726293, 10.19999999999999929, -1.100000000000000311 ) ) ;
#35746 = CARTESIAN_POINT ( 'NONE',  ( -3.973948422136983183, 7.650373902552822791, -0.7216878364870569218 ) ) ;
#35747 = VECTOR ( 'NONE', #110270, 1000.000000000000000 ) ;
#35748 = CARTESIAN_POINT ( 'NONE',  ( 6.533835636172961259, -1.196796279342365210, -1.378804128639096849 ) ) ;
#35749 = CARTESIAN_POINT ( 'NONE',  ( 2.834756127989654484, -1.875839772035441388, -0.5741054328185363209 ) ) ;
#35750 = CARTESIAN_POINT ( 'NONE',  ( 0.6124999999999723999, -0.1041666659838680342, 1.060881119635899816 ) ) ;
#35751 = CARTESIAN_POINT ( 'NONE',  ( -8.748035429315585532, 11.22912730566677553, -1.599625672291263179 ) ) ;
#35752 = CARTESIAN_POINT ( 'NONE',  ( 4.611744806942754238, 8.532119374741881757, -0.7998128361456231517 ) ) ;
#35753 = CARTESIAN_POINT ( 'NONE',  ( 4.688201205076114597, 1.221562550966972527, 1.733079268972044895 ) ) ;
#35754 = CARTESIAN_POINT ( 'NONE',  ( 8.005163354226054295, 8.304055099544019214, 0.000000000000000000 ) ) ;
#35755 = CARTESIAN_POINT ( 'NONE',  ( -8.435144125996554720, 12.99275191363802229, 0.7998128361456341429 ) ) ;
#35756 = ADVANCED_FACE ( 'NONE', ( #98574 ), #103444, .T. ) ;
#35757 = CARTESIAN_POINT ( 'NONE',  ( 2.465759480183654428, -0.4578044685884518072, 2.018832516862689275 ) ) ;
#35759 = CARTESIAN_POINT ( 'NONE',  ( 1.364683531249988757, -0.3031249996585799744, 0.000000000000000000 ) ) ;
#35758 = CARTESIAN_POINT ( 'NONE',  ( 6.827182134110246103, 3.705739211453744630, 2.325493694733235195 ) ) ;
#35761 = EDGE_LOOP ( 'NONE', ( #118774, #64947, #176888, #139517 ) ) ;
#35760 = CARTESIAN_POINT ( 'NONE',  ( 4.846434531455360073, 1.142681229152305633, -1.904705486840562179 ) ) ;
#35762 = CARTESIAN_POINT ( 'NONE',  ( 2.514614159817552430, -2.143548176638510938, 0.8305585572774812908 ) ) ;
#35763 = CARTESIAN_POINT ( 'NONE',  ( 9.083599731475992201, 9.699880562917908122, 0.7216878364870438212 ) ) ;
#35765 = CARTESIAN_POINT ( 'NONE',  ( -1.642778471874998480, -1.801041666188708090, 2.845375778867863303 ) ) ;
#35764 = CARTESIAN_POINT ( 'NONE',  ( 6.699137298928145690, 8.909022496873262753, 1.443375672974065660 ) ) ;
#35766 =( LENGTH_UNIT ( ) NAMED_UNIT ( * ) SI_UNIT ( .MILLI., .METRE. ) );
#35767 = CARTESIAN_POINT ( 'NONE',  ( -10.66822795754452358, 4.187511268866498604, 5.495200216426709083 ) ) ;
#35768 = EDGE_LOOP ( 'NONE', ( #120296, #8957, #173232, #190200 ) ) ;
#35769 = DIRECTION ( 'NONE',  ( 1.276756478318932585E-15, -1.000000000000000000, 1.665334536937738262E-16 ) ) ;
#35770 = CARTESIAN_POINT ( 'NONE',  ( 3.691585721427274258, 1.799035686688513325, -0.6489376663148455071 ) ) ;
#35771 = CARTESIAN_POINT ( 'NONE',  ( -0.4536928783070027782, 6.573802805905836877, -3.398403741207694395 ) ) ;
#35772 = CARTESIAN_POINT ( 'NONE',  ( 3.856244308521704411, 0.6209911617112495730, 1.609288963722750765 ) ) ;
#35773 = CARTESIAN_POINT ( 'NONE',  ( 3.432827581131673522, -1.645759781613131967, 1.164986487700324425 ) ) ;
#35774 = CARTESIAN_POINT ( 'NONE',  ( 4.061395409788411293, -1.323216277904919691, 1.879509618897465817 ) ) ;
#35775 = CARTESIAN_POINT ( 'NONE',  ( -11.43190902327450509, 12.44477871742144615, -3.649704988378223991 ) ) ;
#35776 = CARTESIAN_POINT ( 'NONE',  ( 6.393207918867057415, 1.833407501889987357, -1.036277073347695588 ) ) ;
#35777 = CARTESIAN_POINT ( 'NONE',  ( -6.482206841109545259, 6.735198534148810090, 0.7216878364870257245 ) ) ;
#35778 = CARTESIAN_POINT ( 'NONE',  ( 4.921055611120458195, -0.08698325021493956422, 1.767741905644197642 ) ) ;
#35780 = CARTESIAN_POINT ( 'NONE',  ( 0.4281777144111223454, 1.173252442481845126, -1.969132371278771831 ) ) ;
#35779 = CARTESIAN_POINT ( 'NONE',  ( 6.496291879603339758, 7.608037276739255006, 1.199719254218452935 ) ) ;
#35781 = CARTESIAN_POINT ( 'NONE',  ( -0.02988540731103071432, 0.005807295984020746475, -1.726291166677936362 ) ) ;
#35782 = CARTESIAN_POINT ( 'NONE',  ( -7.391130018105325661, 8.652015104991543026, -1.199719254218452047 ) ) ;
#35783 = CARTESIAN_POINT ( 'NONE',  ( 6.714806894218784628, -0.1628439675423892508, 2.155775914164249407 ) ) ;
#35784 = CARTESIAN_POINT ( 'NONE',  ( -5.164730172163054966, 4.990216387137135889, -0.7998128361456362523 ) ) ;
#35785 = CARTESIAN_POINT ( 'NONE',  ( -1.752700365193352367E-14, -0.3906249996585918205, -1.570758158831796258 ) ) ;
#35786 = CARTESIAN_POINT ( 'NONE',  ( 9.499668754385638181, -7.559700871049417792, 0.07933194154488390493 ) ) ;
#35787 = CARTESIAN_POINT ( 'NONE',  ( 6.848098043024292814, -0.8888149443028300345, 1.868052569137634400 ) ) ;
#35788 = CARTESIAN_POINT ( 'NONE',  ( 1.358611653602972646, -1.916354379050893009, -0.6279873632355145174 ) ) ;
#35789 = CARTESIAN_POINT ( 'NONE',  ( -1.402160292154681736E-14, 0.1187500006828157706, -1.732050807568870754 ) ) ;
#35790 = CARTESIAN_POINT ( 'NONE',  ( 5.057218277682078877, -1.628452160524866521, -1.029070375190293873 ) ) ;
#35791 = CARTESIAN_POINT ( 'NONE',  ( -0.6823417656250039265, 11.81770833367473017, -1.181850606188755259 ) ) ;
#35792 = CARTESIAN_POINT ( 'NONE',  ( 1.318920400837508167, -0.8056321388932115024, -2.070341401348996691 ) ) ;
#35793 = ORIENTED_EDGE ( 'NONE', *, *, #196420, .T. ) ;
#35795 = CARTESIAN_POINT ( 'NONE',  ( -1.244123718695710368, 3.223244533904601195, 0.7750000000000100142 ) ) ;
#35794 = FILL_AREA_STYLE ('',( #118186 ) ) ;
#35796 = CARTESIAN_POINT ( 'NONE',  ( 1.559647396048226220, -1.374772708486730943, 1.500000000000001332 ) ) ;
#35797 = CARTESIAN_POINT ( 'NONE',  ( 8.041957671200231417, 12.53403438304231976, 1.040834085586084257E-14 ) ) ;
#35798 = FILL_AREA_STYLE_COLOUR ( '', #38802 ) ;
#35799 = DIRECTION ( 'NONE',  ( 0.000000000000000000, 0.000000000000000000, 1.000000000000000000 ) ) ;
#35800 = CARTESIAN_POINT ( 'NONE',  ( 4.598987173745545221, -0.4583060902535853187, 1.678952109248931901 ) ) ;
#35801 = CARTESIAN_POINT ( 'NONE',  ( 2.980854556682940082, 1.846358069237159949, 0.6635599008937702603 ) ) ;
#35803 = CARTESIAN_POINT ( 'NONE',  ( -1.201851678989727383E-14, 2.384375000341416584, 1.575800808251672791 ) ) ;
#35802 = CARTESIAN_POINT ( 'NONE',  ( 3.011882680530176604, 6.665613560593854459, 0.7998128361456341429 ) ) ;
#35804 = CARTESIAN_POINT ( 'NONE',  ( -2.324088772396477673E-16, -2.143749999044084031, -3.475000000000000089 ) ) ;
#35805 = AXIS2_PLACEMENT_3D ( 'NONE', #93466, #121758, #122842 ) ;
#35806 = VECTOR ( 'NONE', #121635, 1000.000000000000000 ) ;
#35807 = CARTESIAN_POINT ( 'NONE',  ( 0.2388349330707796314, -2.000390574439359526, -0.5026286349697464129 ) ) ;
#35808 = CARTESIAN_POINT ( 'NONE',  ( -7.832860060393135093, 10.16142270859057462, 1.599625672291295375 ) ) ;
#35809 = CARTESIAN_POINT ( 'NONE',  ( -5.070386261386537363, 5.017798181146802428, 1.214306433183764966E-14 ) ) ;
#35810 = CARTESIAN_POINT ( 'NONE',  ( 5.471888747823221877, -0.9023485654677811940, 1.803414228490702209 ) ) ;
#35811 = CARTESIAN_POINT ( 'NONE',  ( 1.253188901120566134, -1.782426524439745030, 1.393456103103172250 ) ) ;
#35812 = ORIENTED_EDGE ( 'NONE', *, *, #50840, .F. ) ;
#35813 = CARTESIAN_POINT ( 'NONE',  ( -0.7500000000000249800, -0.5270833326505158789, 1.299038105676659116 ) ) ;
#35814 = CARTESIAN_POINT ( 'NONE',  ( 3.110468855859845672, 1.357358932127524120, -1.287316363804760888 ) ) ;
#35815 = CARTESIAN_POINT ( 'NONE',  ( 1.511953044659793077, -1.632839461445406481, 0.5843666143663208690 ) ) ;
#35816 = AXIS2_PLACEMENT_3D ( 'NONE', #26035, #141972, #207984 ) ;
#35817 = CARTESIAN_POINT ( 'NONE',  ( 5.108995794240286159, -0.3219066699026683631, 2.167653318578148358 ) ) ;
#35818 = CARTESIAN_POINT ( 'NONE',  ( 5.157380949817064852, -1.946147191792221953, -1.239698497533547661 ) ) ;
#35819 = CARTESIAN_POINT ( 'NONE',  ( 0.9364841293936125854, 2.030268333626069843, 0.3529954148920669277 ) ) ;
#35820 = CARTESIAN_POINT ( 'NONE',  ( 3.925673184153520179, 1.037972095618071133, -1.641099617876127015 ) ) ;
#35821 = CARTESIAN_POINT ( 'NONE',  ( -3.267151830768946663, 6.755501535964989479, -0.7216878364870257245 ) ) ;
#35822 = CARTESIAN_POINT ( 'NONE',  ( 6.010993879215096314, 1.649516084216671397, 0.8821100558755522458 ) ) ;
#35823 = CARTESIAN_POINT ( 'NONE',  ( 4.128490713069958851, 7.423566268403333446, -0.7082486411538677640 ) ) ;
#35824 = CARTESIAN_POINT ( 'NONE',  ( 6.731795954091533751, -1.842168972580451314, -0.8196458303668037182 ) ) ;
#35825 = CARTESIAN_POINT ( 'NONE',  ( -1.360316468750044638, 1.411458333674720622, 0.7853790794158801436 ) ) ;
#35826 = CARTESIAN_POINT ( 'NONE',  ( 4.043592392309851569, -1.492256208629010761, 1.356298961253152413 ) ) ;
#35827 = CARTESIAN_POINT ( 'NONE',  ( -2.602802303699316866, 5.980427087717073320, 1.040834085586084257E-14 ) ) ;
#35828 = CARTESIAN_POINT ( 'NONE',  ( 7.099665995050449041, 11.43469409420089455, 0.7998128361456462443 ) ) ;
#35829 = CARTESIAN_POINT ( 'NONE',  ( 5.415556014015861841, 5.282846535965431300, -0.7998128361456481317 ) ) ;
#35831 = DIRECTION ( 'NONE',  ( 0.000000000000000000, -1.000000000000000000, 0.000000000000000000 ) ) ;
#35830 = CARTESIAN_POINT ( 'NONE',  ( 1.840199252755945425, 1.805614550920462635, 0.2691313018618191055 ) ) ;
#35832 = CARTESIAN_POINT ( 'NONE',  ( -4.773352600463090845, 7.726605912919016106, 1.199719254218452935 ) ) ;
#35833 = CARTESIAN_POINT ( 'NONE',  ( -4.817943484809862120, 6.714296380401858499, 1.599625672291263401 ) ) ;
#35834 = CARTESIAN_POINT ( 'NONE',  ( -10.43230948805442893, 5.066484524551064794, 5.254757398418679060 ) ) ;
#35835 = ORIENTED_EDGE ( 'NONE', *, *, #109210, .F. ) ;
#35836 = CARTESIAN_POINT ( 'NONE',  ( -5.112833325684908559, 8.018703742390766109, -1.082531754730549967 ) ) ;
#35837 = CARTESIAN_POINT ( 'NONE',  ( -3.440018289565379028, 5.036440642624797626, 1.599625672291267398 ) ) ;
#35838 = CARTESIAN_POINT ( 'NONE',  ( -7.323375529675950624, 11.69568855126397011, -0.7998128361456291469 ) ) ;
#35839 = CARTESIAN_POINT ( 'NONE',  ( 5.461584154626091703, -1.593396655685812124, -1.240940796477793873 ) ) ;
#35840 = CARTESIAN_POINT ( 'NONE',  ( 6.633471381225481522, -0.1569934505771773126, 2.186332552071496682 ) ) ;
#35841 = CARTESIAN_POINT ( 'NONE',  ( -6.261886844665283114, 8.398896966899865646, 1.599625672291269396 ) ) ;
#35842 = CARTESIAN_POINT ( 'NONE',  ( 6.193377243344257543, 6.120028293523423812, -0.7998128361456281477 ) ) ;
#35843 = CARTESIAN_POINT ( 'NONE',  ( 5.629779042149522184, -1.305697561153400965, -1.594503516446880154 ) ) ;
#35844 = CARTESIAN_POINT ( 'NONE',  ( 4.957657809308734898, -1.899617967926207740, -0.6767155953601931007 ) ) ;
#35845 = EDGE_LOOP ( 'NONE', ( #51045, #178776, #21247, #35835 ) ) ;
#35846 = VERTEX_POINT ( 'NONE', #100693 ) ;
#35847 = CARTESIAN_POINT ( 'NONE',  ( -6.471393748265563239, 5.229711127717889596, 2.499999999999998668 ) ) ;
#35848 = CARTESIAN_POINT ( 'NONE',  ( 3.297657676621871925, 4.870353260857385180, 1.599625672291267398 ) ) ;
#35849 = B_SPLINE_CURVE_WITH_KNOTS ( 'NONE', 3,
 ( #39463, #170524, #105559, #22107, #24257, #169461, #204059, #8015 ),
 .UNSPECIFIED., .F., .F.,
 ( 4, 2, 2, 4 ),
 ( 0.000000000000000000, 0.0005156231957999669446, 0.0007734347936999512842, 0.001031246391599935624 ),
 .UNSPECIFIED. ) ;
#35851 = ORIENTED_EDGE ( 'NONE', *, *, #57578, .T. ) ;
#35850 = CARTESIAN_POINT ( 'NONE',  ( -4.620296487206990932, 8.612372678375294299, 0.000000000000000000 ) ) ;
#35852 = CARTESIAN_POINT ( 'NONE',  ( 4.601768607255383614, 8.481659704624913587, -0.1707596084408805059 ) ) ;
#35853 = CARTESIAN_POINT ( 'NONE',  ( 5.343124974464078747, -1.122324884721880078, 1.674632237393176792 ) ) ;
#35854 = CARTESIAN_POINT ( 'NONE',  ( 3.644333108393753573, -1.504320797718930791, 1.061230752167609204 ) ) ;
#35855 = CARTESIAN_POINT ( 'NONE',  ( -0.6685859206620391459, -4.211945764156043381, -0.8419752161881570718 ) ) ;
#35856 = CARTESIAN_POINT ( 'NONE',  ( 2.051827946393524726, -1.855052535695273841, -1.372493790568436012 ) ) ;
#35857 = CARTESIAN_POINT ( 'NONE',  ( 6.424584688029230328, 8.588711117491191871, 1.599625672291268286 ) ) ;
#35858 = CARTESIAN_POINT ( 'NONE',  ( 4.640002929648442631, 0.9288797265196678810, -1.951996720969489951 ) ) ;
#35859 = CARTESIAN_POINT ( 'NONE',  ( 8.718056468787178659, 10.12981962079525289, 1.199719254218462483 ) ) ;
#35860 = CARTESIAN_POINT ( 'NONE',  ( 0.4857531807862237594, -1.927505705540471403, -0.2366729787525098105 ) ) ;
#35861 = CARTESIAN_POINT ( 'NONE',  ( -3.764360206088648297, 7.543504007078730922, -0.7998128361456281477 ) ) ;
#35862 = ORIENTED_EDGE ( 'NONE', *, *, #16332, .T. ) ;
#35863 = EDGE_CURVE ( 'NONE', #59826, #169074, #79181, .T. ) ;
#35864 = PRODUCT_DEFINITION ( 'UNKNOWN', '', #204417, #50390 ) ;
#35865 = CARTESIAN_POINT ( 'NONE',  ( 3.814061661026487915, -1.881531058455442329, 1.319806432912509209 ) ) ;
#35866 = CARTESIAN_POINT ( 'NONE',  ( 2.641766398690003292, 0.3984423641809177741, -0.1533590935930815580 ) ) ;
#35867 = CARTESIAN_POINT ( 'NONE',  ( -6.642568916052639771, 6.714361588341672515, 0.000000000000000000 ) ) ;
#35868 = CARTESIAN_POINT ( 'NONE',  ( 3.414787578387419309, 1.690673485743508619, 0.8009127983473337542 ) ) ;
#35869 =( BOUNDED_SURFACE ( )  B_SPLINE_SURFACE ( 3, 2, ( 
 ( #136845, #68606, #54518 ),
 ( #186641, #101118, #83804 ),
 ( #167205, #33993, #18794 ),
 ( #1465, #100067, #67530 ) ),
 .UNSPECIFIED., .F., .F., .T. ) 
 B_SPLINE_SURFACE_WITH_KNOTS ( ( 4, 4 ),
 ( 3, 3 ),
 ( 0.04893088146668654603, 0.05137248493452926251 ),
 ( 0.000000000000000000, 1.000000000000000000 ),
 .UNSPECIFIED. ) 
 GEOMETRIC_REPRESENTATION_ITEM ( )  RATIONAL_B_SPLINE_SURFACE ( (
 ( 1.000000000000000000, 0.7169884966214677968, 1.000000000000000000),
 ( 1.000000000000000000, 0.7174883642158075281, 1.000000000000000000),
 ( 1.000000000000000000, 0.7180610417773349852, 1.000000000000000000),
 ( 1.000000000000000000, 0.7187540717311197147, 1.000000000000000000) ) ) 
 REPRESENTATION_ITEM ( '' )  SURFACE ( )  );
#35870 = CARTESIAN_POINT ( 'NONE',  ( 6.807508289679640612, -0.4357806327412223624, 1.929964574933268340 ) ) ;
#35872 = CARTESIAN_POINT ( 'NONE',  ( -6.448838341955544173, 7.552674816150118708, 1.199719254218452047 ) ) ;
#35871 = CARTESIAN_POINT ( 'NONE',  ( 1.364683531249988535, 5.405208333674750953, -0.7879004041258300672 ) ) ;
#35873 = CARTESIAN_POINT ( 'NONE',  ( 1.559489335033688251, -1.894147805384650995, -1.132260830144316888 ) ) ;
#35874 = CARTESIAN_POINT ( 'NONE',  ( -5.272649268605510642, 6.486664981949695985, 1.286175789206098319 ) ) ;
#35875 = CARTESIAN_POINT ( 'NONE',  ( 3.520313441042647540, 7.258782781191745137, 0.7998128361456321445 ) ) ;
#35876 = CARTESIAN_POINT ( 'NONE',  ( -4.141125853970233806, 6.918731698685530063, -1.199719254218452047 ) ) ;
#35877 = CARTESIAN_POINT ( 'NONE',  ( -7.743115126736118015, 8.206258200713163475, 0.7216878364870317197 ) ) ;
#35878 = CARTESIAN_POINT ( 'NONE',  ( 6.807508289679640612, -0.4357806327412223624, 1.929964574933268340 ) ) ;
#35879 = CARTESIAN_POINT ( 'NONE',  ( 6.709642313893407817, -0.5169605766506181199, 2.257632290342121539 ) ) ;
#35880 = CARTESIAN_POINT ( 'NONE',  ( 1.820681965693775162, -1.389665069980907441, 1.385087887197037571 ) ) ;
#35881 = CARTESIAN_POINT ( 'NONE',  ( 4.662968416576672048, 1.597784760895196721, -1.304382716673627707 ) ) ;
#35882 = CARTESIAN_POINT ( 'NONE',  ( 4.189106276942576201, 7.831115056500907556, 1.040834085586084257E-14 ) ) ;
#35883 = CARTESIAN_POINT ( 'NONE',  ( 6.261886844665240481, 8.398896966899865646, 1.599625672291268286 ) ) ;
#35884 = EDGE_LOOP ( 'NONE', ( #181968, #34145, #150975, #95989 ) ) ;
#35885 = CARTESIAN_POINT ( 'NONE',  ( 7.334597914868727919, 9.580116872145431728, -1.443375672974058777 ) ) ;
#35886 = CARTESIAN_POINT ( 'NONE',  ( -1.364683531250010295, 4.092708333674751842, 0.7879004041258379498 ) ) ;
#35887 = CARTESIAN_POINT ( 'NONE',  ( -4.955918092712652268, 4.886086657537050293, 0.4932186882876873901 ) ) ;
#35888 = CARTESIAN_POINT ( 'NONE',  ( 4.826339496340538382, 4.733076955259818419, 1.040834085586084257E-14 ) ) ;
#35889 = CARTESIAN_POINT ( 'NONE',  ( 6.232918786939658062, -2.059688491082920070, -0.6869823432723211054 ) ) ;
#35890 = DIRECTION ( 'NONE',  ( 1.224646799147343346E-16, 0.000000000000000000, -1.000000000000000000 ) ) ;
#35891 = CARTESIAN_POINT ( 'NONE',  ( 5.545987530334119953, 6.194280231554463612, -0.9208864965579254269 ) ) ;
#35892 = CARTESIAN_POINT ( 'NONE',  ( -11.89321938400721379, 12.33744721639341968, -1.599605898944043147 ) ) ;
#35893 = CARTESIAN_POINT ( 'NONE',  ( 1.756895065592100291, -1.601674646019658255, -0.9660157589584242865 ) ) ;
#35894 = CARTESIAN_POINT ( 'NONE',  ( -4.695247098932518348, 7.056227087241170537, 1.405392365797274445 ) ) ;
#35895 = CARTESIAN_POINT ( 'NONE',  ( 0.000000000000000000, 3.553060279300588320, 0.000000000000000000 ) ) ;
#35896 = CARTESIAN_POINT ( 'NONE',  ( 6.567098404289990476, 6.791591158854626720, -0.3517435911668670423 ) ) ;
#35897 = CARTESIAN_POINT ( 'NONE',  ( 1.364683531249988535, 4.967708333674756283, -0.7879004041258300672 ) ) ;
#35898 = CARTESIAN_POINT ( 'NONE',  ( 1.137202173061176547, -0.04613941135153501460, 1.911881008470908361 ) ) ;
#35899 = CIRCLE ( 'NONE', #156984, 2.000000000000000000 ) ;
#35900 = CARTESIAN_POINT ( 'NONE',  ( 2.711481306777110412, -1.750889404861367460, 0.2573583090697410536 ) ) ;
#35901 = CARTESIAN_POINT ( 'NONE',  ( 1.137202173061176547, -0.04613941135153502154, 1.911881008470908139 ) ) ;
#35902 = AXIS2_PLACEMENT_3D ( 'NONE', #46037, #211696, #108951 ) ;
#35904 = CARTESIAN_POINT ( 'NONE',  ( 4.851152330137978197, 0.1832884931825354280, -1.906798003172151867 ) ) ;
#35903 = CARTESIAN_POINT ( 'NONE',  ( -9.154780037725563702, 11.70366268214508487, 1.599625672291281386 ) ) ;
#35905 = CARTESIAN_POINT ( 'NONE',  ( -1.777638883463106279, 0.9165151389911794233, 1.199999999999999734 ) ) ;
#35906 = CARTESIAN_POINT ( 'NONE',  ( 5.793399386127640049, -1.781339898235247077, 0.8404781526112365952 ) ) ;
#35907 = CARTESIAN_POINT ( 'NONE',  ( 1.090261293813089560, 1.267680250814690934, 1.699812782343253170 ) ) ;
#35908 = FACE_OUTER_BOUND ( 'NONE', #174816, .T. ) ;
#35909 = CARTESIAN_POINT ( 'NONE',  ( 3.485083742438867649, 1.691615344724434200, -0.7988839237506044633 ) ) ;
#35911 = VERTEX_POINT ( 'NONE', #53008 ) ;
#35910 = CARTESIAN_POINT ( 'NONE',  ( 6.709587848829112744, -0.3662258548819911086, 1.691549535187387932 ) ) ;
#35913 = CARTESIAN_POINT ( 'NONE',  ( 3.389175213736297820, 4.977123720824209840, 1.443375672974062551 ) ) ;
#35912 = CARTESIAN_POINT ( 'NONE',  ( 3.387540773601561916, 1.995160029947869340, -0.9435142334218297178 ) ) ;
#35914 = CARTESIAN_POINT ( 'NONE',  ( 1.364683531249988535, 4.426041667008082214, 0.7879004041258500513 ) ) ;
#35915 = CARTESIAN_POINT ( 'NONE',  ( 1.311062339077714078, -1.627386490012251663, 1.267307609633941956 ) ) ;
#35916 = CARTESIAN_POINT ( 'NONE',  ( 6.642605195691581699, 9.837124264027149678, 1.199719254218462483 ) ) ;
#35917 = CARTESIAN_POINT ( 'NONE',  ( -9.073431116043565225, 11.60875560684942265, -1.599625672291263179 ) ) ;
#35918 = CARTESIAN_POINT ( 'NONE',  ( -8.955454528939414516, 3.019799309333212722, -8.063527476382400749 ) ) ;
#35919 = CARTESIAN_POINT ( 'NONE',  ( -3.422770014095240398, -0.02179599533581897189, -0.4183011094369343819 ) ) ;
#35920 = CARTESIAN_POINT ( 'NONE',  ( -1.499999999999960476, 7.128742170989517568, 10.89107411574800111 ) ) ;
#35921 = ORIENTED_EDGE ( 'NONE', *, *, #28829, .F. ) ;
#35922 = CARTESIAN_POINT ( 'NONE',  ( 3.068866956829822801, 1.501395149897828851, -1.425812640530661479 ) ) ;
#35923 = CARTESIAN_POINT ( 'NONE',  ( 0.7499999999999920064, 4.233333333333352932, 1.299038105676669330 ) ) ;
#35924 = CARTESIAN_POINT ( 'NONE',  ( 1.300320450452172594, -2.161773191439372965, -0.001381507821696103871 ) ) ;
#35925 = CARTESIAN_POINT ( 'NONE',  ( -6.239605170154193026, 7.010755437975583426, 1.009914170685573875 ) ) ;
#35926 = CARTESIAN_POINT ( 'NONE',  ( 1.436200859769844129, -1.123848162932556072, -1.677891559433869473 ) ) ;
#35927 = CARTESIAN_POINT ( 'NONE',  ( 1.441115678601017747, 8.287243072884294293, 3.161846531485674738 ) ) ;
#35929 = CARTESIAN_POINT ( 'NONE',  ( 8.920901888112002354, 9.510066412326583674, 0.7216878364870438212 ) ) ;
#35928 = CARTESIAN_POINT ( 'NONE',  ( 0.1749903794560592751, 2.884130749173496877, -2.444045186936738112 ) ) ;
#35930 = CARTESIAN_POINT ( 'NONE',  ( 1.968007779264384194, -0.3930682408332056843, 0.6607764497958503735 ) ) ;
#35931 = CARTESIAN_POINT ( 'NONE',  ( 6.104688764726555306, 1.790162971792093272, 0.6826718079199489697 ) ) ;
#35932 = CARTESIAN_POINT ( 'NONE',  ( 6.639320575229294086, 2.948176855103799454, 2.655556053213734558 ) ) ;
#35933 = CARTESIAN_POINT ( 'NONE',  ( 3.931328349035985603, -1.512150646884598215, -1.586510368271301541 ) ) ;
#35934 = CARTESIAN_POINT ( 'NONE',  ( 0.7499999999999885647, 3.097916667349487341, -1.299038105676658228 ) ) ;
#35935 = CARTESIAN_POINT ( 'NONE',  ( 2.988426722125224533, -1.135634098421594240, 1.538566774472991394 ) ) ;
#35936 = CARTESIAN_POINT ( 'NONE',  ( -3.893162665418476109, 7.693773542963529444, 1.040834085586084257E-14 ) ) ;
#35937 = CARTESIAN_POINT ( 'NONE',  ( 2.697709378994964879, 6.091152008895348580, 0.7216878364870338292 ) ) ;
#35939 = CARTESIAN_POINT ( 'NONE',  ( 0.9664229901367871189, -1.967894173845800898, -0.4390061282484733485 ) ) ;
#35938 = CARTESIAN_POINT ( 'NONE',  ( -9.368320956918621434, 11.95279375453699622, 1.443375672974076540 ) ) ;
#35941 = CIRCLE ( 'NONE', #42934, 6.959052028703005099 ) ;
#35940 = CARTESIAN_POINT ( 'NONE',  ( -1.364683531250014514, 10.65104166700806942, -0.7879004041258335089 ) ) ;
#35943 = CARTESIAN_POINT ( 'NONE',  ( -3.793249116773374396, 7.647484079536056356, 0.7998128361456352531 ) ) ;
#35942 = CARTESIAN_POINT ( 'NONE',  ( 0.7852321044731135347, 2.018311417075705272, -1.086964541883679303 ) ) ;
#35945 = EDGE_LOOP ( 'NONE', ( #44368, #22160, #30144, #10362 ) ) ;
#35944 = CARTESIAN_POINT ( 'NONE',  ( 4.576996085227628797, -0.001753933126501586170, -1.724958192235986232 ) ) ;
#35946 = CARTESIAN_POINT ( 'NONE',  ( -0.1405533004718494683, 4.096626656942652822, -2.275097870671268563 ) ) ;
#35947 = CARTESIAN_POINT ( 'NONE',  ( 7.969495366734495434, 8.192166104145387706, 1.040834085586084257E-14 ) ) ;
#35948 = CARTESIAN_POINT ( 'NONE',  ( 2.984766373302843778, 6.633977868828633717, -0.7998128361456291469 ) ) ;
#35949 = CARTESIAN_POINT ( 'NONE',  ( -11.33772463945036968, 12.69999999999999929, -3.600000000000000977 ) ) ;
#35950 = CARTESIAN_POINT ( 'NONE',  ( 1.047228354049560828, 1.731870006261830630, -0.9216698261682305660 ) ) ;
#35951 = DIRECTION ( 'NONE',  ( 0.4999999999999999445, 0.000000000000000000, -0.8660254037844387076 ) ) ;
#35952 = CARTESIAN_POINT ( 'NONE',  ( 4.059776932288224671, 6.823824623389866950, 1.199719254218462483 ) ) ;
#35953 = CARTESIAN_POINT ( 'NONE',  ( 0.07536363704233049743, 2.002983476668462881, -2.558365315478607904 ) ) ;
#35954 = ORIENTED_EDGE ( 'NONE', *, *, #41280, .T. ) ;
#35956 =( BOUNDED_CURVE ( )  B_SPLINE_CURVE ( 3, ( #10881, #161436, #42364, #43425 ),
 .UNSPECIFIED., .F., .T. ) 
 B_SPLINE_CURVE_WITH_KNOTS ( ( 4, 4 ),
 ( 1.430804639040424098, 1.438015327900962204 ),
 .UNSPECIFIED. ) 
 CURVE ( )  GEOMETRIC_REPRESENTATION_ITEM ( )  RATIONAL_B_SPLINE_CURVE ( ( 1.000000000000000000, 0.9999956671685397147, 0.9999956671685397147, 1.000000000000000000 ) ) 
 REPRESENTATION_ITEM ( '' )  );
#35955 = CARTESIAN_POINT ( 'NONE',  ( 0.3739936534635743270, -2.030981289472892026, 0.4004457479018645460 ) ) ;
#35957 = ORIENTED_EDGE ( 'NONE', *, *, #29125, .F. ) ;
#35958 = CARTESIAN_POINT ( 'NONE',  ( 3.879414023784663712, 0.2179053609261162039, -1.798230022952992613 ) ) ;
#35959 = ORIENTED_EDGE ( 'NONE', *, *, #79134, .T. ) ;
#35960 = CARTESIAN_POINT ( 'NONE',  ( 6.204791576909545192, 7.267953590263130259, -1.199719254218452047 ) ) ;
#35961 = CARTESIAN_POINT ( 'NONE',  ( 4.000000000000012434, 6.499999999999999112, -1.214306433183764966E-14 ) ) ;
#35962 = CARTESIAN_POINT ( 'NONE',  ( 5.426340414154960712, -0.8198882401838718526, -1.615393417293700784 ) ) ;
#35963 = CARTESIAN_POINT ( 'NONE',  ( 6.834718834620487016, 7.146462526578263308, 0.000000000000000000 ) ) ;
#35964 = DIRECTION ( 'NONE',  ( -0.000000000000000000, -1.000000000000000000, -0.000000000000000000 ) ) ;
#35965 = CARTESIAN_POINT ( 'NONE',  ( 5.737025562671778545, 6.072208551910874164, -0.6475843906825241580 ) ) ;
#35967 = CARTESIAN_POINT ( 'NONE',  ( 8.543609354905870035, 13.11929468069890525, 0.7998128361456462443 ) ) ;
#35966 = CARTESIAN_POINT ( 'NONE',  ( 6.742638014206057129, -1.825417518414352180, -0.3614582840437295941 ) ) ;
#35968 = CARTESIAN_POINT ( 'NONE',  ( 4.341351955572036125, 0.4158663518127497793, -1.869753321735210916 ) ) ;
#35969 = CARTESIAN_POINT ( 'NONE',  ( 1.500000000000039524, 7.378742179571327497, 10.87908636427990494 ) ) ;
#35970 = CARTESIAN_POINT ( 'NONE',  ( -11.34342368903357290, 5.311043228906556557, 5.661199053045820051 ) ) ;
#35971 = CARTESIAN_POINT ( 'NONE',  ( 1.284279953904121641, 3.253360285806104812, 0.7750000000000135669 ) ) ;
#35972 = DIRECTION ( 'NONE',  ( 1.000000000000000000, -0.000000000000000000, -0.000000000000000000 ) ) ;
#35973 = CARTESIAN_POINT ( 'NONE',  ( 6.073689629242148058, 8.109057205581079231, -1.443375672974057666 ) ) ;
#35974 = CARTESIAN_POINT ( 'NONE',  ( -4.437596350374534815, 4.071617251725375475, -0.7998128361456221525 ) ) ;
#35975 = CARTESIAN_POINT ( 'NONE',  ( 1.059701713109785670, 0.4209238396889225520, -2.120155868012041811 ) ) ;
#35976 = CARTESIAN_POINT ( 'NONE',  ( -6.934069218746458318, 7.054445274817795486, -0.7998128361456362523 ) ) ;
#35977 = CARTESIAN_POINT ( 'NONE',  ( 6.378184920586140727, 6.405913593630768510, 0.000000000000000000 ) ) ;
#35978 = CARTESIAN_POINT ( 'NONE',  ( 0.9733497034139363402, 1.760643049788807257, -0.4823509818385819936 ) ) ;
#35979 = CARTESIAN_POINT ( 'NONE',  ( -4.218558352146454915, 8.073401844146177453, 1.040834085586084257E-14 ) ) ;
#35980 = CARTESIAN_POINT ( 'NONE',  ( 3.170728842436408179, -1.686227525993441834, -0.7000332573987508855 ) ) ;
#35981 = CARTESIAN_POINT ( 'NONE',  ( 10.23394195678221763, -9.091017468561378934, -0.1786341213271995521 ) ) ;
#35982 = CARTESIAN_POINT ( 'NONE',  ( 1.564566645345835116, 0.6029492335615972420, 1.814891859350221459 ) ) ;
#35983 = CARTESIAN_POINT ( 'NONE',  ( 2.471101528187972463, 1.758070753236480988, 0.8880565435460830992 ) ) ;
#35984 = CARTESIAN_POINT ( 'NONE',  ( 3.702622889756892022, 1.667158369460784106, 0.9958445826224509023 ) ) ;
#35985 = CARTESIAN_POINT ( 'NONE',  ( -4.462568837553487100, 5.235360394347691404, -1.199719254218453823 ) ) ;
#35987 = CARTESIAN_POINT ( 'NONE',  ( 4.113620189327307664, 1.705085180707970771, 1.260635662952174663 ) ) ;
#35986 = CARTESIAN_POINT ( 'NONE',  ( 5.820193082016415609, 10.01225203898631655, 0.000000000000000000 ) ) ;
#35989 = ADVANCED_FACE ( 'NONE', ( #167831 ), #17289, .F. ) ;
#35988 = DIRECTION ( 'NONE',  ( 0.000000000000000000, -1.000000000000000000, 0.000000000000000000 ) ) ;
#35990 = CARTESIAN_POINT ( 'NONE',  ( 7.801827329660018684, 11.18955008699033726, 1.199719254218460707 ) ) ;
#35991 = CARTESIAN_POINT ( 'NONE',  ( 6.080382892099663650, 6.037283676876850969, 0.3399492115118609714 ) ) ;
#35992 = CARTESIAN_POINT ( 'NONE',  ( 5.794130544993763898, 7.853181283949808744, 1.599625672291269396 ) ) ;
#35993 = DIRECTION ( 'NONE',  ( 0.000000000000000000, 8.546850786086437571E-32, 1.000000000000000000 ) ) ;
#35994 = CARTESIAN_POINT ( 'NONE',  ( 3.791466046568803705, 1.323482414808102137, 1.257835202898072380 ) ) ;
#35995 = CARTESIAN_POINT ( 'NONE',  ( -8.673617379884035472E-15, 3.507114751586604129, -11.99288524841337455 ) ) ;
#35996 = CARTESIAN_POINT ( 'NONE',  ( -9.842856333841300653, 10.58567993234409421, 0.7216878364870438212 ) ) ;
#35997 = CARTESIAN_POINT ( 'NONE',  ( -5.519007765018521638, 7.558588572879005874, 1.349693927849420438 ) ) ;
#35998 = CARTESIAN_POINT ( 'NONE',  ( -15.75000000000000000, 13.40000000000000036, -3.600000000000002309 ) ) ;
#35999 = CARTESIAN_POINT ( 'NONE',  ( 4.996879044411707937, 1.554903924810165705, -1.039696167511289238 ) ) ;
#36000 = CARTESIAN_POINT ( 'NONE',  ( 7.263417608619159083, 9.497073181520933716, -1.599625672291262513 ) ) ;
#36001 = CARTESIAN_POINT ( 'NONE',  ( 3.299358975845566810, 1.519210379524044585, 1.184558777233129412 ) ) ;
#36002 = CARTESIAN_POINT ( 'NONE',  ( 6.192239757033616065, 0.9699301198475211994, -1.705161095427814466 ) ) ;
#36003 = CARTESIAN_POINT ( 'NONE',  ( 4.216749469050096621, 4.878294787768598262, -1.199719254218452047 ) ) ;
#36004 = CARTESIAN_POINT ( 'NONE',  ( 1.364683531249997417, 9.546875000341396245, 2.602085213965210642E-15 ) ) ;
#36005 = CARTESIAN_POINT ( 'NONE',  ( -5.052384799386910430, 9.046199365926717917, 1.214306433183764966E-14 ) ) ;
#36006 = CARTESIAN_POINT ( 'NONE',  ( 2.496672843210871129, 6.064535417054653266, -0.7998128361456291469 ) ) ;
#36007 = CARTESIAN_POINT ( 'NONE',  ( -3.160459205317013076, 6.701303149596211206, -0.7216878364870458196 ) ) ;
#36008 = EDGE_CURVE ( 'NONE', #159583, #138893, #54087, .T. ) ;
#36009 = CARTESIAN_POINT ( 'NONE',  ( 1.177538910780148385, 1.606043500598727247, 1.379722209976147251 ) ) ;
#36010 = AXIS2_PLACEMENT_3D ( 'NONE', #110279, #210892, #176288 ) ;
#36011 = CARTESIAN_POINT ( 'NONE',  ( 8.041957671200231417, 12.53403438304231976, 1.040834085586084257E-14 ) ) ;
#36012 = CARTESIAN_POINT ( 'NONE',  ( 1.499999999999989120, 3.525000000000021227, 1.214306433183764966E-14 ) ) ;
#36013 = CARTESIAN_POINT ( 'NONE',  ( 6.403194803628889709, -1.752124481401344358, 1.102429006916323395 ) ) ;
#36015 = CARTESIAN_POINT ( 'NONE',  ( 4.016789712308713511, 7.804715019974644008, -0.2988979438510626085 ) ) ;
#36014 = CARTESIAN_POINT ( 'NONE',  ( 0.8723036553972834950, -0.04505207493780280514, -1.840872848514919502 ) ) ;
#36016 = CARTESIAN_POINT ( 'NONE',  ( 6.451773728000877561, -2.099535003536470157, -0.9362560538537908483 ) ) ;
#36017 = CARTESIAN_POINT ( 'NONE',  ( 6.656690234629796699, 6.868486149930637552, 1.040834085586084257E-14 ) ) ;
#36019 = FACE_OUTER_BOUND ( 'NONE', #172557, .T. ) ;
#36018 = CARTESIAN_POINT ( 'NONE',  ( 5.248414862265931902, 5.295774558831261913, 0.000000000000000000 ) ) ;
#36020 = CARTESIAN_POINT ( 'NONE',  ( 1.025772235718758196, -1.457823864038493733, -1.768965695191491827 ) ) ;
#36021 = CARTESIAN_POINT ( 'NONE',  ( -3.188928480291558287, 8.980740528189064875, 2.451733079074509547 ) ) ;
#36022 = CARTESIAN_POINT ( 'NONE',  ( -4.437261413422502798, 8.398831758960053406, 0.000000000000000000 ) ) ;
#36023 = CARTESIAN_POINT ( 'NONE',  ( 5.753840666697315420, 0.7890659797671593090, 1.774590222461839506 ) ) ;
#36024 = EDGE_LOOP ( 'NONE', ( #45358, #201417, #178768, #75697 ) ) ;
#36025 = CARTESIAN_POINT ( 'NONE',  ( 8.392133896734662812, 10.81390885098904420, 1.443375672974076540 ) ) ;
#36026 = CARTESIAN_POINT ( 'NONE',  ( 0.4572897223803442102, -1.724499148370229218, 1.038616540587710357 ) ) ;
#36027 = CARTESIAN_POINT ( 'NONE',  ( 6.438686429976131720, -1.555646628146038157, 1.282773817382940162 ) ) ;
#36029 = CARTESIAN_POINT ( 'NONE',  ( 11.04536101718726293, 12.59537905954598358, 1.099999999999999201 ) ) ;
#36028 = CARTESIAN_POINT ( 'NONE',  ( -6.503107236049161521, 10.73870887536603291, 0.7998128361456481317 ) ) ;
#36030 = CARTESIAN_POINT ( 'NONE',  ( 1.642778471875000035, -0.3135416661887088785, -2.845375778867859751 ) ) ;
#36032 = CARTESIAN_POINT ( 'NONE',  ( 2.799370285489965138, -0.5572909556486020932, 1.679871745949900408 ) ) ;
#36031 = CARTESIAN_POINT ( 'NONE',  ( 2.888710413438722924, 1.792813287458893790, -1.075199139784080771 ) ) ;
#36033 = CARTESIAN_POINT ( 'NONE',  ( -11.18654035131441127, 1.000000000000000888, 4.041720556560751021 ) ) ;
#36035 = CARTESIAN_POINT ( 'NONE',  ( 5.033284615878021562, -1.618354306187347769, -1.623638663579999752 ) ) ;
#36034 = DIRECTION ( 'NONE',  ( 0.000000000000000000, 0.000000000000000000, 1.000000000000000000 ) ) ;
#36036 = CARTESIAN_POINT ( 'NONE',  ( 3.573892692743201760, -1.677664982382242931, -0.4625120326062928111 ) ) ;
#36037 = CARTESIAN_POINT ( 'NONE',  ( 8.516493047678546091, 13.08765898893368629, -0.7998128361456352531 ) ) ;
#36038 = DIRECTION ( 'NONE',  ( 0.8003905289055504024, -4.396526966619893387E-05, 0.5994789398347104559 ) ) ;
#36039 = CARTESIAN_POINT ( 'NONE',  ( 3.813592814792550190, -1.418126570600848124, 0.9972168832048341480 ) ) ;
#36040 = CARTESIAN_POINT ( 'NONE',  ( 3.561125603554469610, 1.713606050895712718, -1.333181090037469652 ) ) ;
#36041 = CARTESIAN_POINT ( 'NONE',  ( 5.996784015946103885, 5.890669528225568996, 1.040834085586084257E-14 ) ) ;
#36042 = CARTESIAN_POINT ( 'NONE',  ( 4.452361426671761713, -1.313546101436880109, 1.530156479064001207 ) ) ;
#36043 = CARTESIAN_POINT ( 'NONE',  ( 1.375000000000000888, 2.052068128417951609, -7.865587939079325464E-14 ) ) ;
#36044 = CARTESIAN_POINT ( 'NONE',  ( 1.499999999999989120, 4.327083334016148086, -0.8660254037844323793 ) ) ;
#36045 = CARTESIAN_POINT ( 'NONE',  ( 2.045805558669851365, 0.7393754583576680472, -1.779040955004469904 ) ) ;
#36046 = CARTESIAN_POINT ( 'NONE',  ( 1.364683531250000303, 15.00520833367472839, -0.7879004041258355073 ) ) ;
#36047 = CARTESIAN_POINT ( 'NONE',  ( 5.379204547434111028, -2.008251482569714419, -0.9497353344293004707 ) ) ;
#36048 = ORIENTED_EDGE ( 'NONE', *, *, #194299, .T. ) ;
#36049 = CARTESIAN_POINT ( 'NONE',  ( -0.1108833634137010304, 6.948331553507800962, -2.491992042620773340 ) ) ;
#36050 = CARTESIAN_POINT ( 'NONE',  ( -1.500000000000013101, 1.879166666666692187, -0.8660254037844313801 ) ) ;
#36051 = CARTESIAN_POINT ( 'NONE',  ( 7.311924916471702396, 7.425000578838787391, -0.7998128361456281477 ) ) ;
#36052 = CARTESIAN_POINT ( 'NONE',  ( 3.172244755473273781, 6.644776614786712443, 0.000000000000000000 ) ) ;
#36053 = CARTESIAN_POINT ( 'NONE',  ( 3.285556943749998737, -2.355208332855375453, -1.896917185911906722 ) ) ;
#36054 = CARTESIAN_POINT ( 'NONE',  ( 0.1006276693296826175, -1.041319732255343355, 1.962097497535258084 ) ) ;
#36055 = CARTESIAN_POINT ( 'NONE',  ( 6.092239754786219486, 0.9682357284593717806, -1.706234036142616928 ) ) ;
#36056 = CARTESIAN_POINT ( 'NONE',  ( 7.619319141200057821, 10.87266085050000974, 1.082531754730557072 ) ) ;
#36057 = CARTESIAN_POINT ( 'NONE',  ( -0.3598541952674910727, 3.203739155314830445, 2.034949316489486737 ) ) ;
#36058 = CARTESIAN_POINT ( 'NONE',  ( 0.1753634416057497925, 0.0001173177735149660839, -2.144164757042037017 ) ) ;
#36059 = CLOSED_SHELL ( 'NONE', ( #159368, #23887, #44999, #191268, #113541, #202502, #41438, #160091 ) ) ;
#36060 = CARTESIAN_POINT ( 'NONE',  ( 4.529305835417093640, 7.441884687032027657, -1.199719254218450271 ) ) ;
#36061 = CARTESIAN_POINT ( 'NONE',  ( -4.990809943606281607, 6.915973915664348937, -1.443375672974066548 ) ) ;
#36062 = CARTESIAN_POINT ( 'NONE',  ( 4.492669715648281326, 2.022274968565600517, 0.4054665169595774721 ) ) ;
#36063 = CARTESIAN_POINT ( 'NONE',  ( -6.254388934605767503, 6.191208599995166040, 0.7998128361456341429 ) ) ;
#36064 = CARTESIAN_POINT ( 'NONE',  ( 1.499999999999990896, 4.056250000682819490, 1.214306433183764966E-14 ) ) ;
#36065 = CARTESIAN_POINT ( 'NONE',  ( 0.6823417656249917140, 5.155208333674749177, 1.181850606188765695 ) ) ;
#36066 = CARTESIAN_POINT ( 'NONE',  ( 5.659403934932580427, 0.3656299861228041181, -1.834283699791404043 ) ) ;
#36067 = CARTESIAN_POINT ( 'NONE',  ( 4.271880269886525916, 1.546599990029189575, -0.7845881139060503218 ) ) ;
#36068 = CARTESIAN_POINT ( 'NONE',  ( 3.192619200838729743, 1.373927285412982036, 1.068286041690246657 ) ) ;
#36069 = CARTESIAN_POINT ( 'NONE',  ( 9.124274191872634887, 11.66807252865000244, -1.443375672974058777 ) ) ;
#36070 = CARTESIAN_POINT ( 'NONE',  ( 2.367065275503206667, 0.1088462660112088087, -2.289894902259086429 ) ) ;
#36071 = CARTESIAN_POINT ( 'NONE',  ( -1.364683531250010295, 4.342708333674753618, 0.7879004041258379498 ) ) ;
#36072 = CARTESIAN_POINT ( 'NONE',  ( 5.689037021386003090, 1.583751769416761324, 1.365026519206056665 ) ) ;
#36073 = CARTESIAN_POINT ( 'NONE',  ( 0.04061758243546764735, -1.421021341975825969, -1.170429047309962112 ) ) ;
#36074 = CARTESIAN_POINT ( 'NONE',  ( 0.000000000000000000, 13.79999999999998295, 0.000000000000000000 ) ) ;
#36075 = CARTESIAN_POINT ( 'NONE',  ( 1.529922885524274134, -1.701946718671920600, 1.081067414773040802 ) ) ;
#36076 = CARTESIAN_POINT ( 'NONE',  ( 0.05887529153619439071, -1.959562692596405364, -0.9812908054248059564 ) ) ;
#36077 = CARTESIAN_POINT ( 'NONE',  ( 7.948861177221683505, 14.94981965669310853, -9.879624537148666619 ) ) ;
#36078 = CARTESIAN_POINT ( 'NONE',  ( -7.178152263431422320, 10.46192917639026554, 1.199719254218453823 ) ) ;
#36079 = CARTESIAN_POINT ( 'NONE',  ( 7.142447996300871793, 7.227277505306155092, 0.7998128361456341429 ) ) ;
#36080 = CARTESIAN_POINT ( 'NONE',  ( 2.561320117580662803, -1.761587792986643475, 1.180070990429403555 ) ) ;
#36081 = CARTESIAN_POINT ( 'NONE',  ( 1.364683531249988757, -0.1156249996585798079, 0.000000000000000000 ) ) ;
#36082 = CARTESIAN_POINT ( 'NONE',  ( 5.971303284387838417, 0.1295235881030691594, -1.821162830480331563 ) ) ;
#36083 = VERTEX_POINT ( 'NONE', #183006 ) ;
#36084 = CARTESIAN_POINT ( 'NONE',  ( -5.607179047703544583, 8.699403434699558346, 1.199719254218454489 ) ) ;
#36085 = CARTESIAN_POINT ( 'NONE',  ( 3.285556943750000070, -1.071874999522042016, 0.000000000000000000 ) ) ;
#36086 = CARTESIAN_POINT ( 'NONE',  ( -4.869349725602420520, 8.832658446511480577, 1.040834085586084257E-14 ) ) ;
#36087 = CARTESIAN_POINT ( 'NONE',  ( 2.267837486342203057, 0.5347344578308220742, -1.947668537691170876 ) ) ;
#36088 = CARTESIAN_POINT ( 'NONE',  ( 0.09494852110062798611, -0.4603312545960658864, -2.062269868324863253 ) ) ;
#36089 = CARTESIAN_POINT ( 'NONE',  ( 9.083072846151447166, 12.68433652289702884, 1.199719254218450271 ) ) ;
#36090 = CARTESIAN_POINT ( 'NONE',  ( 4.082723863713003887, 1.765846151219726101, 0.5873946967244033646 ) ) ;
#36091 = CARTESIAN_POINT ( 'NONE',  ( 9.378489572351044856, 11.96465713920816043, -1.599625672291262513 ) ) ;
#36092 = CARTESIAN_POINT ( 'NONE',  ( 11.92619525870751573, 13.52622296793681045, -1.328859154004804699 ) ) ;
#36093 = EDGE_LOOP ( 'NONE', ( #167937, #17062, #7606 ) ) ;
#36094 = CARTESIAN_POINT ( 'NONE',  ( -3.440018289565379028, 5.036440642624797626, 1.599625672291267398 ) ) ;
#36095 = CARTESIAN_POINT ( 'NONE',  ( -6.333630315878337136, 10.54098580183340772, 0.000000000000000000 ) ) ;
#36097 = CARTESIAN_POINT ( 'NONE',  ( -4.061425534073997312, 7.733864674645915649, 0.6335290845049870168 ) ) ;
#36096 = CARTESIAN_POINT ( 'NONE',  ( -5.966470118465691641, 9.118576350588734059, -1.199719254218452047 ) ) ;
#36098 = CARTESIAN_POINT ( 'NONE',  ( -1.364683531250000748, -1.240624999658580752, 0.000000000000000000 ) ) ;
#36099 = CARTESIAN_POINT ( 'NONE',  ( 1.528208422804043121, 1.709223377337875549, -0.2899604983128030722 ) ) ;
#36100 = CARTESIAN_POINT ( 'NONE',  ( 1.288542162703592231, 1.315766340102142662, 1.139191825253932366 ) ) ;
#36102 = CARTESIAN_POINT ( 'NONE',  ( 7.782016984564049444, 11.06247500109133064, 1.082531754730557072 ) ) ;
#36101 = CARTESIAN_POINT ( 'NONE',  ( 5.127664261384059508, -2.192653808335935928, 0.7197182627937804833 ) ) ;
#36103 = CARTESIAN_POINT ( 'NONE',  ( 4.848976215542928792, 5.686169002002086970, 1.199719254218452047 ) ) ;
#36104 = CARTESIAN_POINT ( 'NONE',  ( 1.458354148090333258, 0.8324554894755629153, 1.885337613027091352 ) ) ;
#36105 = CARTESIAN_POINT ( 'NONE',  ( 7.156006149914539982, 7.243095351188763686, 1.040834085586084257E-14 ) ) ;
#36106 = EDGE_CURVE ( 'NONE', #123196, #181120, #157024, .T. ) ;
#36107 = CARTESIAN_POINT ( 'NONE',  ( 6.784486029815019137, -2.232095771774603055, 0.5478248251382932255 ) ) ;
#36108 = CARTESIAN_POINT ( 'NONE',  ( -6.042630808230841359E-15, -1.662500000000000533, 3.474999999999999645 ) ) ;
#36110 = CIRCLE ( 'NONE', #202136, 1.857347330825974252 ) ;
#36109 = CARTESIAN_POINT ( 'NONE',  ( -3.949167883330528372, 7.829389307186077396, 1.214306433183764966E-14 ) ) ;
#36111 = CARTESIAN_POINT ( 'NONE',  ( 0.4617158845385913590, 1.950347379310466422, -0.2869839225536646166 ) ) ;
#36112 = MECHANICAL_DESIGN_GEOMETRIC_PRESENTATION_REPRESENTATION (  '', ( #198748 ), #105424 ) ;
#36114 = CARTESIAN_POINT ( 'NONE',  ( -5.750066545971566079, 8.762142499391876171, 1.082531754730550855 ) ) ;
#36113 = CARTESIAN_POINT ( 'NONE',  ( 4.007995338699682719, -0.7271224857151190601, 1.768968726348684406 ) ) ;
#36115 = CARTESIAN_POINT ( 'NONE',  ( 6.006501602161061548, -0.7906231143557163055, -2.060575041408031272 ) ) ;
#36116 = CARTESIAN_POINT ( 'NONE',  ( -1.225000000000030065, 1.541666667349459230, -0.7072540797573018123 ) ) ;
#36117 = CARTESIAN_POINT ( 'NONE',  ( -6.983858524370814003, 9.241197259889665006, 1.443375672974064550 ) ) ;
#36118 = CARTESIAN_POINT ( 'NONE',  ( 5.248414861821569133, 6.256143772614186638, -1.082531754730548412 ) ) ;
#36119 = CARTESIAN_POINT ( 'NONE',  ( -3.296040741453672318, 6.859481608422314025, 0.7216878364870338292 ) ) ;
#36120 = CARTESIAN_POINT ( 'NONE',  ( -0.07552420640595960966, -0.8660980012666683603, -1.823048286210580793 ) ) ;
#36121 = EDGE_LOOP ( 'NONE', ( #144154, #198195, #38278, #71698 ) ) ;
#36122 = CARTESIAN_POINT ( 'NONE',  ( 3.259088711995949517, -1.748676463734340603, 1.505793948229345869 ) ) ;
#36123 = CARTESIAN_POINT ( 'NONE',  ( 4.721123852359588646, -1.751549048416237486, -0.8839179009662299080 ) ) ;
#36124 = CARTESIAN_POINT ( 'NONE',  ( 0.3913574919355842785, -1.795980968407092426, 0.7896611536716554580 ) ) ;
#36125 = CARTESIAN_POINT ( 'NONE',  ( 6.392587740394330531, -6.532648833121157850, 6.999862025036990509 ) ) ;
#36126 = ORIENTED_EDGE ( 'NONE', *, *, #153215, .T. ) ;
#36127 = CARTESIAN_POINT ( 'NONE',  ( 0.3041147963815365451, -1.138459102943665036, -1.785081232699109233 ) ) ;
#36128 =( BOUNDED_CURVE ( )  B_SPLINE_CURVE ( 2, ( #65244, #96739, #131395 ),
 .UNSPECIFIED., .F., .T. ) 
 B_SPLINE_CURVE_WITH_KNOTS ( ( 3, 3 ),
 ( 0.2458097188974980585, 0.2499999999999997502 ),
 .UNSPECIFIED. ) 
 CURVE ( )  GEOMETRIC_REPRESENTATION_ITEM ( )  RATIONAL_B_SPLINE_CURVE ( ( 0.9330148535346174388, 0.9326330537515126196, 0.9999999999999960032 ) ) 
 REPRESENTATION_ITEM ( '' )  );
#36129 = CARTESIAN_POINT ( 'NONE',  ( -7.914208982075130905, 10.25632978388623684, -1.599625672291263179 ) ) ;
#36131 = CYLINDRICAL_SURFACE ( 'NONE', #75128, 1.250000000000000000 ) ;
#36130 = CIRCLE ( 'NONE', #181464, 0.09999999999999982514 ) ;
#36132 = CARTESIAN_POINT ( 'NONE',  ( 3.450208493196211812, -0.8844140035146315082, 1.982955601465713258 ) ) ;
#36133 = CARTESIAN_POINT ( 'NONE',  ( 0.1277519899680359672, 2.521810436023053992, 1.998702265207899620 ) ) ;
#36134 = CARTESIAN_POINT ( 'NONE',  ( 0.6156802735862785259, 1.737094954450137285, 1.216079458918501333 ) ) ;
#36135 = CARTESIAN_POINT ( 'NONE',  ( -1.201851678989727383E-14, 1.243750000682821044, 1.732050807568877637 ) ) ;
#36136 = CARTESIAN_POINT ( 'NONE',  ( 8.218213668177886788, 12.73966637951625813, 0.7998128361456462443 ) ) ;
#36137 = CARTESIAN_POINT ( 'NONE',  ( 11.86145016429273014, 11.00587876334730453, -1.100000000000000089 ) ) ;
#36138 = CARTESIAN_POINT ( 'NONE',  ( 6.425920342564602983, 6.885296541689900351, -0.7293792964763821107 ) ) ;
#36139 = CARTESIAN_POINT ( 'NONE',  ( 2.020846523693183627, 1.921700534952670791, 0.7446803044362272361 ) ) ;
#36141 = DIRECTION ( 'NONE',  ( -1.000000000000000000, 7.109522442527899011E-16, 0.000000000000000000 ) ) ;
#36140 = CARTESIAN_POINT ( 'NONE',  ( -8.618179199781044630, 13.20629283305325963, 0.7998128361456341429 ) ) ;
#36142 = CARTESIAN_POINT ( 'NONE',  ( -1.364683531250000748, 2.009375000341421913, 1.214306433183764966E-14 ) ) ;
#36143 = CARTESIAN_POINT ( 'NONE',  ( 6.021701820789710169, 7.165471523702656498, -1.202873050745705275 ) ) ;
#36144 = DIRECTION ( 'NONE',  ( 0.1959619652057391359, -0.8823239151465414043, -0.4279058505713422278 ) ) ;
#36145 = ORIENTED_EDGE ( 'NONE', *, *, #14726, .F. ) ;
#36146 = CARTESIAN_POINT ( 'NONE',  ( 4.652931681422667332, 0.3304644650514582116, 1.883354098946861344 ) ) ;
#36147 = CARTESIAN_POINT ( 'NONE',  ( 11.91292854676703961, 12.48518470326975560, -1.446370920797349635 ) ) ;
#36149 =( GEOMETRIC_REPRESENTATION_CONTEXT ( 3 ) GLOBAL_UNCERTAINTY_ASSIGNED_CONTEXT ( ( #123539 ) ) GLOBAL_UNIT_ASSIGNED_CONTEXT ( ( #102807, #20466, #101735 ) ) REPRESENTATION_CONTEXT ( 'NONE', 'WORKASPACE' ) );
#36148 = CARTESIAN_POINT ( 'NONE',  ( 0.4216216942964992609, -0.1093418885590720091, 2.259903825829346680 ) ) ;
#36150 = CARTESIAN_POINT ( 'NONE',  ( -4.600294193738529103, 4.261431402316699035, -0.7998128361456221525 ) ) ;
#36152 = EDGE_CURVE ( 'NONE', #169714, #143658, #45780, .T. ) ;
#36151 = CARTESIAN_POINT ( 'NONE',  ( 1.458926887072587553, -1.529292093677349307, 0.9708203095366783053 ) ) ;
#36153 = CARTESIAN_POINT ( 'NONE',  ( 0.7607752342545861524, -0.05021853532924521607, -1.915246365852550037 ) ) ;
#36154 = CARTESIAN_POINT ( 'NONE',  ( 1.434126425884488354, 1.231690216755284562, 1.664001042209894088 ) ) ;
#36155 = CARTESIAN_POINT ( 'NONE',  ( 1.364683531249986537, 0.7177083336747527298, -0.7879004041258239610 ) ) ;
#36156 = CARTESIAN_POINT ( 'NONE',  ( 6.754772315933175619, -1.444328698515121800, 1.188528157999017454 ) ) ;
#36157 = CARTESIAN_POINT ( 'NONE',  ( 5.496683133134654398, -0.4700625557551000866, -1.868158488084943780 ) ) ;
#36159 = CARTESIAN_POINT ( 'NONE',  ( 6.483128551184942800, 6.753495492978965231, -0.1682882784904728146 ) ) ;
#36158 = CARTESIAN_POINT ( 'NONE',  ( 0.03047818801908425135, -1.425887938121385590, -1.815451699675968644 ) ) ;
#36160 = CARTESIAN_POINT ( 'NONE',  ( -0.6823417656250003738, 1.967708333674753174, -1.181850606188749264 ) ) ;
#36161 = CARTESIAN_POINT ( 'NONE',  ( 3.807127647779250168, -1.688003362470591684, 1.185206751978077788 ) ) ;
#36162 = CARTESIAN_POINT ( 'NONE',  ( -5.982172092127739482, 8.002286745614243912, -1.599625672291263179 ) ) ;
#36163 = CARTESIAN_POINT ( 'NONE',  ( 6.968000882419564945, 10.21675256520979858, 1.199719254218460707 ) ) ;
#36164 = CARTESIAN_POINT ( 'NONE',  ( 4.273844736805817668, 6.009238164405336313, 1.599625672291267175 ) ) ;
#36165 = CARTESIAN_POINT ( 'NONE',  ( 5.789495288235341874, 6.713164910151406595, 1.199719254218462483 ) ) ;
#36168 = CARTESIAN_POINT ( 'NONE',  ( -0.7500000000000215383, 3.941666666666690411, 1.299038105676671107 ) ) ;
#36167 = MECHANICAL_DESIGN_GEOMETRIC_PRESENTATION_REPRESENTATION (  '', ( #91564 ), #67377 ) ;
#36166 = CARTESIAN_POINT ( 'NONE',  ( 5.034254431704021648, 1.084988065057530982, -1.804815602348212256 ) ) ;
#36169 = ADVANCED_FACE ( 'NONE', ( #132175 ), #165766, .F. ) ;
#36170 = CARTESIAN_POINT ( 'NONE',  ( 6.021949436824264978, 2.040384406434097464, -0.3501103912618847014 ) ) ;
#36171 = CARTESIAN_POINT ( 'NONE',  ( 0.6823417656249882723, 0.7385416670080829915, -1.181850606188749264 ) ) ;
#36172 = CARTESIAN_POINT ( 'NONE',  ( 4.727887898869392203, -1.325758432718616042, -1.707240035374466114 ) ) ;
#36173 = CARTESIAN_POINT ( 'NONE',  ( 4.688151973431080144, 1.164670015804763370, 1.649827500200540253 ) ) ;
#36174 = CARTESIAN_POINT ( 'NONE',  ( -1.123270288249902160, 2.800000000000024691, 0.7750000000000117906 ) ) ;
#36175 = VECTOR ( 'NONE', #149991, 1000.000000000000000 ) ;
#36178 = CARTESIAN_POINT ( 'NONE',  ( 5.666945020832177882, 6.674152614801420746, 1.082531754730558626 ) ) ;
#36177 = CARTESIAN_POINT ( 'NONE',  ( -3.285556943749998737, -2.530208332855374831, 1.896917185911908499 ) ) ;
#36176 = CARTESIAN_POINT ( 'NONE',  ( -0.4355862708379995563, -6.583980363595115293, -9.606148981167580203 ) ) ;
#36179 = CARTESIAN_POINT ( 'NONE',  ( -4.796552484184649856, 8.818004674849227342, -0.7998128361456362523 ) ) ;
#36180 = CARTESIAN_POINT ( 'NONE',  ( 3.415250174187448362, -1.861344788686780438, 0.7762291900053899241 ) ) ;
#36181 = CARTESIAN_POINT ( 'NONE',  ( -8.829384350997580455, 11.32403438096243775, 1.599625672291269396 ) ) ;
#36183 = CARTESIAN_POINT ( 'NONE',  ( -10.96562622554683664, -5.341077028191769216, 0.1833053738655391618 ) ) ;
#36182 = CARTESIAN_POINT ( 'NONE',  ( -5.037017762676898158, 5.835274463666530131, -1.199719254218446718 ) ) ;
#36184 = CARTESIAN_POINT ( 'NONE',  ( 0.7500000000000006661, 12.66666666666666607, -1.299038105676657340 ) ) ;
#36185 = CARTESIAN_POINT ( 'NONE',  ( 6.720655732516647163, 2.019696082639847567, 2.477441386028636394 ) ) ;
#36187 = CARTESIAN_POINT ( 'NONE',  ( 4.763296089436113157, 1.880429982106451181, -0.7283946704290320540 ) ) ;
#36186 = CARTESIAN_POINT ( 'NONE',  ( -8.500599125644013654, 9.019713189447241319, 0.7216878364870438212 ) ) ;
#36188 = CARTESIAN_POINT ( 'NONE',  ( 1.499999999999989120, 5.295833333333356485, -0.8660254037844323793 ) ) ;
#36189 = CARTESIAN_POINT ( 'NONE',  ( 0.1699431646460221601, -1.131269863993559222, 1.302202208916112269 ) ) ;
#36190 = CARTESIAN_POINT ( 'NONE',  ( 4.227110032410640095, 8.153655147779589996, 0.7998128361456271485 ) ) ;
#36192 = CARTESIAN_POINT ( 'NONE',  ( 2.550000000000000266, 1.000000000000000888, -1.849324200890695824 ) ) ;
#36191 = CARTESIAN_POINT ( 'NONE',  ( 8.948018195339340508, 9.541702104091804415, -0.7216878364870197293 ) ) ;
#36193 = CARTESIAN_POINT ( 'NONE',  ( -10.64390791476601450, 5.929706677703244111, 5.549313566458391911 ) ) ;
#36194 = CARTESIAN_POINT ( 'NONE',  ( 5.993391575003322203, 1.416176893967495687, 1.222094818194748189 ) ) ;
#36195 = CARTESIAN_POINT ( 'NONE',  ( 6.416276891523604142, -2.012660772237227391, 0.05378525197091872656 ) ) ;
#36196 = DIRECTION ( 'NONE',  ( 0.000000000000000000, 0.000000000000000000, -1.000000000000000000 ) ) ;
#36197 = CARTESIAN_POINT ( 'NONE',  ( -7.390603132780803719, 7.794994207765291172, -0.7216878364870338292 ) ) ;
#36198 = EDGE_LOOP ( 'NONE', ( #49993, #170987, #190985, #200747 ) ) ;
#36199 = CARTESIAN_POINT ( 'NONE',  ( 10.50720586046655391, 11.36075438007358507, 0.7216878364870438212 ) ) ;
#36200 = CARTESIAN_POINT ( 'NONE',  ( 0.1402502066264778580, 0.7743353953559418690, 1.862009890338502505 ) ) ;
#36201 = CARTESIAN_POINT ( 'NONE',  ( 1.177659378823514791, 1.784474613499857032, -0.3112490768260189333 ) ) ;
#36202 = CARTESIAN_POINT ( 'NONE',  ( 3.051993976407674225, 6.574760382535328240, -0.7216878364870338292 ) ) ;
#36203 = CARTESIAN_POINT ( 'NONE',  ( 5.840740251263128791, 0.4172088472891195554, 2.120894824392767664 ) ) ;
#36204 = CARTESIAN_POINT ( 'NONE',  ( 5.615048174354031474, 9.702639970055050966, 0.7998128361456462443 ) ) ;
#36206 = CARTESIAN_POINT ( 'NONE',  ( 0.6201578395632812990, 1.887877179178775400, 0.3243255173654129297 ) ) ;
#36205 = CARTESIAN_POINT ( 'NONE',  ( -5.928993247877788697, 5.811580298812519807, 0.7998128361456341429 ) ) ;
#36207 = DIRECTION ( 'NONE',  ( 0.000000000000000000, 1.000000000000000000, 0.000000000000000000 ) ) ;
#36208 = DIRECTION ( 'NONE',  ( 1.014813233446432150E-15, 1.000000000000000000, -4.583713267641621330E-32 ) ) ;
#36209 = CARTESIAN_POINT ( 'NONE',  ( 5.124618875841165710, 8.922546421882614709, 1.040834085586084257E-14 ) ) ;
#36210 = CARTESIAN_POINT ( 'NONE',  ( -1.402160292154681736E-14, -0.8656249996585829720, 1.575800808251672791 ) ) ;
#36212 = ORIENTED_EDGE ( 'NONE', *, *, #191584, .F. ) ;
#36211 = CARTESIAN_POINT ( 'NONE',  ( 3.633221978782282147, 5.261844946711204507, -1.443375672974057666 ) ) ;
#36213 = CARTESIAN_POINT ( 'NONE',  ( -4.471491734408701291, 4.111161866431900513, 1.214306433183764966E-14 ) ) ;
#36214 = CARTESIAN_POINT ( 'NONE',  ( 3.678741886385179072, -2.082744454470350615, -0.5786317199799120292 ) ) ;
#36215 = CARTESIAN_POINT ( 'NONE',  ( -5.750066545971566079, 8.762142499391876171, 1.082531754730550855 ) ) ;
#36216 = CARTESIAN_POINT ( 'NONE',  ( 5.234856708652222856, 8.161064355852680308, 1.082531754730549078 ) ) ;
#36217 = CARTESIAN_POINT ( 'NONE',  ( 1.143014088299774578, 2.045220145331683614, 0.5602274146137007360 ) ) ;
#36218 = DIRECTION ( 'NONE',  ( 0.9988044021632737079, 8.339466111204228823E-16, -0.04888523518676889112 ) ) ;
#36219 = CARTESIAN_POINT ( 'NONE',  ( 2.266812238764161158, -1.800804572728794239, -0.8025143323158872022 ) ) ;
#36220 = CARTESIAN_POINT ( 'NONE',  ( 4.271672842113056312, 0.4137096367802223784, -1.866957553337177611 ) ) ;
#36221 = ORIENTED_EDGE ( 'NONE', *, *, #12435, .F. ) ;
#36222 = DIRECTION ( 'NONE',  ( 0.000000000000000000, -1.000000000000000000, 0.000000000000000000 ) ) ;
#36223 = CARTESIAN_POINT ( 'NONE',  ( 6.197704753879455630, -1.425424270160932094, -1.359389694413483562 ) ) ;
#36224 = CARTESIAN_POINT ( 'NONE',  ( 0.9197484630441244979, 1.157134895311136669, -1.559417598425276719 ) ) ;
#36225 = VERTEX_POINT ( 'NONE', #102836 ) ;
#36226 = CARTESIAN_POINT ( 'NONE',  ( -3.772911886352873445, 7.623757310712140800, 0.7998128361456352531 ) ) ;
#36227 = CARTESIAN_POINT ( 'NONE',  ( -5.334207092333882017, 5.187939460669764635, 0.7998128361456281477 ) ) ;
#36230 = ADVANCED_FACE ( 'NONE', ( #152645 ), #124604, .T. ) ;
#36229 = CARTESIAN_POINT ( 'NONE',  ( 6.387299765369506055, 7.584842826753462219, -1.082531754730548412 ) ) ;
#36228 = CARTESIAN_POINT ( 'NONE',  ( 7.467843683028853263, 7.606905806488803101, 0.7998128361456341429 ) ) ;
#36232 = ORIENTED_EDGE ( 'NONE', *, *, #55163, .T. ) ;
#36231 = CARTESIAN_POINT ( 'NONE',  ( 4.899028947338643469, -0.2378672112019977747, -1.897373119303269018 ) ) ;
#36233 = CARTESIAN_POINT ( 'NONE',  ( 3.334799921508072806, 2.153101868192684343, 0.4835390122766567433 ) ) ;
#36234 = CARTESIAN_POINT ( 'NONE',  ( 2.397764582540245382, 1.705505620506567510, 1.400368488499253994 ) ) ;
#36235 = CARTESIAN_POINT ( 'NONE',  ( 0.000000000000000000, 0.000000000000000000, 0.000000000000000000 ) ) ;
#36236 = CARTESIAN_POINT ( 'NONE',  ( 0.4164788467995067522, -0.6444665046171775824, -1.800526059235994403 ) ) ;
#36237 = CARTESIAN_POINT ( 'NONE',  ( -0.02319159430947542386, 5.725354828811364705, -2.405035539666657840 ) ) ;
#36238 = CARTESIAN_POINT ( 'NONE',  ( -0.02237740007485569671, 15.46059968838234866, 11.97522600859444353 ) ) ;
#36239 = CARTESIAN_POINT ( 'NONE',  ( -6.761775799040186996, -7.009934032700144257, -6.672971353127118199 ) ) ;
#36240 = CARTESIAN_POINT ( 'NONE',  ( 3.121598655985452275, 0.3063859900464052100, -2.047459029603612368 ) ) ;
#36241 = CARTESIAN_POINT ( 'NONE',  ( -5.949330478298285207, 5.835307067636438028, 0.7998128361456341429 ) ) ;
#36242 = CARTESIAN_POINT ( 'NONE',  ( -4.619186966818853435, 8.364647258818639131, 0.2498820228645174391 ) ) ;
#36244 = CARTESIAN_POINT ( 'NONE',  ( 0.7960496800812133511, -0.7770375076890515542, 2.017388685454111652 ) ) ;
#36243 = CARTESIAN_POINT ( 'NONE',  ( -3.602716132929368875, 5.226254793216122074, 1.599625672291267398 ) ) ;
#36245 = CARTESIAN_POINT ( 'NONE',  ( 2.859115728684503477, 0.3189004193784421015, -2.168101852914063876 ) ) ;
#36246 = CARTESIAN_POINT ( 'NONE',  ( 1.249999999999998890, 0.000000000000000000, -6.123233995736774664E-17 ) ) ;
#36247 = CARTESIAN_POINT ( 'NONE',  ( 0.3106162252735343854, -6.604184692106362498, 9.611175950047659455 ) ) ;
#36248 = CARTESIAN_POINT ( 'NONE',  ( 0.6823417656249934904, 12.75520833367473017, 1.181850606188764807 ) ) ;
#36249 = ADVANCED_FACE ( 'NONE', ( #139624, #169954 ), #87653, .T. ) ;
#36250 = CARTESIAN_POINT ( 'NONE',  ( -4.630991987519598396, 7.560518531151607213, 1.199719254218452935 ) ) ;
#36252 = CARTESIAN_POINT ( 'NONE',  ( 6.100242454504600786, -0.2022020391262440986, 1.722246827497366795 ) ) ;
#36251 = CIRCLE ( 'NONE', #18929, 0.5000000000000016653 ) ;
#36253 = CARTESIAN_POINT ( 'NONE',  ( -2.428882075142555497, 5.985446187641602300, 1.040834085586084257E-14 ) ) ;
#36254 = CARTESIAN_POINT ( 'NONE',  ( 3.678634981485491728, 1.317094234756083893, -1.597214816249421743 ) ) ;
#36255 = CARTESIAN_POINT ( 'NONE',  ( 4.236029508982094072, 2.116713919566749702, -0.05380437090627546853 ) ) ;
#36256 = AXIS2_PLACEMENT_3D ( 'NONE', #196111, #193959, #33591 ) ;
#36257 = CARTESIAN_POINT ( 'NONE',  ( 5.276094334012385367, 9.307193822989793475, 1.040834085586084257E-14 ) ) ;
#36258 = CARTESIAN_POINT ( 'NONE',  ( -1.364683531250012516, 4.738541667008091984, -0.7879004041258300672 ) ) ;
#36259 = CARTESIAN_POINT ( 'NONE',  ( 2.922656654487673311, -1.361644196593906342, 1.423118114318456584 ) ) ;
#36260 = B_SPLINE_CURVE_WITH_KNOTS ( 'NONE', 3,
 ( #25845, #9601, #188349, #6387, #39988, #156943, #190475, #106098, #172120, #63434 ),
 .UNSPECIFIED., .F., .F.,
 ( 4, 2, 2, 2, 4 ),
 ( 0.000000000000000000, 0.0003993275742951113514, 0.0007986551485902227028, 0.001197982722885334054, 0.001597310297180445406 ),
 .UNSPECIFIED. ) ;
#36261 = CARTESIAN_POINT ( 'NONE',  ( 0.9317291061951762376, -1.865162313430932750, 0.4216105838140621342 ) ) ;
#36262 = CARTESIAN_POINT ( 'NONE',  ( 4.804755513996577854, 1.992766236949112812, 1.132715491657744877 ) ) ;
#36263 = CARTESIAN_POINT ( 'NONE',  ( 2.719161800852238464, -0.1789327596440904167, 1.816892639718168168 ) ) ;
#36264 = EDGE_CURVE ( 'NONE', #11923, #121448, #160579, .T. ) ;
#36265 = CARTESIAN_POINT ( 'NONE',  ( 4.927462483923885195, 4.713404084191450849, -0.7998128361456481317 ) ) ;
#36266 = CARTESIAN_POINT ( 'NONE',  ( 4.148431815657221300, 7.783661518334664464, 1.040834085586084257E-14 ) ) ;
#36267 = CARTESIAN_POINT ( 'NONE',  ( -7.881367368245678406, 8.089350105908421185, 0.7998128361456602331 ) ) ;
#36268 = CARTESIAN_POINT ( 'NONE',  ( 4.500248159151196248, -0.9453760218497176959, 1.777399672076788617 ) ) ;
#36269 = AXIS2_PLACEMENT_3D ( 'NONE', #2485, #208170, #191914 ) ;
#36270 = CARTESIAN_POINT ( 'NONE',  ( 4.557442073745519018, 1.573120015848201492, 1.171846803954358363 ) ) ;
#36271 = CARTESIAN_POINT ( 'NONE',  ( -8.667740277838301921, 9.006785167099828016, -0.7998128361456291469 ) ) ;
#36272 = CARTESIAN_POINT ( 'NONE',  ( -5.436983294280064882, 6.301900917203534291, 1.199719254218450271 ) ) ;
#36273 = CARTESIAN_POINT ( 'NONE',  ( 0.1753634416057741896, 2.865130778691078905, -2.632309609290182095 ) ) ;
#36275 = CARTESIAN_POINT ( 'NONE',  ( 5.313276456144085280, -0.2569279779609782155, 1.750970204404985964 ) ) ;
#36274 = CARTESIAN_POINT ( 'NONE',  ( 0.09931936810910445279, -0.5537021472524807919, 2.016037456109684989 ) ) ;
#36276 = DIRECTION ( 'NONE',  ( 5.578564026256490882E-16, 1.000000000000000000, 9.066213480720158442E-32 ) ) ;
#36277 = CARTESIAN_POINT ( 'NONE',  ( 1.394752248596371702, 1.789971953256053627, -1.264032476404143512 ) ) ;
#36278 = CARTESIAN_POINT ( 'NONE',  ( 6.193256023596829252, -0.5794974496134881470, 1.641157367357688246 ) ) ;
#36279 = CARTESIAN_POINT ( 'NONE',  ( 6.154511665599609493, 9.267681812253174556, 1.199719254218462483 ) ) ;
#36280 = CARTESIAN_POINT ( 'NONE',  ( 0.1333692844072559558, 0.7140749627707367875, -2.136770008611441618 ) ) ;
#36281 = CARTESIAN_POINT ( 'NONE',  ( 0.8028309281867166414, 1.407482529003287075, 0.9968052580264019635 ) ) ;
#36282 = CARTESIAN_POINT ( 'NONE',  ( 0.1874131419884322858, 1.628132678060219884, 1.467219630700428157 ) ) ;
#36283 = CARTESIAN_POINT ( 'NONE',  ( 6.573613466494099278, 1.281508381366827765, -1.168108599551227478 ) ) ;
#36284 = CARTESIAN_POINT ( 'NONE',  ( 3.352369063006555905, 2.207063162671081713, 4.936380160885933677E-05 ) ) ;
#36285 = CARTESIAN_POINT ( 'NONE',  ( 6.509000000000012776, 0.004788705324892602276, 2.000274819378269342 ) ) ;
#36286 = CARTESIAN_POINT ( 'NONE',  ( 6.877413710614480813, -0.1567828624706164298, 2.136824976188213654 ) ) ;
#36287 = CYLINDRICAL_SURFACE ( 'NONE', #120755, 0.09999999999999990841 ) ;
#36288 = CARTESIAN_POINT ( 'NONE',  ( 0.7084050413898737020, 1.255986415914780885, -1.704487872487458144 ) ) ;
#36289 = VECTOR ( 'NONE', #203220, 1000.000000000000114 ) ;
#36290 = CARTESIAN_POINT ( 'NONE',  ( 1.872228381520318896, 3.299999999999997158, 0.3999999999999958589 ) ) ;
#36291 = CARTESIAN_POINT ( 'NONE',  ( 6.053727987682750999, 0.5585614288021992779, -1.843621721047507878 ) ) ;
#36292 = EDGE_CURVE ( 'NONE', #173148, #76194, #113896, .T. ) ;
#36293 = ORIENTED_EDGE ( 'NONE', *, *, #8528, .F. ) ;
#36295 = CARTESIAN_POINT ( 'NONE',  ( 1.364683531249986981, -1.053124999658580752, 0.000000000000000000 ) ) ;
#36294 = CARTESIAN_POINT ( 'NONE',  ( 1.628911237561550873, 0.2300632485819526785, 2.280818132175948421 ) ) ;
#36296 = CARTESIAN_POINT ( 'NONE',  ( 4.708759422647839976, 4.387974169377582001, -0.7998128361456211532 ) ) ;
#36297 = CARTESIAN_POINT ( 'NONE',  ( 6.518772930072240790, 6.499656594706071822, -0.7998128361456281477 ) ) ;
#36298 = CARTESIAN_POINT ( 'NONE',  ( 3.879691667246706110, 0.2712996660018602846, -2.204593333604548455 ) ) ;
#36299 = CARTESIAN_POINT ( 'NONE',  ( -8.202319746587722449, 8.671720580548228696, 1.040834085586084257E-14 ) ) ;
#36300 = DIRECTION ( 'NONE',  ( 0.000000000000000000, -1.000000000000000000, 0.000000000000000000 ) ) ;
#36301 = CARTESIAN_POINT ( 'NONE',  ( 4.365362273920230685, 8.036747052974847705, 0.7216878364870298324 ) ) ;
#36302 = CARTESIAN_POINT ( 'NONE',  ( -7.158341917891067219, 11.29522330427417565, 0.000000000000000000 ) ) ;
#36303 = CARTESIAN_POINT ( 'NONE',  ( 6.563555762791525972, 6.830105609444471426, -0.7216878364870458196 ) ) ;
#36304 = CARTESIAN_POINT ( 'NONE',  ( 1.688125190044654556, 1.678006053171029688, 1.117831401076685660 ) ) ;
#36306 = CARTESIAN_POINT ( 'NONE',  ( 1.077094301713815039, 1.904230998939509867, 0.7929820198450258095 ) ) ;
#36305 = CARTESIAN_POINT ( 'NONE',  ( 7.293396569147545527, 10.59638086639245280, 1.199719254218460707 ) ) ;
#36307 = CARTESIAN_POINT ( 'NONE',  ( 0.000000000000000000, 1.750000000000001554, 0.000000000000000000 ) ) ;
#36308 = CARTESIAN_POINT ( 'NONE',  ( 6.997416677984476863, 7.336276677169590421, 0.000000000000000000 ) ) ;
#36309 = SURFACE_SIDE_STYLE ('',( #70927 ) ) ;
#36310 = CARTESIAN_POINT ( 'NONE',  ( -0.6823417656250212460, 4.301041667008085767, 1.181850606188767472 ) ) ;
#36311 = CARTESIAN_POINT ( 'NONE',  ( 3.802820697025221630, 1.879323313303274734, 1.126966401794778250 ) ) ;
#36312 = CARTESIAN_POINT ( 'NONE',  ( 0.9146856577476671912, -1.281363086869342194, -1.556907195799726917 ) ) ;
#36313 = CARTESIAN_POINT ( 'NONE',  ( 0.6789530235665336422, 1.236279375446739603, 1.364625092910062953 ) ) ;
#36314 = CARTESIAN_POINT ( 'NONE',  ( 5.249693134425458041, 2.289860626911474739, -0.1101728261837572470 ) ) ;
#36315 = CARTESIAN_POINT ( 'NONE',  ( 3.468544592087896561, 0.04396668885017079864, -1.840778273432375212 ) ) ;
#36316 =( GEOMETRIC_REPRESENTATION_CONTEXT ( 3 ) GLOBAL_UNCERTAINTY_ASSIGNED_CONTEXT ( ( #55301 ) ) GLOBAL_UNIT_ASSIGNED_CONTEXT ( ( #165748, #63985, #17334 ) ) REPRESENTATION_CONTEXT ( 'NONE', 'WORKASPACE' ) );
#36317 = CARTESIAN_POINT ( 'NONE',  ( 7.560643217915098191, 11.97250085420964716, -0.7998128361456291469 ) ) ;
#36318 = CARTESIAN_POINT ( 'NONE',  ( 3.680510133705969800, -1.759192178946006990, -0.4875382671739314500 ) ) ;
#36319 = CARTESIAN_POINT ( 'NONE',  ( 5.115861365725078436, 0.1511377038382749338, 2.010826595755777824 ) ) ;
#36320 = CARTESIAN_POINT ( 'NONE',  ( -8.585337585951595685, 11.03931315507545108, -1.599625672291263179 ) ) ;
#36322 = CARTESIAN_POINT ( 'NONE',  ( -6.526270840131767059, 8.707344961610770540, -1.599625672291271394 ) ) ;
#36321 = CARTESIAN_POINT ( 'NONE',  ( 4.786124093267453361, -1.070777880904892232, 1.993102913963458400 ) ) ;
#36323 = CARTESIAN_POINT ( 'NONE',  ( 6.475619172616331909, 2.016361193322095957, -0.6077647485315963438 ) ) ;
#36324 = DIRECTION ( 'NONE',  ( 0.000000000000000000, 0.000000000000000000, -1.000000000000000000 ) ) ;
#36325 = CARTESIAN_POINT ( 'NONE',  ( 3.314952806421948672, -1.569539724514938950, 1.350292352848787569 ) ) ;
#36326 = CARTESIAN_POINT ( 'NONE',  ( 4.566398809704347528, 4.221886787610169556, -0.7998128361456211532 ) ) ;
#36327 = CARTESIAN_POINT ( 'NONE',  ( -6.960724307482170605E-14, 1.484375000341481066, 1.570758158831758289 ) ) ;
#36328 = APPLICATION_PROTOCOL_DEFINITION ( 'draft international standard', 'automotive_design', 1998, #162660 ) ;
#36330 = CARTESIAN_POINT ( 'NONE',  ( 1.541497387563552479, -1.395045264726347600, -1.328863961831990181 ) ) ;
#36329 = CARTESIAN_POINT ( 'NONE',  ( -8.371269781434001800, 11.85389961405997816, -1.199719254218446718 ) ) ;
#36331 = UNCERTAINTY_MEASURE_WITH_UNIT (LENGTH_MEASURE( 1.000000000000000082E-05 ), #9616, 'distance_accuracy_value', 'NONE');
#36332 = CARTESIAN_POINT ( 'NONE',  ( -10.50000000000000000, 10.89999999999998259, 3.599999999999999201 ) ) ;
#36333 = CARTESIAN_POINT ( 'NONE',  ( 0.4144234639597261238, 0.7504023841088992564, 1.821203888109582447 ) ) ;
#36334 = CARTESIAN_POINT ( 'NONE',  ( 4.055297343818931033, 6.784911763547157193, 1.082531754730549078 ) ) ;
#36335 = CARTESIAN_POINT ( 'NONE',  ( 5.757945239960298167, 6.059206896687658883, 0.6045188873357760784 ) ) ;
#36336 = CARTESIAN_POINT ( 'NONE',  ( 10.45358220256315285, 1.000000000000000888, -5.892590188894412329 ) ) ;
#36337 = CARTESIAN_POINT ( 'NONE',  ( -4.115063316947640715, 4.759660943649018705, 1.199719254218462483 ) ) ;
#36338 = CARTESIAN_POINT ( 'NONE',  ( 1.635333617853749200, 2.074933741853498770, 0.7937918740310870858 ) ) ;
#36339 = CARTESIAN_POINT ( 'NONE',  ( 3.645630060059632083, -1.593344849414342290, -1.377153647973597073 ) ) ;
#36340 = CARTESIAN_POINT ( 'NONE',  ( -7.422162748838431412, 7.623887726591770608, -0.7998128361456362523 ) ) ;
#36341 = CARTESIAN_POINT ( 'NONE',  ( 8.274553823041976841, 8.548067636504127265, 1.040834085586084257E-14 ) ) ;
#36342 = CARTESIAN_POINT ( 'NONE',  ( 0.9767415019392856612, 1.717539547389279830, 0.7171521658363362306 ) ) ;
#36343 = CARTESIAN_POINT ( 'NONE',  ( 5.262536180398716290, 9.291375977107183104, -0.7998128361456291469 ) ) ;
#36344 = CARTESIAN_POINT ( 'NONE',  ( 3.337278367258157630, 7.045241861776501580, 0.7998128361456341429 ) ) ;
#36345 = CARTESIAN_POINT ( 'NONE',  ( -5.234856708652269042, 7.200695141551334721, 1.443375672974058777 ) ) ;
#36346 = CARTESIAN_POINT ( 'NONE',  ( -7.483737605063437215, 10.71448239167390604, 1.082531754730549967 ) ) ;
#36347 = CARTESIAN_POINT ( 'NONE',  ( 1.775790443353560732, 0.3575140072833470906, -2.090081039791711337 ) ) ;
#36348 = CARTESIAN_POINT ( 'NONE',  ( -5.749539660647037032, 8.865490816466966351, 1.199719254218454489 ) ) ;
#36350 = CARTESIAN_POINT ( 'NONE',  ( 4.510177812457000002, 1.961482754637720927, -0.04604004567236585910 ) ) ;
#36349 = CARTESIAN_POINT ( 'NONE',  ( -1.225000000000033396, 1.000000000000021760, -2.775557561562891351E-14 ) ) ;
#36351 = CARTESIAN_POINT ( 'NONE',  ( 3.010779355932476253, 1.566693023359872372, -1.489686202715050145 ) ) ;
#36352 = CARTESIAN_POINT ( 'NONE',  ( 1.522747961674526085, -1.733470594775164075, 0.6210259959333885860 ) ) ;
#36353 = B_SPLINE_CURVE_WITH_KNOTS ( 'NONE', 3,
 ( #198629, #102220, #185587, #149917 ),
 .UNSPECIFIED., .F., .F.,
 ( 4, 4 ),
 ( 4.091847515137629478E-16, 0.0006466603606995657751 ),
 .UNSPECIFIED. ) ;
#36354 = CARTESIAN_POINT ( 'NONE',  ( -4.192242263785030509, 7.388029550104924681, -0.8017062249071702507 ) ) ;
#36355 = EDGE_CURVE ( 'NONE', #112883, #70347, #58099, .T. ) ;
#36356 = CARTESIAN_POINT ( 'NONE',  ( 4.435344831996881787, 0.7407458870649418214, -1.574957418989342939 ) ) ;
#36357 = CARTESIAN_POINT ( 'NONE',  ( 0.3263184169968956772, 16.00000000000087397, -11.67999999558625213 ) ) ;
#36358 = CARTESIAN_POINT ( 'NONE',  ( 4.514501963670558560, 8.210743357683563559, 1.040834085586084257E-14 ) ) ;
#36359 = CARTESIAN_POINT ( 'NONE',  ( -10.16814981310353616, 6.288261174334121684, -5.589887627215723853 ) ) ;
#36360 = CARTESIAN_POINT ( 'NONE',  ( 7.723341061279088038, 12.16231500480096983, -0.7998128361456291469 ) ) ;
#36361 = CARTESIAN_POINT ( 'NONE',  ( 1.516726440323381331, 1.451591637995581996, -1.601975981646540426 ) ) ;
#36362 = ADVANCED_FACE ( 'NONE', ( #25830 ), #85931, .F. ) ;
#36363 = AXIS2_PLACEMENT_3D ( 'NONE', #152565, #4152, #55075 ) ;
#36364 = CARTESIAN_POINT ( 'NONE',  ( 3.427111092251767133, 0.9039706872599994059, 1.802141633730186543 ) ) ;
#36365 = CARTESIAN_POINT ( 'NONE',  ( -1.500000000000039524, 6.999999999999999112, -10.89724735885167739 ) ) ;
#36366 = CARTESIAN_POINT ( 'NONE',  ( 0.7784641540938314064, -1.199969256800371697, 1.797863220954009966 ) ) ;
#36367 = CARTESIAN_POINT ( 'NONE',  ( 3.151204110225252819, -1.610897424746060791, -1.136263970179009819 ) ) ;
#36368 = CARTESIAN_POINT ( 'NONE',  ( 6.609000000000015973, 2.967897204652646614, 2.453190122791535366 ) ) ;
#36369 = CARTESIAN_POINT ( 'NONE',  ( 3.790518096397344383, 1.638939831120878932, -1.041601972383674468 ) ) ;
#36372 = ORIENTED_EDGE ( 'NONE', *, *, #186277, .T. ) ;
#36371 = FACE_OUTER_BOUND ( 'NONE', #113988, .T. ) ;
#36370 = CARTESIAN_POINT ( 'NONE',  ( -8.581948047326017459, 11.99572790764693409, 1.082531754730558626 ) ) ;
#36373 = CARTESIAN_POINT ( 'NONE',  ( -4.624739795592943459, 6.488892076315448065, -1.443375672974066548 ) ) ;
#36374 = CARTESIAN_POINT ( 'NONE',  ( -0.1106856583841242386, 6.948332279000682732, -2.591999772403537516 ) ) ;
#36375 = CARTESIAN_POINT ( 'NONE',  ( 5.734172623936983904, 5.654565914206774124, 0.7998128361456352531 ) ) ;
#36376 = EDGE_CURVE ( 'NONE', #12663, #1871, #38086, .T. ) ;
#36377 = CARTESIAN_POINT ( 'NONE',  ( -6.154475385960665790, 6.144919136567696505, 0.000000000000000000 ) ) ;
#36378 = CARTESIAN_POINT ( 'NONE',  ( -7.632314129850253259, 7.869064337772231355, 0.7998128361456341429 ) ) ;
#36379 = CARTESIAN_POINT ( 'NONE',  ( -9.666600336419303829, 11.34041714965307968, 1.082531754730558626 ) ) ;
#36380 = CARTESIAN_POINT ( 'NONE',  ( 0.1478802723770406002, -1.707511933842900564, -1.397569297917726550 ) ) ;
#36381 = CARTESIAN_POINT ( 'NONE',  ( -1.642778471874998480, -2.851041666188706802, 2.845375778867863303 ) ) ;
#36382 = CARTESIAN_POINT ( 'NONE',  ( 3.977359813172594905, -0.1486911861427446802, 1.956209631609528099 ) ) ;
#36383 = CARTESIAN_POINT ( 'NONE',  ( 7.690499447449630210, 9.995335326823163058, 1.599625672291281386 ) ) ;
#36384 = CARTESIAN_POINT ( 'NONE',  ( 1.758435621656749603, 1.928751379572872571, -0.5880216644931559600 ) ) ;
#36385 = EDGE_LOOP ( 'NONE', ( #63641, #59927, #89702, #49776 ) ) ;
#36386 = CARTESIAN_POINT ( 'NONE',  ( 3.098929814713128561, 1.916056983672033587, 0.9012583305440853287 ) ) ;
#36387 = CARTESIAN_POINT ( 'NONE',  ( 1.499999999999989120, 1.306250000682816825, 0.000000000000000000 ) ) ;
#36389 = CARTESIAN_POINT ( 'NONE',  ( -6.905180308061733996, 6.950465202360470052, 0.7998128361456341429 ) ) ;
#36388 = CARTESIAN_POINT ( 'NONE',  ( 0.1747926744264677590, 2.047238405490480861, -2.272669950590770149 ) ) ;
#36390 = CARTESIAN_POINT ( 'NONE',  ( 2.993917163610838816, -0.5349900852187582379, -1.761688665035024304 ) ) ;
#36391 = ORIENTED_EDGE ( 'NONE', *, *, #84368, .T. ) ;
#36392 = CARTESIAN_POINT ( 'NONE',  ( -9.006694118179950692, 9.402231314165087284, 1.040834085586084257E-14 ) ) ;
#36393 = CARTESIAN_POINT ( 'NONE',  ( -3.157554866538104066E-14, 3.499999999999961808, 1.052419468952637160 ) ) ;
#36395 = VECTOR ( 'NONE', #201583, 1000.000000000000000 ) ;
#36394 = CARTESIAN_POINT ( 'NONE',  ( 4.219064148821600746, 1.637239594409030330, -1.347683705884415106 ) ) ;
#36396 = CARTESIAN_POINT ( 'NONE',  ( 10.89999999999920810, -2.095423061343886359E-15, 0.2598076211376220135 ) ) ;
#36397 = CARTESIAN_POINT ( 'NONE',  ( 7.786460292950004636, 7.978625184730144149, 1.040834085586084257E-14 ) ) ;
#36398 = CARTESIAN_POINT ( 'NONE',  ( 5.694623797941932963, -0.4965738858758206309, -1.999944147208564171 ) ) ;
#36400 = CARTESIAN_POINT ( 'NONE',  ( 2.173174093899932657, 1.133995793187540180, 1.450494936146892622 ) ) ;
#36399 = CARTESIAN_POINT ( 'NONE',  ( 0.8712809235682484887, -0.2783187086575014679, 1.840006102165496982 ) ) ;
#36401 = CARTESIAN_POINT ( 'NONE',  ( 8.772289083241844310, 10.19309100432570148, -1.199719254218446718 ) ) ;
#36402 = CARTESIAN_POINT ( 'NONE',  ( -6.337068562759858636, 6.936200024879327408, -0.9492287992594623525 ) ) ;
#36403 = CARTESIAN_POINT ( 'NONE',  ( 0.000000000000000000, 13.79999999999999893, 0.000000000000000000 ) ) ;
#36404 = CARTESIAN_POINT ( 'NONE',  ( -4.830635273601783020, 5.066023441139620331, -0.9190199222270474255 ) ) ;
#36405 = DIRECTION ( 'NONE',  ( 0.000000000000000000, -1.000000000000000000, 0.000000000000000000 ) ) ;
#36406 = CARTESIAN_POINT ( 'NONE',  ( 2.508667999599442755, -0.8457060194008919618, -2.038605049697986615 ) ) ;
#36407 = CARTESIAN_POINT ( 'NONE',  ( 4.903763976872734354, -0.6097993234682648200, 2.178603239016148052 ) ) ;
#36408 = CARTESIAN_POINT ( 'NONE',  ( -6.046573322014817897, 9.998159942418544333, 0.7216878364870458196 ) ) ;
#36409 = CARTESIAN_POINT ( 'NONE',  ( 4.974790932252576958, -1.306838681284767212, 1.254843474919357105 ) ) ;
#36410 = CARTESIAN_POINT ( 'NONE',  ( 4.329236433732988942, -1.484621416154695117, -1.210779873830228670 ) ) ;
#36411 = CARTESIAN_POINT ( 'NONE',  ( -1.201851678989727383E-14, 4.134375000341417028, 1.575800808251672791 ) ) ;
#36412 = CARTESIAN_POINT ( 'NONE',  ( 3.432457938460992342, 1.923125764579440844, 0.4332125842720236375 ) ) ;
#36413 = CARTESIAN_POINT ( 'NONE',  ( 5.524238439434661530, 1.113281918156138639, -1.503147240406087271 ) ) ;
#36414 = CARTESIAN_POINT ( 'NONE',  ( 5.195690723081275664, -1.315925274417349522, -1.316268238436297144 ) ) ;
#36415 = CARTESIAN_POINT ( 'NONE',  ( 0.6823417656249917140, 5.342708333674749177, 1.181850606188765695 ) ) ;
#36416 = AXIS2_PLACEMENT_3D ( 'NONE', #132195, #15187, #162544 ) ;
#36417 = CARTESIAN_POINT ( 'NONE',  ( 0.04025042243083893495, 0.7762349914572730381, 1.861342399428978389 ) ) ;
#36419 = CARTESIAN_POINT ( 'NONE',  ( 2.262461133243711675, 0.9012960022399997273, 1.903611236745775814 ) ) ;
#36418 = CARTESIAN_POINT ( 'NONE',  ( -2.616360457312984167, 5.996244933599686355, -0.7216878364870257245 ) ) ;
#36420 = VECTOR ( 'NONE', #209927, 1000.000000000000000 ) ;
#36421 = ADVANCED_FACE ( 'NONE', ( #133530 ), #132772, .T. ) ;
#36422 = CARTESIAN_POINT ( 'NONE',  ( 10.24726517383036928, 10.84956421242393887, 0.000000000000000000 ) ) ;
#36424 = CARTESIAN_POINT ( 'NONE',  ( 0.07479286986305544449, 2.888457405263197941, -2.344396930208477947 ) ) ;
#36423 = CARTESIAN_POINT ( 'NONE',  ( -1.001543065824772872E-14, 4.884375000341420581, 1.575800808251672791 ) ) ;
#36425 = CARTESIAN_POINT ( 'NONE',  ( 3.480829117359967917, -1.421471314662653196, 1.573842340227212366 ) ) ;
#36426 = CARTESIAN_POINT ( 'NONE',  ( -9.623628927379540343, -9.094708467121344952, 0.4567741993462124950 ) ) ;
#36427 = CARTESIAN_POINT ( 'NONE',  ( 1.617450697425420802, 1.681603173096592796, 1.118491831857356456 ) ) ;
#36428 = CARTESIAN_POINT ( 'NONE',  ( 0.6823417656249882723, 1.926041667008083991, -1.181850606188749264 ) ) ;
#36429 = CARTESIAN_POINT ( 'NONE',  ( -3.226477370372317743, 4.787309570232886280, 1.443375672974064550 ) ) ;
#36430 = ADVANCED_FACE ( 'NONE', ( #3461 ), #201659, .T. ) ;
#36431 = CARTESIAN_POINT ( 'NONE',  ( 3.499976210622149253, 7.235056012367825140, 0.7998128361456321445 ) ) ;
#36432 = ORIENTED_EDGE ( 'NONE', *, *, #149426, .F. ) ;
#36433 = CARTESIAN_POINT ( 'NONE',  ( 2.565889408427945995, 2.120439650033152379, -0.4189318973958494619 ) ) ;
#36434 = CARTESIAN_POINT ( 'NONE',  ( 6.890000000000025437, 1.315307137738566556, 1.839292676857922304 ) ) ;
#36437 = CARTESIAN_POINT ( 'NONE',  ( 4.202664430556261266, 4.005456045178151570, 0.7216878364870317197 ) ) ;
#36436 = DIRECTION ( 'NONE',  ( 0.000000000000000000, 8.546850786086437571E-32, 1.000000000000000000 ) ) ;
#36435 = CARTESIAN_POINT ( 'NONE',  ( 5.273195401072370281, 5.116759154198018855, -0.7998128361456481317 ) ) ;
#36438 = CARTESIAN_POINT ( 'NONE',  ( 11.94105721237523277, 10.07259215598211100, 1.187919463087244720 ) ) ;
#36439 = CARTESIAN_POINT ( 'NONE',  ( -8.043985462411137988, -6.893136966056773396, 7.503460210123606977 ) ) ;
#36440 = CARTESIAN_POINT ( 'NONE',  ( -7.863365906246061243, 10.19701286208565705, -1.443375672974059665 ) ) ;
#36441 = B_SPLINE_CURVE_WITH_KNOTS ( 'NONE', 3,
 ( #190954, #209327, #126057, #26327, #107660, #176863, #25265, #43682, #45816, #60974 ),
 .UNSPECIFIED., .F., .F.,
 ( 4, 2, 2, 2, 4 ),
 ( 0.000000000000000000, 0.0002216178067634645894, 0.0004432356135269291788, 0.0006648534202903938223, 0.0008864712270538583575 ),
 .UNSPECIFIED. ) ;
#36442 = CARTESIAN_POINT ( 'NONE',  ( 1.400213348495438437, -0.7931047570679079506, -2.043190674350242819 ) ) ;
#36443 = DIRECTION ( 'NONE',  ( 0.000000000000000000, 1.000000000000000000, 0.000000000000000000 ) ) ;
#36445 = CARTESIAN_POINT ( 'NONE',  ( -8.012344526598182026E-15, 11.54687500034139980, -1.575800808251669460 ) ) ;
#36444 = CARTESIAN_POINT ( 'NONE',  ( 1.762946358529001056, -1.599227303849257043, 1.600698272852623338 ) ) ;
#36446 = CARTESIAN_POINT ( 'NONE',  ( -8.727698198895085469, 11.20540053684285553, -1.599625672291263179 ) ) ;
#36447 = CARTESIAN_POINT ( 'NONE',  ( -5.734735788456164940, 5.792872629394710593, 0.7216878364870317197 ) ) ;
#36448 = CARTESIAN_POINT ( 'NONE',  ( 1.364683531249988535, 2.176041667008087543, 0.7879004041258500513 ) ) ;
#36449 = CARTESIAN_POINT ( 'NONE',  ( 4.693755526227673336, 8.251780594207492214, -0.6034641085399840010 ) ) ;
#36450 = CARTESIAN_POINT ( 'NONE',  ( 1.499999999999993117, 10.35416666666666607, 0.8660254037844409281 ) ) ;
#36451 = CARTESIAN_POINT ( 'NONE',  ( 3.685938805993322909, -0.8483273805379875077, 1.501759545097125059 ) ) ;
#36452 = CARTESIAN_POINT ( 'NONE',  ( 5.011674058906918638, 5.875983152593414971, 1.199719254218452047 ) ) ;
#36453 = CARTESIAN_POINT ( 'NONE',  ( 2.442341840454059554, 0.3829199517304190947, 1.727643488062768240 ) ) ;
#36454 = CARTESIAN_POINT ( 'NONE',  ( 2.860023507607223792, 0.7224298503675909977, -1.879176508647899535 ) ) ;
#36455 = CARTESIAN_POINT ( 'NONE',  ( 5.860442804830619856, 0.8892231252738895808, 2.019869304780027353 ) ) ;
#36456 = ORIENTED_EDGE ( 'NONE', *, *, #3651, .T. ) ;
#36457 = CARTESIAN_POINT ( 'NONE',  ( 4.043226763451240657, 0.1031935428237283348, 2.017299519520795670 ) ) ;
#36458 = CARTESIAN_POINT ( 'NONE',  ( -6.261886844665283114, 8.398896966899865646, 1.599625672291269396 ) ) ;
#36459 = CARTESIAN_POINT ( 'NONE',  ( 3.480092364642515701, -2.014234743589532695, -0.09611699103692641910 ) ) ;
#36461 = VERTEX_POINT ( 'NONE', #205949 ) ;
#36460 = CARTESIAN_POINT ( 'NONE',  ( 4.394648900434598104, -1.758782010937329110, -0.4337233627825891613 ) ) ;
#36462 = ORIENTED_EDGE ( 'NONE', *, *, #175516, .T. ) ;
#36463 = CARTESIAN_POINT ( 'NONE',  ( 2.992876365407059147, 1.605230647100181596, -0.9602576221170722182 ) ) ;
#36464 = CARTESIAN_POINT ( 'NONE',  ( 1.483456582844651095, 7.293967155396083868, -4.258619948151496359 ) ) ;
#36465 = CARTESIAN_POINT ( 'NONE',  ( 1.898553772666348394, -1.876154101037771582, -0.3696338911259658411 ) ) ;
#36467 = AXIS2_PLACEMENT_3D ( 'NONE', #31472, #136431, #201383 ) ;
#36466 = CARTESIAN_POINT ( 'NONE',  ( 1.220146605508150803E-14, 9.687500000000000000, -1.499999999999998446 ) ) ;
#36468 = CARTESIAN_POINT ( 'NONE',  ( -10.76260246389097297, 4.190717020667873882, -6.707086991120802644 ) ) ;
#36469 = CARTESIAN_POINT ( 'NONE',  ( 3.147653791585693028, 8.920000000000001705, 2.419999999999999485 ) ) ;
#36470 = CARTESIAN_POINT ( 'NONE',  ( 0.6823417656249899377, 2.655208333674753618, 1.181850606188767472 ) ) ;
#36471 = CARTESIAN_POINT ( 'NONE',  ( 0.3692113334803036606, -1.616751421056546789, -1.021125667832627260 ) ) ;
#36472 = PRESENTATION_LAYER_ASSIGNMENT (  '', '', ( #71085 ) ) ;
#36473 = CARTESIAN_POINT ( 'NONE',  ( 5.397554552016216256, 7.390509292142662723, 1.443375672974065660 ) ) ;
#36474 = CARTESIAN_POINT ( 'NONE',  ( 1.767943819387544968, -1.947426213878332035, 0.2369139692007388165 ) ) ;
#36475 = CARTESIAN_POINT ( 'NONE',  ( 0.3685172633814579046, -0.5404119286356176000, 1.942243004588292132 ) ) ;
#36476 = CARTESIAN_POINT ( 'NONE',  ( -5.074494633264801990, 9.142270515442742607, 0.7998128361456291469 ) ) ;
#36477 = CARTESIAN_POINT ( 'NONE',  ( 3.972980863544761654, -1.569110274459505350, 1.426624754300914510 ) ) ;
#36479 = CARTESIAN_POINT ( 'NONE',  ( -10.52284260640670688, 5.420240069097000735, -5.071998063130033430 ) ) ;
#36478 = CARTESIAN_POINT ( 'NONE',  ( 9.317477881089539338, 11.89347683273640932, 1.599625672291279388 ) ) ;
#36480 = CARTESIAN_POINT ( 'NONE',  ( 5.518811311470022574, 1.820418058502238035, 0.7569790930031635723 ) ) ;
#36481 = CARTESIAN_POINT ( 'NONE',  ( 1.364683531249988535, 1.613541667008084879, 0.7879004041258500513 ) ) ;
#36482 = ORIENTED_EDGE ( 'NONE', *, *, #19306, .F. ) ;
#36483 = CARTESIAN_POINT ( 'NONE',  ( 1.599367111750239934, -0.2554771505851380908, 2.101684664062503316 ) ) ;
#36484 = CARTESIAN_POINT ( 'NONE',  ( 11.09412727165957691, 8.002531996343789089, 4.594739555395619846 ) ) ;
#36485 = CARTESIAN_POINT ( 'NONE',  ( 3.051297593704501043, 1.777051743073382761, -1.062048545217339823 ) ) ;
#36486 = CARTESIAN_POINT ( 'NONE',  ( 4.309512724297349884, 6.121127159803966933, 1.599625672291261402 ) ) ;
#36487 = CARTESIAN_POINT ( 'NONE',  ( 5.306037014901791693, 7.283738832175834510, 1.599625672291269396 ) ) ;
#36488 = ORIENTED_EDGE ( 'NONE', *, *, #159575, .F. ) ;
#36490 = CARTESIAN_POINT ( 'NONE',  ( 3.680148631105580215, 6.380924938676771241, -1.199719254218446718 ) ) ;
#36489 = CARTESIAN_POINT ( 'NONE',  ( 4.400388060213418662, 1.616114658936588011, -1.326231919226998901 ) ) ;
#36493 = ORIENTED_EDGE ( 'NONE', *, *, #69678, .T. ) ;
#36492 = CARTESIAN_POINT ( 'NONE',  ( 1.119438638434491429, -0.4408070000805932032, 1.756890142956100576 ) ) ;
#36491 = CARTESIAN_POINT ( 'NONE',  ( 3.311362000969253039, -0.3573404788377897989, 1.790086433339547201 ) ) ;
#36494 = CARTESIAN_POINT ( 'NONE',  ( 10.16199982864259788, 11.81442020729326536, 1.199719254218452047 ) ) ;
#36495 = CARTESIAN_POINT ( 'NONE',  ( 9.379604873787226182, 12.64221115367513626, 6.544017673515419631 ) ) ;
#36496 = CARTESIAN_POINT ( 'NONE',  ( 5.807716119225245777, -0.5415507062403871474, 2.139171552897000339 ) ) ;
#36497 = CARTESIAN_POINT ( 'NONE',  ( -0.6823417656250039265, 9.130208333674726617, -1.181850606188755259 ) ) ;
#36498 = ORIENTED_EDGE ( 'NONE', *, *, #85279, .F. ) ;
#36499 = CARTESIAN_POINT ( 'NONE',  ( 4.160738352132353768, 0.5130957772990808463, 1.842076966104645663 ) ) ;
#36500 = CARTESIAN_POINT ( 'NONE',  ( -4.485049888022365927, 4.126979712314507331, 0.7998128361456341429 ) ) ;
#36501 = CARTESIAN_POINT ( 'NONE',  ( 6.774270308322468459, 11.05506579301824743, 0.7998128361456462443 ) ) ;
#36502 = CARTESIAN_POINT ( 'NONE',  ( 6.672334155782003506, -0.9722939650993901450, -1.827837255792996718 ) ) ;
#36503 = CARTESIAN_POINT ( 'NONE',  ( -1.360316468750021768, 0.1718750003414371008, -3.295974604355933479E-14 ) ) ;
#36504 = CARTESIAN_POINT ( 'NONE',  ( 4.243338890952890630, 5.973648010910253880, -1.443375672974051449 ) ) ;
#36505 = CARTESIAN_POINT ( 'NONE',  ( 6.603104432341277530, -0.4828188497946246382, 2.145653685147373313 ) ) ;
#36506 = CARTESIAN_POINT ( 'NONE',  ( 6.098455030413784783, 7.112933956528650015, -1.126327413477963502 ) ) ;
#36507 = CARTESIAN_POINT ( 'NONE',  ( -5.600682685854159182, 15.51843887179352244, -10.62222670599373764 ) ) ;
#36508 = CARTESIAN_POINT ( 'NONE',  ( 3.268673085221412311, -1.727008210369033847, -0.7190761260571985058 ) ) ;
#36509 = CARTESIAN_POINT ( 'NONE',  ( 1.642778471875001811, -1.830208332855375097, 2.845375778867859751 ) ) ;
#36510 = CYLINDRICAL_SURFACE ( 'NONE', #46543, 1.250000000000000000 ) ;
#36511 = CARTESIAN_POINT ( 'NONE',  ( -7.551528373131759508, 7.912463978182924684, 1.040834085586084257E-14 ) ) ;
#36512 = CARTESIAN_POINT ( 'NONE',  ( 5.422335090822693715, 5.290755458906732933, 0.000000000000000000 ) ) ;
#36513 = CARTESIAN_POINT ( 'NONE',  ( 6.308621549060418054, 6.254479983525607523, 0.7998128361456341429 ) ) ;
#36514 = CARTESIAN_POINT ( 'NONE',  ( 0.2859135117265668158, -1.207096249910791563, -1.556650298907244823 ) ) ;
#36515 = CARTESIAN_POINT ( 'NONE',  ( 0.7554827284574801016, 1.942536278707338360, -0.5405140857882018146 ) ) ;
#36516 = CARTESIAN_POINT ( 'NONE',  ( -8.123306592882240551, 12.62894145833798376, 0.000000000000000000 ) ) ;
#36517 = CARTESIAN_POINT ( 'NONE',  ( 5.885121196783658526, 9.023669275293071834, 1.199719254218452047 ) ) ;
#36518 = FACE_OUTER_BOUND ( 'NONE', #186431, .T. ) ;
#36519 = CARTESIAN_POINT ( 'NONE',  ( 0.9553299046189435151, 0.4242123182428610972, -2.149831459026855907 ) ) ;
#36520 = CARTESIAN_POINT ( 'NONE',  ( 6.006453938882227561, -0.6616566355047011072, -1.701761020394356283 ) ) ;
#36521 = CARTESIAN_POINT ( 'NONE',  ( -3.623053363349869382, 5.249981562040033189, 1.599625672291267398 ) ) ;
#36522 = CARTESIAN_POINT ( 'NONE',  ( 4.665414256878284149, 6.536345614481700927, -1.443375672974068769 ) ) ;
#36523 = CARTESIAN_POINT ( 'NONE',  ( 7.913155211870404493, 12.38376484715752213, 0.7998128361456462443 ) ) ;
#36524 = CARTESIAN_POINT ( 'NONE',  ( 4.729096653068339151, 4.411700938201493116, -0.7998128361456211532 ) ) ;
#36525 = CARTESIAN_POINT ( 'NONE',  ( 3.902768115887398803, 5.646591783325653147, -1.599625672291269396 ) ) ;
#36526 = VERTEX_POINT ( 'NONE', #190758 ) ;
#36528 = CARTESIAN_POINT ( 'NONE',  ( 0.7857919059152475016, 1.939557017834290020, -0.5388494671653855095 ) ) ;
#36527 = CARTESIAN_POINT ( 'NONE',  ( 3.931074656914943954, -1.272613488525012659, -1.330884258478791438 ) ) ;
#36529 = CARTESIAN_POINT ( 'NONE',  ( 1.827921470121370850, -1.625240468190300103, 1.625389258475460563 ) ) ;
#36531 = CARTESIAN_POINT ( 'NONE',  ( 0.4087542164426588021, -1.499397391050528050, 1.102066480322369202 ) ) ;
#36530 = CARTESIAN_POINT ( 'NONE',  ( 4.121315508874254796, 5.831287398485176077, -1.443375672974051449 ) ) ;
#36532 = CARTESIAN_POINT ( 'NONE',  ( -3.474999999999998312, -0.6708333333333343917, 2.006292185433951047 ) ) ;
#36533 = CARTESIAN_POINT ( 'NONE',  ( -5.739179097286464248, 5.590130456455974617, -0.7998128361456221525 ) ) ;
#36534 = CARTESIAN_POINT ( 'NONE',  ( -9.404907904283509978, 14.48154074430288851, -7.453273792521815544 ) ) ;
#36535 = CARTESIAN_POINT ( 'NONE',  ( 4.166199421025416960, 1.911861072351704882, -0.05224187775455800542 ) ) ;
#36536 = CARTESIAN_POINT ( 'NONE',  ( -9.622536337397040285, 12.24937836509514710, 1.599625672291281386 ) ) ;
#36537 = CARTESIAN_POINT ( 'NONE',  ( 6.483128551184942800, 6.753495492978965231, -0.1682882784904728146 ) ) ;
#36538 = CARTESIAN_POINT ( 'NONE',  ( -5.641601317062239218, 8.635599732330991429, -1.082531754730549967 ) ) ;
#36540 = CARTESIAN_POINT ( 'NONE',  ( 2.447944060942487621, 1.870205405844455049, 0.04815357881200743595 ) ) ;
#36539 = CARTESIAN_POINT ( 'NONE',  ( 3.790639713653580767, 1.765158817303988048, -1.120165474576743536 ) ) ;
#36541 = CARTESIAN_POINT ( 'NONE',  ( 7.266807147244743526, 11.42176607185347414, -0.7216878364870267237 ) ) ;
#36542 = CARTESIAN_POINT ( 'NONE',  ( -1.364683531250010740, 5.551041667008087543, -0.7879004041258300672 ) ) ;
#36543 = CARTESIAN_POINT ( 'NONE',  ( 3.122313433385078607, 0.04571620936353942150, 1.740018996352102443 ) ) ;
#36544 = CARTESIAN_POINT ( 'NONE',  ( 4.741601036477289810, 6.554953847355395880, 1.599625672291267398 ) ) ;
#36545 = CARTESIAN_POINT ( 'NONE',  ( -5.507549045659300369, 6.008722659170706137, 0.9225295215002001781 ) ) ;
#36546 = CARTESIAN_POINT ( 'NONE',  ( 3.633171361085251849, -1.593041208078986193, 0.6618793944016196917 ) ) ;
#36547 =( BOUNDED_SURFACE ( )  B_SPLINE_SURFACE ( 1, 2, ( 
 ( #86550, #201337, #70269, #54055, #37801, #152615, #4199, #151566, #133203, #184037, #103876, #87620, #85480, #167802, #83334, #19399, #2064, #150504, #153691, #3133, #69203, #52977, #5260, #174230, #124476, #6342, #156901, #122349, #7410, #89779, #140675, #9562, #157971, #72414, #206690, #139593, #56188, #73492, #138515, #58319, #205616, #190433, #42092, #71336, #141746, #108207, #25804, #170994, #155826, #121268, #75638, #57256, #23669, #123416, #204539, #104954, #189380, #91913, #187243, #173155, #137453, #203467, #55122, #41023, #38869, #188304, #88699, #39946, #22593, #154758, #107132, #106053, #24737, #172077, #90838, #8489, #74573, #21145, #118741, #17955, #100297, #136009, #202022, #184725, #86183, #34225, #104580, #102427, #170625, #101359, #87249, #166364, #153314, #182601, #19029, #134957, #36349, #22211, #53682, #88324, #70967, #3825, #133908, #1703, #154388, #117686, #119813, #169563, #85109, #84042, #203102, #4889, #186870, #150130, #168496, #137077, #167437, #183678, #67757, #54747, #199914, #51561, #116608, #5966, #185793, #20095, #138149, #151195, #35283, #2766, #68837, #200965, #52612, #152252, #69898, #37426, #103503, #120897, #72036, #38502, #50487, #89402, #207397, #56883, #106756, #156534, #189012, #73111, #23292, #174930, #42799, #90467, #204158, #121968, #157604, #191133, #26510, #11320, #24357, #139211, #43862, #173865, #108907, #155451, #175988, #109978, #8125, #206324, #92619, #172784, #158661, #74211, #25440, #159722, #55813, #7034, #141387, #57949, #107838, #9200, #40655, #39564, #140306, #10259, #91546, #124114, #41729, #190077, #76334, #75272, #208448, #142441, #187934 ),
 ( #27582, #59016, #125172, #60081, #126238, #192200, #93680, #205242, #77399, #105666, #123058, #171693, #107522, #123803, #189763, #142125, #27258, #42481, #41415, #209196, #90158, #188702, #172467, #156224, #24055, #105347, #73893, #72808, #57643, #7801, #6729, #11001, #22975, #174618, #138909, #124856, #40338, #139987, #206008, #106444, #204929, #155147, #92309, #26194, #173552, #121659, #39254, #74958, #108590, #158353, #143206, #25126, #56580, #175670, #91229, #9946, #122739, #93366, #159402, #157289, #8879, #76022, #141068, #208138, #207075, #58706, #77078, #187627, #190820, #59768, #125927, #191885, #43546, #109668, #171384, #89093, #94433, #129131, #197220, #176724, #130183, #60836, #164729, #126997, #79217, #196176, #28336, #192956, #160472, #146382, #64038, #110724, #148493, #12079, #62961, #96567, #211337, #14191, #31548, #195107, #78146, #144277, #212395, #47817, #46743, #162614, #44608, #114975, #112856, #180976, #80283, #97623, #194026, #178872, #210270, #61908, #163681, #82403, #128070, #15263, #113929, #213454, #48861, #32598, #81350, #147430, #179925, #45676, #30483, #65077, #131232, #98673, #16318, #111793, #177798, #145336, #29415, #95506, #161553, #13141, #199337, #83469, #54179, #152742, #67196, #185222, #34715, #52050, #134400, #168990, #170049, #104005, #50983, #20589, #184164, #100786, #118177, #117105, #86675, #35785, #4323, #70393, #60, #21634, #136510, #202530, #165800, #68267, #49917, #37931, #101861, #2191, #200402, #201462, #183106, #166868, #17385, #18462, #198275, #133333, #84540, #135441, #150630, #69330, #3262, #167929, #87742, #19528, #66124, #85605, #132267, #36846, #116038 ) ),
 .UNSPECIFIED., .F., .F., .F. ) 
 B_SPLINE_SURFACE_WITH_KNOTS ( ( 2, 2 ),
 ( 3, 2, 2, 2, 2, 2, 2, 2, 2, 2, 2, 2, 2, 2, 2, 2, 2, 2, 2, 2, 2, 2, 2, 2, 2, 2, 2, 2, 2, 2, 2, 2, 2, 2, 2, 2, 2, 2, 2, 2, 2, 2, 2, 2, 2, 2, 2, 2, 2, 2, 2, 2, 2, 2, 2, 2, 2, 2, 2, 2, 2, 2, 2, 2, 2, 2, 2, 2, 2, 2, 2, 2, 2, 2, 2, 2, 2, 2, 2, 2, 2, 2, 2, 2, 2, 2, 2, 2, 2, 2, 2, 2, 2, 2, 2, 2, 3 ),
 ( 0.000000000000000000, 1.000000000000000000 ),
 ( 0.000000000000000000, 0.01041666666666666609, 0.02083333333333333218, 0.03125000000000000000, 0.04166666666666666435, 0.05208333333333333565, 0.06250000000000000000, 0.07291666666666667129, 0.08333333333333332871, 0.09375000000000000000, 0.1041666666666666713, 0.1145833333333333287, 0.1250000000000000000, 0.1354166666666666574, 0.1458333333333333426, 0.1562500000000000000, 0.1666666666666666574, 0.1770833333333333426, 0.1875000000000000000, 0.1979166666666666574, 0.2083333333333333426, 0.2187500000000000000, 0.2291666666666666574, 0.2395833333333333426, 0.2500000000000000000, 0.2604166666666666852, 0.2708333333333333148, 0.2812500000000000000, 0.2916666666666666852, 0.3020833333333333148, 0.3125000000000000000, 0.3229166666666666852, 0.3333333333333333148, 0.3437500000000000000, 0.3541666666666666852, 0.3645833333333333148, 0.3750000000000000000, 0.3854166666666666852, 0.3958333333333333148, 0.4062500000000000000, 0.4166666666666666852, 0.4270833333333333148, 0.4375000000000000000, 0.4479166666666666852, 0.4583333333333333148, 0.4687500000000000000, 0.4791666666666666852, 0.4895833333333333148, 0.5000000000000000000, 0.5104166666666666297, 0.5208333333333333703, 0.5312500000000000000, 0.5416666666666666297, 0.5520833333333333703, 0.5625000000000000000, 0.5729166666666666297, 0.5833333333333333703, 0.5937500000000000000, 0.6041666666666666297, 0.6145833333333333703, 0.6250000000000000000, 0.6354166666666666297, 0.6458333333333333703, 0.6562500000000000000, 0.6666666666666666297, 0.6770833333333333703, 0.6875000000000000000, 0.6979166666666666297, 0.7083333333333333703, 0.7187500000000000000, 0.7291666666666666297, 0.7395833333333333703, 0.7500000000000000000, 0.7604166666666666297, 0.7708333333333333703, 0.7812500000000000000, 0.7916666666666666297, 0.8020833333333333703, 0.8125000000000000000, 0.8229166666666666297, 0.8333333333333333703, 0.8437500000000000000, 0.8541666666666666297, 0.8645833333333333703, 0.8750000000000000000, 0.8854166666666666297, 0.8958333333333333703, 0.9062500000000000000, 0.9166666666666666297, 0.9270833333333333703, 0.9375000000000000000, 0.9479166666666666297, 0.9583333333333333703, 0.9687500000000000000, 0.9791666666666666297, 0.9895833333333333703, 1.000000000000000000 ),
 .UNSPECIFIED. ) 
 GEOMETRIC_REPRESENTATION_ITEM ( )  RATIONAL_B_SPLINE_SURFACE ( (
 ( 1.000000000000000000, 0.8660254037844387076, 1.000000000000000000, 0.8660254037844387076, 1.000000000000000000, 0.8660254037844387076, 1.000000000000000000, 0.8660254037844387076, 1.000000000000000000, 0.8660254037844387076, 1.000000000000000000, 0.8660254037844387076, 1.000000000000000000, 0.8660254037844387076, 1.000000000000000000, 0.8660254037844387076, 1.000000000000000000, 0.8660254037844387076, 1.000000000000000000, 0.8660254037844387076, 1.000000000000000000, 0.8660254037844387076, 1.000000000000000000, 0.8660254037844387076, 1.000000000000000000, 0.8660254037844387076, 1.000000000000000000, 0.8660254037844387076, 1.000000000000000000, 0.8660254037844387076, 1.000000000000000000, 0.8660254037844387076, 1.000000000000000000, 0.8660254037844387076, 1.000000000000000000, 0.8660254037844387076, 1.000000000000000000, 0.8660254037844387076, 1.000000000000000000, 0.8660254037844387076, 1.000000000000000000, 0.8660254037844387076, 1.000000000000000000, 0.8660254037844387076, 1.000000000000000000, 0.8660254037844387076, 1.000000000000000000, 0.8660254037844387076, 1.000000000000000000, 0.8660254037844387076, 1.000000000000000000, 0.8660254037844387076, 1.000000000000000000, 0.8660254037844387076, 1.000000000000000000, 0.8660254037844387076, 1.000000000000000000, 0.8660254037844387076, 1.000000000000000000, 0.8660254037844387076, 1.000000000000000000, 0.8660254037844387076, 1.000000000000000000, 0.8660254037844387076, 1.000000000000000000, 0.8660254037844387076, 1.000000000000000000, 0.8660254037844387076, 1.000000000000000000, 0.8660254037844387076, 1.000000000000000000, 0.8660254037844387076, 1.000000000000000000, 0.8660254037844387076, 1.000000000000000000, 0.8660254037844387076, 1.000000000000000000, 0.8660254037844387076, 1.000000000000000000, 0.8660254037844387076, 1.000000000000000000, 0.8660254037844387076, 1.000000000000000000, 0.8660254037844387076, 1.000000000000000000, 0.8660254037844387076, 1.000000000000000000, 0.8660254037844387076, 1.000000000000000000, 0.8660254037844387076, 1.000000000000000000, 0.8660254037844387076, 1.000000000000000000, 0.8660254037844387076, 1.000000000000000000, 0.8660254037844387076, 1.000000000000000000, 0.8660254037844387076, 1.000000000000000000, 0.8660254037844387076, 1.000000000000000000, 0.8660254037844387076, 1.000000000000000000, 0.8660254037844387076, 1.000000000000000000, 0.8660254037844387076, 1.000000000000000000, 0.8660254037844387076, 1.000000000000000000, 0.8660254037844387076, 1.000000000000000000, 0.8660254037844387076, 1.000000000000000000, 0.8660254037844387076, 1.000000000000000000, 0.8660254037844387076, 1.000000000000000000, 0.8660254037844387076, 1.000000000000000000, 0.8660254037844387076, 1.000000000000000000, 0.8660254037844387076, 1.000000000000000000, 0.8660254037844387076, 1.000000000000000000, 0.8660254037844387076, 1.000000000000000000, 0.8660254037844387076, 1.000000000000000000, 0.8660254037844387076, 1.000000000000000000, 0.8660254037844387076, 1.000000000000000000, 0.8660254037844387076, 1.000000000000000000, 0.8660254037844387076, 1.000000000000000000, 0.8660254037844387076, 1.000000000000000000, 0.8660254037844387076, 1.000000000000000000, 0.8660254037844387076, 1.000000000000000000, 0.8660254037844387076, 1.000000000000000000, 0.8660254037844387076, 1.000000000000000000, 0.8660254037844387076, 1.000000000000000000, 0.8660254037844387076, 1.000000000000000000, 0.8660254037844387076, 1.000000000000000000, 0.8660254037844387076, 1.000000000000000000, 0.8660254037844387076, 1.000000000000000000, 0.8660254037844387076, 1.000000000000000000, 0.8660254037844387076, 1.000000000000000000, 0.8660254037844387076, 1.000000000000000000, 0.8660254037844387076, 1.000000000000000000, 0.8660254037844387076, 1.000000000000000000, 0.8660254037844387076, 1.000000000000000000, 0.8660254037844387076, 1.000000000000000000, 0.8660254037844387076, 1.000000000000000000, 0.8660254037844387076, 1.000000000000000000, 0.8660254037844387076, 1.000000000000000000, 0.8660254037844387076, 1.000000000000000000, 0.8660254037844387076, 1.000000000000000000, 0.8660254037844387076, 1.000000000000000000, 0.8660254037844387076, 1.000000000000000000, 0.8660254037844387076, 1.000000000000000000, 0.8660254037844387076, 1.000000000000000000, 0.8660254037844387076, 1.000000000000000000, 0.8660254037844387076, 1.000000000000000000),
 ( 1.000000000000000000, 0.8660254037844387076, 1.000000000000000000, 0.8660254037844387076, 1.000000000000000000, 0.8660254037844387076, 1.000000000000000000, 0.8660254037844387076, 1.000000000000000000, 0.8660254037844387076, 1.000000000000000000, 0.8660254037844387076, 1.000000000000000000, 0.8660254037844387076, 1.000000000000000000, 0.8660254037844387076, 1.000000000000000000, 0.8660254037844387076, 1.000000000000000000, 0.8660254037844387076, 1.000000000000000000, 0.8660254037844387076, 1.000000000000000000, 0.8660254037844387076, 1.000000000000000000, 0.8660254037844387076, 1.000000000000000000, 0.8660254037844387076, 1.000000000000000000, 0.8660254037844387076, 1.000000000000000000, 0.8660254037844387076, 1.000000000000000000, 0.8660254037844387076, 1.000000000000000000, 0.8660254037844387076, 1.000000000000000000, 0.8660254037844387076, 1.000000000000000000, 0.8660254037844387076, 1.000000000000000000, 0.8660254037844387076, 1.000000000000000000, 0.8660254037844387076, 1.000000000000000000, 0.8660254037844387076, 1.000000000000000000, 0.8660254037844387076, 1.000000000000000000, 0.8660254037844387076, 1.000000000000000000, 0.8660254037844387076, 1.000000000000000000, 0.8660254037844387076, 1.000000000000000000, 0.8660254037844387076, 1.000000000000000000, 0.8660254037844387076, 1.000000000000000000, 0.8660254037844387076, 1.000000000000000000, 0.8660254037844387076, 1.000000000000000000, 0.8660254037844387076, 1.000000000000000000, 0.8660254037844387076, 1.000000000000000000, 0.8660254037844387076, 1.000000000000000000, 0.8660254037844387076, 1.000000000000000000, 0.8660254037844387076, 1.000000000000000000, 0.8660254037844387076, 1.000000000000000000, 0.8660254037844387076, 1.000000000000000000, 0.8660254037844387076, 1.000000000000000000, 0.8660254037844387076, 1.000000000000000000, 0.8660254037844387076, 1.000000000000000000, 0.8660254037844387076, 1.000000000000000000, 0.8660254037844387076, 1.000000000000000000, 0.8660254037844387076, 1.000000000000000000, 0.8660254037844387076, 1.000000000000000000, 0.8660254037844387076, 1.000000000000000000, 0.8660254037844387076, 1.000000000000000000, 0.8660254037844387076, 1.000000000000000000, 0.8660254037844387076, 1.000000000000000000, 0.8660254037844387076, 1.000000000000000000, 0.8660254037844387076, 1.000000000000000000, 0.8660254037844387076, 1.000000000000000000, 0.8660254037844387076, 1.000000000000000000, 0.8660254037844387076, 1.000000000000000000, 0.8660254037844387076, 1.000000000000000000, 0.8660254037844387076, 1.000000000000000000, 0.8660254037844387076, 1.000000000000000000, 0.8660254037844387076, 1.000000000000000000, 0.8660254037844387076, 1.000000000000000000, 0.8660254037844387076, 1.000000000000000000, 0.8660254037844387076, 1.000000000000000000, 0.8660254037844387076, 1.000000000000000000, 0.8660254037844387076, 1.000000000000000000, 0.8660254037844387076, 1.000000000000000000, 0.8660254037844387076, 1.000000000000000000, 0.8660254037844387076, 1.000000000000000000, 0.8660254037844387076, 1.000000000000000000, 0.8660254037844387076, 1.000000000000000000, 0.8660254037844387076, 1.000000000000000000, 0.8660254037844387076, 1.000000000000000000, 0.8660254037844387076, 1.000000000000000000, 0.8660254037844387076, 1.000000000000000000, 0.8660254037844387076, 1.000000000000000000, 0.8660254037844387076, 1.000000000000000000, 0.8660254037844387076, 1.000000000000000000, 0.8660254037844387076, 1.000000000000000000, 0.8660254037844387076, 1.000000000000000000, 0.8660254037844387076, 1.000000000000000000, 0.8660254037844387076, 1.000000000000000000, 0.8660254037844387076, 1.000000000000000000, 0.8660254037844387076, 1.000000000000000000, 0.8660254037844387076, 1.000000000000000000, 0.8660254037844387076, 1.000000000000000000, 0.8660254037844387076, 1.000000000000000000, 0.8660254037844387076, 1.000000000000000000, 0.8660254037844387076, 1.000000000000000000, 0.8660254037844387076, 1.000000000000000000, 0.8660254037844387076, 1.000000000000000000, 0.8660254037844387076, 1.000000000000000000, 0.8660254037844387076, 1.000000000000000000, 0.8660254037844387076, 1.000000000000000000, 0.8660254037844387076, 1.000000000000000000, 0.8660254037844387076, 1.000000000000000000, 0.8660254037844387076, 1.000000000000000000, 0.8660254037844387076, 1.000000000000000000, 0.8660254037844387076, 1.000000000000000000) ) ) 
 REPRESENTATION_ITEM ( '' )  SURFACE ( )  );
#36548 = CARTESIAN_POINT ( 'NONE',  ( 3.702820756938397295, 1.880440254450808757, 1.125299312022425280 ) ) ;
#36549 = CARTESIAN_POINT ( 'NONE',  ( 6.006501602161061548, -0.7906231143557163055, -2.060575041408031272 ) ) ;
#36550 = DIRECTION ( 'NONE',  ( 0.000000000000000000, -1.000000000000000000, 0.000000000000000000 ) ) ;
#36551 = CARTESIAN_POINT ( 'NONE',  ( 4.153319900303814372, 1.837149938469440302, -1.156618460589062813 ) ) ;
#36552 = CARTESIAN_POINT ( 'NONE',  ( 2.332394550857110893, 1.770734860448031300, 0.4440693575865002907 ) ) ;
#36553 = CARTESIAN_POINT ( 'NONE',  ( -1.500000000000015099, 9.260416667349463893, -0.8660254037844309360 ) ) ;
#36554 = CARTESIAN_POINT ( 'NONE',  ( 4.768830992622041798, -0.2625661012465319022, -2.100967800990781509 ) ) ;
#36555 = VERTEX_POINT ( 'NONE', #105280 ) ;
#36557 = CARTESIAN_POINT ( 'NONE',  ( 1.364683531249986537, 2.467708333674753174, -0.7879004041258239610 ) ) ;
#36556 = CARTESIAN_POINT ( 'NONE',  ( 4.493851497812589635, -2.291808737193799406, -0.05710960328321466883 ) ) ;
#36558 = CARTESIAN_POINT ( 'NONE',  ( 6.720655732516650716, 1.268691918110446570, 2.040305333170799429 ) ) ;
#36559 = CARTESIAN_POINT ( 'NONE',  ( 9.083072846151447166, 12.68433652289702884, 1.199719254218450271 ) ) ;
#36560 = CARTESIAN_POINT ( 'NONE',  ( 0.9266185682500321930, -0.9568284065921551784, -1.892426592148554132 ) ) ;
#36561 = CARTESIAN_POINT ( 'NONE',  ( -4.229780737783618072, 6.918199379847403740, 1.082531754730560403 ) ) ;
#36562 = ADVANCED_FACE ( 'NONE', ( #23991 ), #107462, .T. ) ;
#36563 = AXIS2_PLACEMENT_3D ( 'NONE', #137896, #9999, #104318 ) ;
#36564 = DIRECTION ( 'NONE',  ( 1.000000000000000000, 0.000000000000000000, -1.224646799147353207E-16 ) ) ;
#36565 = CARTESIAN_POINT ( 'NONE',  ( -6.385527161912131433, 6.552129231760014605, 0.7216878364870317197 ) ) ;
#36567 = CARTESIAN_POINT ( 'NONE',  ( -0.7500000000000006661, 11.98958333401613174, -1.299038105676657340 ) ) ;
#36566 = CARTESIAN_POINT ( 'NONE',  ( 6.883263157960366030, 0.5727201817382967519, 2.105997115537924902 ) ) ;
#36568 = ORIENTED_EDGE ( 'NONE', *, *, #60217, .F. ) ;
#36569 = CARTESIAN_POINT ( 'NONE',  ( 5.731092321990707283, 2.014232586630093191, 0.09613807139101374077 ) ) ;
#36571 = CARTESIAN_POINT ( 'NONE',  ( 4.821169966264648998, -1.840000718094082943, -0.9321929973984711681 ) ) ;
#36570 = CARTESIAN_POINT ( 'NONE',  ( 6.010342169559767633, 5.906487374108181143, -0.7998128361456281477 ) ) ;
#36573 = CARTESIAN_POINT ( 'NONE',  ( 0.000000000000000000, -3.587500000000000355, -4.012584370867899430 ) ) ;
#36572 = CARTESIAN_POINT ( 'NONE',  ( 6.047819040147648373, 9.213483425884394507, 1.199719254218452047 ) ) ;
#36574 = CARTESIAN_POINT ( 'NONE',  ( 5.688527969385528849, 8.794310509995222347, -1.199719254218452047 ) ) ;
#36575 = CARTESIAN_POINT ( 'NONE',  ( -1.642778471875000035, -0.8677083328553769626, -2.845375778867859751 ) ) ;
#36576 = CARTESIAN_POINT ( 'NONE',  ( -0.7500000000000179856, 12.79166666666666607, 1.299038105676658228 ) ) ;
#36577 = CARTESIAN_POINT ( 'NONE',  ( 1.078203232848734094, -2.040033308301641757, -0.4564361842656887713 ) ) ;
#36578 = CARTESIAN_POINT ( 'NONE',  ( 4.518204034511161815, -1.842447959940773705, 0.8197716922626956393 ) ) ;
#36579 = CARTESIAN_POINT ( 'NONE',  ( 4.476008884455379366, -1.787108923542475525, -0.4427587100873929815 ) ) ;
#36580 = CARTESIAN_POINT ( 'NONE',  ( 5.656776405399742025, 7.622658444431597680, -1.599625672291262513 ) ) ;
#36581 = CARTESIAN_POINT ( 'NONE',  ( 0.9204217893557011809, 1.591181625417271039, 0.6660807200309772913 ) ) ;
#36582 = CARTESIAN_POINT ( 'NONE',  ( -2.103486388414573138, 5.605817886458954291, 1.040834085586084257E-14 ) ) ;
#36583 = CARTESIAN_POINT ( 'NONE',  ( 1.319383182065179128, 1.127869332580781148, -2.002907031218110312 ) ) ;
#36584 = CARTESIAN_POINT ( 'NONE',  ( -7.074657228232555717, 7.148188275893099686, 1.040834085586084257E-14 ) ) ;
#36585 = CARTESIAN_POINT ( 'NONE',  ( 1.792605694782311243, -2.251445656634944559, -0.2226877779667023882 ) ) ;
#36586 = CARTESIAN_POINT ( 'NONE',  ( 2.947987317136715468, 0.7576180897185936791, -1.965265766029665295 ) ) ;
#36587 = CARTESIAN_POINT ( 'NONE',  ( -5.646044625448194410, 5.551749915969804938, 0.000000000000000000 ) ) ;
#36588 = CARTESIAN_POINT ( 'NONE',  ( 7.935599982700328958, 8.152621489438862667, 0.7998128361456481317 ) ) ;
#36589 = CARTESIAN_POINT ( 'NONE',  ( 4.706088717274885092, 8.504537580213796133, 0.7216878364870317197 ) ) ;
#36590 = CARTESIAN_POINT ( 'NONE',  ( 6.187500000000010658, -1.451031289060719320, 1.451031289061361473 ) ) ;
#36591 = CARTESIAN_POINT ( 'NONE',  ( -5.819474248763749635, 7.812472595022922128, -1.599625672291256295 ) ) ;
#36592 = CARTESIAN_POINT ( 'NONE',  ( 6.954969613686092345, 7.216478758829655504, -0.7216878364870257245 ) ) ;
#36593 = CARTESIAN_POINT ( 'NONE',  ( 4.170588824514860349, 7.607689953969209995, 0.8569815457360376865 ) ) ;
#36594 = CARTESIAN_POINT ( 'NONE',  ( -4.111146893441842920, 5.819424013814012753, 1.599625672291267398 ) ) ;
#36595 = CARTESIAN_POINT ( 'NONE',  ( 4.676165968894677505, 2.197079021736783044, -0.3272799971512970196 ) ) ;
#36596 = CARTESIAN_POINT ( 'NONE',  ( 2.045129345224237394, -1.761195505111545989, -1.303888621850733509 ) ) ;
#36597 = CARTESIAN_POINT ( 'NONE',  ( -5.063080299699540987, 7.994345218703034384, 1.199719254218464037 ) ) ;
#36598 = CARTESIAN_POINT ( 'NONE',  ( -3.122120512896910505, 6.864500708346841229, 0.7998128361456352531 ) ) ;
#36599 = CARTESIAN_POINT ( 'NONE',  ( 4.949637131784443866, 1.452432516441283905, 1.319008059494260143 ) ) ;
#36600 = CARTESIAN_POINT ( 'NONE',  ( -1.364683531249997417, 2.509375000341422357, 1.214306433183764966E-14 ) ) ;
#36601 = CARTESIAN_POINT ( 'NONE',  ( 6.890000000000044977, 2.990039200936049468, 2.173945303097582382 ) ) ;
#36604 = VERTEX_POINT ( 'NONE', #188638 ) ;
#36603 = CARTESIAN_POINT ( 'NONE',  ( -4.433153041988574294, 8.115836282387899558, 1.040834085586084257E-14 ) ) ;
#36602 = AXIS2_PLACEMENT_3D ( 'NONE', #58859, #90304, #74049 ) ;
#36605 = CARTESIAN_POINT ( 'NONE',  ( 4.201511661969238531, 1.892856375164463367, -0.9562558712687405649 ) ) ;
#36606 = CARTESIAN_POINT ( 'NONE',  ( -5.451787166470911217, 9.374519104275787384, 0.7216878364870267237 ) ) ;
#36607 = EDGE_LOOP ( 'NONE', ( #117413, #46676, #156208, #154426 ) ) ;
#36609 = CARTESIAN_POINT ( 'NONE',  ( 0.000000000000000000, 4.400000000000001243, 0.000000000000000000 ) ) ;
#36608 = CARTESIAN_POINT ( 'NONE',  ( -5.478903473698255588, 7.485416367438324059, -1.443375672974066548 ) ) ;
#36610 = CARTESIAN_POINT ( 'NONE',  ( 5.147291874682557555, 9.156924287104992288, 0.7998128361456462443 ) ) ;
#36611 = CARTESIAN_POINT ( 'NONE',  ( 4.757273854911123756, 1.820453720981948242, -0.2752165127944474210 ) ) ;
#36612 = FILL_AREA_STYLE ('',( #151455 ) ) ;
#36613 = CARTESIAN_POINT ( 'NONE',  ( -0.6823417656250003738, 2.280208333674753174, -1.181850606188749264 ) ) ;
#36614 = CARTESIAN_POINT ( 'NONE',  ( 0.6084659026615606425, -0.2575236531317924293, 1.721126145854386946 ) ) ;
#36615 = CARTESIAN_POINT ( 'NONE',  ( 1.280216254274687104, 3.682822186084150573, 0.4723901200327977890 ) ) ;
#36616 = CARTESIAN_POINT ( 'NONE',  ( 1.364683531249984538, -1.032291666325247714, -0.7879004041258309554 ) ) ;
#36617 = CARTESIAN_POINT ( 'NONE',  ( 5.843201017809841247, 5.919415396974013532, 1.040834085586084257E-14 ) ) ;
#36618 = CARTESIAN_POINT ( 'NONE',  ( 5.436455051933180016, 2.129025116502227810, 0.3735886874452337691 ) ) ;
#36619 = CARTESIAN_POINT ( 'NONE',  ( -4.298098390732130625, 4.973201863064262263, 1.199719254218462483 ) ) ;
#36620 = STYLED_ITEM ( 'NONE', ( #183053 ), #7322 ) ;
#36621 = CARTESIAN_POINT ( 'NONE',  ( -7.714226216051410567, 9.062647342557177410, 1.082531754730558626 ) ) ;
#36622 = AXIS2_PLACEMENT_3D ( 'NONE', #37589, #203266, #151352 ) ;
#36623 = CARTESIAN_POINT ( 'NONE',  ( 5.120075222393803749, -1.153228217640640985, -1.828211184805514922 ) ) ;
#36624 = CARTESIAN_POINT ( 'NONE',  ( -0.6823417656249969321, 3.467708333674754506, -1.181850606188749264 ) ) ;
#36625 = CARTESIAN_POINT ( 'NONE',  ( 5.167239647397361857, 0.1962102620695851674, -1.961592271633934903 ) ) ;
#36626 = CARTESIAN_POINT ( 'NONE',  ( 3.866272716362227690, -0.5049011280162157833, 1.658656615756588959 ) ) ;
#36627 = CARTESIAN_POINT ( 'NONE',  ( 0.9607770615731696662, -1.983481723135366304, -0.9323335341336475013 ) ) ;
#36628 = CARTESIAN_POINT ( 'NONE',  ( 2.503307172793560298, 1.853534942699623045, -1.374368423928104876 ) ) ;
#36629 = CARTESIAN_POINT ( 'NONE',  ( 5.184866321732980232, -0.2479502356789231865, -2.045719655484798949 ) ) ;
#36630 = CARTESIAN_POINT ( 'NONE',  ( 6.269086997039995168, 1.857158234874217939, -0.5679118324898363435 ) ) ;
#36631 = CARTESIAN_POINT ( 'NONE',  ( -6.792271770322117597, 9.907772251142352715, 1.082531754730549967 ) ) ;
#36632 = VECTOR ( 'NONE', #85863, 1000.000000000000000 ) ;
#36633 = CARTESIAN_POINT ( 'NONE',  ( -4.793689830883590020, 7.750332681742931662, 1.199719254218452935 ) ) ;
#36634 = CARTESIAN_POINT ( 'NONE',  ( -11.86145016429273724, 13.50587408513255738, -1.100000000000002531 ) ) ;
#36635 = EDGE_CURVE ( 'NONE', #65489, #108697, #146700, .T. ) ;
#36636 = DIRECTION ( 'NONE',  ( -0.000000000000000000, -1.000000000000000000, -0.000000000000000000 ) ) ;
#36637 = CARTESIAN_POINT ( 'NONE',  ( -7.199016378732087773, 7.501199984716642177, 0.7216878364870317197 ) ) ;
#36638 = CARTESIAN_POINT ( 'NONE',  ( 3.346891443098894303, 0.5343612633194516626, 2.140983517310310891 ) ) ;
#36639 = CARTESIAN_POINT ( 'NONE',  ( 0.000000000000000000, -2.034374999522043481, -3.793834371823813001 ) ) ;
#36640 = CARTESIAN_POINT ( 'NONE',  ( 0.4087542164426588021, -1.499397391050528050, 1.102066480322369202 ) ) ;
#36641 = CARTESIAN_POINT ( 'NONE',  ( -6.042630808230841359E-15, -1.968749999044084875, 3.474999999999999645 ) ) ;
#36642 = LINE ( 'NONE', #49702, #55864 ) ;
#36643 = CARTESIAN_POINT ( 'NONE',  ( -9.579665964948885559, -7.473374494045003757, 1.020505294851981049E-14 ) ) ;
#36645 = CARTESIAN_POINT ( 'NONE',  ( 6.925078400183521943, 1.220207665023531174, 2.355644635573426182 ) ) ;
#36644 = CARTESIAN_POINT ( 'NONE',  ( -4.905272163827030241, 8.130510659208837865, -1.040677472382423474 ) ) ;
#36646 = CARTESIAN_POINT ( 'NONE',  ( 11.94105721237523277, 13.40000000000000036, 1.187919463087248273 ) ) ;
#36647 = VERTEX_POINT ( 'NONE', #174555 ) ;
#36648 = CARTESIAN_POINT ( 'NONE',  ( 2.834896919975951057, 0.2507222237850720847, 2.045500233692464587 ) ) ;
#36649 = CARTESIAN_POINT ( 'NONE',  ( 1.360316468749983576, 1.515625000341386253, -4.163336342344337027E-14 ) ) ;
#36650 = CARTESIAN_POINT ( 'NONE',  ( -6.718228810771495141, 7.796687353110217877, 1.199719254218450271 ) ) ;
#36651 = CARTESIAN_POINT ( 'NONE',  ( 2.613930769413209898, -0.6315753767559011411, 1.918467498408537919 ) ) ;
#36652 = CARTESIAN_POINT ( 'NONE',  ( -1.500000000000013101, -0.07916666666664513852, 0.8660254037844403729 ) ) ;
#36653 = CARTESIAN_POINT ( 'NONE',  ( 2.984766373302843778, 6.633977868828633717, -0.7998128361456291469 ) ) ;
#36654 = CARTESIAN_POINT ( 'NONE',  ( 1.727488365587977359, -1.940856233752264348, 0.6934696639643816996 ) ) ;
#36655 = ADVANCED_FACE ( 'NONE', ( #42421 ), #125864, .F. ) ;
#36657 = CARTESIAN_POINT ( 'NONE',  ( -1.402160292154681736E-14, 12.67187500034139802, 1.575800808251682339 ) ) ;
#36656 = CARTESIAN_POINT ( 'NONE',  ( -1.607015867998815128, 0.9165151389911810886, 1.199999999999999734 ) ) ;
#36658 = CARTESIAN_POINT ( 'NONE',  ( 7.494959990256193194, 7.638541498254023843, -0.7998128361456281477 ) ) ;
#36659 = CARTESIAN_POINT ( 'NONE',  ( 5.339680242214618566, 4.685059543140487115, 2.440369273555429874 ) ) ;
#36660 = CARTESIAN_POINT ( 'NONE',  ( 5.303435803989668074, 1.802500012205746183, 1.273053691228965389 ) ) ;
#36661 = CARTESIAN_POINT ( 'NONE',  ( 1.054251131370760319, 2.159144779032458050, -0.1049546803274861440 ) ) ;
#36662 = CARTESIAN_POINT ( 'NONE',  ( -5.016153647376219382, 6.875265226737464985, 1.443375672974064550 ) ) ;
#36663 = CARTESIAN_POINT ( 'NONE',  ( 0.3742329010679063539, -2.001858617179689492, -0.2420261300371470137 ) ) ;
#36664 = DIRECTION ( 'NONE',  ( 1.000000000000000000, 0.000000000000000000, -3.706092522800016599E-15 ) ) ;
#36665 = CARTESIAN_POINT ( 'NONE',  ( 1.499999999999993117, 12.13541666734946212, 0.8660254037844408170 ) ) ;
#36666 = CARTESIAN_POINT ( 'NONE',  ( -15.75000000000000000, 10.90000000000000036, 0.6999999999999992895 ) ) ;
#36667 = CARTESIAN_POINT ( 'NONE',  ( 1.744777856283234785, -1.581906188472384400, 0.9981555316627908070 ) ) ;
#36668 = CARTESIAN_POINT ( 'NONE',  ( 3.678922940808615483, 1.700962499606586853, -1.082838980105811366 ) ) ;
#36670 = CARTESIAN_POINT ( 'NONE',  ( 11.49966000274946509, 13.74232845564725558, 3.429881629453341851 ) ) ;
#36669 = CARTESIAN_POINT ( 'NONE',  ( 0.6823417656249882723, 1.426041667008083547, -1.181850606188749264 ) ) ;
#36672 = CARTESIAN_POINT ( 'NONE',  ( 4.705754021700633949, -0.5625300431781330435, 2.029483779808038957 ) ) ;
#36671 = CARTESIAN_POINT ( 'NONE',  ( -7.365103760721662951, 9.615707025640515937, 1.599625672291295375 ) ) ;
#36673 = EDGE_CURVE ( 'NONE', #94599, #172216, #169168, .T. ) ;
#36674 = CARTESIAN_POINT ( 'NONE',  ( 8.145751363712157911, 8.397798100619326078, -0.7998128361456281477 ) ) ;
#36676 = CARTESIAN_POINT ( 'NONE',  ( -7.446452682403657874, 9.710614100936176385, -1.599625672291263179 ) ) ;
#36675 = CARTESIAN_POINT ( 'NONE',  ( 5.923986774528332333, 5.876015756563318426, -0.7998128361456481317 ) ) ;
#36677 = CARTESIAN_POINT ( 'NONE',  ( -0.3561222683123435040, -6.532648913095006726, -9.473215147174805395 ) ) ;
#36678 = CARTESIAN_POINT ( 'NONE',  ( 4.799084794409138155, -0.2512425647771680537, -2.004053532012660455 ) ) ;
#36679 = CARTESIAN_POINT ( 'NONE',  ( -0.6823417656250212460, 5.551041667008087543, 1.181850606188767472 ) ) ;
#36680 = ADVANCED_FACE ( 'NONE', ( #156158 ), #101098, .T. ) ;
#36681 = CARTESIAN_POINT ( 'NONE',  ( 0.9892170606862679128, 0.1480104381128030111, 2.057284718974061288 ) ) ;
#36682 = CARTESIAN_POINT ( 'NONE',  ( 7.565086526745395723, 10.80938946696957004, -1.082531754730543083 ) ) ;
#36683 = CARTESIAN_POINT ( 'NONE',  ( 6.008198349511364000, 7.038594824965278995, 1.199719254218453823 ) ) ;
#36684 = CARTESIAN_POINT ( 'NONE',  ( -1.364683531250014514, -0.6989583329919100141, -0.7879004041258359514 ) ) ;
#36686 = CARTESIAN_POINT ( 'NONE',  ( -7.721398836998378812, -6.134628647623499909, 7.721398836998403681 ) ) ;
#36685 = CARTESIAN_POINT ( 'NONE',  ( 4.030516805012513082, 7.924296382481737844, 0.000000000000000000 ) ) ;
#36687 = CARTESIAN_POINT ( 'NONE',  ( 6.087247782411444597, 10.04561347954795281, -0.7216878364870267237 ) ) ;
#36689 = CARTESIAN_POINT ( 'NONE',  ( 1.734723475976807094E-15, 15.00041888085534758, 12.17999951260719982 ) ) ;
#36688 = CARTESIAN_POINT ( 'NONE',  ( 2.963510081828163223, 1.832883945819727689, 1.163594247970006990 ) ) ;
#36691 = CARTESIAN_POINT ( 'NONE',  ( 2.190726087351921425, 1.424366561657765207, 1.166803476217087576 ) ) ;
#36690 = CARTESIAN_POINT ( 'NONE',  ( -3.619663825168619731, 7.166765529431275539, 1.040834085586084257E-14 ) ) ;
#36692 = COLOUR_RGB ( '', 0.72549020, 0.75294118, 0.79215686) ;
#36693 = CARTESIAN_POINT ( 'NONE',  ( -1.364683531249997417, 3.759375000341423689, 1.214306433183764966E-14 ) ) ;
#36694 = CARTESIAN_POINT ( 'NONE',  ( 4.722331747100577459, 2.097238624054961864, 0.6360808509995665716 ) ) ;
#36695 = CARTESIAN_POINT ( 'NONE',  ( 6.883263157960404222, 4.689511904294953126, 2.716359706997414136 ) ) ;
#36696 = CARTESIAN_POINT ( 'NONE',  ( 5.243177039506740300, -1.943355607328334678, 1.158386780943015504 ) ) ;
#36697 = CARTESIAN_POINT ( 'NONE',  ( -5.799137018343247796, 7.788745826199009237, -1.599625672291256295 ) ) ;
#36698 = DIRECTION ( 'NONE',  ( -0.3502638921866460531, 1.953969548649011466E-16, -0.9366510587354619499 ) ) ;
#36699 = CARTESIAN_POINT ( 'NONE',  ( 4.641544345285703699, 8.432478572106539616, -0.4375188090333537727 ) ) ;
#36700 = CARTESIAN_POINT ( 'NONE',  ( -0.7500000000000006661, 14.20833333333333748, -1.299038105676657340 ) ) ;
#36701 = CARTESIAN_POINT ( 'NONE',  ( -5.356880090730904875, 7.343055753976412525, 1.443375672974058777 ) ) ;
#36702 = CARTESIAN_POINT ( 'NONE',  ( 4.529832720741620022, 7.338536369956936589, -1.082531754730548412 ) ) ;
#36703 = CARTESIAN_POINT ( 'NONE',  ( 5.360532716240259177, -1.281408969121943464, 1.220901466008792235 ) ) ;
#36704 = CARTESIAN_POINT ( 'NONE',  ( 7.820355676984174664, 8.018169799436671852, -0.7998128361456281477 ) ) ;
#36705 = CARTESIAN_POINT ( 'NONE',  ( 2.169099057653073093, -1.925109178590768799, -0.8542606987168609445 ) ) ;
#36707 = CARTESIAN_POINT ( 'NONE',  ( 1.499999999999989120, 3.004166666666689522, 0.8660254037844524744 ) ) ;
#36706 = CARTESIAN_POINT ( 'NONE',  ( 0.6823417656249934904, 11.44270833367473728, 1.181850606188764807 ) ) ;
#36708 = CARTESIAN_POINT ( 'NONE',  ( 2.558991062574625275, 1.583523548174452733, -1.170949712736363502 ) ) ;
#36709 = CARTESIAN_POINT ( 'NONE',  ( 1.094370286708164386, -0.4508366001288487412, -1.815394955969009239 ) ) ;
#36710 = CARTESIAN_POINT ( 'NONE',  ( 0.1683002474503410839, -0.8351952195557797998, -1.773497582445908938 ) ) ;
#36712 = ORIENTED_EDGE ( 'NONE', *, *, #189945, .F. ) ;
#36711 = CARTESIAN_POINT ( 'NONE',  ( 5.924035771748266122, -1.796794102754266431, 0.2306889152782486963 ) ) ;
#36713 = CARTESIAN_POINT ( 'NONE',  ( 5.829642864196162400, 7.824335979694092558, 1.443375672974062551 ) ) ;
#36714 = CARTESIAN_POINT ( 'NONE',  ( 1.364683531249986537, -0.2822916663252520997, -0.7879004041258309554 ) ) ;
#36716 = CARTESIAN_POINT ( 'NONE',  ( 5.524238439434661530, 1.113281918156138639, -1.503147240406087271 ) ) ;
#36715 = CIRCLE ( 'NONE', #5611, 0.08000000000000004330 ) ;
#36717 = CARTESIAN_POINT ( 'NONE',  ( 8.530051201292206287, 13.10347683481629488, 0.000000000000000000 ) ) ;
#36718 = CARTESIAN_POINT ( 'NONE',  ( 5.858279169847476098, -2.070434559870216074, -0.005763162253501210100 ) ) ;
#36719 = DIRECTION ( 'NONE',  ( 0.000000000000000000, -1.000000000000000000, 0.000000000000000000 ) ) ;
#36720 = CARTESIAN_POINT ( 'NONE',  ( -6.441532379824190357, 6.687744995982559892, 0.7216878364870257245 ) ) ;
#36722 = CARTESIAN_POINT ( 'NONE',  ( -1.402160292154681736E-14, 1.087500000000024336, -1.732050807568863648 ) ) ;
#36721 = CIRCLE ( 'NONE', #157818, 12.00000000000000178 ) ;
#36723 = CARTESIAN_POINT ( 'NONE',  ( 7.076466111328892694, 10.34329533227067799, -1.199719254218441611 ) ) ;
#36724 = CARTESIAN_POINT ( 'NONE',  ( -8.341290820905609138, 10.75459192918846618, 1.599625672291269396 ) ) ;
#36725 = CARTESIAN_POINT ( 'NONE',  ( 6.703580607314123085, 6.785541894813420072, 0.000000000000000000 ) ) ;
#36726 = CARTESIAN_POINT ( 'NONE',  ( 1.364683531249986537, 0.1135416670080857532, 0.7879004041258500513 ) ) ;
#36727 = CARTESIAN_POINT ( 'NONE',  ( 0.7499999999999885647, 0.5666666666666875241, -1.299038105676652899 ) ) ;
#36729 = CARTESIAN_POINT ( 'NONE',  ( 5.522248639467795428, 5.337044922334209573, -0.7998128361456231517 ) ) ;
#36728 = CARTESIAN_POINT ( 'NONE',  ( 4.861744986159981075, -0.5251177144562025889, 1.890194517805739771 ) ) ;
#36730 = CARTESIAN_POINT ( 'NONE',  ( 3.479842141819572188, 1.821463063354014533, 0.8645922719773958542 ) ) ;
#36731 = CARTESIAN_POINT ( 'NONE',  ( 3.010844082872287331, 0.05196181304293297915, 1.915202476457795511 ) ) ;
#36732 = CARTESIAN_POINT ( 'NONE',  ( 0.07999999999998980149, -6.134628647623513231, -10.91970695577493977 ) ) ;
#36733 = CARTESIAN_POINT ( 'NONE',  ( 0.2225716830646235489, 2.098996182288978218, 0.6302611576235670476 ) ) ;
#36734 =( BOUNDED_SURFACE ( )  B_SPLINE_SURFACE ( 3, 2, ( 
 ( #125879, #128025, #157240 ),
 ( #74912, #45627, #177750 ),
 ( #195056, #207029, #58658 ),
 ( #124811, #108541, #30438 ),
 ( #34672, #97579, #84493 ),
 ( #32552, #98628, #48816 ),
 ( #134353, #132224, #164689 ),
 ( #16273, #166824, #113886 ) ),
 .UNSPECIFIED., .F., .F., .T. ) 
 B_SPLINE_SURFACE_WITH_KNOTS ( ( 4, 2, 2, 4 ),
 ( 3, 3 ),
 ( 0.000000000000000000, 0.0005109843281227146802, 0.0007664764921840720203, 0.001021968656245429360 ),
 ( 0.000000000000000000, 1.000000000000000000 ),
 .UNSPECIFIED. ) 
 GEOMETRIC_REPRESENTATION_ITEM ( )  RATIONAL_B_SPLINE_SURFACE ( (
 ( 1.000000000000000000, 0.7045118851637687252, 1.000000000000000000),
 ( 1.000000000000000000, 0.6478559580219998004, 1.000000000000000000),
 ( 1.000000000000000000, 0.5832506164449653419, 1.000000000000000000),
 ( 1.000000000000000000, 0.4879709628488582140, 1.000000000000000000),
 ( 1.000000000000000000, 0.4561823831828598630, 1.000000000000000000),
 ( 1.000000000000000000, 0.4039565156453471806, 1.000000000000000000),
 ( 1.000000000000000000, 0.3848936348732069912, 1.000000000000000000),
 ( 1.000000000000000000, 0.3826834323650904479, 1.000000000000000000) ) ) 
 REPRESENTATION_ITEM ( '' )  SURFACE ( )  );
#36735 = CARTESIAN_POINT ( 'NONE',  ( 0.2331713839410941569, 0.7381306520543399197, -2.038767774274966360 ) ) ;
#36736 = CARTESIAN_POINT ( 'NONE',  ( 2.583089905966722277, 1.711919019956799737, -0.7542334906679578621 ) ) ;
#36737 = CARTESIAN_POINT ( 'NONE',  ( -1.500000000000015099, -0.3395833326505143801, -0.8660254037844383745 ) ) ;
#36738 = CARTESIAN_POINT ( 'NONE',  ( 3.832292871861494810, -1.038684978035837592, -1.724458057284683710 ) ) ;
#36739 = CARTESIAN_POINT ( 'NONE',  ( -7.751511138711140170, 10.06651563329490529, -1.599625672291263179 ) ) ;
#36741 = CARTESIAN_POINT ( 'NONE',  ( 4.411780756640943046, -1.303739072956756617, -1.668109288273095014 ) ) ;
#36740 = CARTESIAN_POINT ( 'NONE',  ( -5.314433026876900001, 6.262888621853549331, 1.082531754730548412 ) ) ;
#36742 = DIRECTION ( 'NONE',  ( 7.387867266669436732E-31, -1.000000000000000000, -8.546850786086424434E-32 ) ) ;
#36743 = CARTESIAN_POINT ( 'NONE',  ( 5.635237798060349412, -0.04710594754482424346, -2.069988403558701062 ) ) ;
#36745 = CARTESIAN_POINT ( 'NONE',  ( 6.720655732516641834, 2.402268298795938950, 2.653651172607660591 ) ) ;
#36744 = CARTESIAN_POINT ( 'NONE',  ( 1.663735998746267652, 1.077533827470295913, 1.791552697131219229 ) ) ;
#36747 = ORIENTED_EDGE ( 'NONE', *, *, #49562, .T. ) ;
#36746 = CARTESIAN_POINT ( 'NONE',  ( 6.334959139596201716, 0.1821375521317940283, 1.816452708017932238 ) ) ;
#36748 = CARTESIAN_POINT ( 'NONE',  ( 7.670162217029129259, 9.971608557999250166, 1.599625672291281386 ) ) ;
#36749 = CARTESIAN_POINT ( 'NONE',  ( 9.427850895902817996, 13.54474674066948481, 7.423989997610750180 ) ) ;
#36750 = CARTESIAN_POINT ( 'NONE',  ( -0.07933194154489606187, -9.900000000000005684, -9.499668754385620417 ) ) ;
#36751 = CARTESIAN_POINT ( 'NONE',  ( -9.811677024507259759, 4.107325997343203028, 6.339424533126782002 ) ) ;
#36752 = CARTESIAN_POINT ( 'NONE',  ( 6.656690234185433042, 7.828855363713562276, -1.082531754730543971 ) ) ;
#36753 = CARTESIAN_POINT ( 'NONE',  ( 5.495418255317095380, 6.026204583819558813, -0.7979391942483996525 ) ) ;
#36755 = CARTESIAN_POINT ( 'NONE',  ( 0.6272531361488179469, -0.2670696439982013781, 1.791522762418327419 ) ) ;
#36754 = CARTESIAN_POINT ( 'NONE',  ( 8.005163354226054295, 8.304055099544019214, 0.000000000000000000 ) ) ;
#36757 = CARTESIAN_POINT ( 'NONE',  ( -7.832860060393135093, 10.16142270859057462, 1.599625672291295375 ) ) ;
#36756 = CIRCLE ( 'NONE', #67810, 0.5000000000000013323 ) ;
#36758 = CARTESIAN_POINT ( 'NONE',  ( 4.493637847925535667, 7.329995691633395261, -1.199719254218452047 ) ) ;
#36759 = CARTESIAN_POINT ( 'NONE',  ( 0.4694063952341813728, -6.893137084989856334, 10.98997987423603995 ) ) ;
#36760 = CARTESIAN_POINT ( 'NONE',  ( 4.050410598061423784, 7.525715715152009544, -0.4746587800704554772 ) ) ;
#36761 = CARTESIAN_POINT ( 'NONE',  ( 3.440018289565364817, 5.036440642624797626, 1.599625672291267398 ) ) ;
#36762 = ORIENTED_EDGE ( 'NONE', *, *, #151886, .T. ) ;
#36763 =( GEOMETRIC_REPRESENTATION_CONTEXT ( 3 ) GLOBAL_UNCERTAINTY_ASSIGNED_CONTEXT ( ( #206865 ) ) GLOBAL_UNIT_ASSIGNED_CONTEXT ( ( #5118, #123279, #104810 ) ) REPRESENTATION_CONTEXT ( 'NONE', 'WORKASPACE' ) );
#36764 = CARTESIAN_POINT ( 'NONE',  ( 6.468375372808552903, -1.978050569928070379, -0.3905794195708453542 ) ) ;
#36765 = CARTESIAN_POINT ( 'NONE',  ( 0.4520119014386895229, -1.502510013782244025, -1.496567369470555020 ) ) ;
#36766 = CARTESIAN_POINT ( 'NONE',  ( -3.003428079110303184, 6.384049572106303749, -0.7531072163598397928 ) ) ;
#36767 = CARTESIAN_POINT ( 'NONE',  ( 0.1405533004714253908, 5.720147882271004569, -2.873730252010114228 ) ) ;
#36768 = DIRECTION ( 'NONE',  ( 1.000000000000000000, -7.771561172376096769E-16, -4.440892098500627148E-16 ) ) ;
#36769 = CARTESIAN_POINT ( 'NONE',  ( -3.606105671554953318, 7.150947683548662503, 0.7216878364870317197 ) ) ;
#36770 = CARTESIAN_POINT ( 'NONE',  ( 9.137832345930652522, 10.72352116074969075, -1.082531754730543083 ) ) ;
#36771 = CARTESIAN_POINT ( 'NONE',  ( 4.047672669870348905, 1.423397643995693684, 1.361350234347382226 ) ) ;
#36772 = CARTESIAN_POINT ( 'NONE',  ( 5.079703922733037835, -0.7231256174668048153, 1.882480835741196845 ) ) ;
#36773 = CARTESIAN_POINT ( 'NONE',  ( -7.152089726408780379, 8.302858421353754181, -1.199719254218446718 ) ) ;
#36774 = DIRECTION ( 'NONE',  ( 0.000000000000000000, -1.000000000000000000, 0.000000000000000000 ) ) ;
#36775 = CARTESIAN_POINT ( 'NONE',  ( -10.91804383151481339, -8.407420853759283830, 0.1905751639681794174 ) ) ;
#36776 = AXIS2_PLACEMENT_3D ( 'NONE', #123488, #204609, #141818 ) ;
#36777 = CARTESIAN_POINT ( 'NONE',  ( 4.980524279605372584, -0.2661484459187679064, -2.175167798947100994 ) ) ;
#36778 = CARTESIAN_POINT ( 'NONE',  ( 3.592722855893375478, -0.3746021097269113809, -1.889456300395859989 ) ) ;
#36779 = CARTESIAN_POINT ( 'NONE',  ( -8.179646747746328828, 8.437342715325849341, -0.7998128361456291469 ) ) ;
#36780 = CARTESIAN_POINT ( 'NONE',  ( -0.02968770228140015649, 0.7448490463385792903, -1.910291535987144629 ) ) ;
#36781 = DIRECTION ( 'NONE',  ( 0.000000000000000000, -1.000000000000000000, -9.023263958591317418E-17 ) ) ;
#36782 = EDGE_CURVE ( 'NONE', #81332, #111937, #190929, .T. ) ;
#36783 = CYLINDRICAL_SURFACE ( 'NONE', #151542, 11.49999999999998934 ) ;
#36784 = ORIENTED_EDGE ( 'NONE', *, *, #204783, .T. ) ;
#36785 = CARTESIAN_POINT ( 'NONE',  ( 3.879041347285658414, 6.579279767591636130, -1.082531754730548412 ) ) ;
#36786 = CARTESIAN_POINT ( 'NONE',  ( 5.664895447484411761, 1.493751497301420761, -1.283663174101207005 ) ) ;
#36788 = CARTESIAN_POINT ( 'NONE',  ( 4.371743676962040581, 0.4387793907001916738, -1.964547544987900851 ) ) ;
#36787 = CARTESIAN_POINT ( 'NONE',  ( 0.1869208759678643028, 1.439853572182720587, 1.303434232916983015 ) ) ;
#36789 = CARTESIAN_POINT ( 'NONE',  ( 5.026898302747025760, 2.274369689431681163, -0.3307130315356506256 ) ) ;
#36791 = CARTESIAN_POINT ( 'NONE',  ( 4.240933880512650411, -0.1787712432332102808, -1.852300418306342955 ) ) ;
#36790 = CARTESIAN_POINT ( 'NONE',  ( 11.89829993707161471, 11.32919228251124366, 1.561606677374347329 ) ) ;
#36792 = CARTESIAN_POINT ( 'NONE',  ( 5.840530312436913007, 10.03597880781023299, 0.000000000000000000 ) ) ;
#36793 = CYLINDRICAL_SURFACE ( 'NONE', #57058, 1.500000000000000222 ) ;
#36794 = DIRECTION ( 'NONE',  ( 0.000000000000000000, -1.000000000000000000, 0.000000000000000000 ) ) ;
#36795 = CARTESIAN_POINT ( 'NONE',  ( -5.845536785786364931, 9.971543350059432598, 0.000000000000000000 ) ) ;
#36796 = CARTESIAN_POINT ( 'NONE',  ( -3.298413662870199659, -0.9801510035281409960, 1.084536036895182187 ) ) ;
#36797 = CARTESIAN_POINT ( 'NONE',  ( 0.8025787753177977546, 1.655945718051672566, -1.435626523826734280 ) ) ;
#36798 = CARTESIAN_POINT ( 'NONE',  ( 6.019457014787495730, 6.125047393447951016, -0.7216878364870257245 ) ) ;
#36799 = ORIENTED_EDGE ( 'NONE', *, *, #156430, .T. ) ;
#36800 = EDGE_CURVE ( 'NONE', #81951, #45069, #5556, .T. ) ;
#36801 = CARTESIAN_POINT ( 'NONE',  ( -3.122962944146551845, 6.587281168238894757, 0.4581612399161954507 ) ) ;
#36802 = LINE ( 'NONE', #101814, #200108 ) ;
#36803 = CARTESIAN_POINT ( 'NONE',  ( 0.3459771380207553593, 1.820543102168985961, 0.1377627428671979182 ) ) ;
#36804 = CARTESIAN_POINT ( 'NONE',  ( -5.434120640978981065, 5.234228924097238611, -0.7998128361456221525 ) ) ;
#36805 = CARTESIAN_POINT ( 'NONE',  ( 2.637049607583162203, 0.5866705090989009497, 1.632017879250416525 ) ) ;
#36806 = CARTESIAN_POINT ( 'NONE',  ( -11.04986227068298277, 9.990600021556637955, -1.056429153205399984 ) ) ;
#36807 = CARTESIAN_POINT ( 'NONE',  ( 1.734723475976807094E-15, 1.000000000000000888, 3.150000000000001243 ) ) ;
#36808 = CARTESIAN_POINT ( 'NONE',  ( 5.619710272201024814, -1.780234218580947436, 0.4041525643716862848 ) ) ;
#36809 = CARTESIAN_POINT ( 'NONE',  ( 3.467582345443523728, -0.3871886708083654427, 1.922995549214156608 ) ) ;
#36810 = ADVANCED_FACE ( 'NONE', ( #209134 ), #99911, .T. ) ;
#36811 = CARTESIAN_POINT ( 'NONE',  ( -3.355169270512988773E-14, -0.4999999993171823642, -1.414508159514593411 ) ) ;
#36812 = CARTESIAN_POINT ( 'NONE',  ( -9.016335848287868160, 10.47781223021269170, 1.199719254218462483 ) ) ;
#36813 = CARTESIAN_POINT ( 'NONE',  ( 7.396136491454752715, 8.587579647240744407, 1.199719254218462483 ) ) ;
#36814 = CARTESIAN_POINT ( 'NONE',  ( 4.424552244980545446, -0.9075887007226298708, -1.916591080935086788 ) ) ;
#36815 = CARTESIAN_POINT ( 'NONE',  ( 7.679767667498067496, 7.924426798361372093, 0.000000000000000000 ) ) ;
#36816 = EDGE_CURVE ( 'NONE', #142253, #204026, #164684, .T. ) ;
#36817 = CARTESIAN_POINT ( 'NONE',  ( -10.47097470845587175, 11.11055866948701443, 1.040834085586084257E-14 ) ) ;
#36818 = CARTESIAN_POINT ( 'NONE',  ( 2.940353189855488658, -1.068159618217549234, 1.773299548953041871 ) ) ;
#36820 = CARTESIAN_POINT ( 'NONE',  ( -0.6823417656250003738, 0.03020833367475134201, -1.181850606188749264 ) ) ;
#36819 = SURFACE_STYLE_FILL_AREA ( #3236 ) ;
#36822 = VERTEX_POINT ( 'NONE', #31487 ) ;
#36821 = CARTESIAN_POINT ( 'NONE',  ( 4.231244787023562992, 2.030907777374240997, 0.9001406952713184584 ) ) ;
#36823 = CARTESIAN_POINT ( 'NONE',  ( 3.129784643070336436, 0.5604733119842463251, 2.229205935122404725 ) ) ;
#36824 = CARTESIAN_POINT ( 'NONE',  ( 8.948018195339340508, 9.541702104091804415, -0.7216878364870197293 ) ) ;
#36826 = CARTESIAN_POINT ( 'NONE',  ( 1.642778471875000035, -1.626041666188710044, -2.845375778867859751 ) ) ;
#36825 = CARTESIAN_POINT ( 'NONE',  ( 6.048345925472166762, 10.07050432311064903, 0.7216878364870317197 ) ) ;
#36827 = SURFACE_STYLE_FILL_AREA ( #148475 ) ;
#36828 = CARTESIAN_POINT ( 'NONE',  ( 10.95308175811721085, 13.79999999999998295, 1.799999999999999600 ) ) ;
#36829 = DIRECTION ( 'NONE',  ( -0.000000000000000000, -1.000000000000000000, -0.000000000000000000 ) ) ;
#36830 = CARTESIAN_POINT ( 'NONE',  ( 2.830216799141628492, -0.9462872844297947061, -1.661813493071498726 ) ) ;
#36831 = CARTESIAN_POINT ( 'NONE',  ( -11.84668730067608600, 13.40000000000000036, -1.400000000000001910 ) ) ;
#36832 = CARTESIAN_POINT ( 'NONE',  ( 4.559404828610894356, 0.3762245950137115269, -1.683048502377647804 ) ) ;
#36833 = CARTESIAN_POINT ( 'NONE',  ( 3.819546216251490822, -1.394084564108012403, -1.457236891723237449 ) ) ;
#36834 = CARTESIAN_POINT ( 'NONE',  ( 3.868082235913085309, -0.2263641512248204812, -2.287543476887623051 ) ) ;
#36835 = DIRECTION ( 'NONE',  ( 0.6507913734559640506, -0.7592566023653004592, 0.000000000000000000 ) ) ;
#36836 = CARTESIAN_POINT ( 'NONE',  ( 0.1533209562146371774, -1.769702838771534559, 1.318327933512997152 ) ) ;
#36837 = CARTESIAN_POINT ( 'NONE',  ( -5.424670859243583720, 8.382514198209223721, 1.082531754730550855 ) ) ;
#36838 = ORIENTED_EDGE ( 'NONE', *, *, #144102, .F. ) ;
#36839 = CARTESIAN_POINT ( 'NONE',  ( 4.481574309046215454, 1.155277477370730832, 1.340746495013745543 ) ) ;
#36841 = CARTESIAN_POINT ( 'NONE',  ( 0.6566820891428931661, -1.656472902050255991, 1.584714856167362074 ) ) ;
#36840 = CARTESIAN_POINT ( 'NONE',  ( 7.862802741282558294, 8.137967717776607657, 0.000000000000000000 ) ) ;
#36842 = CARTESIAN_POINT ( 'NONE',  ( 0.3393031230796061948, 1.735299727462248587, 0.1329522994921657764 ) ) ;
#36843 = CARTESIAN_POINT ( 'NONE',  ( -3.216308754939891212, 4.775446185561722956, -1.599625672291262513 ) ) ;
#36844 = CARTESIAN_POINT ( 'NONE',  ( 5.736325210887869730, 0.4244523575273988492, 2.149783713274712404 ) ) ;
#36845 = CARTESIAN_POINT ( 'NONE',  ( -4.004454267989906668, 5.765225627445230927, 1.599625672291270506 ) ) ;
#36846 = CARTESIAN_POINT ( 'NONE',  ( -1.360316468750024876, -1.057291666325259172, 0.7853790794158601596 ) ) ;
#36847 = CARTESIAN_POINT ( 'NONE',  ( 6.966220764712121927, 6.002124920821316323, 2.420000000000000373 ) ) ;
#36848 = CARTESIAN_POINT ( 'NONE',  ( 0.2214384409217939054, -1.939739064610836339, -0.9756505802681545436 ) ) ;
#36849 = CARTESIAN_POINT ( 'NONE',  ( 0.8312679839070147292, -1.592664559859976237, -1.236796411087807801 ) ) ;
#36850 = CARTESIAN_POINT ( 'NONE',  ( 1.499999999999987566, -0.6937499993171849511, 0.000000000000000000 ) ) ;
#36851 = CARTESIAN_POINT ( 'NONE',  ( 4.811117629317255506, 1.676929503210132122, 0.9481960042460689797 ) ) ;
#36852 = CARTESIAN_POINT ( 'NONE',  ( 1.364683531249997417, 12.23437500034139980, 2.602085213965210642E-15 ) ) ;
#36853 = CARTESIAN_POINT ( 'NONE',  ( 0.7212869692094016072, 1.677245448433011710, -1.456619292340176841 ) ) ;
#36855 = ORIENTED_EDGE ( 'NONE', *, *, #131734, .F. ) ;
#36854 = FACE_OUTER_BOUND ( 'NONE', #144248, .T. ) ;
#36857 = CARTESIAN_POINT ( 'NONE',  ( -1.257518954445032477, 3.216479010054028809, 0.7750000000000100142 ) ) ;
#36856 = PLANE ( 'NONE',  #95737 ) ;
#36858 = DIRECTION ( 'NONE',  ( -0.6507913734559641616, -0.7592566023653004592, 0.000000000000000000 ) ) ;
#36859 = CARTESIAN_POINT ( 'NONE',  ( 4.864678189204997949, 4.569879397027603929, 0.7998128361456341429 ) ) ;
#36860 = CARTESIAN_POINT ( 'NONE',  ( -3.474999999999997868, -2.420833333333334725, 2.006292185433951047 ) ) ;
#36861 = CARTESIAN_POINT ( 'NONE',  ( -15.75000000000000000, 13.40000000000000036, 0.6999999999999992895 ) ) ;
#36862 = CARTESIAN_POINT ( 'NONE',  ( 4.423245670630183923, -1.075405338609165318, -1.368339626032973211 ) ) ;
#36863 = CARTESIAN_POINT ( 'NONE',  ( 2.734756269166933151, -1.876540383875524576, -0.5722209215143353456 ) ) ;
#36865 = CARTESIAN_POINT ( 'NONE',  ( -0.6823417656250003738, 2.780208333674753618, -1.181850606188749264 ) ) ;
#36864 = CARTESIAN_POINT ( 'NONE',  ( 4.313465427442102929, 8.184126765324453601, 0.7998128361456462443 ) ) ;
#36866 = CARTESIAN_POINT ( 'NONE',  ( -5.901845825571131243, 6.006233656505717278, 0.1738135011533047114 ) ) ;
#36867 = CARTESIAN_POINT ( 'NONE',  ( 9.827407719474571479, -6.362962251424049143, -0.4359508081058064421 ) ) ;
#36868 = CIRCLE ( 'NONE', #33475, 0.2000000000000000111 ) ;
#36869 = CARTESIAN_POINT ( 'NONE',  ( 6.877413162628407406, -0.1429737755889188000, 1.930079329684093237 ) ) ;
#36870 = CARTESIAN_POINT ( 'NONE',  ( -8.532158741701643123, 8.848606708273724308, 0.7998128361456462443 ) ) ;
#36871 = CARTESIAN_POINT ( 'NONE',  ( -5.246642258364192735, 5.223430177620739023, 0.7216878364870317197 ) ) ;
#36872 = CARTESIAN_POINT ( 'NONE',  ( 4.979703994296570180, -0.7212954316567052881, 1.883311551353183511 ) ) ;
#36873 = AXIS2_PLACEMENT_3D ( 'NONE', #131496, #197500, #44891 ) ;
#36874 = CARTESIAN_POINT ( 'NONE',  ( 1.095004809772756493, -0.5519004177921453813, -2.194067758203117169 ) ) ;
#36876 = VERTEX_POINT ( 'NONE', #97563 ) ;
#36875 = CARTESIAN_POINT ( 'NONE',  ( -6.043183783389232566, 8.073467052085995022, 1.599625672291269396 ) ) ;
#36877 = CARTESIAN_POINT ( 'NONE',  ( 0.7499999999999867883, -0.1520833326505155458, -1.299038105676652899 ) ) ;
#36878 = CARTESIAN_POINT ( 'NONE',  ( 1.370139650511486007, -1.190941340819328564, 1.442406204513801971 ) ) ;
#36879 = CARTESIAN_POINT ( 'NONE',  ( 0.4043864329151745651, -0.9253471945274373001, -1.466404024333650247 ) ) ;
#36880 = CARTESIAN_POINT ( 'NONE',  ( 4.019203527901527018, -2.096847714747759106, 0.6372333828079318474 ) ) ;
#36881 = CARTESIAN_POINT ( 'NONE',  ( 6.124106107054944736, -1.275020473110911157, -1.923184551904693507 ) ) ;
#36882 = CARTESIAN_POINT ( 'NONE',  ( 0.8134386948647929216, -0.3029782207385351422, 2.038374528180360912 ) ) ;
#36883 = CARTESIAN_POINT ( 'NONE',  ( 3.872937777176552299, 1.828215432968218535, -0.6551730591081408317 ) ) ;
#36884 = CARTESIAN_POINT ( 'NONE',  ( -2.941756144040963417, 6.375873234782333476, -0.7216878364870257245 ) ) ;
#36885 = CARTESIAN_POINT ( 'NONE',  ( 5.466025653875023593, 0.9211120992074215419, 1.627924866423650530 ) ) ;
#36886 = CARTESIAN_POINT ( 'NONE',  ( 0.8723278719310798568, 13.34875300405935761, -1.099941997284231476 ) ) ;
#36887 = EDGE_CURVE ( 'NONE', #168810, #69998, #78087, .T. ) ;
#36888 = CARTESIAN_POINT ( 'NONE',  ( 3.445180431648313224, 7.033477913649446300, 0.7216878364870257245 ) ) ;
#36889 = CARTESIAN_POINT ( 'NONE',  ( -1.360316468750054630, 0.9114583336747262843, 0.7853790794158721500 ) ) ;
#36890 = CARTESIAN_POINT ( 'NONE',  ( 4.289685514112329123, 1.556909497225898109, -1.281360267751927129 ) ) ;
#36891 = CARTESIAN_POINT ( 'NONE',  ( -5.056828107772872727, 5.001980335264194721, -0.7216878364870197293 ) ) ;
#36892 = CARTESIAN_POINT ( 'NONE',  ( -6.252245114557387851, 7.323316050852266557, -1.199719254218453823 ) ) ;
#36893 = CARTESIAN_POINT ( 'NONE',  ( 9.423080456697809026, 10.95234760669099749, -1.199719254218446718 ) ) ;
#36895 = CARTESIAN_POINT ( 'NONE',  ( -6.818239715405332468, -6.631671885544856870, 6.594971855056608767 ) ) ;
#36894 = CARTESIAN_POINT ( 'NONE',  ( 2.525780997283606499, -1.050937884436175418, -1.492673824175783093 ) ) ;
#36896 = CARTESIAN_POINT ( 'NONE',  ( -3.610214042988883598, 7.433943160120816351, 0.7998128361456352531 ) ) ;
#36897 = CYLINDRICAL_SURFACE ( 'NONE', #116747, 2.725000000000000089 ) ;
#36898 = CARTESIAN_POINT ( 'NONE',  ( -10.20579153398542616, 5.000000000000003553, 7.525503907114123869 ) ) ;
#36899 = VERTEX_POINT ( 'NONE', #114916 ) ;
#36900 = CARTESIAN_POINT ( 'NONE',  ( -5.275531169048909952, 7.248148678680751189, -1.443375672974066548 ) ) ;
#36901 = CARTESIAN_POINT ( 'NONE',  ( -3.358669367883384105, 4.941533567329135401, -1.599625672291262513 ) ) ;
#36902 = CARTESIAN_POINT ( 'NONE',  ( -8.109748439268576803, 12.61312361245537517, 0.7998128361456481317 ) ) ;
#36903 = CARTESIAN_POINT ( 'NONE',  ( 5.619787797283516184, -0.4887302510508689801, 1.959527308111078669 ) ) ;
#36905 = ORIENTED_EDGE ( 'NONE', *, *, #136243, .T. ) ;
#36904 = CARTESIAN_POINT ( 'NONE',  ( 0.3641364058636682999, 0.6611385597973111761, -2.014868753213174823 ) ) ;
#36906 = CARTESIAN_POINT ( 'NONE',  ( -4.938913097128142304, 8.984092056616635347, -0.7998128361456362523 ) ) ;
#36907 = CARTESIAN_POINT ( 'NONE',  ( 4.656335691289526402, 7.519809842224722374, -1.199719254218452047 ) ) ;
#36908 = CARTESIAN_POINT ( 'NONE',  ( 5.875869988399868404, 1.225711027941748466, 1.656622483273604729 ) ) ;
#36909 = CARTESIAN_POINT ( 'NONE',  ( 5.203750078570229753, 1.864167652161516031, 0.7691231355932278690 ) ) ;
#36910 = VERTEX_POINT ( 'NONE', #147369 ) ;
#36911 = ORIENTED_EDGE ( 'NONE', *, *, #58073, .F. ) ;
#36912 = CARTESIAN_POINT ( 'NONE',  ( 3.602603900285803462, 7.346728939927271718, 0.3723553007324384989 ) ) ;
#36913 = CARTESIAN_POINT ( 'NONE',  ( 4.376584659113025744, 4.000436945253625254, 0.7998128361456341429 ) ) ;
#36914 = AXIS2_PLACEMENT_3D ( 'NONE', #38645, #155599, #138291 ) ;
#36916 = ORIENTED_EDGE ( 'NONE', *, *, #144311, .T. ) ;
#36915 = CARTESIAN_POINT ( 'NONE',  ( -5.981082042284069367, 7.006959133200059142, 1.199719254218452935 ) ) ;
#36917 = CARTESIAN_POINT ( 'NONE',  ( 4.666526410304530970, 8.402211131567142388, 0.5382107299411863499 ) ) ;
#36918 = CARTESIAN_POINT ( 'NONE',  ( 4.815779736370030761, -1.620933320526974031, 1.198678058543983571 ) ) ;
#36919 = CARTESIAN_POINT ( 'NONE',  ( 4.101369424419714527, -1.836060619117799497, 0.1375280490283348478 ) ) ;
#36920 = CARTESIAN_POINT ( 'NONE',  ( -0.02338929933905826986, 0.006294950389555685130, -1.710968156697996401 ) ) ;
#36921 = CARTESIAN_POINT ( 'NONE',  ( 2.456097291302907770, 0.6137686719557032822, -2.224517260854632639 ) ) ;
#36922 = CARTESIAN_POINT ( 'NONE',  ( 6.156284269057003655, 9.340026192945279249, -1.199719254218452047 ) ) ;
#36923 = CARTESIAN_POINT ( 'NONE',  ( 4.587301040747738590, 1.933109172225886185, -0.9673573668882375909 ) ) ;
#36924 = CARTESIAN_POINT ( 'NONE',  ( 8.229962938695207342, 9.560377169021284871, 1.199719254218462483 ) ) ;
#36925 = CARTESIAN_POINT ( 'NONE',  ( -0.02402099761080173090, -1.884047281740467872, -0.4708274727777494451 ) ) ;
#36926 = CARTESIAN_POINT ( 'NONE',  ( -4.924636110261798372, 6.768494766770632332, 1.599625672291267398 ) ) ;
#36927 =( GEOMETRIC_REPRESENTATION_CONTEXT ( 3 ) GLOBAL_UNCERTAINTY_ASSIGNED_CONTEXT ( ( #185278 ) ) GLOBAL_UNIT_ASSIGNED_CONTEXT ( ( #107039, #20381, #137366 ) ) REPRESENTATION_CONTEXT ( 'NONE', 'WORKASPACE' ) );
#36928 = CARTESIAN_POINT ( 'NONE',  ( 2.624193383061829365, 0.3882907696143748644, -0.1722368472184270249 ) ) ;
#36929 = CARTESIAN_POINT ( 'NONE',  ( -1.500000000000015099, 12.76041666734946212, -0.8660254037844309360 ) ) ;
#36930 = CARTESIAN_POINT ( 'NONE',  ( 3.555401268124198655, 0.4554524271490404952, -1.814226883376020671 ) ) ;
#36931 = CARTESIAN_POINT ( 'NONE',  ( 6.244996228834688523, -1.665663155820007013, 1.054347381401467887 ) ) ;
#36932 = B_SPLINE_CURVE_WITH_KNOTS ( 'NONE', 3,
 ( #143296, #187720, #6820, #58799 ),
 .UNSPECIFIED., .F., .F.,
 ( 4, 4 ),
 ( 0.000000000000000000, 0.0004304244924211256284 ),
 .UNSPECIFIED. ) ;
#36934 = CARTESIAN_POINT ( 'NONE',  ( -8.100070429521727178, 8.414780020722290033, 0.7998128361456341429 ) ) ;
#36933 = CARTESIAN_POINT ( 'NONE',  ( -1.602468905319636405E-14, -1.131249999317182064, -1.732050807568870754 ) ) ;
#36935 = CARTESIAN_POINT ( 'NONE',  ( 2.192262590105994668, -0.9421081357594159877, 1.995820444975453745 ) ) ;
#36936 = EDGE_LOOP ( 'NONE', ( #88507, #156816, #206433, #129327 ) ) ;
#36937 = EDGE_CURVE ( 'NONE', #61771, #90338, #200367, .T. ) ;
#36938 = CARTESIAN_POINT ( 'NONE',  ( 1.262825079187945398, 3.294887467576579798, 0.7750000000000100142 ) ) ;
#36939 = CARTESIAN_POINT ( 'NONE',  ( 2.679707916995359263, 6.278076336469897711, -0.7998128361456291469 ) ) ;
#36940 = CARTESIAN_POINT ( 'NONE',  ( -5.111587607552082524, 5.922272616020886282, 1.199719254218450271 ) ) ;
#36941 = AXIS2_PLACEMENT_3D ( 'NONE', #63243, #146660, #95773 ) ;
#36942 = CARTESIAN_POINT ( 'NONE',  ( -2.331034670843834533E-15, -8.526088927971001041, -10.80093815994595730 ) ) ;
#36943 = CARTESIAN_POINT ( 'NONE',  ( 1.001173315506132422, 1.609201512179364135, 1.138472824994830379 ) ) ;
#36944 = CARTESIAN_POINT ( 'NONE',  ( 6.551428954101934821, -1.849038126066489207, -1.380618780084260644 ) ) ;
#36945 = CARTESIAN_POINT ( 'NONE',  ( 0.8362905744919849615, -1.092891352686057527, 1.629061181365853539 ) ) ;
#36946 = EDGE_CURVE ( 'NONE', #116745, #121840, #87170, .T. ) ;
#36947 = CARTESIAN_POINT ( 'NONE',  ( 4.416881224320576393, -1.531859844946925397, 1.381376250335116795 ) ) ;
#36948 = CARTESIAN_POINT ( 'NONE',  ( 5.883875478650832491, 6.927238148923188454, -1.082531754730543083 ) ) ;
#36949 = CARTESIAN_POINT ( 'NONE',  ( 7.340813827156391191, 7.528980651296110160, 0.7998128361456281477 ) ) ;
#36950 = ORIENTED_EDGE ( 'NONE', *, *, #184582, .T. ) ;
#36951 = CARTESIAN_POINT ( 'NONE',  ( 8.419250203962011625, 8.924806114151579095, -0.7216878364870267237 ) ) ;
#36952 = CARTESIAN_POINT ( 'NONE',  ( -1.001543065824772872E-14, 4.884375000341420581, 1.575800808251672791 ) ) ;
#36953 = CARTESIAN_POINT ( 'NONE',  ( -0.4655551865852154414, -8.176568542494919711, -9.512045263456256450 ) ) ;
#36954 = CARTESIAN_POINT ( 'NONE',  ( 3.511198595814921219, 7.040222761851976152, 0.7216878364870317197 ) ) ;
#36955 = CARTESIAN_POINT ( 'NONE',  ( 6.830535128024421532, -1.341686296255087063, 1.707861204732928018 ) ) ;
#36957 = CARTESIAN_POINT ( 'NONE',  ( 5.319803798718575116, 1.092037692397327620, -1.482314076171886708 ) ) ;
#36956 = CARTESIAN_POINT ( 'NONE',  ( 9.622374086701777074, -9.063146643177445227, -0.5328106107931120938 ) ) ;
#36958 = EDGE_CURVE ( 'NONE', #211239, #85368, #22711, .T. ) ;
#36959 = CARTESIAN_POINT ( 'NONE',  ( 9.469892045836674654, -6.532648833121171172, -0.4294077647110511320 ) ) ;
#36960 = CARTESIAN_POINT ( 'NONE',  ( -11.92619525870750508, 12.57377703206319808, -1.328859154004902621 ) ) ;
#36961 = CARTESIAN_POINT ( 'NONE',  ( 1.499999999999990896, 5.775000000000023448, 1.040834085586084257E-14 ) ) ;
#36962 = CARTESIAN_POINT ( 'NONE',  ( -4.867404985860277478, 6.905081695904778272, 1.445136279841979121 ) ) ;
#36963 = CARTESIAN_POINT ( 'NONE',  ( 5.620636616140949116, 7.477306742562066511, -1.332712173395997013 ) ) ;
#36964 = CARTESIAN_POINT ( 'NONE',  ( 1.364683531249990311, 5.676041667008088432, 0.7879004041258500513 ) ) ;
#36965 = CARTESIAN_POINT ( 'NONE',  ( 1.172351427048579531, 0.7757545017167379875, 1.748050575570128107 ) ) ;
#36966 = CARTESIAN_POINT ( 'NONE',  ( 1.674285954873380167, -1.679204462075728488, -0.5593204692268695100 ) ) ;
#36967 = CARTESIAN_POINT ( 'NONE',  ( 5.848296790250511634, 0.9903421736442417078, -1.752559156024376508 ) ) ;
#36969 = CARTESIAN_POINT ( 'NONE',  ( 4.622610566699385082, 0.3315282304991398754, 1.886534565956134335 ) ) ;
#36968 = CARTESIAN_POINT ( 'NONE',  ( -8.319899820280397762, 12.85830022363583147, -0.7998128361456281477 ) ) ;
#36970 = CARTESIAN_POINT ( 'NONE',  ( -1.792021045695255545E-15, 2.999999999999988898, 1.224999999999993427 ) ) ;
#36971 = CARTESIAN_POINT ( 'NONE',  ( 5.670349227943210835, -0.8838483254627060859, -1.760150121488897490 ) ) ;
#36972 = CARTESIAN_POINT ( 'NONE',  ( 6.187761630889374587, 1.931537729788906477, -0.5904018810464291001 ) ) ;
#36973 = DIRECTION ( 'NONE',  ( 0.000000000000000000, 1.000000000000000000, 0.000000000000000000 ) ) ;
#36974 = CARTESIAN_POINT ( 'NONE',  ( 4.065207594588423845, 0.2294239933214488880, -1.856472568989680161 ) ) ;
#36976 = ORIENTED_EDGE ( 'NONE', *, *, #109534, .T. ) ;
#36975 = CARTESIAN_POINT ( 'NONE',  ( 6.129511981615775262, -1.621618681806114459, 0.5882815792577487102 ) ) ;
#36978 = CARTESIAN_POINT ( 'NONE',  ( 2.562127843302666186, 5.932973550587659517, 0.000000000000000000 ) ) ;
#36977 = CARTESIAN_POINT ( 'NONE',  ( 3.809358915828209735, 1.892446193107431451, 1.135094405146239049 ) ) ;
#36979 = CARTESIAN_POINT ( 'NONE',  ( 0.6823417656249899377, 2.905208333674754062, 1.181850606188765695 ) ) ;
#36980 = CARTESIAN_POINT ( 'NONE',  ( 0.3267250850040852583, -1.348467290049197853, 1.560915443186759122 ) ) ;
#36981 = CARTESIAN_POINT ( 'NONE',  ( 7.019370843573166319, 9.212351955633947043, 1.599625672291281386 ) ) ;
#36982 = CARTESIAN_POINT ( 'NONE',  ( -9.528683032306089373, 10.01121838064558744, 0.7998128361456462443 ) ) ;
#36983 = DIRECTION ( 'NONE',  ( 1.000000000000000000, 0.000000000000000000, 0.000000000000000000 ) ) ;
#36984 = CARTESIAN_POINT ( 'NONE',  ( -3.418627288940168096, 7.140148937072163804, -0.7998128361456282587 ) ) ;
#36985 = ADVANCED_FACE ( 'NONE', ( #198216 ), #18399, .T. ) ;
#36986 = CARTESIAN_POINT ( 'NONE',  ( -1.499999999999963141, 7.750000000000000000, 10.86128356754324820 ) ) ;
#36987 = ORIENTED_EDGE ( 'NONE', *, *, #40952, .T. ) ;
#36988 = CARTESIAN_POINT ( 'NONE',  ( 2.857943571468853250, -0.6518772230660694333, 1.965110387975615991 ) ) ;
#36989 = CARTESIAN_POINT ( 'NONE',  ( -1.500000000000011324, 4.170833333333359150, 0.8660254037844403729 ) ) ;
#36990 = CARTESIAN_POINT ( 'NONE',  ( 4.147904930777053245, 6.926640621626830807, -1.199719254218452047 ) ) ;
#36991 = CARTESIAN_POINT ( 'NONE',  ( -6.546709703855362328, 6.802806841334552601, 0.4695730141109008549 ) ) ;
#36992 = CARTESIAN_POINT ( 'NONE',  ( 0.8385427299653764877, 1.201306043029852777, -1.623412603403198373 ) ) ;
#36994 = CARTESIAN_POINT ( 'NONE',  ( 8.053180056837369705, 11.37883191874353805, -1.082531754730543083 ) ) ;
#36993 = CARTESIAN_POINT ( 'NONE',  ( 0.1747926744264659826, 0.006858446013176252437, -1.855468577918440332 ) ) ;
#36995 = CARTESIAN_POINT ( 'NONE',  ( 6.468125021464291358, 1.674632898861495134, 1.122323893169609565 ) ) ;
#36996 = CARTESIAN_POINT ( 'NONE',  ( 5.507027455500737467, -0.04000985115821522470, 1.915467925163343965 ) ) ;
#36997 = CARTESIAN_POINT ( 'NONE',  ( 6.639320575229281651, 0.5623622132289189945, 2.255000583061476771 ) ) ;
#36998 = CARTESIAN_POINT ( 'NONE',  ( 3.298540952264991777, 1.726358142885858316, -1.349911518210664241 ) ) ;
#37000 = PRESENTATION_LAYER_ASSIGNMENT (  '', '', ( #19829 ) ) ;
#36999 = CARTESIAN_POINT ( 'NONE',  ( -0.7500000000000006661, 3.139583334016149418, -1.299038105676652011 ) ) ;
#37001 = CARTESIAN_POINT ( 'NONE',  ( 2.250135261179100343, 0.8981609309555338427, -1.688322754368525747 ) ) ;
#37002 = CARTESIAN_POINT ( 'NONE',  ( -5.091250377131585125, 5.898545847196970726, 1.199719254218450271 ) ) ;
#37003 = CARTESIAN_POINT ( 'NONE',  ( 3.619663824724254741, 6.206396314611513532, -1.082531754730543971 ) ) ;
#37005 = CARTESIAN_POINT ( 'NONE',  ( 0.5445462702219765472, -1.458543044971000402, 1.392561646250379814 ) ) ;
#37004 = DIRECTION ( 'NONE',  ( 0.000000000000000000, -1.000000000000000000, 0.000000000000000000 ) ) ;
#37006 = CARTESIAN_POINT ( 'NONE',  ( -0.6823417656250003738, 11.46354166700806765, 1.181850606188754593 ) ) ;
#37008 = CARTESIAN_POINT ( 'NONE',  ( -6.005335696210345020, 5.970922831858983315, 0.7998128361456281477 ) ) ;
#37007 = CARTESIAN_POINT ( 'NONE',  ( 5.987848539424092564, -2.180829346447300310, -0.2163489798085171945 ) ) ;
#37010 = VERTEX_POINT ( 'NONE', #153750 ) ;
#37009 = CARTESIAN_POINT ( 'NONE',  ( 2.537784596217841138, 0.8154259780687975745, -1.519840121599738803 ) ) ;
#37011 = CARTESIAN_POINT ( 'NONE',  ( 7.096803341749390981, 10.36702210109460154, -1.199719254218441611 ) ) ;
#37012 = CARTESIAN_POINT ( 'NONE',  ( 3.798255590122797898, 7.583048621785260401, -0.7998128361456221525 ) ) ;
#37013 = CARTESIAN_POINT ( 'NONE',  ( -1.150222622689967888, 2.972854968409793575, -0.7749999999993613109 ) ) ;
#37014 = CARTESIAN_POINT ( 'NONE',  ( 1.293326634533353170, -1.775083115552608559, 0.8357255594537355003 ) ) ;
#37015 = DIRECTION ( 'NONE',  ( -5.578564026256490882E-16, -1.000000000000000000, -9.066213480720158442E-32 ) ) ;
#37016 = CARTESIAN_POINT ( 'NONE',  ( 0.07556134207196538166, 0.2286499876833356648, -2.278112926217394030 ) ) ;
#37017 = ORIENTED_EDGE ( 'NONE', *, *, #56788, .T. ) ;
#37018 = CARTESIAN_POINT ( 'NONE',  ( -0.3585786437627170309, 3.975028841772325627, -0.9637995837463111393 ) ) ;
#37019 = ORIENTED_EDGE ( 'NONE', *, *, #209526, .T. ) ;
#37020 = CARTESIAN_POINT ( 'NONE',  ( 3.949720763895887110, -1.252031560403286337, -1.309370340798710730 ) ) ;
#37021 = EDGE_LOOP ( 'NONE', ( #113052, #180091, #192697, #169705 ) ) ;
#37022 = CARTESIAN_POINT ( 'NONE',  ( 9.887974103068218668, 10.43039129653476493, 0.7998128361456462443 ) ) ;
#37023 = DIRECTION ( 'NONE',  ( -7.387867266669436732E-31, 1.000000000000000000, -8.546850786086437571E-32 ) ) ;
#37024 = CARTESIAN_POINT ( 'NONE',  ( 5.391193890671133637, -0.05051413884850668168, -1.810949582550380521 ) ) ;
#37025 = CARTESIAN_POINT ( 'NONE',  ( 6.156811153937166381, 10.19704708965311468, 0.000000000000000000 ) ) ;
#37026 = CARTESIAN_POINT ( 'NONE',  ( 0.3591838038534900801, -8.233137084989865073, 9.493791972417897185 ) ) ;
#37027 = CARTESIAN_POINT ( 'NONE',  ( 5.770924896911269641, 6.051163903260999177, -0.5763553215429690901 ) ) ;
#37029 = CARTESIAN_POINT ( 'NONE',  ( 1.364683531249996529, 15.21354166700806587, 0.7879004041258405033 ) ) ;
#37028 = CARTESIAN_POINT ( 'NONE',  ( 5.107777090148794663, 0.5842497386982176133, -1.767012650282340003 ) ) ;
#37030 = CARTESIAN_POINT ( 'NONE',  ( 2.425271589312021359, -1.421058436811825754, -1.284788359014801706 ) ) ;
#37031 = CARTESIAN_POINT ( 'NONE',  ( -0.08000000000000367928, -7.473374494045017968, 9.579665964948883783 ) ) ;
#37032 = CARTESIAN_POINT ( 'NONE',  ( -10.45142682343936791, 5.144546645612242841, 5.216777551074719632 ) ) ;
#37033 = CIRCLE ( 'NONE', #175432, 0.08000000000000020983 ) ;
#37034 = CARTESIAN_POINT ( 'NONE',  ( 1.499999999999956257, 5.577083334016155192, -0.8660254037844512531 ) ) ;
#37035 = DIRECTION ( 'NONE',  ( 1.000000000000000000, -0.000000000000000000, -0.000000000000000000 ) ) ;
#37036 = CARTESIAN_POINT ( 'NONE',  ( 6.982085921357777281, 7.248114451113292667, 1.040834085586084257E-14 ) ) ;
#37037 = CARTESIAN_POINT ( 'NONE',  ( -4.776550190716183586, 4.467063398790632966, 1.214306433183764966E-14 ) ) ;
#37038 = CARTESIAN_POINT ( 'NONE',  ( -3.469446951953614189E-15, 3.236073672982384242, -5.377642775528101993E-14 ) ) ;
#37039 = CARTESIAN_POINT ( 'NONE',  ( -5.101610940492132151, 9.173906207207963348, -0.7998128361456362523 ) ) ;
#37040 = CARTESIAN_POINT ( 'NONE',  ( 0.8145359132093257237, 1.932373828749304856, 0.7984225692715187783 ) ) ;
#37041 = CARTESIAN_POINT ( 'NONE',  ( 4.518610335104485287, 8.493738834255713854, 0.000000000000000000 ) ) ;
#37042 = CARTESIAN_POINT ( 'NONE',  ( 1.360069071312763223, 0.7361036424862777983, 1.670779996689908398 ) ) ;
#37043 = CARTESIAN_POINT ( 'NONE',  ( -5.752737250900127997, 5.605948302338584099, 0.000000000000000000 ) ) ;
#37044 = CARTESIAN_POINT ( 'NONE',  ( 2.344514592193002400, 0.3973361102717864468, 1.781653928021959432 ) ) ;
#37045 = ADVANCED_FACE ( 'NONE', ( #51991 ), #67135, .T. ) ;
#37046 = DIRECTION ( 'NONE',  ( 0.000000000000000000, 0.000000000000000000, 1.000000000000000000 ) ) ;
#37047 = CARTESIAN_POINT ( 'NONE',  ( 1.933716311909071006, -1.854087253938462521, 0.4680378644332866545 ) ) ;
#37048 = CARTESIAN_POINT ( 'NONE',  ( 1.099984078287146394, 0.8012805854674235340, -1.799388124431312797 ) ) ;
#37049 = ORIENTED_EDGE ( 'NONE', *, *, #123836, .F. ) ;
#37050 = CARTESIAN_POINT ( 'NONE',  ( 4.036618323093550842, -1.688041843851136425, 0.9601762628524412868 ) ) ;
#37051 = ORIENTED_EDGE ( 'NONE', *, *, #57845, .F. ) ;
#37052 = CARTESIAN_POINT ( 'NONE',  ( -5.191846479390389568, 5.021852078902356631, 0.7998128361456281477 ) ) ;
#37054 = CARTESIAN_POINT ( 'NONE',  ( 4.535463010148616192, -0.1012041512906610846, 2.118281909017679432 ) ) ;
#37053 = CARTESIAN_POINT ( 'NONE',  ( 3.923105346307896202, 5.670318552149568703, -1.599625672291269396 ) ) ;
#37055 = CARTESIAN_POINT ( 'NONE',  ( 6.500815856195029774, -6.554751173179699464, 6.901817412891874781 ) ) ;
#37056 = CARTESIAN_POINT ( 'NONE',  ( 7.964525173024008531, 11.37936423758166526, 1.199719254218460707 ) ) ;
#37057 = CARTESIAN_POINT ( 'NONE',  ( 5.951559787436734084, 6.118878616701469042, 0.7174803059855124898 ) ) ;
#37058 = CARTESIAN_POINT ( 'NONE',  ( 0.2331563151865738703, 7.629137130509052511, -2.545728013813946866 ) ) ;
#37059 = ORIENTED_EDGE ( 'NONE', *, *, #85823, .T. ) ;
#37060 = CARTESIAN_POINT ( 'NONE',  ( 6.282224075085741433, 8.422623735723785643, 1.599625672291268286 ) ) ;
#37061 = CARTESIAN_POINT ( 'NONE',  ( 3.633072077242065861E-15, -6.802539632833518519E-15, -0.2598076211376265099 ) ) ;
#37062 = CARTESIAN_POINT ( 'NONE',  ( 4.301258635363705451, 1.467727663998198429, 1.085573330547324744 ) ) ;
#37063 = CARTESIAN_POINT ( 'NONE',  ( 10.99946651476068205, -9.910601012391426323, -0.1083346235443097966 ) ) ;
#37064 = CARTESIAN_POINT ( 'NONE',  ( -8.676855123066019360, 11.14608361504227574, -1.443375672974059665 ) ) ;
#37065 = VECTOR ( 'NONE', #4372, 1000.000000000000000 ) ;
#37066 = CARTESIAN_POINT ( 'NONE',  ( -4.631600894319110040, 8.440630447364583233, 0.4419995416731822280 ) ) ;
#37067 = CARTESIAN_POINT ( 'NONE',  ( 7.055786748302883993, -6.583711766989194913, -6.534012848837080334 ) ) ;
#37068 = CARTESIAN_POINT ( 'NONE',  ( 5.084763247618332649, -0.2297073032716222263, -1.856415652357709778 ) ) ;
#37069 = CARTESIAN_POINT ( 'NONE',  ( 7.130698725783555680, 10.40656671580112658, 1.199719254218460707 ) ) ;
#37070 = CARTESIAN_POINT ( 'NONE',  ( 1.857912668630396169, 1.921361403365331677, -0.1415498456752254663 ) ) ;
#37071 = CARTESIAN_POINT ( 'NONE',  ( 6.209812062937981381, 0.5727486527220859713, -1.876249287704085722 ) ) ;
#37073 = EDGE_CURVE ( 'NONE', #69090, #92214, #40847, .T. ) ;
#37072 =( GEOMETRIC_REPRESENTATION_CONTEXT ( 3 ) GLOBAL_UNCERTAINTY_ASSIGNED_CONTEXT ( ( #42268 ) ) GLOBAL_UNIT_ASSIGNED_CONTEXT ( ( #55053, #57186, #58252 ) ) REPRESENTATION_CONTEXT ( 'NONE', 'WORKASPACE' ) );
#37074 = CARTESIAN_POINT ( 'NONE',  ( 4.542145155778077203, 5.257923088951247159, -1.199719254218452047 ) ) ;
#37075 = CARTESIAN_POINT ( 'NONE',  ( 0.6823417656249969321, 8.838541667008065872, -1.181850606188757036 ) ) ;
#37076 = CARTESIAN_POINT ( 'NONE',  ( -7.237355071596549116, 7.338002426484427687, 1.040834085586084257E-14 ) ) ;
#37077 = CARTESIAN_POINT ( 'NONE',  ( 5.684946482831785275, 5.526859072925533134, -0.7998128361456231517 ) ) ;
#37078 = CARTESIAN_POINT ( 'NONE',  ( -4.272227801637618505, 7.998366511970260717, 0.7216878364870338292 ) ) ;
#37079 = CARTESIAN_POINT ( 'NONE',  ( 1.458780272697857594, -2.011719176664223951, -0.6602987507247930488 ) ) ;
#37080 = CARTESIAN_POINT ( 'NONE',  ( 10.55232363013785246, 11.20546574478267132, 0.000000000000000000 ) ) ;
#37081 = LINE ( 'NONE', #169221, #18309 ) ;
#37082 = CARTESIAN_POINT ( 'NONE',  ( 6.051642586050198780, 1.563818258945088191, 1.356687170345116211 ) ) ;
#37084 = CARTESIAN_POINT ( 'NONE',  ( 4.024405658984873568, 7.794362949307388710, 0.3537781459504486525 ) ) ;
#37083 = CARTESIAN_POINT ( 'NONE',  ( 0.5207438388301621757, -1.748553680932497745, 0.5769860859521497298 ) ) ;
#37085 = CARTESIAN_POINT ( 'NONE',  ( 6.135373049470649320, 0.7166818055565070678, 2.184152129457237912 ) ) ;
#37086 = CARTESIAN_POINT ( 'NONE',  ( 4.989037340148863464, 8.764367963574922982, -0.7216878364870257245 ) ) ;
#37088 = CARTESIAN_POINT ( 'NONE',  ( 0.3384194684227018746, 6.989896059384769877, 3.860023792759414096 ) ) ;
#37087 = CARTESIAN_POINT ( 'NONE',  ( 4.502716413514295191, 6.346531463890372926, -1.443375672974068769 ) ) ;
#37089 = CARTESIAN_POINT ( 'NONE',  ( 1.201600019185744994, -0.5526092242729553350, 2.224544611104557035 ) ) ;
#37090 = LINE ( 'NONE', #188681, #78022 ) ;
#37091 = VECTOR ( 'NONE', #123524, 1000.000000000000000 ) ;
#37092 = CARTESIAN_POINT ( 'NONE',  ( -5.478376588373717659, 8.549133898814758936, -1.199719254218452047 ) ) ;
#37093 = CARTESIAN_POINT ( 'NONE',  ( 6.509718631618705231, -0.9178700960432868428, -1.711342201762585002 ) ) ;
#37094 = ORIENTED_EDGE ( 'NONE', *, *, #207217, .F. ) ;
#37095 = CARTESIAN_POINT ( 'NONE',  ( 8.392133896734668141, 9.853539636687704828, 1.082531754730558626 ) ) ;
#37096 = ADVANCED_FACE ( 'NONE', ( #2129 ), #68204, .F. ) ;
#37097 = ORIENTED_EDGE ( 'NONE', *, *, #92378, .F. ) ;
#37098 = CARTESIAN_POINT ( 'NONE',  ( -0.01731850797281712928, -1.311767784893268285, 1.527291784361783922 ) ) ;
#37099 = CARTESIAN_POINT ( 'NONE',  ( 6.298064597363540074, -0.9548514761729166578, -1.776169100128288658 ) ) ;
#37101 = DIRECTION ( 'NONE',  ( 1.000000000000000000, -0.000000000000000000, -0.000000000000000000 ) ) ;
#37100 = CARTESIAN_POINT ( 'NONE',  ( -9.365985188942097750, 9.821404230054264772, 0.7998128361456462443 ) ) ;
#37102 = CARTESIAN_POINT ( 'NONE',  ( -10.39320420135713263, 4.932286138528427344, 5.331284845095887626 ) ) ;
#37104 = CARTESIAN_POINT ( 'NONE',  ( 1.674285954873380167, -1.679204462075728488, -0.5593204692268695100 ) ) ;
#37103 = CARTESIAN_POINT ( 'NONE',  ( 2.835970919032384963, 2.074939634868844252, 0.2550863383830522801 ) ) ;
#37105 = CARTESIAN_POINT ( 'NONE',  ( 0.06263693352612137444, -7.008128100062071653, -9.499802063084663573 ) ) ;
#37106 = B_SPLINE_CURVE_WITH_KNOTS ( 'NONE', 3,
 ( #85789, #151870, #38112, #201640, #69511, #53288, #152922, #119421 ),
 .UNSPECIFIED., .F., .F.,
 ( 4, 2, 2, 4 ),
 ( 0.000000000000000000, 0.0004365159022975865317, 0.0006547738534463801770, 0.0008730318045951738224 ),
 .UNSPECIFIED. ) ;
#37108 = CARTESIAN_POINT ( 'NONE',  ( 4.277453538519633724, 1.495592673709666531, 1.737217383791799463 ) ) ;
#37107 = CARTESIAN_POINT ( 'NONE',  ( 5.422335090822693715, 5.290755458906732933, 0.000000000000000000 ) ) ;
#37109 = CARTESIAN_POINT ( 'NONE',  ( 3.064111502348449978, -1.608305157344312564, -0.6653965878143754953 ) ) ;
#37110 = CARTESIAN_POINT ( 'NONE',  ( 2.381428537494710618, 5.930083727052461562, 0.7998128361456462443 ) ) ;
#37111 = CARTESIAN_POINT ( 'NONE',  ( 4.050854035433010480, 7.948023151305657841, 0.000000000000000000 ) ) ;
#37112 = CARTESIAN_POINT ( 'NONE',  ( 3.233448856393176474, -1.601016440221241455, -0.6660543662743572124 ) ) ;
#37113 = CARTESIAN_POINT ( 'NONE',  ( 3.684171759641508448, -1.290596846074614223, -1.745836057026050714 ) ) ;
#37114 = CARTESIAN_POINT ( 'NONE',  ( 5.497994985541524215, 6.373081223675282736, -1.199719254218445830 ) ) ;
#37115 = CARTESIAN_POINT ( 'NONE',  ( 4.487517715496184501, -0.5331711073110931842, 1.944729879240604253 ) ) ;
#37116 = CARTESIAN_POINT ( 'NONE',  ( 2.562500000000001332, -1.451031289061222251, -1.451031289061014196 ) ) ;
#37117 = CARTESIAN_POINT ( 'NONE',  ( 1.499999999999990896, 3.306250000682818602, 1.214306433183764966E-14 ) ) ;
#37118 = CARTESIAN_POINT ( 'NONE',  ( 1.659075543930859764, -1.650851203806924294, -0.9926060514057006845 ) ) ;
#37119 = CARTESIAN_POINT ( 'NONE',  ( -1.402160292154681736E-14, 8.843750000682797818, 1.732050807568881190 ) ) ;
#37120 = CARTESIAN_POINT ( 'NONE',  ( 4.201594209339031494, 1.983332154306137518, -1.000733898520693499 ) ) ;
#37121 = ORIENTED_EDGE ( 'NONE', *, *, #134227, .F. ) ;
#37122 = CARTESIAN_POINT ( 'NONE',  ( -0.1106856583841086261, 0.2435294909829844312, -2.031701206977332586 ) ) ;
#37123 = CARTESIAN_POINT ( 'NONE',  ( 1.499999999999989120, 2.275000000000019895, 1.214306433183764966E-14 ) ) ;
#37124 = CARTESIAN_POINT ( 'NONE',  ( 6.962275575817444384, 8.081408578997208991, -1.199719254218446718 ) ) ;
#37125 = CARTESIAN_POINT ( 'NONE',  ( 4.650083499362867911, 6.448183387388563226, 1.443375672974062551 ) ) ;
#37126 = CARTESIAN_POINT ( 'NONE',  ( -1.642778471874998480, -2.151041666188707957, 2.845375778867863303 ) ) ;
#37127 = CARTESIAN_POINT ( 'NONE',  ( 0.2764465059262249391, 2.196205179236205396, -0.3323138113263158222 ) ) ;
#37128 = CARTESIAN_POINT ( 'NONE',  ( 5.986763597034561180, 1.890319730748804439, 0.5246630281777533433 ) ) ;
#37129 = CARTESIAN_POINT ( 'NONE',  ( 7.117667457494414762, 11.24776976714476184, 1.040834085586084257E-14 ) ) ;
#37130 = CARTESIAN_POINT ( 'NONE',  ( 0.6148119136215323133, 1.491057340773978668, -1.565211586912764741 ) ) ;
#37131 = CARTESIAN_POINT ( 'NONE',  ( 6.229045230835819069, 6.231917288922055320, -0.7998128361456481317 ) ) ;
#37132 = CARTESIAN_POINT ( 'NONE',  ( -5.668717624289589807, 5.786127781192186958, 0.7216878364870257245 ) ) ;
#37133 = CARTESIAN_POINT ( 'NONE',  ( 3.121586329596927722, 0.3053734461533639255, -2.039847365138738766 ) ) ;
#37134 = CARTESIAN_POINT ( 'NONE',  ( -5.850506979496850057, 6.784345216623154151, -1.199719254218446718 ) ) ;
#37135 =( BOUNDED_CURVE ( )  B_SPLINE_CURVE ( 2, ( #104673, #69991, #136103, #39660, #37522, #206416, #169655, #202119, #119912 ),
 .UNSPECIFIED., .F., .T. ) 
 B_SPLINE_CURVE_WITH_KNOTS ( ( 3, 2, 2, 2, 3 ),
 ( 0.8660714285714286031, 0.8690476190476190688, 0.8750000000000000000, 0.8809523809523809312, 0.8839285714285713969 ),
 .UNSPECIFIED. ) 
 CURVE ( )  GEOMETRIC_REPRESENTATION_ITEM ( )  RATIONAL_B_SPLINE_CURVE ( ( 0.9330127018922194093, 0.9330127018922194093, 1.000000000000000000, 0.8660254037844387076, 1.000000000000000000, 0.8660254037844387076, 1.000000000000000000, 0.9330127018922194093, 0.9330127018922194093 ) ) 
 REPRESENTATION_ITEM ( '' )  );
#37136 = CARTESIAN_POINT ( 'NONE',  ( 1.499999999999990896, 4.556250000682819490, 1.214306433183764966E-14 ) ) ;
#37137 = CARTESIAN_POINT ( 'NONE',  ( -1.364683531250012516, 5.051041667008085767, -0.7879004041258300672 ) ) ;
#37138 = CARTESIAN_POINT ( 'NONE',  ( 5.114452126850835612, 1.290914414355217366, -1.353902443742838191 ) ) ;
#37139 = CARTESIAN_POINT ( 'NONE',  ( 3.867547151669390448, -0.1745043776680033631, -1.725349009328189576 ) ) ;
#37140 = CARTESIAN_POINT ( 'NONE',  ( 3.473892794100913672, -1.678317346756386108, -0.4606119698754263525 ) ) ;
#37141 = CARTESIAN_POINT ( 'NONE',  ( 0.2930494462585155335, 1.901387222806522503, -1.280258756811911702 ) ) ;
#37142 = CARTESIAN_POINT ( 'NONE',  ( -1.364683531249997417, 3.571875000341423245, 1.214306433183764966E-14 ) ) ;
#37143 = CARTESIAN_POINT ( 'NONE',  ( 6.075741423153157683, -1.117747424998961403, 1.766673535877111290 ) ) ;
#37144 = CARTESIAN_POINT ( 'NONE',  ( 6.369087006730828726, 1.857646680926292815, -0.5659663566517159072 ) ) ;
#37145 = CARTESIAN_POINT ( 'NONE',  ( 1.419999999999989049, 6.120000000000041851, -2.579999999999995630 ) ) ;
#37146 =( NAMED_UNIT ( * ) PLANE_ANGLE_UNIT ( ) SI_UNIT ( $, .RADIAN. ) );
#37147 = CARTESIAN_POINT ( 'NONE',  ( 2.057267738415057057, -1.238319999287675888, 1.591319116112683618 ) ) ;
#37148 = EDGE_CURVE ( 'NONE', #193127, #195818, #89717, .T. ) ;
#37149 = CARTESIAN_POINT ( 'NONE',  ( 0.4456111923471540170, 0.6836232613432815519, -2.082162021007263331 ) ) ;
#37150 = CARTESIAN_POINT ( 'NONE',  ( 8.299603047032746872, 13.24802564661077575, -8.551073489896891644 ) ) ;
#37151 = CARTESIAN_POINT ( 'NONE',  ( -8.178592977541617515, 10.56477777859713463, 1.599625672291295375 ) ) ;
#37152 =( BOUNDED_SURFACE ( )  B_SPLINE_SURFACE ( 3, 2, ( 
 ( #272, #1347, #182246 ),
 ( #145549, #15476, #166013 ),
 ( #114145, #46955, #81560 ),
 ( #161765, #99949, #147644 ) ),
 .UNSPECIFIED., .F., .F., .T. ) 
 B_SPLINE_SURFACE_WITH_KNOTS ( ( 4, 4 ),
 ( 3, 3 ),
 ( 3.141592653589793116, 4.712388980384689674 ),
 ( 0.000000000000000000, 1.000000000000000000 ),
 .UNSPECIFIED. ) 
 GEOMETRIC_REPRESENTATION_ITEM ( )  RATIONAL_B_SPLINE_SURFACE ( (
 ( 1.000000000000000000, 0.8661919058288115592, 1.000000000000000000),
 ( 1.000000000000000000, 0.8676977444973651421, 1.000000000000000000),
 ( 1.000000000000000000, 0.8014503788334911283, 1.000000000000000000),
 ( 1.000000000000000000, 0.7071067811865225927, 1.000000000000000000) ) ) 
 REPRESENTATION_ITEM ( '' )  SURFACE ( )  );
#37153 = CARTESIAN_POINT ( 'NONE',  ( 5.686755365928134687, 8.721966129303114101, 1.199719254218462483 ) ) ;
#37154 = CARTESIAN_POINT ( 'NONE',  ( 2.438272501909013901, -1.223040458498025673, -1.732039452853536776 ) ) ;
#37155 = AXIS2_PLACEMENT_3D ( 'NONE', #190575, #42231, #74713 ) ;
#37156 = ADVANCED_BREP_SHAPE_REPRESENTATION ( '', ( #84085, #200407 ), #13653 ) ;
#37157 = CARTESIAN_POINT ( 'NONE',  ( 1.364683531249988757, -0.6156249996585803075, 0.000000000000000000 ) ) ;
#37158 = CARTESIAN_POINT ( 'NONE',  ( 5.777927443424748510, 1.091106472389313131, 1.463626628978510702 ) ) ;
#37159 = VERTEX_POINT ( 'NONE', #21571 ) ;
#37160 = CARTESIAN_POINT ( 'NONE',  ( -5.498713818794216834, 8.572860667638675380, -1.199719254218452047 ) ) ;
#37161 = CARTESIAN_POINT ( 'NONE',  ( -0.3000000000000241918, 4.000000000000003553, -1.007084189318394385 ) ) ;
#37162 = CARTESIAN_POINT ( 'NONE',  ( 7.634649897826745857, 8.079715433652276957, 0.7216878364870267237 ) ) ;
#37163 = CARTESIAN_POINT ( 'NONE',  ( 1.001543065824772753E-15, -1.159374999522043481, 3.793834371823811669 ) ) ;
#37164 = CARTESIAN_POINT ( 'NONE',  ( -7.206322340863467346, 8.366129804884193888, 1.199719254218450271 ) ) ;
#37165 = CARTESIAN_POINT ( 'NONE',  ( 2.707290811070970804, 1.730213373471348737, -1.041854834777849126 ) ) ;
#37166 = CARTESIAN_POINT ( 'NONE',  ( 0.3234443461216755522, -0.1028566021752069376, 2.103582624919388078 ) ) ;
#37167 = CARTESIAN_POINT ( 'NONE',  ( 9.728138913005292210, 11.30824913904973705, -1.199719254218440723 ) ) ;
#37168 = CARTESIAN_POINT ( 'NONE',  ( 4.399146427517338864, -1.620787001191201560, 0.9142094169404291204 ) ) ;
#37169 = CARTESIAN_POINT ( 'NONE',  ( 9.215791728987056786, 11.77484298861683598, -1.599625672291262513 ) ) ;
#37170 =( BOUNDED_SURFACE ( )  B_SPLINE_SURFACE ( 3, 1, ( 
 ( #91947, #137492 ),
 ( #173193, #41061 ),
 ( #202441, #120233 ),
 ( #58356, #190469 ),
 ( #172116, #171033 ),
 ( #140713, #107168 ),
 ( #38909, #203508 ) ),
 .UNSPECIFIED., .T., .F., .F. ) 
 B_SPLINE_SURFACE_WITH_KNOTS ( ( 4, 3, 4 ),
 ( 2, 2 ),
 ( 0.000000000000000000, 0.5000000000000000000, 1.000000000000000000 ),
 ( 0.000000000000000000, 1.000000000000000000 ),
 .UNSPECIFIED. ) 
 GEOMETRIC_REPRESENTATION_ITEM ( )  RATIONAL_B_SPLINE_SURFACE ( (
 ( 1.000000000000000000, 1.000000000000000000),
 ( 0.3333333333333333703, 0.3333333333333333703),
 ( 0.3333333333333333703, 0.3333333333333333703),
 ( 1.000000000000000000, 1.000000000000000000),
 ( 0.3333333333333333703, 0.3333333333333333703),
 ( 0.3333333333333333703, 0.3333333333333333703),
 ( 1.000000000000000000, 1.000000000000000000) ) ) 
 REPRESENTATION_ITEM ( '' )  SURFACE ( )  );
#37171 = CARTESIAN_POINT ( 'NONE',  ( 4.207966135563057541, 7.175396087857926375, 2.420000000000000373 ) ) ;
#37172 = ORIENTED_EDGE ( 'NONE', *, *, #176059, .T. ) ;
#37173 = VERTEX_POINT ( 'NONE', #103942 ) ;
#37174 = CARTESIAN_POINT ( 'NONE',  ( -4.090809663021341969, 5.795697244990093644, 1.599625672291267398 ) ) ;
#37175 = CARTESIAN_POINT ( 'NONE',  ( -7.507464373665155399, 9.781794407407920389, 1.599625672291295375 ) ) ;
#37176 = CARTESIAN_POINT ( 'NONE',  ( 5.004447790439923160, -0.6182884515001166870, -1.717943145347331502 ) ) ;
#37178 = CARTESIAN_POINT ( 'NONE',  ( -4.277728075731661583, 7.474117497184462167, -1.086723757153153835 ) ) ;
#37177 = CARTESIAN_POINT ( 'NONE',  ( -7.123883369337781879, 7.275895117174344229, 0.7998128361456341429 ) ) ;
#37179 = CARTESIAN_POINT ( 'NONE',  ( -1.364683531250014514, -1.219791666325248602, 0.7879004041258379498 ) ) ;
#37180 = CARTESIAN_POINT ( 'NONE',  ( 1.510678448032206189, 1.731588368038105896, 0.09119125932234918575 ) ) ;
#37181 = CARTESIAN_POINT ( 'NONE',  ( 0.2865101139537007402, 1.286042648715233216, 1.172746904078510122 ) ) ;
#37183 = CARTESIAN_POINT ( 'NONE',  ( 8.649738815838679429, 10.15407870897571563, -1.082531754730543083 ) ) ;
#37182 = CARTESIAN_POINT ( 'NONE',  ( 5.075001523147505189, -2.171532227461204556, -0.7813444033149226087 ) ) ;
#37184 = CARTESIAN_POINT ( 'NONE',  ( -10.48266952940149466, 5.268049057482275366, -5.154014898524191146 ) ) ;
#37185 = CARTESIAN_POINT ( 'NONE',  ( 1.475930922893650798, 1.225283507603215805, 1.656815433548680438 ) ) ;
#37186 = CARTESIAN_POINT ( 'NONE',  ( 6.433027599926354867, 1.173280253959343211, 1.976260322036479167 ) ) ;
#37187 = CARTESIAN_POINT ( 'NONE',  ( 8.665224416106017458, 14.86907450242385309, -8.237936485434854461 ) ) ;
#37188 = CARTESIAN_POINT ( 'NONE',  ( -5.966470118465691641, 9.118576350588734059, -1.199719254218452047 ) ) ;
#37189 = CARTESIAN_POINT ( 'NONE',  ( 0.1101414390347132816, -0.8398613168552993002, -1.781629259513841657 ) ) ;
#37190 = AXIS2_PLACEMENT_3D ( 'NONE', #52763, #153477, #5049 ) ;
#37192 = CARTESIAN_POINT ( 'NONE',  ( -2.959422669532919326, 6.674686557755516780, 0.7998128361456352531 ) ) ;
#37191 = CARTESIAN_POINT ( 'NONE',  ( 3.638835171272115421, 1.817485770107383436, 0.5952672491930725007 ) ) ;
#37193 = CARTESIAN_POINT ( 'NONE',  ( 5.391335350415090488, 1.947751002805158560, -1.037606470750504828 ) ) ;
#37194 = CARTESIAN_POINT ( 'NONE',  ( 0.6124999999999707345, 2.145833334016141070, 1.060881119635899816 ) ) ;
#37195 = ADVANCED_FACE ( 'NONE', ( #185158 ), #36783, .T. ) ;
#37196 = CARTESIAN_POINT ( 'NONE',  ( -8.041394506236766659, 8.554250810130591631, -0.7216878364870338292 ) ) ;
#37197 = CARTESIAN_POINT ( 'NONE',  ( 3.377389663135653031, 6.954388683717978026, -0.7216878364870338292 ) ) ;
#37198 = CARTESIAN_POINT ( 'NONE',  ( -5.275531169048922386, 5.327410250078064458, -0.7216878364870338292 ) ) ;
#37199 = CARTESIAN_POINT ( 'NONE',  ( 5.602226918196428151, -0.9533447246646039597, 1.894147766696724799 ) ) ;
#37200 = ORIENTED_EDGE ( 'NONE', *, *, #190444, .F. ) ;
#37201 = CARTESIAN_POINT ( 'NONE',  ( 3.821538862543779391, -0.1730032229720068482, 2.301163704417693356 ) ) ;
#37202 = CARTESIAN_POINT ( 'NONE',  ( 4.070719198475009293, 1.388998261151509039, -1.385754695631277844 ) ) ;
#37203 = CARTESIAN_POINT ( 'NONE',  ( -5.204350862799341115, 7.165104988056252289, -1.599625672291271394 ) ) ;
#37204 = CARTESIAN_POINT ( 'NONE',  ( 1.252704021237858401, -0.4712815170893420724, -1.904206577484176321 ) ) ;
#37205 = CARTESIAN_POINT ( 'NONE',  ( 9.319154265906131940, 13.69453762107142225, 7.487145396731793134 ) ) ;
#37206 = CARTESIAN_POINT ( 'NONE',  ( -11.86239285000045918, 13.87999999999998302, 1.812080536912751061 ) ) ;
#37207 = ORIENTED_EDGE ( 'NONE', *, *, #36292, .T. ) ;
#37208 = CARTESIAN_POINT ( 'NONE',  ( 6.087125082597877324, 1.679220375458953862, 1.116214469231976869 ) ) ;
#37209 = CARTESIAN_POINT ( 'NONE',  ( -9.494787648271923786, 9.971673765939062406, 1.040834085586084257E-14 ) ) ;
#37210 = DIRECTION ( 'NONE',  ( -0.000000000000000000, -1.000000000000000000, -0.000000000000000000 ) ) ;
#37211 = CARTESIAN_POINT ( 'NONE',  ( 3.678747780723041760, 1.381198535464265520, -1.675025177318607783 ) ) ;
#37212 = CARTESIAN_POINT ( 'NONE',  ( 5.903649544107831382, 5.852288987739401982, -0.7998128361456481317 ) ) ;
#37214 = EDGE_CURVE ( 'NONE', #132173, #144032, #173215, .T. ) ;
#37213 = CARTESIAN_POINT ( 'NONE',  ( 0.7738737444688469358, 0.4079195088417563730, -2.080830740624163955 ) ) ;
#37215 = CARTESIAN_POINT ( 'NONE',  ( -1.500000000000013101, 2.202083334016153859, 0.8660254037844403729 ) ) ;
#37216 = CARTESIAN_POINT ( 'NONE',  ( 9.378489572351044856, 11.96465713920816043, -1.599625672291262513 ) ) ;
#37217 = CARTESIAN_POINT ( 'NONE',  ( 1.857254922381494255, 2.486639013987944402, 2.482058795360528869 ) ) ;
#37218 = CARTESIAN_POINT ( 'NONE',  ( 6.104935607482663507, 7.108274908414393245, 1.121150977946131722 ) ) ;
#37219 = CARTESIAN_POINT ( 'NONE',  ( 1.282574848904423082, -2.009897191344016232, -0.4543217371432185514 ) ) ;
#37221 = CARTESIAN_POINT ( 'NONE',  ( 0.1023730323140637083, 2.520000000000004903, 1.999999999999999556 ) ) ;
#37220 = CARTESIAN_POINT ( 'NONE',  ( -9.154780037725563702, 11.70366268214508487, 1.599625672291281386 ) ) ;
#37222 = CARTESIAN_POINT ( 'NONE',  ( 0.6823417656249882723, 2.426041667008084435, -1.181850606188749264 ) ) ;
#37223 = CYLINDRICAL_SURFACE ( 'NONE', #150023, 11.99999999999999112 ) ;
#37224 = ORIENTED_EDGE ( 'NONE', *, *, #52716, .F. ) ;
#37225 = CARTESIAN_POINT ( 'NONE',  ( 4.266199323752727146, 1.911794059647478949, -0.05023246155653331158 ) ) ;
#37226 = CIRCLE ( 'NONE', #130691, 11.00000000000000000 ) ;
#37227 =( BOUNDED_CURVE ( )  B_SPLINE_CURVE ( 2, ( #137060, #69880, #55795 ),
 .UNSPECIFIED., .F., .T. ) 
 B_SPLINE_CURVE_WITH_KNOTS ( ( 3, 3 ),
 ( 0.000000000000000000, 0.0005080973304710143749 ),
 .UNSPECIFIED. ) 
 CURVE ( )  GEOMETRIC_REPRESENTATION_ITEM ( )  RATIONAL_B_SPLINE_CURVE ( ( 1.000000000000000000, 0.9950988063024598373, 0.9905562134193928170 ) ) 
 REPRESENTATION_ITEM ( '' )  );
#37228 = FACE_OUTER_BOUND ( 'NONE', #69975, .T. ) ;
#37229 = CARTESIAN_POINT ( 'NONE',  ( 6.282224075085741433, 8.422623735723785643, 1.599625672291268286 ) ) ;
#37230 = CARTESIAN_POINT ( 'NONE',  ( -4.223528545856940042, 4.886203710709899006, -1.199719254218446718 ) ) ;
#37231 = CARTESIAN_POINT ( 'NONE',  ( 0.3338568476279568653, -0.9693210200989417213, -1.530242633214883963 ) ) ;
#37233 = CARTESIAN_POINT ( 'NONE',  ( 0.6553225869628921396, 1.845336034500634437, -0.5141059209906836402 ) ) ;
#37232 = CARTESIAN_POINT ( 'NONE',  ( 7.681709917290610257, -6.443545996361870642, 7.726139724254744046 ) ) ;
#37234 = CARTESIAN_POINT ( 'NONE',  ( 1.803268859043684058, -1.750145871244257467, 1.105767233283899920 ) ) ;
#37235 = CARTESIAN_POINT ( 'NONE',  ( -1.364683531250000748, -0.4281249996585800854, 0.000000000000000000 ) ) ;
#37236 = AXIS2_PLACEMENT_3D ( 'NONE', #157163, #8754, #127947 ) ;
#37237 = CARTESIAN_POINT ( 'NONE',  ( 1.059376886711576260, 0.3867523390363221125, -1.932997803022660666 ) ) ;
#37238 = CARTESIAN_POINT ( 'NONE',  ( 2.508196354075361789, -0.6984789837382252564, -1.686990664346368796 ) ) ;
#37240 = CARTESIAN_POINT ( 'NONE',  ( 5.701630405109389343, 7.302376724489803905, 1.216486997566777584 ) ) ;
#37239 = CARTESIAN_POINT ( 'NONE',  ( 0.4698728525199142303, 0.2201595520019784535, -2.297181220480988717 ) ) ;
#37241 = CARTESIAN_POINT ( 'NONE',  ( 0.6823417656249882723, 1.426041667008083547, -1.181850606188749264 ) ) ;
#37242 = CARTESIAN_POINT ( 'NONE',  ( 3.771981659335025938, -2.032644659601599457, 0.3498187521492699403 ) ) ;
#37243 = CARTESIAN_POINT ( 'NONE',  ( -6.358937740009323214, 7.377514437221045718, -1.199719254218446718 ) ) ;
#37244 = CARTESIAN_POINT ( 'NONE',  ( 8.423693512792301163, 8.722063941212843119, 0.7998128361456481317 ) ) ;
#37245 = CARTESIAN_POINT ( 'NONE',  ( 5.355634372598031767, 6.206993841907870291, -1.199719254218445830 ) ) ;
#37246 = ADVANCED_FACE ( 'NONE', ( #38929 ), #68479, .T. ) ;
#37247 = CARTESIAN_POINT ( 'NONE',  ( 5.005985031943777308, 6.863401842066294556, -1.599625672291256295 ) ) ;
#37249 = CARTESIAN_POINT ( 'NONE',  ( 1.499999999999987121, 3.545833333333356041, -0.8660254037844262731 ) ) ;
#37248 = CARTESIAN_POINT ( 'NONE',  ( 4.999102919943527290, 1.752478773177888582, -1.167534824283325667 ) ) ;
#37250 = CARTESIAN_POINT ( 'NONE',  ( 6.197728532230423859, -1.496850047335227085, -1.430563974149069661 ) ) ;
#37251 = CARTESIAN_POINT ( 'NONE',  ( 1.364683531249986537, 1.217708333674754950, -0.7879004041258239610 ) ) ;
#37252 = CARTESIAN_POINT ( 'NONE',  ( 3.321700061091820366, -2.084211496276411779, 0.5730272365244912791 ) ) ;
#37253 = CARTESIAN_POINT ( 'NONE',  ( 3.861976953351463848, 0.6784905939434657807, -1.902444917487989606 ) ) ;
#37254 = CARTESIAN_POINT ( 'NONE',  ( 6.620655732516628866, 4.686767102414819419, 2.836268676114994669 ) ) ;
#37257 = CARTESIAN_POINT ( 'NONE',  ( 6.493992391265805075, 6.678671999339316656, 1.040834085586084257E-14 ) ) ;
#37256 = CARTESIAN_POINT ( 'NONE',  ( -1.642778471875000035, -3.317708332855374476, -2.845375778867859751 ) ) ;
#37255 = CARTESIAN_POINT ( 'NONE',  ( 11.33772463945037146, 10.89999999999998259, 3.599999999999999201 ) ) ;
#37258 = CARTESIAN_POINT ( 'NONE',  ( -5.875479466675803231, 7.948088359245467416, -1.599625672291271394 ) ) ;
#37259 = CARTESIAN_POINT ( 'NONE',  ( 2.219935720625454412, 0.9462983093676997637, -1.780669029686342331 ) ) ;
#37260 = CARTESIAN_POINT ( 'NONE',  ( -9.664264568442742842, 10.16939683947169115, -0.7998128361456291469 ) ) ;
#37261 = CARTESIAN_POINT ( 'NONE',  ( -3.567766978690493307, 7.314145241780881435, 1.040834085586084257E-14 ) ) ;
#37262 = B_SPLINE_CURVE_WITH_KNOTS ( 'NONE', 3,
 ( #83712, #164973, #133582, #184408 ),
 .UNSPECIFIED., .F., .F.,
 ( 4, 4 ),
 ( 0.000000000000000000, 0.0007521701867342633907 ),
 .UNSPECIFIED. ) ;
#37263 = CARTESIAN_POINT ( 'NONE',  ( 0.7500000000000006661, 12.58333333333333570, 1.299038105676657340 ) ) ;
#37264 =( NAMED_UNIT ( * ) SI_UNIT ( $, .STERADIAN. ) SOLID_ANGLE_UNIT ( ) );
#37265 = CARTESIAN_POINT ( 'NONE',  ( -0.7500000000000006661, 13.20833333333333570, -1.299038105676657340 ) ) ;
#37267 = CARTESIAN_POINT ( 'NONE',  ( 4.622672832840883039, 0.3474877929729481840, 1.986098205159859909 ) ) ;
#37266 = CARTESIAN_POINT ( 'NONE',  ( -8.202319746143382773, 9.632089794331152532, 1.082531754730558626 ) ) ;
#37268 = CARTESIAN_POINT ( 'NONE',  ( -1.500000000000011324, 4.670833333333353821, 0.8660254037844403729 ) ) ;
#37269 = CARTESIAN_POINT ( 'NONE',  ( 6.088827306860007837, -0.2580713809433569650, -1.705207211698676062 ) ) ;
#37270 = CARTESIAN_POINT ( 'NONE',  ( 4.525389411911321602, 8.501647757197021704, -0.7998128361456381397 ) ) ;
#37272 = CARTESIAN_POINT ( 'NONE',  ( -0.4019237886466933696, 10.58258545099816850, 1.500000000000005995 ) ) ;
#37271 = CARTESIAN_POINT ( 'NONE',  ( 7.605760987586388744, 11.81721221891873697, 1.040834085586084257E-14 ) ) ;
#37273 = DIRECTION ( 'NONE',  ( 5.551115123125764829E-17, 0.000000000000000000, -1.000000000000000000 ) ) ;
#37274 = CARTESIAN_POINT ( 'NONE',  ( 5.624238404463478780, 1.114819804898508515, -1.501858222471161408 ) ) ;
#37275 = CARTESIAN_POINT ( 'NONE',  ( 0.2057266557286231146, 1.493221433009199517, 1.350316897416648843 ) ) ;
#37276 = CARTESIAN_POINT ( 'NONE',  ( -2.428612866367529932E-14, 2.999999999999999112, 7.500000000000000000 ) ) ;
#37277 = CARTESIAN_POINT ( 'NONE',  ( 0.4359507092142514972, -8.863025497814007281, -9.827344407697072626 ) ) ;
#37278 = ORIENTED_EDGE ( 'NONE', *, *, #137200, .T. ) ;
#37279 = CARTESIAN_POINT ( 'NONE',  ( 8.541273586484978253, 12.90864358430044589, 0.000000000000000000 ) ) ;
#37280 = CARTESIAN_POINT ( 'NONE',  ( 1.107046246104196552, -0.04665650516593074226, 2.016035445577879504 ) ) ;
#37281 = CARTESIAN_POINT ( 'NONE',  ( 1.037045679623523897, -0.04297598538225732429, 1.811226269459820903 ) ) ;
#37282 = CARTESIAN_POINT ( 'NONE',  ( 3.567203813726949058, 7.175838526074521440, 0.7216878364870257245 ) ) ;
#37283 = CARTESIAN_POINT ( 'NONE',  ( 5.591005849568446706, 5.791977450266268868, -0.7139200525481930182 ) ) ;
#37284 = CARTESIAN_POINT ( 'NONE',  ( 6.602457619730749627, 10.64669162308715222, 0.7216878364870438212 ) ) ;
#37285 = CARTESIAN_POINT ( 'NONE',  ( 5.587931867126699537, 9.671004278289832001, -0.7998128361456291469 ) ) ;
#37287 = CARTESIAN_POINT ( 'NONE',  ( 6.151949797202925119, 0.9892698599738621867, 1.640257924793379063 ) ) ;
#37286 = CARTESIAN_POINT ( 'NONE',  ( -6.240830780992103755, 6.175390754112560110, 1.040834085586084257E-14 ) ) ;
#37288 = CARTESIAN_POINT ( 'NONE',  ( 1.896098101912840894, 8.993996023093842496, 0.7750000000000004663 ) ) ;
#37289 = CARTESIAN_POINT ( 'NONE',  ( 3.929058411375439874, -1.000000000000000888, 0.7500000000000006661 ) ) ;
#37290 = CARTESIAN_POINT ( 'NONE',  ( -6.116136693540540570, 10.14959355252369910, 0.000000000000000000 ) ) ;
#37292 = ORIENTED_EDGE ( 'NONE', *, *, #137027, .F. ) ;
#37291 = CARTESIAN_POINT ( 'NONE',  ( 2.887523530030648988, 6.312601851770308414, 0.000000000000000000 ) ) ;
#37293 = CARTESIAN_POINT ( 'NONE',  ( -3.623053363349869382, 5.249981562040033189, 1.599625672291267398 ) ) ;
#37294 = CARTESIAN_POINT ( 'NONE',  ( 3.696290335837215224, -2.159122111672501454, -0.1082323872379290508 ) ) ;
#37295 = CARTESIAN_POINT ( 'NONE',  ( -2.823841133396259639, 6.516508098929413961, -0.7998128361456481317 ) ) ;
#37296 = CARTESIAN_POINT ( 'NONE',  ( 4.882344714696929877, 8.710169577206153591, -0.7216878364870458196 ) ) ;
#37297 = CARTESIAN_POINT ( 'NONE',  ( 0.2641366190093488164, 0.6592694798918593557, -2.015615888626711705 ) ) ;
#37298 = CARTESIAN_POINT ( 'NONE',  ( 5.350558509363329662, 0.5315954154057299652, 1.746479326997903092 ) ) ;
#37299 = CARTESIAN_POINT ( 'NONE',  ( 2.196496099369545263, -0.5219070890916230887, -1.900975273168264534 ) ) ;
#37300 = CARTESIAN_POINT ( 'NONE',  ( 4.746305163667582150, 0.9781546018433548983, -1.643150005489722787 ) ) ;
#37301 = ORIENTED_EDGE ( 'NONE', *, *, #105692, .T. ) ;
#37302 = DIRECTION ( 'NONE',  ( 0.000000000000000000, 0.000000000000000000, 1.000000000000000000 ) ) ;
#37303 = CARTESIAN_POINT ( 'NONE',  ( 6.074653383054481104, 1.324031319358546677, -1.458257743282452834 ) ) ;
#37304 = CARTESIAN_POINT ( 'NONE',  ( 0.7439598490389126573, 0.5628818913385369438, 1.858577368155549525 ) ) ;
#37305 = ORIENTED_EDGE ( 'NONE', *, *, #213004, .F. ) ;
#37306 = CARTESIAN_POINT ( 'NONE',  ( -3.634467696915153034, 6.397906858779740524, 1.199719254218452935 ) ) ;
#37307 = CARTESIAN_POINT ( 'NONE',  ( -3.363304624641834106, 6.081549941127532222, -1.199719254218452047 ) ) ;
#37309 = CARTESIAN_POINT ( 'NONE',  ( 6.333067150914808430, 8.481940657524365434, 1.443375672974063439 ) ) ;
#37308 = CARTESIAN_POINT ( 'NONE',  ( 6.774270308322468459, 11.05506579301824743, 0.7998128361456462443 ) ) ;
#37311 = ORIENTED_EDGE ( 'NONE', *, *, #181736, .T. ) ;
#37310 = CARTESIAN_POINT ( 'NONE',  ( 4.547458224165379370, -1.746952781796942133, 0.7782266863690868730 ) ) ;
#37312 = CARTESIAN_POINT ( 'NONE',  ( 0.3412290553763823175, 0.3797058362894656369, 2.173699509851903855 ) ) ;
#37313 = CARTESIAN_POINT ( 'NONE',  ( 1.495402192688908727, 8.717956978849549898, 2.557532308801792720 ) ) ;
#37314 = CARTESIAN_POINT ( 'NONE',  ( 6.217445370822936468, 1.674971474680493788, 1.116412877057591624 ) ) ;
#37315 = CARTESIAN_POINT ( 'NONE',  ( -0.02319159430949797526, 7.629137130509074716, -2.410989586153565067 ) ) ;
#37316 = CARTESIAN_POINT ( 'NONE',  ( -0.05740707158673791916, 15.49542554636510339, 11.99731162103223525 ) ) ;
#37317 = CARTESIAN_POINT ( 'NONE',  ( -6.645879322773616593, -6.896483513897168294, -6.785280070212523107 ) ) ;
#37318 = CARTESIAN_POINT ( 'NONE',  ( 2.611853368047814872, 0.5545374748289233491, -1.994631108499920646 ) ) ;
#37319 = CARTESIAN_POINT ( 'NONE',  ( -3.913499895838973508, 7.717500311787445000, 1.040834085586084257E-14 ) ) ;
#37320 = CIRCLE ( 'NONE', #182655, 0.07999999999999994615 ) ;
#37321 = CARTESIAN_POINT ( 'NONE',  ( -4.610539993796915148, 8.375707290415371986, 0.1689211187793551172 ) ) ;
#37323 = CARTESIAN_POINT ( 'NONE',  ( 0.6730137850648570952, -2.035850703004048246, -0.7271551459356735414 ) ) ;
#37322 = CARTESIAN_POINT ( 'NONE',  ( -4.874319919312905647, 5.645460313075203018, -1.199719254218446718 ) ) ;
#37324 = CARTESIAN_POINT ( 'NONE',  ( 6.938893903907228378E-15, 10.64264068711930733, 1.214306433183764966E-14 ) ) ;
#37325 = SURFACE_SIDE_STYLE ('',( #54645 ) ) ;
#37326 = CARTESIAN_POINT ( 'NONE',  ( 0.000000000000000000, 0.000000000000000000, 9.579665964948883783 ) ) ;
#37327 = EDGE_CURVE ( 'NONE', #155586, #195844, #94874, .T. ) ;
#37328 = CARTESIAN_POINT ( 'NONE',  ( 0.6823417656249934904, 13.50520833367473195, 1.181850606188764807 ) ) ;
#37330 = CARTESIAN_POINT ( 'NONE',  ( -5.794130544993808307, 7.853181283949808744, 1.599625672291263179 ) ) ;
#37329 = CARTESIAN_POINT ( 'NONE',  ( 6.825078400183582694, 7.052760558784821221, 2.553807217019073761 ) ) ;
#37331 = CARTESIAN_POINT ( 'NONE',  ( 5.643113243286411063, 0.7107029072939261560, 1.582047324045066095 ) ) ;
#37332 = CARTESIAN_POINT ( 'NONE',  ( -3.469997250093771246, 6.135748327496311383, -1.199719254218452935 ) ) ;
#37334 = CIRCLE ( 'NONE', #158420, 0.5000000000000004441 ) ;
#37333 = CONICAL_SURFACE ( 'NONE', #9653, 11.53746066217573762, 0.1181278931043537039 ) ;
#37335 = CARTESIAN_POINT ( 'NONE',  ( 3.661042849074844785, 1.635018244968543977, -1.269851595989857085 ) ) ;
#37336 = CARTESIAN_POINT ( 'NONE',  ( 4.112992273575425628, 0.1058706520744826102, 2.114715381611050660 ) ) ;
#37337 = CARTESIAN_POINT ( 'NONE',  ( 8.260995669428309540, 8.532249790621511565, 0.7998128361456481317 ) ) ;
#37338 = CARTESIAN_POINT ( 'NONE',  ( 0.6823417656249899377, 4.426041667008086655, -1.181850606188754593 ) ) ;
#37339 = CARTESIAN_POINT ( 'NONE',  ( 2.711712322018722698, 0.5300763513187057852, -1.896665901777684127 ) ) ;
#37340 = CARTESIAN_POINT ( 'NONE',  ( 0.8965662283535699162, -1.866366896104875162, -0.4163465257057268332 ) ) ;
#37341 = CARTESIAN_POINT ( 'NONE',  ( 4.875077803184670877, 2.140050280577758812, -0.8218066810307764758 ) ) ;
#37342 = CARTESIAN_POINT ( 'NONE',  ( 3.281694405262673087, 1.158851912627656189, 1.410738560442346801 ) ) ;
#37343 = CARTESIAN_POINT ( 'NONE',  ( 5.713835393516482952, 5.630839145382857680, 0.7998128361456352531 ) ) ;
#37344 = CARTESIAN_POINT ( 'NONE',  ( 6.792271770322100721, 7.026664608238323950, -0.7216878364870257245 ) ) ;
#37345 = CARTESIAN_POINT ( 'NONE',  ( -5.371001409308059138, 9.417918744168066070, -0.7998128361456231517 ) ) ;
#37346 = CARTESIAN_POINT ( 'NONE',  ( 3.920185232657522167, -2.007512044478755531, 0.1524921764288286741 ) ) ;
#37347 = CARTESIAN_POINT ( 'NONE',  ( 2.922649740298603138, -1.356309479035762378, 1.417576456850026867 ) ) ;
#37348 = CARTESIAN_POINT ( 'NONE',  ( -6.723954117373590833, 9.932031339322813679, -1.199719254218440723 ) ) ;
#37349 = CARTESIAN_POINT ( 'NONE',  ( -4.577849422908604637, 8.492574760035358494, -0.7998128361456281477 ) ) ;
#37350 = CYLINDRICAL_SURFACE ( 'NONE', #67917, 0.7500000000000011102 ) ;
#37352 = CARTESIAN_POINT ( 'NONE',  ( 4.539784583036060361, 0.7555593814247036910, -1.600612801534553542 ) ) ;
#37351 = CARTESIAN_POINT ( 'NONE',  ( 6.615180898807764720, -2.028213694748048024, 0.5066274125750843682 ) ) ;
#37353 = CARTESIAN_POINT ( 'NONE',  ( 1.499999999999822586, 7.388542872122531691, 4.154462424328221104 ) ) ;
#37354 = CARTESIAN_POINT ( 'NONE',  ( 0.7795418844130063141, 1.474435645617519164, 1.621430000501473900 ) ) ;
#37355 = CARTESIAN_POINT ( 'NONE',  ( 0.1337851541256071808, 0.2942392587969425155, 1.715217768732644643 ) ) ;
#37356 = CARTESIAN_POINT ( 'NONE',  ( 6.913768267964901071, 10.15348118167935709, -1.199719254218441611 ) ) ;
#37357 = CARTESIAN_POINT ( 'NONE',  ( 1.394453263437886604E-15, -1.312499999999999556, 3.474999999999999645 ) ) ;
#37358 = CARTESIAN_POINT ( 'NONE',  ( 0.8787516259003292918, -0.3353366030727308877, 2.273710652787809039 ) ) ;
#37359 = CARTESIAN_POINT ( 'NONE',  ( 0.3104468679729632807, 1.506874830639578056, -1.591553791636945991 ) ) ;
#37360 = CARTESIAN_POINT ( 'NONE',  ( 6.714187037452940210, -1.395258515317991943, -1.029009966057025549 ) ) ;
#37361 = CARTESIAN_POINT ( 'NONE',  ( 3.492985898914053866, -0.4302566696539159574, -2.164365734511737305 ) ) ;
#37362 = AXIS2_PLACEMENT_3D ( 'NONE', #107032, #173058, #75543 ) ;
#37363 = CARTESIAN_POINT ( 'NONE',  ( 6.461400869420954152, 1.801464151850284301, 1.211653227174382952 ) ) ;
#37364 = CARTESIAN_POINT ( 'NONE',  ( 1.710321574826153324, 1.214426542090217609, -1.734289745093554380 ) ) ;
#37365 = CARTESIAN_POINT ( 'NONE',  ( 4.062500000000002665, -1.451031289061280205, -1.451031289060952467 ) ) ;
#37366 = CARTESIAN_POINT ( 'NONE',  ( 6.620655732516642189, 2.417337544263608251, 2.554705107920357321 ) ) ;
#37367 = CARTESIAN_POINT ( 'NONE',  ( 4.963854806921006002, 1.905440169433350484, -0.2825122895667788181 ) ) ;
#37368 = EDGE_LOOP ( 'NONE', ( #47876, #84195, #192, #37905 ) ) ;
#37370 = CARTESIAN_POINT ( 'NONE',  ( 1.499999999999990896, 5.275000000000022560, 1.214306433183764966E-14 ) ) ;
#37369 = CARTESIAN_POINT ( 'NONE',  ( 1.048812564444784989, -1.803156034432966681, 1.415383320267731726 ) ) ;
#37371 = CARTESIAN_POINT ( 'NONE',  ( 4.172158584703322681, 5.890604320285754980, -1.599625672291256295 ) ) ;
#37372 = CARTESIAN_POINT ( 'NONE',  ( 5.952193131599331721, 6.902979060742733708, 1.199719254218462483 ) ) ;
#37373 = VECTOR ( 'NONE', #35690, 1000.000000000000000 ) ;
#37374 = CARTESIAN_POINT ( 'NONE',  ( 4.073042245396302441, -1.645747789204109468, 1.492029542161198430 ) ) ;
#37375 = CARTESIAN_POINT ( 'NONE',  ( -6.887178846062105286, 10.97886638714038554, -0.7216878364870267237 ) ) ;
#37376 = FILL_AREA_STYLE_COLOUR ( '', #11471 ) ;
#37377 = CARTESIAN_POINT ( 'NONE',  ( 6.643132081016125845, 6.852668304048034287, 0.7216878364870317197 ) ) ;
#37378 = CARTESIAN_POINT ( 'NONE',  ( -7.144783764277399030, 11.27940545839156528, 0.7216878364870458196 ) ) ;
#37379 = CARTESIAN_POINT ( 'NONE',  ( 6.211043768836181478, 7.379210830797944709, 1.082531754730549967 ) ) ;
#37380 = CARTESIAN_POINT ( 'NONE',  ( 2.162732623366144136, 1.242727809108796322, 1.587836805404294171 ) ) ;
#37382 = CARTESIAN_POINT ( 'NONE',  ( 6.373490837812130216, -0.2564121905142978664, 2.046633738985944806 ) ) ;
#37381 = CARTESIAN_POINT ( 'NONE',  ( 6.428537391173986038, 10.65171072301167854, 0.7998128361456462443 ) ) ;
#37383 = DIRECTION ( 'NONE',  ( 0.000000000000000000, 1.000000000000000000, 0.000000000000000000 ) ) ;
#37384 = CARTESIAN_POINT ( 'NONE',  ( 6.522881301506172846, 6.782652071278222117, -0.7216878364870458196 ) ) ;
#37385 = CARTESIAN_POINT ( 'NONE',  ( 6.251467208264422482, 1.735085017428819931, -0.1376019381845137446 ) ) ;
#37386 = CARTESIAN_POINT ( 'NONE',  ( 4.161989969715248705, 4.726297878971393196, -2.500000000000000444 ) ) ;
#37387 = CARTESIAN_POINT ( 'NONE',  ( -1.364683531250012516, 2.488541667008088876, -0.7879004041258289570 ) ) ;
#37388 = CARTESIAN_POINT ( 'NONE',  ( 2.547821756505376012, 1.769265940657601011, 0.04812675368598590825 ) ) ;
#37389 = CARTESIAN_POINT ( 'NONE',  ( 1.213517774399593740, 1.944071949784083264, 0.5350861613380719639 ) ) ;
#37390 = CARTESIAN_POINT ( 'NONE',  ( -0.1237769027084348328, -0.1346504581853508187, -1.811164470923332104 ) ) ;
#37391 = CARTESIAN_POINT ( 'NONE',  ( 4.933284685991359275, -1.619851263076008019, -1.622297632854825755 ) ) ;
#37392 = CARTESIAN_POINT ( 'NONE',  ( 3.363068133243895197, 1.796009578954290253, -0.4044003374430102382 ) ) ;
#37393 = CARTESIAN_POINT ( 'NONE',  ( 7.235247531187115833, 11.59287255302699648, -0.7998128361456291469 ) ) ;
#37394 = CARTESIAN_POINT ( 'NONE',  ( 3.715676801689533626, -1.798647723735953496, 0.3114480851732701061 ) ) ;
#37395 = CARTESIAN_POINT ( 'NONE',  ( 5.098279808040273586, -0.2930726886911338425, 1.994869512123042199 ) ) ;
#37396 = CARTESIAN_POINT ( 'NONE',  ( -9.664264568442742842, 10.16939683947169115, -0.7998128361456291469 ) ) ;
#37398 = CARTESIAN_POINT ( 'NONE',  ( -7.228432174741334038, 8.462200954400218578, -1.199719254218452047 ) ) ;
#37397 = CARTESIAN_POINT ( 'NONE',  ( 3.538171838403024516, 1.019457259465136101, -2.019903332531754803 ) ) ;
#37399 = CARTESIAN_POINT ( 'NONE',  ( 6.440466061264603859, 2.082495663875443714, 0.3126870252899079938 ) ) ;
#37400 = CARTESIAN_POINT ( 'NONE',  ( -0.4000000000000496492, 3.372708439410135206, 0.4999999999999483746 ) ) ;
#37401 =( BOUNDED_CURVE ( )  B_SPLINE_CURVE ( 2, ( #24616, #41977, #56073 ),
 .UNSPECIFIED., .F., .T. ) 
 B_SPLINE_CURVE_WITH_KNOTS ( ( 3, 3 ),
 ( 0.000000000000000000, 0.002220828379238361412 ),
 .UNSPECIFIED. ) 
 CURVE ( )  GEOMETRIC_REPRESENTATION_ITEM ( )  RATIONAL_B_SPLINE_CURVE ( ( 1.000000000000000000, 0.9285916995105953919, 0.9333044775364149892 ) ) 
 REPRESENTATION_ITEM ( '' )  );
#37402 = CARTESIAN_POINT ( 'NONE',  ( 3.191909353267761151, -1.388477207968623839, -1.535938721777901472 ) ) ;
#37403 = CARTESIAN_POINT ( 'NONE',  ( 8.866142388332804103, 12.43125098877526113, -1.199719254218446718 ) ) ;
#37404 = CARTESIAN_POINT ( 'NONE',  ( 1.360316468750004448, 2.546875000341383810, -3.295974604355933479E-14 ) ) ;
#37405 = CARTESIAN_POINT ( 'NONE',  ( 6.340501840829311675, 1.221348521443364143, -1.733245716811770087 ) ) ;
#37406 = SHAPE_DEFINITION_REPRESENTATION ( #148873, #84563 ) ;
#37408 = CARTESIAN_POINT ( 'NONE',  ( 1.805176890173798565, 1.601487618425012638, 1.070529213009919101 ) ) ;
#37407 = CARTESIAN_POINT ( 'NONE',  ( -8.859363311525973117, 12.42334206583395328, -1.199719254218446718 ) ) ;
#37409 = CARTESIAN_POINT ( 'NONE',  ( -5.015590482412729756, 4.816220082428420923, 0.000000000000000000 ) ) ;
#37410 = CARTESIAN_POINT ( 'NONE',  ( 6.403175662787183420, -1.665661181276241853, 1.050507712364300072 ) ) ;
#37411 = CARTESIAN_POINT ( 'NONE',  ( 4.760321331729593375, 5.686701320840210627, -1.082531754730548412 ) ) ;
#37412 = CARTESIAN_POINT ( 'NONE',  ( 5.639205186016292615, 6.133955845365204773, 0.8069632701028349731 ) ) ;
#37413 = CARTESIAN_POINT ( 'NONE',  ( 2.609770642201842072, -0.3830433331901555993, -0.1872689674646474400 ) ) ;
#37414 = CARTESIAN_POINT ( 'NONE',  ( -4.172158584703340445, 5.890604320285754980, -1.599625672291256295 ) ) ;
#37415 = CARTESIAN_POINT ( 'NONE',  ( 0.8970957097632881183, -2.168902827774013442, -0.4795612232612302961 ) ) ;
#37416 = CARTESIAN_POINT ( 'NONE',  ( 3.680784645728672810, -2.029037780879865416, -0.5636793167548505012 ) ) ;
#37417 = CARTESIAN_POINT ( 'NONE',  ( -4.655245641445871385, 6.524482229810530498, 1.599625672291263179 ) ) ;
#37418 = CARTESIAN_POINT ( 'NONE',  ( 6.262976894508937242, 9.394224579314053969, -1.199719254218440723 ) ) ;
#37419 = CARTESIAN_POINT ( 'NONE',  ( 0.7833917827068856976, -1.768883884249613736, 0.5786898513908571573 ) ) ;
#37420 = CARTESIAN_POINT ( 'NONE',  ( 5.612185521052973414, 8.634967976948757951, -1.199719254218440723 ) ) ;
#37421 = CARTESIAN_POINT ( 'NONE',  ( 3.811813743736467419, 7.598866467667865443, 1.040834085586084257E-14 ) ) ;
#37422 = CARTESIAN_POINT ( 'NONE',  ( -6.373741612200205076, 8.529394195690610303, 1.443375672974064550 ) ) ;
#37423 = CARTESIAN_POINT ( 'NONE',  ( -7.537970219518083326, 9.817384560903001045, -1.443375672974059665 ) ) ;
#37424 = CARTESIAN_POINT ( 'NONE',  ( 0.9320672075895162223, -2.067649466203642206, 0.4702014512557165515 ) ) ;
#37425 = DIRECTION ( 'NONE',  ( 0.000000000000000000, 0.000000000000000000, -1.000000000000000000 ) ) ;
#37427 = CARTESIAN_POINT ( 'NONE',  ( 4.000408739481801312, 1.952204270133122810, 0.1946113827649766925 ) ) ;
#37426 = CARTESIAN_POINT ( 'NONE',  ( -2.553934817853170728E-14, 0.1875000000000329459, -1.414508159514617391 ) ) ;
#37428 = CARTESIAN_POINT ( 'NONE',  ( 1.604591590977550108, -0.7782141685120853580, -2.016947388195994062 ) ) ;
#37429 = CARTESIAN_POINT ( 'NONE',  ( 2.261056740009634414, 1.805359621025553363, -0.3608742708730780513 ) ) ;
#37431 = CARTESIAN_POINT ( 'NONE',  ( -5.704936041347759001, 6.126156357109620032, -0.7369488182252960096 ) ) ;
#37430 = CARTESIAN_POINT ( 'NONE',  ( -2.810282979782591006, 6.500690253046801814, 0.000000000000000000 ) ) ;
#37432 = CARTESIAN_POINT ( 'NONE',  ( 3.433312839113885850, 0.7810296162102482453, -1.555295924109141303 ) ) ;
#37434 = COLOUR_RGB ( '', 0.31764706, 0.68627451, 0.89019608) ;
#37433 = CARTESIAN_POINT ( 'NONE',  ( 4.036703073083682369, 7.757870032734638599, 0.4269520307091502209 ) ) ;
#37435 = CARTESIAN_POINT ( 'NONE',  ( 5.341549334104188418, 7.254893527920112994, 1.443375672974062551 ) ) ;
#37436 = CARTESIAN_POINT ( 'NONE',  ( -10.71030397718323890, 6.055815897892919075, -4.668189396100475008 ) ) ;
#37437 = CARTESIAN_POINT ( 'NONE',  ( 0.5851287433712646369, -0.2658872486876809327, -2.145209338178376335 ) ) ;
#37438 = CARTESIAN_POINT ( 'NONE',  ( 3.743517394402117837, -1.942243990624907823, -0.5404084370827856310 ) ) ;
#37439 = CARTESIAN_POINT ( 'NONE',  ( 5.346851039111029991, 6.199209027673978412, 7.500000000000000000 ) ) ;
#37440 = CARTESIAN_POINT ( 'NONE',  ( -3.902768115887413014, 5.646591783325653147, -1.599625672291283607 ) ) ;
#37441 = CARTESIAN_POINT ( 'NONE',  ( 3.256668630020958410, -1.493913901992610205, 1.286540209188108630 ) ) ;
#37442 = CARTESIAN_POINT ( 'NONE',  ( 6.509000000000021657, 1.267728212239338959, 2.115804336118334295 ) ) ;
#37443 = CARTESIAN_POINT ( 'NONE',  ( 2.524863302051027159, -1.811236869417539141, 0.7011504990855742525 ) ) ;
#37446 = ORIENTED_EDGE ( 'NONE', *, *, #163845, .T. ) ;
#37445 = CARTESIAN_POINT ( 'NONE',  ( -5.316205630334276400, 5.374863788244313767, -0.7216878364870338292 ) ) ;
#37444 = CARTESIAN_POINT ( 'NONE',  ( 6.451426615364327155, -1.705040744490589066, 0.8662930942644477827 ) ) ;
#37447 = CARTESIAN_POINT ( 'NONE',  ( -5.763624699140894592, 5.896852701852039580, -0.7216878364870338292 ) ) ;
#37448 = CARTESIAN_POINT ( 'NONE',  ( 5.747730777550676073, 5.670383760089384495, 0.000000000000000000 ) ) ;
#37449 = CARTESIAN_POINT ( 'NONE',  ( -3.657667580636712934, 7.489305620709952649, -0.7998128361456481317 ) ) ;
#37450 = CARTESIAN_POINT ( 'NONE',  ( -7.456058132872594335, 7.663432341298296535, 0.000000000000000000 ) ) ;
#37451 = CARTESIAN_POINT ( 'NONE',  ( -7.971831134711019118, 12.24429405723079967, 0.000000000000000000 ) ) ;
#37452 = CARTESIAN_POINT ( 'NONE',  ( 0.3939699847536023980, 1.636818068892214040, 1.480257586202008646 ) ) ;
#37453 = CARTESIAN_POINT ( 'NONE',  ( -3.285556943749998737, -3.230208332855375897, 1.896917185911908499 ) ) ;
#37454 = CARTESIAN_POINT ( 'NONE',  ( 4.012515129279304205, 0.7020173944642660313, 1.832041770129029468 ) ) ;
#37455 = CARTESIAN_POINT ( 'NONE',  ( 9.094822116668764167, 9.505047312402055582, 0.7998128361456462443 ) ) ;
#37456 = CARTESIAN_POINT ( 'NONE',  ( 1.670546294658280084, 1.392546765991018454, 1.458555661489918442 ) ) ;
#37457 = VERTEX_POINT ( 'NONE', #207808 ) ;
#37458 = CARTESIAN_POINT ( 'NONE',  ( 2.325544253341553347, -1.572509993196508971, -1.418087145738779808 ) ) ;
#37459 = CARTESIAN_POINT ( 'NONE',  ( -1.500000000000013101, 2.160416667349489561, -0.8660254037844313801 ) ) ;
#37461 = CARTESIAN_POINT ( 'NONE',  ( -6.013204822860843457, 6.974159367214481264, -1.199719254218446718 ) ) ;
#37460 = CARTESIAN_POINT ( 'NONE',  ( -4.308793891044708779, 3.921347715840572956, 1.214306433183764966E-14 ) ) ;
#37462 = CARTESIAN_POINT ( 'NONE',  ( 3.626748959588219634, -1.700609458330613055, 0.7059681596332522124 ) ) ;
#37463 = ORIENTED_EDGE ( 'NONE', *, *, #68847, .F. ) ;
#37464 = CARTESIAN_POINT ( 'NONE',  ( -9.169391961543940539, 9.592045464756413509, 1.040834085586084257E-14 ) ) ;
#37465 = PRESENTATION_STYLE_ASSIGNMENT (( #185834 ) ) ;
#37467 = EDGE_CURVE ( 'NONE', #180436, #115335, #190491, .T. ) ;
#37466 = CARTESIAN_POINT ( 'NONE',  ( 4.623349522974431025, 1.846400237221163865, 1.042759738753673338 ) ) ;
#37468 = CARTESIAN_POINT ( 'NONE',  ( -10.38614328979765489, 3.507114751586604129, -5.996442624206661520 ) ) ;
#37469 = CARTESIAN_POINT ( 'NONE',  ( 7.949158136313996259, 8.168439335321471262, 1.040834085586084257E-14 ) ) ;
#37470 = CARTESIAN_POINT ( 'NONE',  ( 4.956353021003493176, 0.7848952607251434843, 1.905660951107574608 ) ) ;
#37472 = CARTESIAN_POINT ( 'NONE',  ( 2.911469271472226339, -0.9098125248445630975, -1.600700954789348263 ) ) ;
#37471 = CARTESIAN_POINT ( 'NONE',  ( -6.039267359883488950, 9.133230122250985517, 1.199719254218452047 ) ) ;
#37473 = CARTESIAN_POINT ( 'NONE',  ( 8.127223016387999266, 11.56917838817298616, 1.199719254218460707 ) ) ;
#37474 = CARTESIAN_POINT ( 'NONE',  ( -1.364683531250010295, 5.488541667008087543, -0.7879004041258300672 ) ) ;
#37475 = FILL_AREA_STYLE ('',( #119864 ) ) ;
#37476 = CARTESIAN_POINT ( 'NONE',  ( -4.837049282416619356, 5.053169767094015441, -0.9039271902641244916 ) ) ;
#37477 = DIRECTION ( 'NONE',  ( 0.000000000000000000, -1.000000000000000000, 0.000000000000000000 ) ) ;
#37478 = MECHANICAL_DESIGN_GEOMETRIC_PRESENTATION_REPRESENTATION (  '', ( #137691 ), #16738 ) ;
#37479 = CARTESIAN_POINT ( 'NONE',  ( 1.858336453454629611, 2.200810804183956026, -0.1644699235988852648 ) ) ;
#37480 = CARTESIAN_POINT ( 'NONE',  ( 3.831548730252303248, -2.092150397999822165, 0.8615055239265239084 ) ) ;
#37481 = CARTESIAN_POINT ( 'NONE',  ( -8.541273586929371220, 9.067166727613487964, 0.7216878364870438212 ) ) ;
#37482 = CARTESIAN_POINT ( 'NONE',  ( 3.621195883455626596, 1.556580008595293219, 0.9264731596013916493 ) ) ;
#37483 = CARTESIAN_POINT ( 'NONE',  ( 4.047977829471119726, 0.9080738158676031624, 1.686857792009839097 ) ) ;
#37484 = CARTESIAN_POINT ( 'NONE',  ( -0.6823417656250212460, 4.613541667008086655, 1.181850606188767472 ) ) ;
#37485 = CARTESIAN_POINT ( 'NONE',  ( 4.118015666179648093, -1.012585719757435498, -1.691412322542594326 ) ) ;
#37486 = CARTESIAN_POINT ( 'NONE',  ( 1.448133341116746964, 1.924057924963176180, 0.09734726817032554602 ) ) ;
#37487 = CARTESIAN_POINT ( 'NONE',  ( 4.539837415608827698, 0.7997722286730184482, -1.691214532891088362 ) ) ;
#37488 = CARTESIAN_POINT ( 'NONE',  ( 3.264621958926614109, 1.037573782609865436, 2.061359394274730583 ) ) ;
#37489 = CARTESIAN_POINT ( 'NONE',  ( 4.510102262511601623, 1.860682779278443277, -0.04454786357706643635 ) ) ;
#37490 = CARTESIAN_POINT ( 'NONE',  ( -1.001543065824772872E-14, 5.071875000341421469, 1.575800808251672791 ) ) ;
#37492 = AXIS2_PLACEMENT_3D ( 'NONE', #114066, #28467, #160601 ) ;
#37491 = VECTOR ( 'NONE', #37512, 1000.000000000000114 ) ;
#37493 = CARTESIAN_POINT ( 'NONE',  ( 0.3039231887648624619, -1.082844287645868375, -1.700959134490941160 ) ) ;
#37494 = EDGE_CURVE ( 'NONE', #65102, #70481, #168799, .T. ) ;
#37496 = CARTESIAN_POINT ( 'NONE',  ( 1.629656122859889811, -1.982562362509328047, 0.7109879831135539341 ) ) ;
#37495 = CARTESIAN_POINT ( 'NONE',  ( -4.921246571636213929, 4.843801876438091902, 0.7216878364870317197 ) ) ;
#37497 = CARTESIAN_POINT ( 'NONE',  ( 3.890826896997583884, 4.602014803661035103, -1.082531754730543083 ) ) ;
#37499 = CARTESIAN_POINT ( 'NONE',  ( 0.000000000000000000, -1.000000000000000888, 0.000000000000000000 ) ) ;
#37498 = CARTESIAN_POINT ( 'NONE',  ( -1.364683531249997417, 5.071875000341417916, 1.214306433183764966E-14 ) ) ;
#37500 = CARTESIAN_POINT ( 'NONE',  ( 2.742561299210785286, 1.174483946500170184, -1.765453564165630596 ) ) ;
#37501 = DIRECTION ( 'NONE',  ( -0.7071067811865489050, 0.000000000000000000, -0.7071067811865462405 ) ) ;
#37502 = CARTESIAN_POINT ( 'NONE',  ( 0.7737015921927943296, 0.3898077916253924746, -1.981631471940727973 ) ) ;
#37503 = CARTESIAN_POINT ( 'NONE',  ( 0.6823417656249882723, 1.176041667008083325, -1.181850606188749264 ) ) ;
#37504 = CARTESIAN_POINT ( 'NONE',  ( -2.819732761962332024, 6.233512622357263666, -0.7216878364870267237 ) ) ;
#37505 = CARTESIAN_POINT ( 'NONE',  ( 4.449046963578762615, 8.342305224150557308, -0.7998128361456231517 ) ) ;
#37506 = ORIENTED_EDGE ( 'NONE', *, *, #188015, .T. ) ;
#37507 = CARTESIAN_POINT ( 'NONE',  ( 2.442841770826277958, 0.4709965094221583159, 2.109507199432036018 ) ) ;
#37508 = CARTESIAN_POINT ( 'NONE',  ( 4.311129659465574804, 7.013106455143060636, -1.082531754730548412 ) ) ;
#37511 = CARTESIAN_POINT ( 'NONE',  ( -3.921423297084331239, 8.995353878514519508, -0.7749999999999979128 ) ) ;
#37510 = CARTESIAN_POINT ( 'NONE',  ( 6.925078400183531713, 2.446544591822760850, 2.338552149501707422 ) ) ;
#37509 = CARTESIAN_POINT ( 'NONE',  ( 6.235824307642648279, 6.239826211863360506, 0.000000000000000000 ) ) ;
#37512 = DIRECTION ( 'NONE',  ( 0.7592566023653004592, -0.6507913734559639396, 0.000000000000000000 ) ) ;
#37513 = CARTESIAN_POINT ( 'NONE',  ( 5.524625123954316486, 0.3981063221985549072, 1.976670730632006601 ) ) ;
#37514 = CARTESIAN_POINT ( 'NONE',  ( -7.971831135155409420, 11.28392484344787405, 1.082531754730549967 ) ) ;
#37515 = CARTESIAN_POINT ( 'NONE',  ( 0.2752733618501881363, 2.042644424557562122, -0.7945232813236638991 ) ) ;
#37516 = CARTESIAN_POINT ( 'NONE',  ( -0.4645879757425588341, -7.605490376146412324, -10.08385597498927488 ) ) ;
#37518 = CARTESIAN_POINT ( 'NONE',  ( -1.364683531250000748, 11.35937500034139802, 0.000000000000000000 ) ) ;
#37517 = CARTESIAN_POINT ( 'NONE',  ( 0.6907310396802420760, -2.245820052064306349, -0.2739839911451089627 ) ) ;
#37519 = CARTESIAN_POINT ( 'NONE',  ( -9.104463846776669200, 10.58062822844965645, -1.199719254218441611 ) ) ;
#37520 = CARTESIAN_POINT ( 'NONE',  ( -4.975479186090865369, 6.827811688571220117, 1.443375672974064550 ) ) ;
#37521 = CARTESIAN_POINT ( 'NONE',  ( -0.6823417656250003738, 1.780208333674752952, -1.181850606188749264 ) ) ;
#37522 = CARTESIAN_POINT ( 'NONE',  ( 1.500000000000001332, 9.375000000000001776, 0.000000000000000000 ) ) ;
#37523 = CARTESIAN_POINT ( 'NONE',  ( -1.402160292154681736E-14, 10.06249999999999822, 1.732050807568881190 ) ) ;
#37524 = CARTESIAN_POINT ( 'NONE',  ( 4.160587402808674007, -1.276020550970466516, 1.160787852381778062 ) ) ;
#37525 = CARTESIAN_POINT ( 'NONE',  ( 4.179656494762836516, 8.098292687190454586, -0.7998128361456362523 ) ) ;
#37526 = CARTESIAN_POINT ( 'NONE',  ( 1.580939025779507956, 1.637719487297364163, -0.6712238910871449749 ) ) ;
#37527 = CARTESIAN_POINT ( 'NONE',  ( 2.824860481609407614, 1.456601328488495106, -1.389772560336500318 ) ) ;
#37528 = CARTESIAN_POINT ( 'NONE',  ( 4.788207028248289809, -1.043783763870303360, 1.944324211313207318 ) ) ;
#37529 = ORIENTED_EDGE ( 'NONE', *, *, #120145, .F. ) ;
#37530 = CARTESIAN_POINT ( 'NONE',  ( 4.236585392707596043, 1.239412559483305198, -1.594744479876673005 ) ) ;
#37531 = CARTESIAN_POINT ( 'NONE',  ( -7.774674742793745708, 8.035151719539642912, 0.7998128361456341429 ) ) ;
#37533 = CARTESIAN_POINT ( 'NONE',  ( 4.569935513796226978, -0.9480243344661150040, 1.779636403143824985 ) ) ;
#37532 = CARTESIAN_POINT ( 'NONE',  ( 4.512424090126602394, -2.120028616272570332, -0.05109941365945279423 ) ) ;
#37534 = VERTEX_POINT ( 'NONE', #156958 ) ;
#37535 = CARTESIAN_POINT ( 'NONE',  ( 5.083381250481017410, 4.895309311841474553, 0.7998128361456352531 ) ) ;
#37536 = AXIS2_PLACEMENT_3D ( 'NONE', #148434, #66067, #166809 ) ;
#37537 = ORIENTED_EDGE ( 'NONE', *, *, #178413, .T. ) ;
#37538 = CARTESIAN_POINT ( 'NONE',  ( 1.955717210371358483, 1.865846021326333926, -0.1348392221205765851 ) ) ;
#37539 = CARTESIAN_POINT ( 'NONE',  ( -10.39230484541323563, 3.038454817776168770, 6.000000000000048850 ) ) ;
#37540 = CARTESIAN_POINT ( 'NONE',  ( 6.199861008060345569, 1.254605797456327831, 1.306922710324806225 ) ) ;
#37541 = DIRECTION ( 'NONE',  ( 9.436895709313856232E-16, -0.8656921114426506803, -0.5005768354468324022 ) ) ;
#37542 = CARTESIAN_POINT ( 'NONE',  ( -10.12724049293007766, 3.240713040256745003, -5.870485300885818880 ) ) ;
#37543 = FACE_OUTER_BOUND ( 'NONE', #206984, .T. ) ;
#37544 = CARTESIAN_POINT ( 'NONE',  ( -1.201851678989727383E-14, 3.259375000341420581, -1.575800808251660134 ) ) ;
#37545 = CARTESIAN_POINT ( 'NONE',  ( -0.2108831679770960255, -0.001785917861228669690, -1.896958272444612792 ) ) ;
#37546 = CARTESIAN_POINT ( 'NONE',  ( 4.394251184604957672, 8.140727125432173139, -0.7216878364870357165 ) ) ;
#37547 = CARTESIAN_POINT ( 'NONE',  ( 1.873419974815058842, -0.2433403713097622156, 1.946663811685337420 ) ) ;
#37548 = CARTESIAN_POINT ( 'NONE',  ( -5.180624094197616714, 5.216685329418210948, 0.7216878364870257245 ) ) ;
#37549 = CARTESIAN_POINT ( 'NONE',  ( -5.448397627845328550, 7.449826213943242514, 1.599625672291263179 ) ) ;
#37550 = CARTESIAN_POINT ( 'NONE',  ( 3.920270587443939636, -2.114697630030224929, 0.1593259359235904837 ) ) ;
#37552 = CARTESIAN_POINT ( 'NONE',  ( -10.57232898948313604, 5.599354254162436817, 4.968808419985093039 ) ) ;
#37551 = CARTESIAN_POINT ( 'NONE',  ( 10.23370702021670020, 10.83374636654133383, 0.7998128361456462443 ) ) ;
#37553 = CARTESIAN_POINT ( 'NONE',  ( 5.026621361268301946, 1.885657091993764745, 0.5748499752153258813 ) ) ;
#37554 = CARTESIAN_POINT ( 'NONE',  ( -1.364683531250014514, 1.488541667008084435, -0.7879004041258289570 ) ) ;
#37555 = CARTESIAN_POINT ( 'NONE',  ( 0.8088407350804104334, -0.4930801656862683346, -1.951752914270672212 ) ) ;
#37556 = ORIENTED_EDGE ( 'NONE', *, *, #158769, .F. ) ;
#37557 = CARTESIAN_POINT ( 'NONE',  ( 0.8786900280967164800, -0.5185874880111912555, -2.052613615991748297 ) ) ;
#37558 = CARTESIAN_POINT ( 'NONE',  ( 11.83847906649667436, 6.805419798594589231, -1.976859043548241823 ) ) ;
#37559 = CARTESIAN_POINT ( 'NONE',  ( 3.086448098943677998, 1.152334561581969785, -1.719836228861029603 ) ) ;
#37560 = ORIENTED_EDGE ( 'NONE', *, *, #113892, .T. ) ;
#37561 = CARTESIAN_POINT ( 'NONE',  ( 4.634908411025333130, 6.500755460986618495, 1.599625672291268286 ) ) ;
#37562 = CARTESIAN_POINT ( 'NONE',  ( 5.682802662783380754, 6.658966523782627434, 1.199719254218452935 ) ) ;
#37563 = VERTEX_POINT ( 'NONE', #26925 ) ;
#37565 = CARTESIAN_POINT ( 'NONE',  ( 5.494078562035752178, 7.432844293840273231, -1.599625672291262513 ) ) ;
#37564 = CARTESIAN_POINT ( 'NONE',  ( 4.998031443873323099, -0.7039345487453112504, -1.968691415026160962 ) ) ;
#37568 = ORIENTED_EDGE ( 'NONE', *, *, #8637, .T. ) ;
#37567 = CARTESIAN_POINT ( 'NONE',  ( 1.576514528963068429, -1.280961997807128938, 1.281107859597712118 ) ) ;
#37566 = CARTESIAN_POINT ( 'NONE',  ( 3.627796970749700201, -1.086779551322129445, -1.466705181690882709 ) ) ;
#37569 = CARTESIAN_POINT ( 'NONE',  ( -11.07790593930098311, 13.79999999999999893, -0.7000000000000009548 ) ) ;
#37570 = CARTESIAN_POINT ( 'NONE',  ( 8.916922505737264970, 12.80282292485108186, 7.559592800977426919 ) ) ;
#37571 = CARTESIAN_POINT ( 'NONE',  ( 4.208205882762393379, -2.201082536721191474, 0.1591639695062776749 ) ) ;
#37572 = CARTESIAN_POINT ( 'NONE',  ( 6.272618624616828953, 10.46980549536166016, 1.040834085586084257E-14 ) ) ;
#37573 = CARTESIAN_POINT ( 'NONE',  ( 1.364683531250000748, 9.817708333674737275, -0.7879004041258355073 ) ) ;
#37574 = ORIENTED_EDGE ( 'NONE', *, *, #48686, .T. ) ;
#37575 = CARTESIAN_POINT ( 'NONE',  ( 3.826736342760712173, 1.350229473097919630, -1.354399478966497261 ) ) ;
#37576 = CARTESIAN_POINT ( 'NONE',  ( -4.796887421136680985, 4.490790167614548523, 1.214306433183764966E-14 ) ) ;
#37577 = CARTESIAN_POINT ( 'NONE',  ( 8.945682426918439845, 9.331051007693339727, 1.040834085586084257E-14 ) ) ;
#37578 = CARTESIAN_POINT ( 'NONE',  ( 6.232888004217203459, -1.964670499678453197, -0.6532144590316590893 ) ) ;
#37579 = CARTESIAN_POINT ( 'NONE',  ( 5.478137895480934105, -2.137967713159651506, -0.4810252310911074525 ) ) ;
#37580 = CARTESIAN_POINT ( 'NONE',  ( 6.007156502879952953, 7.179297369210805080, -1.191424252104013037 ) ) ;
#37581 = CARTESIAN_POINT ( 'NONE',  ( -4.795807126352183758, 15.46909917608900109, -11.00906995846085223 ) ) ;
#37582 = ORIENTED_EDGE ( 'NONE', *, *, #38322, .F. ) ;
#37583 = EDGE_LOOP ( 'NONE', ( #113904, #170117, #51081, #184931 ) ) ;
#37584 = AXIS2_PLACEMENT_3D ( 'NONE', #108442, #191733, #109510 ) ;
#37585 = CARTESIAN_POINT ( 'NONE',  ( 4.871153761480781164, 8.051123856976298399, 0.9350251597124116243 ) ) ;
#37586 = EDGE_CURVE ( 'NONE', #179011, #168570, #161911, .T. ) ;
#37587 = CARTESIAN_POINT ( 'NONE',  ( 3.198369223161025676, -0.5396142385952484855, -1.791042426047453784 ) ) ;
#37588 = CARTESIAN_POINT ( 'NONE',  ( -3.246376473470825363, -0.8887487162375362626, 0.5058895364790267912 ) ) ;
#37589 = CARTESIAN_POINT ( 'NONE',  ( 0.000000000000000000, 0.000000000000000000, 0.000000000000000000 ) ) ;
#37590 = CARTESIAN_POINT ( 'NONE',  ( -6.887178846062105286, 10.97886638714038554, -0.7216878364870267237 ) ) ;
#37591 = CARTESIAN_POINT ( 'NONE',  ( 4.655245641445829641, 6.524482229810530498, 1.599625672291269396 ) ) ;
#37592 = CARTESIAN_POINT ( 'NONE',  ( 6.473496638176248652, -0.2593738453590052617, 2.053908440964563376 ) ) ;
#37593 = CARTESIAN_POINT ( 'NONE',  ( 0.6851730022342136239, 1.650096953764205399, 1.158669022729153175 ) ) ;
#37594 = CARTESIAN_POINT ( 'NONE',  ( -9.592557376868645846, 11.15007068022363157, -1.199719254218441611 ) ) ;
#37595 = CARTESIAN_POINT ( 'NONE',  ( 6.367489420273535039, 7.457767740854454708, -1.199719254218452047 ) ) ;
#37596 = CARTESIAN_POINT ( 'NONE',  ( -10.49167095263961613, 5.343775707538777731, -5.730694126968513658 ) ) ;
#37597 = CARTESIAN_POINT ( 'NONE',  ( 1.623246906879351581, -2.062630869249089116, 0.7406334225198917265 ) ) ;
#37598 = CARTESIAN_POINT ( 'NONE',  ( 5.971303284387838417, 0.1295235881030691594, -1.821162830480331563 ) ) ;
#37599 = CARTESIAN_POINT ( 'NONE',  ( -2.611917148927046295, 6.198987107056845858, 1.040834085586084257E-14 ) ) ;
#37600 = EDGE_CURVE ( 'NONE', #83422, #97605, #136311, .T. ) ;
#37601 = CARTESIAN_POINT ( 'NONE',  ( 4.502716413514295191, 6.346531463890372926, -1.443375672974068769 ) ) ;
#37602 = CARTESIAN_POINT ( 'NONE',  ( 10.18233705906309972, 11.83814697611718714, 1.199719254218450271 ) ) ;
#37603 = CARTESIAN_POINT ( 'NONE',  ( 3.354752944377597856, 6.001296637494123232, -1.199719254218446718 ) ) ;
#37604 = CARTESIAN_POINT ( 'NONE',  ( 8.000720045840086669, 8.506797273001177828, 0.7216878364870267237 ) ) ;
#37605 = ORIENTED_EDGE ( 'NONE', *, *, #149120, .T. ) ;
#37607 = CARTESIAN_POINT ( 'NONE',  ( 0.8912715949961318440, -0.05164314158133917476, -2.012595864970234238 ) ) ;
#37606 = CARTESIAN_POINT ( 'NONE',  ( 4.194743914777058436, 1.481411246205705412, 1.093257649623424754 ) ) ;
#37608 = CARTESIAN_POINT ( 'NONE',  ( 1.986132587416184370, 2.144477605524505393, 0.8272852225373708013 ) ) ;
#37610 = CARTESIAN_POINT ( 'NONE',  ( 6.121922100595678096, 1.933298025717408608, -0.3319332437697538607 ) ) ;
#37609 = CARTESIAN_POINT ( 'NONE',  ( 4.202664430556257713, 4.965825259479493603, 1.082531754730560403 ) ) ;
#37611 = CARTESIAN_POINT ( 'NONE',  ( 3.285556943750000070, -3.784374999522041705, 0.000000000000000000 ) ) ;
#37612 = CARTESIAN_POINT ( 'NONE',  ( -4.066556009095094737, 6.831733546331167695, 1.199719254218464037 ) ) ;
#37613 =( LENGTH_UNIT ( ) NAMED_UNIT ( * ) SI_UNIT ( .MILLI., .METRE. ) );
#37614 = CARTESIAN_POINT ( 'NONE',  ( 4.992401499097729456, -1.057410677138232780, 1.593263788312593743 ) ) ;
#37615 = CARTESIAN_POINT ( 'NONE',  ( -10.13202086811422475, 10.71511252242175161, -0.7998128361456291469 ) ) ;
#37616 = CARTESIAN_POINT ( 'NONE',  ( 6.348694402744908594, 6.841026321354189754, -0.6301123915167846645 ) ) ;
#37617 = CARTESIAN_POINT ( 'NONE',  ( -4.146814880933400005, 5.931313009212638931, 1.599625672291270506 ) ) ;
#37619 = CARTESIAN_POINT ( 'NONE',  ( 2.254581950620972997, -1.447608085528677480, 1.184820545849271767 ) ) ;
#37618 = CARTESIAN_POINT ( 'NONE',  ( 2.911755628046075906, -1.032623549580795608, -1.817877418097467501 ) ) ;
#37620 = CARTESIAN_POINT ( 'NONE',  ( 8.649738815838679429, 10.15407870897571563, -1.082531754730543083 ) ) ;
#37621 = CARTESIAN_POINT ( 'NONE',  ( 1.364683531249992088, 5.446875000341417916, 1.214306433183764966E-14 ) ) ;
#37622 = CARTESIAN_POINT ( 'NONE',  ( 3.350842269037973331, 0.4194941847268919832, -1.688999647770361490 ) ) ;
#37623 = CARTESIAN_POINT ( 'NONE',  ( 4.310602774141044868, 7.116454772218158809, -1.199719254218452047 ) ) ;
#37625 = CARTESIAN_POINT ( 'NONE',  ( -0.002066265982046951426, 3.412835225567954378, -2.002356613009339981 ) ) ;
#37624 = CARTESIAN_POINT ( 'NONE',  ( -7.045261094876551944, -5.790678129197933899, -7.662794434365294727 ) ) ;
#37626 = CARTESIAN_POINT ( 'NONE',  ( 4.195721234439112379, -0.6572638427989171417, 1.594953032058670894 ) ) ;
#37627 = CARTESIAN_POINT ( 'NONE',  ( 3.984055765753656164, -2.167877601896048390, -0.3204034371554059235 ) ) ;
#37628 = CARTESIAN_POINT ( 'NONE',  ( 5.988949835885216011, -0.3198878037087344306, -2.183464699167809275 ) ) ;
#37629 = CARTESIAN_POINT ( 'NONE',  ( 0.000000000000000000, 3.599999999999999201, 0.000000000000000000 ) ) ;
#37630 =( GEOMETRIC_REPRESENTATION_CONTEXT ( 3 ) GLOBAL_UNCERTAINTY_ASSIGNED_CONTEXT ( ( #120084 ) ) GLOBAL_UNIT_ASSIGNED_CONTEXT ( ( #114427, #199847, #133836 ) ) REPRESENTATION_CONTEXT ( 'NONE', 'WORKASPACE' ) );
#37631 = CARTESIAN_POINT ( 'NONE',  ( 3.696278757040452057, 0.9809249153905131857, -1.936940462344426628 ) ) ;
#37632 = CARTESIAN_POINT ( 'NONE',  ( 2.244514701088017539, 0.3993153960501935051, 1.781317584591130432 ) ) ;
#37633 = CARTESIAN_POINT ( 'NONE',  ( -5.000000000000013323, 8.499999999999996447, -0.7750000000000013545 ) ) ;
#37634 = CARTESIAN_POINT ( 'NONE',  ( 4.171193994350897327, 1.889596262492127199, -0.9554925290978563135 ) ) ;
#37635 = EDGE_CURVE ( 'NONE', #30840, #127879, #127738, .T. ) ;
#37636 = EDGE_LOOP ( 'NONE', ( #208577, #163984, #101568, #185543 ) ) ;
#37638 = CARTESIAN_POINT ( 'NONE',  ( -0.6823417656250003738, 2.280208333674753174, -1.181850606188749264 ) ) ;
#37637 = CARTESIAN_POINT ( 'NONE',  ( 5.196947908113320302, 1.872795242347685463, 1.321741379092307600 ) ) ;
#37639 = CARTESIAN_POINT ( 'NONE',  ( 6.620655732516644854, 4.701125524277991907, 2.388986273831222640 ) ) ;
#37640 = CARTESIAN_POINT ( 'NONE',  ( 2.866659414285625651, 5.431854185720147221, -1.199719254218446718 ) ) ;
#37641 = CARTESIAN_POINT ( 'NONE',  ( 0.3816889160728508812, 0.2035859187828891470, -2.110680546376259681 ) ) ;
#37642 = CARTESIAN_POINT ( 'NONE',  ( -5.178851490740209229, 7.065079377328788546, 1.443375672974064550 ) ) ;
#37643 = DIRECTION ( 'NONE',  ( 0.000000000000000000, 0.000000000000000000, -1.000000000000000000 ) ) ;
#37644 = CARTESIAN_POINT ( 'NONE',  ( -5.626270559546828309, 7.587068290936515247, 1.443375672974064550 ) ) ;
#37645 = AXIS2_PLACEMENT_3D ( 'NONE', #57837, #77290, #123999 ) ;
#37647 = CARTESIAN_POINT ( 'NONE',  ( 1.500000000000001332, 10.90625000068279249, 0.000000000000000000 ) ) ;
#37646 = CARTESIAN_POINT ( 'NONE',  ( -10.91804381884000641, -9.954640477432109336, 0.1905751637469953186 ) ) ;
#37648 = VERTEX_POINT ( 'NONE', #31215 ) ;
#37649 = CARTESIAN_POINT ( 'NONE',  ( 5.151017605526480025, 0.9962996879465220168, 1.753031629501592192 ) ) ;
#37651 = CARTESIAN_POINT ( 'NONE',  ( 4.557522945366278222, 1.653560713460072051, 1.232637662666216549 ) ) ;
#37650 = CARTESIAN_POINT ( 'NONE',  ( 6.471319392424407901, 6.444294134116939077, 0.7998128361456341429 ) ) ;
#37653 = FACE_OUTER_BOUND ( 'NONE', #174303, .T. ) ;
#37652 = CARTESIAN_POINT ( 'NONE',  ( 7.042534447655770080, 7.180988041878682004, -0.7998128361456341429 ) ) ;
#37654 = ADVANCED_FACE ( 'NONE', ( #63701 ), #211798, .T. ) ;
#37655 = CARTESIAN_POINT ( 'NONE',  ( 5.664274315459256748, 9.830346811336296398, -0.7998128361456481317 ) ) ;
#37656 = CARTESIAN_POINT ( 'NONE',  ( 1.001543065824772753E-15, -1.071874999522043792, 3.793834371823811669 ) ) ;
#37657 = DIRECTION ( 'NONE',  ( -0.000000000000000000, -0.000000000000000000, 1.000000000000000000 ) ) ;
#37658 = CARTESIAN_POINT ( 'NONE',  ( 0.1817335109410072314, -0.9834369453871127931, 1.844881371607492326 ) ) ;
#37659 = CARTESIAN_POINT ( 'NONE',  ( 4.430314669760617718, -1.560499787156752971, -1.277043788614096176 ) ) ;
#37660 = CARTESIAN_POINT ( 'NONE',  ( 3.315785976855676775, 1.165629053876730659, -1.425327459889616177 ) ) ;
#37661 = EDGE_CURVE ( 'NONE', #76787, #123444, #168841, .T. ) ;
#37662 = CARTESIAN_POINT ( 'NONE',  ( 5.738125327081736060, 7.717565519727259904, 1.599625672291267398 ) ) ;
#37663 =( LENGTH_UNIT ( ) NAMED_UNIT ( * ) SI_UNIT ( .MILLI., .METRE. ) );
#37664 = CARTESIAN_POINT ( 'NONE',  ( 0.4106395295978342297, 1.496939291644447279, 0.8566152473860905170 ) ) ;
#37665 = CARTESIAN_POINT ( 'NONE',  ( -3.952365473583647315, 4.569846793057691592, 1.199719254218462483 ) ) ;
#37666 = CARTESIAN_POINT ( 'NONE',  ( 0.6338907866723633155, 0.6742984703760960263, 2.197570948669794966 ) ) ;
#37667 = CARTESIAN_POINT ( 'NONE',  ( -5.412729640353771465, 7.337937218544611895, 1.599625672291269396 ) ) ;
#37668 = CARTESIAN_POINT ( 'NONE',  ( 0.4216216942964992609, -0.1093418885590720091, 2.259903825829346680 ) ) ;
#37669 = CARTESIAN_POINT ( 'NONE',  ( 3.229229631591294503, 0.05193219833012594627, 2.105601595880735033 ) ) ;
#37670 = CARTESIAN_POINT ( 'NONE',  ( -5.632486471834530661, 5.535932070087196344, -0.7998128361456362523 ) ) ;
#37671 = CARTESIAN_POINT ( 'NONE',  ( 7.182068686937156166, 9.402166106225269715, 1.599625672291281386 ) ) ;
#37672 = CARTESIAN_POINT ( 'NONE',  ( 6.061904078641523697, 7.205214525570814210, -1.082531754730548412 ) ) ;
#37673 = CARTESIAN_POINT ( 'NONE',  ( 6.281249999999699796, 0.7852924748228357066, 1.895863743163936022 ) ) ;
#37674 = CARTESIAN_POINT ( 'NONE',  ( -7.237355071596549116, 7.338002426484427687, 1.040834085586084257E-14 ) ) ;
#37675 = CARTESIAN_POINT ( 'NONE',  ( 5.300874872818821082, 9.128178418356554857, 0.7216878364870438212 ) ) ;
#37676 = CARTESIAN_POINT ( 'NONE',  ( 4.867170269011318773, 6.911508770089412224, 1.419371323323643130 ) ) ;
#37677 = CARTESIAN_POINT ( 'NONE',  ( -4.406563619641430840, 5.099744630125142564, -1.199719254218446718 ) ) ;
#37679 = CARTESIAN_POINT ( 'NONE',  ( 3.533611464748823927, -0.1604399991079318022, 2.215644447872004985 ) ) ;
#37678 = CARTESIAN_POINT ( 'NONE',  ( 2.443736651115399283, -1.977012053918187906, 0.7674769708189137507 ) ) ;
#37680 = CARTESIAN_POINT ( 'NONE',  ( 1.834175572193702530, 2.167931929539984814, 0.3193665180123914094 ) ) ;
#37681 = CARTESIAN_POINT ( 'NONE',  ( -5.052384799386910430, 9.046199365926717917, 1.214306433183764966E-14 ) ) ;
#37682 = CARTESIAN_POINT ( 'NONE',  ( -3.284818356260900796, 7.054314858938165678, 0.7998128361456352531 ) ) ;
#37683 = CARTESIAN_POINT ( 'NONE',  ( 6.039501783790233169, 1.813256598412491982, -0.7494862575098264479 ) ) ;
#37684 = CARTESIAN_POINT ( 'NONE',  ( -1.364683531250012516, 2.488541667008088876, -0.7879004041258289570 ) ) ;
#37685 = CARTESIAN_POINT ( 'NONE',  ( -5.153507786970285665, 5.185049637652990207, -0.7216878364870338292 ) ) ;
#37687 = ORIENTED_EDGE ( 'NONE', *, *, #102848, .T. ) ;
#37686 = CARTESIAN_POINT ( 'NONE',  ( -4.270455198624581783, 7.926022131796578662, 1.040834085586084257E-14 ) ) ;
#37688 = CARTESIAN_POINT ( 'NONE',  ( 4.605793411009856619, 1.573235607984494688, 1.422142093439874522 ) ) ;
#37689 = CARTESIAN_POINT ( 'NONE',  ( -6.116136693540540570, 10.14959355252370266, 0.000000000000000000 ) ) ;
#37690 = ORIENTED_EDGE ( 'NONE', *, *, #143656, .T. ) ;
#37692 = CARTESIAN_POINT ( 'NONE',  ( 6.350466702034289312, 0.6732396885240909956, 2.054270918568662729 ) ) ;
#37691 = CARTESIAN_POINT ( 'NONE',  ( -5.966997003790232235, 7.094489604910957148, -1.082531754730549967 ) ) ;
#37693 = CARTESIAN_POINT ( 'NONE',  ( 6.114890974963323345, 7.092793211334054604, 1.199719254218462483 ) ) ;
#37694 = CARTESIAN_POINT ( 'NONE',  ( 5.091278345985558396, -0.6575378499774006125, 1.720029930423284448 ) ) ;
#37695 = UNCERTAINTY_MEASURE_WITH_UNIT (LENGTH_MEASURE( 1.000000000000000082E-05 ), #169790, 'distance_accuracy_value', 'NONE');
#37696 =( LENGTH_UNIT ( ) NAMED_UNIT ( * ) SI_UNIT ( .MILLI., .METRE. ) );
#37697 = CARTESIAN_POINT ( 'NONE',  ( 1.364683531249988757, 2.446875000341415696, 1.214306433183764966E-14 ) ) ;
#37698 = CARTESIAN_POINT ( 'NONE',  ( 0.5908509756735094154, -0.6286620326499070543, 1.623129586062905805 ) ) ;
#37699 = CARTESIAN_POINT ( 'NONE',  ( -0.7500000000000006661, 11.23958333401613174, -1.299038105676657340 ) ) ;
#37700 = DIRECTION ( 'NONE',  ( 0.000000000000000000, 1.000000000000000000, 0.000000000000000000 ) ) ;
#37701 = DIRECTION ( 'NONE',  ( 0.000000000000000000, 0.000000000000000000, 1.000000000000000000 ) ) ;
#37702 = CARTESIAN_POINT ( 'NONE',  ( 5.207972885698374022, -2.151664816535401314, 0.2080130470862306957 ) ) ;
#37703 = CIRCLE ( 'NONE', #141498, 11.09999999999999964 ) ;
#37704 = CARTESIAN_POINT ( 'NONE',  ( -5.596818484342970912, 5.424043074688562172, -0.7998128361456221525 ) ) ;
#37705 = CARTESIAN_POINT ( 'NONE',  ( -6.019457014343129408, 9.966524250134902729, 0.000000000000000000 ) ) ;
#37706 = CARTESIAN_POINT ( 'NONE',  ( 4.944278945467968533, 2.155654431248493985, 0.1625706239713892443 ) ) ;
#37707 = CARTESIAN_POINT ( 'NONE',  ( 5.378184286887115029, -1.097432272127541131, 1.637457850930480241 ) ) ;
#37708 = CARTESIAN_POINT ( 'NONE',  ( 3.919074646851735455, 0.6231337533108800564, 1.618193163429545223 ) ) ;
#37709 = CARTESIAN_POINT ( 'NONE',  ( 1.101424459656743071, -0.5276332240332289869, 2.126988402630063835 ) ) ;
#37710 = CARTESIAN_POINT ( 'NONE',  ( 1.747554699363640607, -1.948627443588932806, 1.235768562340158194 ) ) ;
#37711 = CARTESIAN_POINT ( 'NONE',  ( 3.444654265643578128, 0.4973230594479564060, 1.999757164544394561 ) ) ;
#37712 = CARTESIAN_POINT ( 'NONE',  ( 0.3572357504952353158, 1.920940290975415854, -0.2841381762913769427 ) ) ;
#37714 = ORIENTED_EDGE ( 'NONE', *, *, #45494, .T. ) ;
#37713 = CARTESIAN_POINT ( 'NONE',  ( -6.819388077549415783, 10.89977715720891815, 0.7216878364870458196 ) ) ;
#37715 = CARTESIAN_POINT ( 'NONE',  ( -5.764151584465413869, 6.753873599078290546, -1.199719254218453823 ) ) ;
#37716 = CARTESIAN_POINT ( 'NONE',  ( -6.521108698048779573, 8.631046119188804155, -1.443375672974058777 ) ) ;
#37717 = CARTESIAN_POINT ( 'NONE',  ( 3.083271082906696048, -0.1608111237268796401, -2.200959079826501075 ) ) ;
#37718 = CARTESIAN_POINT ( 'NONE',  ( -1.642778471874998480, -1.888541666188708890, 2.845375778867863303 ) ) ;
#37719 = ORIENTED_EDGE ( 'NONE', *, *, #52063, .T. ) ;
#37720 = CARTESIAN_POINT ( 'NONE',  ( 0.2505320230819003680, -0.3960800208489853036, -1.824604621477694311 ) ) ;
#37721 = CARTESIAN_POINT ( 'NONE',  ( -0.1288028175206881731, 1.984098898469729200, -2.687169534535143178 ) ) ;
#37722 = LINE ( 'NONE', #150422, #82208 ) ;
#37724 = CARTESIAN_POINT ( 'NONE',  ( 6.825078400183572036, 7.629137130509069387, 2.744348168701661095 ) ) ;
#37723 = CARTESIAN_POINT ( 'NONE',  ( -6.087900257701670981, 7.118292344597175081, -1.149031449265491167 ) ) ;
#37725 = DIRECTION ( 'NONE',  ( 0.000000000000000000, 0.000000000000000000, 1.000000000000000000 ) ) ;
#37726 = ORIENTED_EDGE ( 'NONE', *, *, #140961, .F. ) ;
#37727 = CARTESIAN_POINT ( 'NONE',  ( 3.327077596220921141, 0.04893577929474152155, 2.060475874978876298 ) ) ;
#37728 = CARTESIAN_POINT ( 'NONE',  ( 1.360316468749955598, -0.005208332991877948244, 0.7853790794158660438 ) ) ;
#37729 = CARTESIAN_POINT ( 'NONE',  ( -4.855791571988752331, 8.816840600628864877, 0.7998128361456481317 ) ) ;
#37730 = CARTESIAN_POINT ( 'NONE',  ( -0.1290005225502922348, 7.629137130509076492, -2.773995091683972625 ) ) ;
#37732 = EDGE_CURVE ( 'NONE', #90486, #100328, #131377, .T. ) ;
#37731 = FILL_AREA_STYLE ('',( #188236 ) ) ;
#37733 = AXIS2_PLACEMENT_3D ( 'NONE', #177876, #63043, #112936 ) ;
#37734 = CARTESIAN_POINT ( 'NONE',  ( 4.172158584703322681, 5.890604320285754980, -1.599625672291256295 ) ) ;
#37735 = CARTESIAN_POINT ( 'NONE',  ( 1.463821189631772990, 2.030551501382936497, -0.3513165408277911794 ) ) ;
#37737 = CARTESIAN_POINT ( 'NONE',  ( -0.6823417656250039265, 13.06770833367473017, -1.181850606188755259 ) ) ;
#37736 = CARTESIAN_POINT ( 'NONE',  ( -0.4019237886466871523, 12.44866454968463287, -1.499999999999998668 ) ) ;
#37738 = CARTESIAN_POINT ( 'NONE',  ( 5.120175567455225618, 9.125288595339771547, -0.7998128361456281477 ) ) ;
#37739 = B_SPLINE_CURVE_WITH_KNOTS ( 'NONE', 3,
 ( #29192, #63816, #13977, #144053, #163464, #77932, #210048, #113711 ),
 .UNSPECIFIED., .F., .F.,
 ( 4, 2, 2, 4 ),
 ( 1.734723475976852932E-18, 0.0002034531274099198050, 0.0004069062548198378753, 0.0008138125096396721728 ),
 .UNSPECIFIED. ) ;
#37740 = LINE ( 'NONE', #154696, #32619 ) ;
#37741 = CARTESIAN_POINT ( 'NONE',  ( 5.672569038193632451, -1.402732290180560337, 1.703733612381942653 ) ) ;
#37742 = CARTESIAN_POINT ( 'NONE',  ( 0.2280961430754513408, -1.329988288769240024, -1.704746276402234528 ) ) ;
#37743 = COLOUR_RGB ( '', 0.09019608, 0.27058824, 0.51372549) ;
#37744 = CARTESIAN_POINT ( 'NONE',  ( -5.273758566035884776, 5.255065869904374409, 0.000000000000000000 ) ) ;
#37745 = CARTESIAN_POINT ( 'NONE',  ( 0.3215004009857677092, -1.429452135790244549, -1.422604240635255479 ) ) ;
#37746 = CARTESIAN_POINT ( 'NONE',  ( 1.529136539685072238, 2.264261833246409505, -0.3938019620175516322 ) ) ;
#37747 = CARTESIAN_POINT ( 'NONE',  ( -5.270602541814852086E-14, 4.000000000000003553, 1.829047314007930636 ) ) ;
#37748 = CARTESIAN_POINT ( 'NONE',  ( 6.375647946566725288, 0.3219878414668366218, -1.884816399834337686 ) ) ;
#37749 = CARTESIAN_POINT ( 'NONE',  ( 1.846004154127491415, 8.940320519588478732, -0.7749999999999996891 ) ) ;
#37750 = CARTESIAN_POINT ( 'NONE',  ( 1.516246529245099284, 1.258767711876613848, -1.383943980506313398 ) ) ;
#37751 = CARTESIAN_POINT ( 'NONE',  ( 3.362517798112668821, -1.944730434982215650, -0.5331690889110105580 ) ) ;
#37753 = CARTESIAN_POINT ( 'NONE',  ( 6.639320575229257670, 2.033582276073117701, 2.408309898857839304 ) ) ;
#37752 = CARTESIAN_POINT ( 'NONE',  ( -1.364683531250000748, 1.009375000341421247, 0.000000000000000000 ) ) ;
#37754 = B_SPLINE_CURVE_WITH_KNOTS ( 'NONE', 3,
 ( #70798, #136911, #74037, #139049 ),
 .UNSPECIFIED., .F., .F.,
 ( 4, 4 ),
 ( 0.000000000000000000, 0.002003498272494338549 ),
 .UNSPECIFIED. ) ;
#37756 = CARTESIAN_POINT ( 'NONE',  ( 5.549480973255512595, -1.659368771798474196, -1.296820645603852018 ) ) ;
#37755 = CARTESIAN_POINT ( 'NONE',  ( -8.064402442030170093, 8.302891025323665630, 0.7998128361456602331 ) ) ;
#37757 = CARTESIAN_POINT ( 'NONE',  ( 6.446011968293428041, 9.607765498729298415, -1.199719254218440723 ) ) ;
#37759 = CARTESIAN_POINT ( 'NONE',  ( -6.256197817702116026, 9.386315656372753224, -1.199719254218440723 ) ) ;
#37758 = CARTESIAN_POINT ( 'NONE',  ( 3.874598038455354665, 7.742391154831717692, -0.7998128361456362523 ) ) ;
#37760 = CARTESIAN_POINT ( 'NONE',  ( -0.3912817730721762643, -6.709848117146501423, -9.483257663144962990 ) ) ;
#37761 = CARTESIAN_POINT ( 'NONE',  ( 3.761977063697896639, 0.6766415394236917624, -1.903234751996728757 ) ) ;
#37762 = CARTESIAN_POINT ( 'NONE',  ( 0.6823417656249899377, 4.676041667008086655, -1.181850606188754593 ) ) ;
#37763 = EDGE_CURVE ( 'NONE', #108500, #16927, #79336, .T. ) ;
#37764 = CARTESIAN_POINT ( 'NONE',  ( 0.2860855845884663351, -1.266418373674676134, -1.628825195542679793 ) ) ;
#37765 = CARTESIAN_POINT ( 'NONE',  ( 7.944714827928039291, 11.25228915168265864, 1.082531754730557072 ) ) ;
#37766 = CARTESIAN_POINT ( 'NONE',  ( 5.518883860308030798, 1.994880785013030788, 0.8329173350848093627 ) ) ;
#37767 = CARTESIAN_POINT ( 'NONE',  ( 4.864343252252968597, 8.897093904262280972, 0.000000000000000000 ) ) ;
#37768 = CARTESIAN_POINT ( 'NONE',  ( -1.402160292154681736E-14, -0.4906249996585810846, -1.575800808251665908 ) ) ;
#37769 = CARTESIAN_POINT ( 'NONE',  ( 4.694866332082116678, 8.699370830729650450, 0.7998128361456341429 ) ) ;
#37770 = CARTESIAN_POINT ( 'NONE',  ( 6.873620692004076105, 10.00267932643801672, -1.082531754730537976 ) ) ;
#37772 = CARTESIAN_POINT ( 'NONE',  ( 0.000000000000000000, 10.00000000000000888, -4.500000000000000000 ) ) ;
#37771 = CARTESIAN_POINT ( 'NONE',  ( 2.629531826656985150, 0.1086732114553476541, -2.168588674111065817 ) ) ;
#37774 = CARTESIAN_POINT ( 'NONE',  ( 2.014959344526063845, -1.785600367564584179, 0.4486904387498573676 ) ) ;
#37773 = CARTESIAN_POINT ( 'NONE',  ( -6.412643469583822586, 6.583764924043652655, 1.040834085586084257E-14 ) ) ;
#37775 = CARTESIAN_POINT ( 'NONE',  ( -1.364683531249997417, 4.009375000341424133, 1.214306433183764966E-14 ) ) ;
#37776 = CARTESIAN_POINT ( 'NONE',  ( 2.964592600559623037, -2.025863808726846127, -0.8364240203130177687 ) ) ;
#37777 = FACE_OUTER_BOUND ( 'NONE', #175724, .T. ) ;
#37778 = CARTESIAN_POINT ( 'NONE',  ( 4.926805006903203221, 2.163674774341369123, 0.6614253976126910350 ) ) ;
#37779 = CARTESIAN_POINT ( 'NONE',  ( -5.880485940025243607, 7.883652901494672349, 1.599625672291269396 ) ) ;
#37780 = CARTESIAN_POINT ( 'NONE',  ( -1.364683531250010295, 5.551041667008087543, -0.7879004041258300672 ) ) ;
#37781 = CARTESIAN_POINT ( 'NONE',  ( 6.485343392949857844, 6.752073445700102816, -0.1478272009810890908 ) ) ;
#37782 = CARTESIAN_POINT ( 'NONE',  ( 0.7500000000000006661, 13.16666666666666607, -1.299038105676657340 ) ) ;
#37783 = CARTESIAN_POINT ( 'NONE',  ( -5.817857313595549584, 6.920493299683823096, 1.082531754730549078 ) ) ;
#37784 = CARTESIAN_POINT ( 'NONE',  ( 4.692530564105613422, 7.528350520548263702, -1.082531754730548412 ) ) ;
#37785 = CARTESIAN_POINT ( 'NONE',  ( 5.975818619601467319, 1.055637459841787473, 1.420274316496936917 ) ) ;
#37786 = COLOUR_RGB ( '', 0.09019608, 0.27058824, 0.51372549) ;
#37787 = CARTESIAN_POINT ( 'NONE',  ( 6.611572464958476836, 10.86525164242692298, 0.7998128361456462443 ) ) ;
#37788 = CARTESIAN_POINT ( 'NONE',  ( 2.327300794530688055, -0.001011052439145453856, 2.106147100168444197 ) ) ;
#37790 = CARTESIAN_POINT ( 'NONE',  ( 1.499999999999989120, 2.525000000000020339, 1.214306433183764966E-14 ) ) ;
#37789 = CARTESIAN_POINT ( 'NONE',  ( -0.6823417656250003738, 12.15104166700806054, 1.181850606188754593 ) ) ;
#37791 = CARTESIAN_POINT ( 'NONE',  ( 1.978894816976022097, 1.836590731562221412, 0.7118427970769640734 ) ) ;
#37792 = DIRECTION ( 'NONE',  ( 0.000000000000000000, 0.000000000000000000, -1.000000000000000000 ) ) ;
#37793 = FACE_OUTER_BOUND ( 'NONE', #66991, .T. ) ;
#37795 = ORIENTED_EDGE ( 'NONE', *, *, #117997, .F. ) ;
#37794 = CARTESIAN_POINT ( 'NONE',  ( 6.064714483498689468, 0.5772776769059180246, 1.717211531030158556 ) ) ;
#37796 = CARTESIAN_POINT ( 'NONE',  ( 4.989037340148863464, 8.764367963574922982, -0.7216878364870257245 ) ) ;
#37797 = CARTESIAN_POINT ( 'NONE',  ( 1.364683531249986537, -0.8239583329919186738, 0.7879004041258500513 ) ) ;
#37798 = EDGE_CURVE ( 'NONE', #33524, #37159, #7505, .T. ) ;
#37799 = CARTESIAN_POINT ( 'NONE',  ( 5.102362337376947998, -0.6309395149336484154, -1.761181640970374884 ) ) ;
#37800 = CARTESIAN_POINT ( 'NONE',  ( 6.069205674026176389, 1.823072449729469247, 0.9810699074010442722 ) ) ;
#37801 = CARTESIAN_POINT ( 'NONE',  ( 0.6125000000000123679, 2.916666666666671404, -1.060881119635948444 ) ) ;
#37802 = CARTESIAN_POINT ( 'NONE',  ( -4.895902867866254837, 7.765618208269001066, 1.082531754730549967 ) ) ;
#37803 = CARTESIAN_POINT ( 'NONE',  ( 1.080614271145773575, -0.9701817977426218098, 3.262761386485118376 ) ) ;
#37804 = CARTESIAN_POINT ( 'NONE',  ( 0.7499999999999885647, 0.8166666666666877461, -1.299038105676652899 ) ) ;
#37805 = CARTESIAN_POINT ( 'NONE',  ( 8.288111976655649471, 8.563885482386732306, -0.7998128361456291469 ) ) ;
#37806 = CARTESIAN_POINT ( 'NONE',  ( -10.00321840878439339, 10.56484298653695397, 1.040834085586084257E-14 ) ) ;
#37807 = CARTESIAN_POINT ( 'NONE',  ( 5.936491157937257235, 8.019268665717216749, 1.599625672291268286 ) ) ;
#37808 = CARTESIAN_POINT ( 'NONE',  ( 0.6823417656249864960, -0.5739583329919112353, -1.181850606188749264 ) ) ;
#37809 = CARTESIAN_POINT ( 'NONE',  ( 1.499999999999989120, 1.775000000000019673, 0.000000000000000000 ) ) ;
#37811 = CARTESIAN_POINT ( 'NONE',  ( 6.322179702674084467, 6.270297829408224111, 1.040834085586084257E-14 ) ) ;
#37810 = CARTESIAN_POINT ( 'NONE',  ( 5.195737816846159873, -1.386088135442983260, -1.388664821390848347 ) ) ;
#37812 = CARTESIAN_POINT ( 'NONE',  ( 3.198592129611950607, -1.351947076146834403, -1.495823048609262296 ) ) ;
#37813 = CARTESIAN_POINT ( 'NONE',  ( 2.079167605185348044, 1.483516914179264790, 1.212129443301296128 ) ) ;
#37814 = PLANE ( 'NONE',  #89976 ) ;
#37815 = CARTESIAN_POINT ( 'NONE',  ( -0.04112450405316381286, -1.960553898366865555, -0.9795403211517728082 ) ) ;
#37816 = CARTESIAN_POINT ( 'NONE',  ( 2.336979506217982117, -1.672866993182718698, 0.8370366242000035761 ) ) ;
#37817 = CARTESIAN_POINT ( 'NONE',  ( -1.364683531249997417, 5.759375000341418804, 1.214306433183764966E-14 ) ) ;
#37818 = CARTESIAN_POINT ( 'NONE',  ( 4.183843882646627321, 1.951733592454238497, -0.4931575689418183917 ) ) ;
#37819 = CARTESIAN_POINT ( 'NONE',  ( -8.076906825439122528, 10.44614393447756129, -1.599625672291263179 ) ) ;
#37821 = CARTESIAN_POINT ( 'NONE',  ( 4.394233635046361108, -0.9068805580662200327, -1.913321081533605028 ) ) ;
#37820 = CARTESIAN_POINT ( 'NONE',  ( -5.422898255786203769, 6.389431388914436738, -1.082531754730544860 ) ) ;
#37822 = CARTESIAN_POINT ( 'NONE',  ( 0.000000000000000000, 1.000000000000000888, 0.000000000000000000 ) ) ;
#37823 = CARTESIAN_POINT ( 'NONE',  ( 6.496543107701719499, 2.047251205643263017, 0.3077783505985449142 ) ) ;
#37824 = CARTESIAN_POINT ( 'NONE',  ( 1.487951815845720338, -2.081006265264739419, -0.2013860056617396421 ) ) ;
#37826 = VERTEX_POINT ( 'NONE', #139691 ) ;
#37825 = CARTESIAN_POINT ( 'NONE',  ( 6.194357462883206544, -1.817092693925310032, -0.1759843941628037589 ) ) ;
#37827 = EDGE_CURVE ( 'NONE', #86684, #68781, #193058, .T. ) ;
#37828 = CARTESIAN_POINT ( 'NONE',  ( 6.238723240582662477, 10.43026088065513513, -0.7998128361456291469 ) ) ;
#37829 = CARTESIAN_POINT ( 'NONE',  ( 7.927630635717423324, -6.615717645446945738, -7.626802973668249663 ) ) ;
#37830 = CARTESIAN_POINT ( 'NONE',  ( 9.704905176613070950, 13.32621205788646002, -8.135614888031417635 ) ) ;
#37831 = PRESENTATION_LAYER_ASSIGNMENT (  '', '', ( #162299 ) ) ;
#37832 = CARTESIAN_POINT ( 'NONE',  ( -10.44369227015510404, 5.112964020592959180, 5.232143560358712087 ) ) ;
#37834 = CARTESIAN_POINT ( 'NONE',  ( 6.277061933002774374, 9.306694107603160404, 1.082531754730558626 ) ) ;
#37833 = CARTESIAN_POINT ( 'NONE',  ( 5.770966940911189447, 9.884545197705074671, -0.7998128361456291469 ) ) ;
#37836 =( BOUNDED_SURFACE ( )  B_SPLINE_SURFACE ( 1, 2, ( 
 ( #89235, #75103, #172613, #6868, #190961, #122886, #42626, #188845, #10089, #76163, #40481, #24189, #90292, #57782, #123943, #60984, #30634, #209336, #96719, #161702, #210419, #109808, #162768, #15411, #131374, #213598, #65224, #176872, #45823, #145487, #14346, #28484, #111944, #43691, #175817, #146535, #27410, #44759, #80436, #113007, #196323, #180074, #163832, #212554, #81501, #127138, #93508, #13295, #64193, #47967, #211482, #79368, #159549, #177946, #128216, #110867, #193110, #130334, #11146, #31697, #94575, #97772, #114083, #160618, #147579, #78290, #95652, #29560, #77223, #143342, #12219, #144417, #62061, #63118, #194178, #129283, #195258, #46893, #179017, #201612, #135591, #197370, #4471, #151840, #53261, #148640, #51134, #32747, #20733, #167020, #199488, #117256, #184310, #33806, #99885, #206, #165947, #181126, #50071, #116192, #66276, #183255, #198425, #182177, #17531, #152892, #83620, #86828, #149702, #70542, #19681, #49012, #103082, #1283, #115131, #67341, #98829, #164878, #169138, #18614, #16473, #200551, #36999, #82553, #35934, #132424, #102013, #3417, #84694, #34859, #133486, #100933, #85760, #150781, #2344, #68420, #134547, #52198, #118324, #168082, #69483, #119392, #185380, #139869, #190710, #186447, #189653, #71616, #41304, #91117, #23942, #188588, #204813, #120474, #57534, #153969, #205900, #87896, #25015, #140954, #137729, #105231, #203749, #138793, #6618, #5536, #123691, #55393, #107412, #40220, #88978, #202686, #173436, #108482, #9835, #92197, #158246, #121548, #56464, #90046, #157176, #187519, #122626, #136661, #54335, #8770, #38083, #39150, #74853, #206966, #58595, #124750, #42371, #174506, #26082, #171272, #104155, #106330, #170203, #21787, #156105, #172352, #22865, #7690, #72698, #155033, #73773, #112747, #191776, #212286, #159289, #130076, #14079, #143090, #46624, #110616, #127965, #210154, #30371, #31436, #179817, #60719, #96458, #45563, #176616, #193917, #126882, #162508, #111680, #80169, #146275, #75911, #97514, #63920, #196071, #27151, #144162, #125814, #113817, #177687, #78038, #61796, #62851, #192840, #44499, #93255, #28228, #59657, #209082, #94321, #10888, #29298, #76963, #160362, #11965, #163571, #95392, #142014, #43432, #129013, #161443, #194990, #47703, #13024, #79101, #145219, #109556, #211225, #178759, #208029, #175560, #118069, #19419, #16208, #198170, #82291, #17277, #99622, #32488, #2082, #180867, #68155, #133219, #181917, #81240, #134289, #201354, #102823, #185111, #36737, #148384, #83353, #116994, #200294, #214385, #149438, #15154, #147322, #184055, #213349, #66015, #51946, #84432, #167819, #151584, #135340, #35674, #52995, #98562, #64972, #199225, #101752, #85497, #182994, #50872, #131125, #1020, #165688, #132164, #164623, #3151, #197114, #69221, #49803, #119131, #48753, #115929, #114866, #33549, #67085, #34611, #100680, #166758, #18354, #150521, #189395, #138531 ),
 ( #37817, #120209, #58334, #21527, #172094, #73508, #203485, #202419, #107147, #205633, #90854, #4218, #154776, #123433, #71355, #87638, #186184, #57271, #136403, #70287, #20482, #74588, #89796, #22609, #42107, #137471, #153709, #5278, #55138, #121283, #152631, #187259, #103894, #122366, #140691, #6360, #168878, #41037, #124490, #169942, #190449, #38886, #23686, #139611, #104971, #54074, #173173, #24752, #156918, #171012, #72429, #8507, #88717, #204554, #56203, #206707, #188322, #39962, #86569, #106070, #155842, #7427, #195794, #76701, #175299, #159033, #142818, #10626, #91927, #60455, #59394, #61525, #79896, #94055, #108220, #128743, #63659, #157987, #25817, #208825, #62581, #174245, #9575, #126612, #26885, #125550, #75652, #46356, #192575, #141759, #176354, #95118, #144948, #129813, #44230, #43176, #162236, #77773, #161167, #207767, #146005, #13822, #110351, #27962, #12753, #160096, #78827, #11699, #143893, #191511, #109289, #92988, #45293, #209887, #127691, #193651, #111413, #177417, #29035, #210954, #194717, #30095, #112476, #178485, #96185, #212015, #47432, #14879, #85230, #198957, #116725, #80972, #132954, #50600, #97244, #135079, #163298, #49534, #83089, #147063, #213083, #167556, #48491, #64714, #130857, #182725, #34344, #181654, #149168, #31171, #101486, #99365, #19157, #98297, #84167, #196853, #18079, #179550, #15944, #131897, #115660, #151319, #100417, #2887, #67881, #745, #114609, #180600, #32225, #150255, #164360, #183798, #82028, #68959, #200034, #148121, #1823, #214122, #165417, #33280, #134027, #113547, #65751, #197905, #51686, #17013, #66811, #166488, #117808, #35408, #22344, #205376, #139346, #201092, #8251, #155584, #57013, #152376, #54878, #36481, #24487, #170756, #203234, #121032, #188063, #37554, #103634, #3955, #169686, #184853, #53814, #119943, #70022, #186999, #202154, #185919, #21274, #156659, #87380, #90599, #153448, #77258, #23421, #52733, #106887, #5021, #118867, #71095, #102556, #168617, #172913, #88457, #20219, #204289, #40781, #86306, #39692, #136138, #105803, #7169, #154517, #38630, #104707, #137212, #122099, #6098, #55946, #72167, #89532, #123183, #138275, #171827, #73239, #189143, #13324, #160651, #130366, #94608, #196356, #46923, #95679, #209371, #47997, #115165, #16505, #98860, #164912, #62089, #145515, #30666, #114114, #128247, #211514, #143372, #61015, #31731, #127173, #144448, #180107, #212585, #81532, #65257, #49045, #97804, #181159, #12249, #193142, #113041, #163865, #147613, #96749, #179047, #44791, #63151, #79398, #29593, #32783, #110897, #176903, #162799, #28517, #146566, #197404, #78326, #15443, #210451, #213631, #131404, #14376, #195291, #129315, #194211, #64224, #45856, #111977, #177978, #161733, #80466, #83651, #51170, #149740, #84728, #167057, #99920, #69521, #33839, #135628, #200586, #34895, #148674, #201648, #54374, #170240, #38120, #104192, #1317, #150816 ) ),
 .UNSPECIFIED., .F., .F., .T. ) 
 B_SPLINE_SURFACE_WITH_KNOTS ( ( 2, 2 ),
 ( 3, 2, 2, 2, 2, 2, 2, 2, 2, 2, 2, 2, 2, 2, 2, 2, 2, 2, 2, 2, 2, 2, 2, 2, 2, 2, 2, 2, 2, 2, 2, 2, 2, 2, 2, 2, 2, 2, 2, 2, 2, 2, 2, 2, 2, 2, 2, 2, 2, 2, 2, 2, 2, 2, 2, 2, 2, 2, 2, 2, 2, 2, 2, 2, 2, 2, 2, 2, 2, 2, 2, 2, 2, 2, 2, 2, 2, 2, 2, 2, 2, 2, 2, 2, 2, 2, 2, 2, 2, 2, 2, 2, 2, 2, 2, 2, 2, 2, 2, 2, 2, 2, 2, 2, 2, 2, 2, 2, 2, 2, 2, 2, 2, 2, 2, 2, 2, 2, 2, 2, 2, 2, 2, 2, 2, 2, 2, 2, 2, 2, 2, 2, 2, 2, 2, 2, 2, 2, 2, 2, 2, 2, 2, 2, 2, 2, 2, 2, 2, 2, 2, 2, 2, 2, 2, 2, 2, 2, 2, 2, 2, 2, 2, 2, 2, 2, 2, 2, 3 ),
 ( 0.000000000000000000, 1.000000000000000000 ),
 ( 0.000000000000000000, 0.005952380952380952051, 0.01190476190476190410, 0.01785714285714285615, 0.02380952380952380820, 0.02976190476190476025, 0.03571428571428571230, 0.04166666666666666435, 0.04761904761904761640, 0.05357142857142856845, 0.05952380952380952051, 0.06547619047619047949, 0.07142857142857142461, 0.07738095238095238360, 0.08333333333333332871, 0.08928571428571428770, 0.09523809523809523281, 0.1011904761904761918, 0.1071428571428571369, 0.1130952380952380959, 0.1190476190476190410, 0.1250000000000000000, 0.1309523809523809590, 0.1369047619047619180, 0.1428571428571428492, 0.1488095238095238082, 0.1547619047619047672, 0.1607142857142857262, 0.1666666666666666574, 0.1726190476190476164, 0.1785714285714285754, 0.1845238095238095344, 0.1904761904761904656, 0.1964285714285714246, 0.2023809523809523836, 0.2083333333333333426, 0.2142857142857142738, 0.2202380952380952328, 0.2261904761904761918, 0.2321428571428571508, 0.2380952380952380820, 0.2440476190476190410, 0.2500000000000000000, 0.2559523809523809312, 0.2619047619047619180, 0.2678571428571428492, 0.2738095238095238360, 0.2797619047619047672, 0.2857142857142856984, 0.2916666666666666852, 0.2976190476190476164, 0.3035714285714285476, 0.3095238095238095344, 0.3154761904761904656, 0.3214285714285714524, 0.3273809523809523836, 0.3333333333333333148, 0.3392857142857143016, 0.3452380952380952328, 0.3511904761904761640, 0.3571428571428571508, 0.3630952380952380820, 0.3690476190476190688, 0.3750000000000000000, 0.3809523809523809312, 0.3869047619047619180, 0.3928571428571428492, 0.3988095238095238360, 0.4047619047619047672, 0.4107142857142856984, 0.4166666666666666852, 0.4226190476190476164, 0.4285714285714285476, 0.4345238095238095344, 0.4404761904761904656, 0.4464285714285714524, 0.4523809523809523836, 0.4583333333333333148, 0.4642857142857143016, 0.4702380952380952328, 0.4761904761904761640, 0.4821428571428571508, 0.4880952380952380820, 0.4940476190476190688, 0.5000000000000000000, 0.5059523809523809312, 0.5119047619047618625, 0.5178571428571429047, 0.5238095238095238360, 0.5297619047619047672, 0.5357142857142856984, 0.5416666666666666297, 0.5476190476190476719, 0.5535714285714286031, 0.5595238095238095344, 0.5654761904761904656, 0.5714285714285713969, 0.5773809523809523281, 0.5833333333333333703, 0.5892857142857143016, 0.5952380952380952328, 0.6011904761904761640, 0.6071428571428570953, 0.6130952380952381375, 0.6190476190476190688, 0.6250000000000000000, 0.6309523809523809312, 0.6369047619047618625, 0.6428571428571429047, 0.6488095238095238360, 0.6547619047619047672, 0.6607142857142856984, 0.6666666666666666297, 0.6726190476190476719, 0.6785714285714286031, 0.6845238095238095344, 0.6904761904761904656, 0.6964285714285713969, 0.7023809523809523281, 0.7083333333333333703, 0.7142857142857143016, 0.7202380952380952328, 0.7261904761904761640, 0.7321428571428570953, 0.7380952380952381375, 0.7440476190476190688, 0.7500000000000000000, 0.7559523809523809312, 0.7619047619047618625, 0.7678571428571429047, 0.7738095238095238360, 0.7797619047619047672, 0.7857142857142856984, 0.7916666666666666297, 0.7976190476190476719, 0.8035714285714286031, 0.8095238095238095344, 0.8154761904761904656, 0.8214285714285713969, 0.8273809523809523281, 0.8333333333333333703, 0.8392857142857143016, 0.8452380952380952328, 0.8511904761904761640, 0.8571428571428570953, 0.8630952380952381375, 0.8690476190476190688, 0.8750000000000000000, 0.8809523809523809312, 0.8869047619047618625, 0.8928571428571429047, 0.8988095238095238360, 0.9047619047619047672, 0.9107142857142856984, 0.9166666666666666297, 0.9226190476190476719, 0.9285714285714286031, 0.9345238095238095344, 0.9404761904761904656, 0.9464285714285713969, 0.9523809523809523281, 0.9583333333333333703, 0.9642857142857143016, 0.9702380952380952328, 0.9761904761904761640, 0.9821428571428570953, 0.9880952380952381375, 0.9940476190476190688, 1.000000000000000000 ),
 .UNSPECIFIED. ) 
 GEOMETRIC_REPRESENTATION_ITEM ( )  RATIONAL_B_SPLINE_SURFACE ( (
 ( 1.000000000000000000, 0.8660254037844387076, 1.000000000000000000, 0.8660254037844387076, 1.000000000000000000, 0.8660254037844387076, 1.000000000000000000, 0.8660254037844387076, 1.000000000000000000, 0.8660254037844387076, 1.000000000000000000, 0.8660254037844387076, 1.000000000000000000, 0.8660254037844387076, 1.000000000000000000, 0.8660254037844387076, 1.000000000000000000, 0.8660254037844387076, 1.000000000000000000, 0.8660254037844387076, 1.000000000000000000, 0.8660254037844387076, 1.000000000000000000, 0.8660254037844387076, 1.000000000000000000, 0.8660254037844387076, 1.000000000000000000, 0.8660254037844387076, 1.000000000000000000, 0.8660254037844387076, 1.000000000000000000, 0.8660254037844387076, 1.000000000000000000, 0.8660254037844387076, 1.000000000000000000, 0.8660254037844387076, 1.000000000000000000, 0.8660254037844387076, 1.000000000000000000, 0.8660254037844387076, 1.000000000000000000, 0.8660254037844387076, 1.000000000000000000, 0.8660254037844387076, 1.000000000000000000, 0.8660254037844387076, 1.000000000000000000, 0.8660254037844387076, 1.000000000000000000, 0.8660254037844387076, 1.000000000000000000, 0.8660254037844387076, 1.000000000000000000, 0.8660254037844387076, 1.000000000000000000, 0.8660254037844387076, 1.000000000000000000, 0.8660254037844387076, 1.000000000000000000, 0.8660254037844387076, 1.000000000000000000, 0.8660254037844387076, 1.000000000000000000, 0.8660254037844387076, 1.000000000000000000, 0.8660254037844387076, 1.000000000000000000, 0.8660254037844387076, 1.000000000000000000, 0.8660254037844387076, 1.000000000000000000, 0.8660254037844387076, 1.000000000000000000, 0.8660254037844387076, 1.000000000000000000, 0.8660254037844387076, 1.000000000000000000, 0.8660254037844387076, 1.000000000000000000, 0.8660254037844387076, 1.000000000000000000, 0.8660254037844387076, 1.000000000000000000, 0.8660254037844387076, 1.000000000000000000, 0.8660254037844387076, 1.000000000000000000, 0.8660254037844387076, 1.000000000000000000, 0.8660254037844387076, 1.000000000000000000, 0.8660254037844387076, 1.000000000000000000, 0.8660254037844387076, 1.000000000000000000, 0.8660254037844387076, 1.000000000000000000, 0.8660254037844387076, 1.000000000000000000, 0.8660254037844387076, 1.000000000000000000, 0.8660254037844387076, 1.000000000000000000, 0.8660254037844387076, 1.000000000000000000, 0.8660254037844387076, 1.000000000000000000, 0.8660254037844387076, 1.000000000000000000, 0.8660254037844387076, 1.000000000000000000, 0.8660254037844387076, 1.000000000000000000, 0.8660254037844387076, 1.000000000000000000, 0.8660254037844387076, 1.000000000000000000, 0.8660254037844387076, 1.000000000000000000, 0.8660254037844387076, 1.000000000000000000, 0.8660254037844387076, 1.000000000000000000, 0.8660254037844387076, 1.000000000000000000, 0.8660254037844387076, 1.000000000000000000, 0.8660254037844387076, 1.000000000000000000, 0.8660254037844387076, 1.000000000000000000, 0.8660254037844387076, 1.000000000000000000, 0.8660254037844387076, 1.000000000000000000, 0.8660254037844387076, 1.000000000000000000, 0.8660254037844387076, 1.000000000000000000, 0.8660254037844387076, 1.000000000000000000, 0.8660254037844387076, 1.000000000000000000, 0.8660254037844387076, 1.000000000000000000, 0.8660254037844387076, 1.000000000000000000, 0.8660254037844387076, 1.000000000000000000, 0.8660254037844387076, 1.000000000000000000, 0.8660254037844387076, 1.000000000000000000, 0.8660254037844387076, 1.000000000000000000, 0.8660254037844387076, 1.000000000000000000, 0.8660254037844387076, 1.000000000000000000, 0.8660254037844387076, 1.000000000000000000, 0.8660254037844387076, 1.000000000000000000, 0.8660254037844387076, 1.000000000000000000, 0.8660254037844387076, 1.000000000000000000, 0.8660254037844387076, 1.000000000000000000, 0.8660254037844387076, 1.000000000000000000, 0.8660254037844387076, 1.000000000000000000, 0.8660254037844387076, 1.000000000000000000, 0.8660254037844387076, 1.000000000000000000, 0.8660254037844387076, 1.000000000000000000, 0.8660254037844387076, 1.000000000000000000, 0.8660254037844387076, 1.000000000000000000, 0.8660254037844387076, 1.000000000000000000, 0.8660254037844387076, 1.000000000000000000, 0.8660254037844387076, 1.000000000000000000, 0.8660254037844387076, 1.000000000000000000, 0.8660254037844387076, 1.000000000000000000, 0.8660254037844387076, 1.000000000000000000, 0.8660254037844387076, 1.000000000000000000, 0.8660254037844387076, 1.000000000000000000, 0.8660254037844387076, 1.000000000000000000, 0.8660254037844387076, 1.000000000000000000, 0.8660254037844387076, 1.000000000000000000, 0.8660254037844387076, 1.000000000000000000, 0.8660254037844387076, 1.000000000000000000, 0.8660254037844387076, 1.000000000000000000, 0.8660254037844387076, 1.000000000000000000, 0.8660254037844387076, 1.000000000000000000, 0.8660254037844387076, 1.000000000000000000, 0.8660254037844387076, 1.000000000000000000, 0.8660254037844387076, 1.000000000000000000, 0.8660254037844387076, 1.000000000000000000, 0.8660254037844387076, 1.000000000000000000, 0.8660254037844387076, 1.000000000000000000, 0.8660254037844387076, 1.000000000000000000, 0.8660254037844387076, 1.000000000000000000, 0.8660254037844387076, 1.000000000000000000, 0.8660254037844387076, 1.000000000000000000, 0.8660254037844387076, 1.000000000000000000, 0.8660254037844387076, 1.000000000000000000, 0.8660254037844387076, 1.000000000000000000, 0.8660254037844387076, 1.000000000000000000, 0.8660254037844387076, 1.000000000000000000, 0.8660254037844387076, 1.000000000000000000, 0.8660254037844387076, 1.000000000000000000, 0.8660254037844387076, 1.000000000000000000, 0.8660254037844387076, 1.000000000000000000, 0.8660254037844387076, 1.000000000000000000, 0.8660254037844387076, 1.000000000000000000, 0.8660254037844387076, 1.000000000000000000, 0.8660254037844387076, 1.000000000000000000, 0.8660254037844387076, 1.000000000000000000, 0.8660254037844387076, 1.000000000000000000, 0.8660254037844387076, 1.000000000000000000, 0.8660254037844387076, 1.000000000000000000, 0.8660254037844387076, 1.000000000000000000, 0.8660254037844387076, 1.000000000000000000, 0.8660254037844387076, 1.000000000000000000, 0.8660254037844387076, 1.000000000000000000, 0.8660254037844387076, 1.000000000000000000, 0.8660254037844387076, 1.000000000000000000, 0.8660254037844387076, 1.000000000000000000, 0.8660254037844387076, 1.000000000000000000, 0.8660254037844387076, 1.000000000000000000, 0.8660254037844387076, 1.000000000000000000, 0.8660254037844387076, 1.000000000000000000, 0.8660254037844387076, 1.000000000000000000, 0.8660254037844387076, 1.000000000000000000, 0.8660254037844387076, 1.000000000000000000, 0.8660254037844387076, 1.000000000000000000, 0.8660254037844387076, 1.000000000000000000, 0.8660254037844387076, 1.000000000000000000, 0.8660254037844387076, 1.000000000000000000, 0.8660254037844387076, 1.000000000000000000, 0.8660254037844387076, 1.000000000000000000, 0.8660254037844387076, 1.000000000000000000, 0.8660254037844387076, 1.000000000000000000, 0.8660254037844387076, 1.000000000000000000, 0.8660254037844387076, 1.000000000000000000, 0.8660254037844387076, 1.000000000000000000, 0.8660254037844387076, 1.000000000000000000, 0.8660254037844387076, 1.000000000000000000, 0.8660254037844387076, 1.000000000000000000, 0.8660254037844387076, 1.000000000000000000, 0.8660254037844387076, 1.000000000000000000, 0.8660254037844387076, 1.000000000000000000, 0.8660254037844387076, 1.000000000000000000, 0.8660254037844387076, 1.000000000000000000, 0.8660254037844387076, 1.000000000000000000),
 ( 1.000000000000000000, 0.8660254037844387076, 1.000000000000000000, 0.8660254037844387076, 1.000000000000000000, 0.8660254037844387076, 1.000000000000000000, 0.8660254037844387076, 1.000000000000000000, 0.8660254037844387076, 1.000000000000000000, 0.8660254037844387076, 1.000000000000000000, 0.8660254037844387076, 1.000000000000000000, 0.8660254037844387076, 1.000000000000000000, 0.8660254037844387076, 1.000000000000000000, 0.8660254037844387076, 1.000000000000000000, 0.8660254037844387076, 1.000000000000000000, 0.8660254037844387076, 1.000000000000000000, 0.8660254037844387076, 1.000000000000000000, 0.8660254037844387076, 1.000000000000000000, 0.8660254037844387076, 1.000000000000000000, 0.8660254037844387076, 1.000000000000000000, 0.8660254037844387076, 1.000000000000000000, 0.8660254037844387076, 1.000000000000000000, 0.8660254037844387076, 1.000000000000000000, 0.8660254037844387076, 1.000000000000000000, 0.8660254037844387076, 1.000000000000000000, 0.8660254037844387076, 1.000000000000000000, 0.8660254037844387076, 1.000000000000000000, 0.8660254037844387076, 1.000000000000000000, 0.8660254037844387076, 1.000000000000000000, 0.8660254037844387076, 1.000000000000000000, 0.8660254037844387076, 1.000000000000000000, 0.8660254037844387076, 1.000000000000000000, 0.8660254037844387076, 1.000000000000000000, 0.8660254037844387076, 1.000000000000000000, 0.8660254037844387076, 1.000000000000000000, 0.8660254037844387076, 1.000000000000000000, 0.8660254037844387076, 1.000000000000000000, 0.8660254037844387076, 1.000000000000000000, 0.8660254037844387076, 1.000000000000000000, 0.8660254037844387076, 1.000000000000000000, 0.8660254037844387076, 1.000000000000000000, 0.8660254037844387076, 1.000000000000000000, 0.8660254037844387076, 1.000000000000000000, 0.8660254037844387076, 1.000000000000000000, 0.8660254037844387076, 1.000000000000000000, 0.8660254037844387076, 1.000000000000000000, 0.8660254037844387076, 1.000000000000000000, 0.8660254037844387076, 1.000000000000000000, 0.8660254037844387076, 1.000000000000000000, 0.8660254037844387076, 1.000000000000000000, 0.8660254037844387076, 1.000000000000000000, 0.8660254037844387076, 1.000000000000000000, 0.8660254037844387076, 1.000000000000000000, 0.8660254037844387076, 1.000000000000000000, 0.8660254037844387076, 1.000000000000000000, 0.8660254037844387076, 1.000000000000000000, 0.8660254037844387076, 1.000000000000000000, 0.8660254037844387076, 1.000000000000000000, 0.8660254037844387076, 1.000000000000000000, 0.8660254037844387076, 1.000000000000000000, 0.8660254037844387076, 1.000000000000000000, 0.8660254037844387076, 1.000000000000000000, 0.8660254037844387076, 1.000000000000000000, 0.8660254037844387076, 1.000000000000000000, 0.8660254037844387076, 1.000000000000000000, 0.8660254037844387076, 1.000000000000000000, 0.8660254037844387076, 1.000000000000000000, 0.8660254037844387076, 1.000000000000000000, 0.8660254037844387076, 1.000000000000000000, 0.8660254037844387076, 1.000000000000000000, 0.8660254037844387076, 1.000000000000000000, 0.8660254037844387076, 1.000000000000000000, 0.8660254037844387076, 1.000000000000000000, 0.8660254037844387076, 1.000000000000000000, 0.8660254037844387076, 1.000000000000000000, 0.8660254037844387076, 1.000000000000000000, 0.8660254037844387076, 1.000000000000000000, 0.8660254037844387076, 1.000000000000000000, 0.8660254037844387076, 1.000000000000000000, 0.8660254037844387076, 1.000000000000000000, 0.8660254037844387076, 1.000000000000000000, 0.8660254037844387076, 1.000000000000000000, 0.8660254037844387076, 1.000000000000000000, 0.8660254037844387076, 1.000000000000000000, 0.8660254037844387076, 1.000000000000000000, 0.8660254037844387076, 1.000000000000000000, 0.8660254037844387076, 1.000000000000000000, 0.8660254037844387076, 1.000000000000000000, 0.8660254037844387076, 1.000000000000000000, 0.8660254037844387076, 1.000000000000000000, 0.8660254037844387076, 1.000000000000000000, 0.8660254037844387076, 1.000000000000000000, 0.8660254037844387076, 1.000000000000000000, 0.8660254037844387076, 1.000000000000000000, 0.8660254037844387076, 1.000000000000000000, 0.8660254037844387076, 1.000000000000000000, 0.8660254037844387076, 1.000000000000000000, 0.8660254037844387076, 1.000000000000000000, 0.8660254037844387076, 1.000000000000000000, 0.8660254037844387076, 1.000000000000000000, 0.8660254037844387076, 1.000000000000000000, 0.8660254037844387076, 1.000000000000000000, 0.8660254037844387076, 1.000000000000000000, 0.8660254037844387076, 1.000000000000000000, 0.8660254037844387076, 1.000000000000000000, 0.8660254037844387076, 1.000000000000000000, 0.8660254037844387076, 1.000000000000000000, 0.8660254037844387076, 1.000000000000000000, 0.8660254037844387076, 1.000000000000000000, 0.8660254037844387076, 1.000000000000000000, 0.8660254037844387076, 1.000000000000000000, 0.8660254037844387076, 1.000000000000000000, 0.8660254037844387076, 1.000000000000000000, 0.8660254037844387076, 1.000000000000000000, 0.8660254037844387076, 1.000000000000000000, 0.8660254037844387076, 1.000000000000000000, 0.8660254037844387076, 1.000000000000000000, 0.8660254037844387076, 1.000000000000000000, 0.8660254037844387076, 1.000000000000000000, 0.8660254037844387076, 1.000000000000000000, 0.8660254037844387076, 1.000000000000000000, 0.8660254037844387076, 1.000000000000000000, 0.8660254037844387076, 1.000000000000000000, 0.8660254037844387076, 1.000000000000000000, 0.8660254037844387076, 1.000000000000000000, 0.8660254037844387076, 1.000000000000000000, 0.8660254037844387076, 1.000000000000000000, 0.8660254037844387076, 1.000000000000000000, 0.8660254037844387076, 1.000000000000000000, 0.8660254037844387076, 1.000000000000000000, 0.8660254037844387076, 1.000000000000000000, 0.8660254037844387076, 1.000000000000000000, 0.8660254037844387076, 1.000000000000000000, 0.8660254037844387076, 1.000000000000000000, 0.8660254037844387076, 1.000000000000000000, 0.8660254037844387076, 1.000000000000000000, 0.8660254037844387076, 1.000000000000000000, 0.8660254037844387076, 1.000000000000000000, 0.8660254037844387076, 1.000000000000000000, 0.8660254037844387076, 1.000000000000000000, 0.8660254037844387076, 1.000000000000000000, 0.8660254037844387076, 1.000000000000000000, 0.8660254037844387076, 1.000000000000000000, 0.8660254037844387076, 1.000000000000000000, 0.8660254037844387076, 1.000000000000000000, 0.8660254037844387076, 1.000000000000000000, 0.8660254037844387076, 1.000000000000000000, 0.8660254037844387076, 1.000000000000000000, 0.8660254037844387076, 1.000000000000000000, 0.8660254037844387076, 1.000000000000000000, 0.8660254037844387076, 1.000000000000000000, 0.8660254037844387076, 1.000000000000000000, 0.8660254037844387076, 1.000000000000000000, 0.8660254037844387076, 1.000000000000000000, 0.8660254037844387076, 1.000000000000000000, 0.8660254037844387076, 1.000000000000000000, 0.8660254037844387076, 1.000000000000000000, 0.8660254037844387076, 1.000000000000000000, 0.8660254037844387076, 1.000000000000000000, 0.8660254037844387076, 1.000000000000000000, 0.8660254037844387076, 1.000000000000000000, 0.8660254037844387076, 1.000000000000000000, 0.8660254037844387076, 1.000000000000000000, 0.8660254037844387076, 1.000000000000000000, 0.8660254037844387076, 1.000000000000000000, 0.8660254037844387076, 1.000000000000000000, 0.8660254037844387076, 1.000000000000000000, 0.8660254037844387076, 1.000000000000000000, 0.8660254037844387076, 1.000000000000000000, 0.8660254037844387076, 1.000000000000000000, 0.8660254037844387076, 1.000000000000000000, 0.8660254037844387076, 1.000000000000000000) ) ) 
 REPRESENTATION_ITEM ( '' )  SURFACE ( )  );
#37835 = CARTESIAN_POINT ( 'NONE',  ( -1.913843478179667823, 3.256154753185136475, 0.4414708703499633513 ) ) ;
#37837 = CARTESIAN_POINT ( 'NONE',  ( 0.3108108888784698598, 1.507076236086818399, -1.004716094995859121 ) ) ;
#37838 = CARTESIAN_POINT ( 'NONE',  ( -7.670162217029145246, 9.971608557999250166, 1.599625672291295375 ) ) ;
#37839 = CARTESIAN_POINT ( 'NONE',  ( 4.482942347612929979, 8.381849838857084123, 1.040834085586084257E-14 ) ) ;
#37840 = CARTESIAN_POINT ( 'NONE',  ( 0.2118258318327995438, -6.614835951978765394, 10.99866081003794527 ) ) ;
#37841 = DIRECTION ( 'NONE',  ( -0.7592566023652994600, 0.6507913734559651608, 0.000000000000000000 ) ) ;
#37842 = CARTESIAN_POINT ( 'NONE',  ( 2.683624340501134853, 5.218313266304903664, -1.199719254218446718 ) ) ;
#37843 = VERTEX_POINT ( 'NONE', #205713 ) ;
#37844 = CARTESIAN_POINT ( 'NONE',  ( 5.817982510940042040, 0.9913841921252890543, -1.755779027446252138 ) ) ;
#37845 = CARTESIAN_POINT ( 'NONE',  ( -0.09290056220616692284, -0.4702265987995763452, -2.075310686570643437 ) ) ;
#37846 = CARTESIAN_POINT ( 'NONE',  ( 6.983263157960373668, 7.629137130509066722, 2.546189081643289942 ) ) ;
#37847 = CARTESIAN_POINT ( 'NONE',  ( -1.284279953904125193, 10.64264068711930733, 0.7750000000000117906 ) ) ;
#37848 = CARTESIAN_POINT ( 'NONE',  ( 1.806654366501771136, 2.518449987798942136, 2.499999999999998668 ) ) ;
#37849 = CARTESIAN_POINT ( 'NONE',  ( -3.931501358282937009, 7.530575984731317618, 0.7216878364870317197 ) ) ;
#37850 = CARTESIAN_POINT ( 'NONE',  ( 8.595506201383999567, 12.97191496834930113, 0.7216878364870438212 ) ) ;
#37851 = CARTESIAN_POINT ( 'NONE',  ( 3.010559277710533888, 0.6591459557328577246, 1.856027811050243947 ) ) ;
#37852 = CARTESIAN_POINT ( 'NONE',  ( 4.675407748274028386, 1.496063595514389943, 1.352143027241403450 ) ) ;
#37853 = CARTESIAN_POINT ( 'NONE',  ( -6.555530967407501741, 7.606873202518897870, 1.199719254218450271 ) ) ;
#37854 = FILL_AREA_STYLE ('',( #140465 ) ) ;
#37855 = DIRECTION ( 'NONE',  ( -1.000000000000000000, -3.451266460341927087E-31, -8.638326563840810896E-31 ) ) ;
#37856 = CARTESIAN_POINT ( 'NONE',  ( 5.138714532536901913, -1.880766731008373993, 1.124575086929799239 ) ) ;
#37857 = CARTESIAN_POINT ( 'NONE',  ( 3.913718639709028668, 2.801499522163732880, 0.7750000000000135669 ) ) ;
#37858 = CARTESIAN_POINT ( 'NONE',  ( 3.012629298554883484, 1.396463203792638996, -1.327218363718547511 ) ) ;
#37859 = CARTESIAN_POINT ( 'NONE',  ( -7.670162217029145246, 9.971608557999250166, 1.599625672291295375 ) ) ;
#37860 = CARTESIAN_POINT ( 'NONE',  ( -0.1296875068448125334, 4.095146142119266308, -2.381513845672214913 ) ) ;
#37861 = CARTESIAN_POINT ( 'NONE',  ( 0.1884680354247054990, -1.036234488384666586, 1.948478269905975946 ) ) ;
#37862 = EDGE_CURVE ( 'NONE', #33092, #114840, #57347, .T. ) ;
#37863 = DIRECTION ( 'NONE',  ( 0.000000000000000000, -1.000000000000000000, 0.000000000000000000 ) ) ;
#37864 = ORIENTED_EDGE ( 'NONE', *, *, #11497, .F. ) ;
#37865 = CARTESIAN_POINT ( 'NONE',  ( 3.743459811148990291, 7.381470523066878009, -0.7216878364870338292 ) ) ;
#37866 = ORIENTED_EDGE ( 'NONE', *, *, #109624, .F. ) ;
#37867 = CARTESIAN_POINT ( 'NONE',  ( 4.575031941739591268, 1.798972412501558260, 0.8019633677735745758 ) ) ;
#37868 = VERTEX_POINT ( 'NONE', #140768 ) ;
#37870 = CARTESIAN_POINT ( 'NONE',  ( 3.510405448560415032, -2.010878083398774052, -0.09666398930169986525 ) ) ;
#37869 = CARTESIAN_POINT ( 'NONE',  ( 0.3802858058059845336, -0.2390265653847540028, -1.927249604900363122 ) ) ;
#37871 = CARTESIAN_POINT ( 'NONE',  ( 5.009243775243890973, 2.291699508649183592, 0.1762380284849179579 ) ) ;
#37873 = CARTESIAN_POINT ( 'NONE',  ( 4.328838875689292820, -1.735142615721802395, -0.6730405439913983434 ) ) ;
#37872 = CARTESIAN_POINT ( 'NONE',  ( -7.553827861469316396, 8.841829255582865699, -1.199719254218452047 ) ) ;
#37874 = CARTESIAN_POINT ( 'NONE',  ( 5.501576472095266901, 9.640532660744973725, -0.7998128361456481317 ) ) ;
#37875 = DIRECTION ( 'NONE',  ( 0.000000000000000000, 0.000000000000000000, -1.000000000000000000 ) ) ;
#37876 = DIRECTION ( 'NONE',  ( -0.9692622846690300831, 1.734723475976804255E-14, -0.2460297208025325477 ) ) ;
#37877 = CARTESIAN_POINT ( 'NONE',  ( -7.206322340863467346, 8.366129804884193888, 1.199719254218450271 ) ) ;
#37878 = CARTESIAN_POINT ( 'NONE',  ( -5.655159470675923394, 5.770309935309573923, 0.000000000000000000 ) ) ;
#37879 = CARTESIAN_POINT ( 'NONE',  ( 0.8553300576445364012, 0.4222666777726029608, -2.150330908352434012 ) ) ;
#37880 = CARTESIAN_POINT ( 'NONE',  ( 5.666945020832170776, 7.634521829102760115, 1.443375672974062551 ) ) ;
#37881 = ORIENTED_EDGE ( 'NONE', *, *, #150934, .T. ) ;
#37882 = DIRECTION ( 'NONE',  ( 0.6507913734559688246, 0.7592566023652963514, 0.000000000000000000 ) ) ;
#37883 = CARTESIAN_POINT ( 'NONE',  ( 0.04711308451243316486, -1.408776630263553375, -1.161003007932148501 ) ) ;
#37884 = CARTESIAN_POINT ( 'NONE',  ( -2.761056838677368397, 6.372983411765559048, 0.7998128361456341429 ) ) ;
#37885 = CARTESIAN_POINT ( 'NONE',  ( 2.742450610247765486, 1.725592070310760118, -0.1720703960508932762 ) ) ;
#37886 = CARTESIAN_POINT ( 'NONE',  ( -4.950135482320918712, 7.828889591799445213, -1.082531754730549967 ) ) ;
#37887 = CARTESIAN_POINT ( 'NONE',  ( 6.509000000000048303, 0.5949247728001515467, 1.954148248227548290 ) ) ;
#37888 = CARTESIAN_POINT ( 'NONE',  ( -4.869349725602420520, 8.832658446511480577, 1.040834085586084257E-14 ) ) ;
#37889 = DIRECTION ( 'NONE',  ( 0.000000000000000000, -1.000000000000000000, 0.000000000000000000 ) ) ;
#37890 = CARTESIAN_POINT ( 'NONE',  ( 0.7255434793691470929, 0.2065170452952343472, -2.059959488672699290 ) ) ;
#37891 = CARTESIAN_POINT ( 'NONE',  ( 5.760330229460346452, 0.7440287100829169331, 1.667389206893993725 ) ) ;
#37892 = CARTESIAN_POINT ( 'NONE',  ( 3.186327686730246800, 1.093712407854827706, -1.628379936052851917 ) ) ;
#37893 = CARTESIAN_POINT ( 'NONE',  ( -1.225000000000042055, -1.187499999317158439, -4.857225732735059864E-14 ) ) ;
#37894 = CARTESIAN_POINT ( 'NONE',  ( -7.883176251342026042, 11.28445716228600126, -1.199719254218446718 ) ) ;
#37895 = CARTESIAN_POINT ( 'NONE',  ( 6.317209508963599340, 9.457495962844502557, 1.199719254218462483 ) ) ;
#37896 = AXIS2_PLACEMENT_3D ( 'NONE', #95902, #145736, #127395 ) ;
#37897 = CARTESIAN_POINT ( 'NONE',  ( 3.422626747576805961, -0.8610355553571764631, -1.937992358232228041 ) ) ;
#37898 = CARTESIAN_POINT ( 'NONE',  ( 6.994027139803230320, 9.253060644560830994, -1.599625672291267398 ) ) ;
#37899 = CARTESIAN_POINT ( 'NONE',  ( -10.15913717534155047, 10.74674821418697057, 0.7998128361456462443 ) ) ;
#37900 = CARTESIAN_POINT ( 'NONE',  ( 1.358353136502856939, -2.070434559563800736, -0.003889755252693693176 ) ) ;
#37902 = CARTESIAN_POINT ( 'NONE',  ( 1.364683531249986537, -0.7822916663252464931, -0.7879004041258309554 ) ) ;
#37901 = DIRECTION ( 'NONE',  ( 0.000000000000000000, 9.023263958591318651E-17, -1.000000000000000000 ) ) ;
#37903 = ORIENTED_EDGE ( 'NONE', *, *, #182978, .T. ) ;
#37905 = ORIENTED_EDGE ( 'NONE', *, *, #2431, .F. ) ;
#37904 = CARTESIAN_POINT ( 'NONE',  ( 4.670683837814712192, 0.8496151569591952057, 2.052583376702998397 ) ) ;
#37906 = CARTESIAN_POINT ( 'NONE',  ( 1.600609022366938916, -0.2761435782051116505, 2.281986030651184993 ) ) ;
#37907 = CARTESIAN_POINT ( 'NONE',  ( 7.754900677336718395, 11.99120852362745460, -0.7216878364870267237 ) ) ;
#37909 = CARTESIAN_POINT ( 'NONE',  ( -3.474999999999998312, -0.6708333333333343917, 2.006292185433951047 ) ) ;
#37908 = CARTESIAN_POINT ( 'NONE',  ( 8.000720045840086669, 8.506797273001177828, 0.7216878364870267237 ) ) ;
#37910 = EDGE_CURVE ( 'NONE', #12050, #65799, #189671, .T. ) ;
#37911 = DIRECTION ( 'NONE',  ( 0.9990890794760038940, 0.000000000000000000, -0.04267330865764931702 ) ) ;
#37912 = ORIENTED_EDGE ( 'NONE', *, *, #74682, .T. ) ;
#37913 = CARTESIAN_POINT ( 'NONE',  ( -5.473998445134435009, 6.274837103192765220, -1.008633756803478443 ) ) ;
#37914 = EDGE_CURVE ( 'NONE', #108790, #58716, #122443, .T. ) ;
#37915 = CARTESIAN_POINT ( 'NONE',  ( 2.724755696555291262, 1.382288352666941389, -1.321784923088549446 ) ) ;
#37916 = CARTESIAN_POINT ( 'NONE',  ( -0.5637493975453833350, 6.831070374499072173, -3.741427165998697291 ) ) ;
#37917 = CARTESIAN_POINT ( 'NONE',  ( 4.453923018928796829, 1.724380149092176850, -0.04373908735122617603 ) ) ;
#37918 = CARTESIAN_POINT ( 'NONE',  ( 2.448454179885678705, -1.387098808145654560, 1.463928423225707931 ) ) ;
#37919 = CARTESIAN_POINT ( 'NONE',  ( 3.832918613053246659, 0.7734572015929435107, -2.164792806810557746 ) ) ;
#37920 = DIRECTION ( 'NONE',  ( -1.224646799147355426E-16, 0.000000000000000000, -1.000000000000000000 ) ) ;
#37921 = CARTESIAN_POINT ( 'NONE',  ( 5.971333374016301043, 0.1563851966441217600, -2.100315135224324337 ) ) ;
#37922 = CARTESIAN_POINT ( 'NONE',  ( -4.163762573172648196, 7.871823745427799501, 0.000000000000000000 ) ) ;
#37923 = ORIENTED_EDGE ( 'NONE', *, *, #178754, .F. ) ;
#37924 = CARTESIAN_POINT ( 'NONE',  ( 4.604631121011967920, 1.368492104089440442, -1.122162792211104820 ) ) ;
#37926 = CARTESIAN_POINT ( 'NONE',  ( 0.3051332635122120385, 1.997493689478089252, 1.124391992203729540 ) ) ;
#37925 = CARTESIAN_POINT ( 'NONE',  ( 5.365994935958575240, 9.482354201918870018, 0.7998128361456341429 ) ) ;
#37927 = CARTESIAN_POINT ( 'NONE',  ( 5.103375755629981469, -1.831930319445294719, 0.1838923505294575433 ) ) ;
#37928 = CARTESIAN_POINT ( 'NONE',  ( -3.867100128395853709, 5.534702787927018974, -1.599625672291256295 ) ) ;
#37929 = CARTESIAN_POINT ( 'NONE',  ( 6.105464321129510097, -2.175355461714892691, 0.2646407054325700670 ) ) ;
#37930 = CARTESIAN_POINT ( 'NONE',  ( -5.468734858265826837, 7.473552982767158070, 1.599625672291263179 ) ) ;
#37931 = CARTESIAN_POINT ( 'NONE',  ( -1.360316468750048635, -0.5989583329919208055, -0.7853790794159082322 ) ) ;
#37932 = CARTESIAN_POINT ( 'NONE',  ( -9.333041836230014709, 15.44694763438214302, 7.472413793098208856 ) ) ;
#37933 = CARTESIAN_POINT ( 'NONE',  ( 5.793440749948310042, -1.873300974885267589, 0.8818263447485861217 ) ) ;
#37934 = CARTESIAN_POINT ( 'NONE',  ( 1.534389036647098692, 0.6371565916030231813, 1.913260934284975345 ) ) ;
#37935 = CARTESIAN_POINT ( 'NONE',  ( 0.7499999999999867883, -1.152083332650516434, -1.299038105676652011 ) ) ;
#37936 = CARTESIAN_POINT ( 'NONE',  ( 4.125552361149776637, -1.843237290211484192, 0.5602470265201089372 ) ) ;
#37937 = CARTESIAN_POINT ( 'NONE',  ( -0.6823417656250039265, 11.31770833367473728, -1.181850606188755259 ) ) ;
#37938 = CARTESIAN_POINT ( 'NONE',  ( 1.617743263029525869, 1.850308847857740968, 1.228972131997711381 ) ) ;
#37940 = EDGE_LOOP ( 'NONE', ( #105698, #162490, #131327, #117046, #123551 ) ) ;
#37939 = FACE_OUTER_BOUND ( 'NONE', #34112, .T. ) ;
#37942 = CARTESIAN_POINT ( 'NONE',  ( 11.92619526913699879, 13.40000000000000036, -1.328859060402686199 ) ) ;
#37941 = DIRECTION ( 'NONE',  ( 0.000000000000000000, 1.000000000000000000, 0.000000000000000000 ) ) ;
#37943 = CARTESIAN_POINT ( 'NONE',  ( 1.499999999999959588, 7.128742170989514904, -10.89107411574800288 ) ) ;
#37944 = CARTESIAN_POINT ( 'NONE',  ( 3.192055101013606233, 5.811482486902795230, -1.199719254218446718 ) ) ;
#37945 = CARTESIAN_POINT ( 'NONE',  ( -0.9311234436981447038, -2.521869630441519572, -3.475000000000004086 ) ) ;
#37946 = SURFACE_STYLE_USAGE ( .BOTH. , #166886 ) ;
#37947 = CARTESIAN_POINT ( 'NONE',  ( 4.704519267438088015, 1.517481324781422503, 0.8521212890505409643 ) ) ;
#37948 = CARTESIAN_POINT ( 'NONE',  ( 2.594135478747404022, 0.9273930874063830432, -1.728848471177657942 ) ) ;
#37950 = CARTESIAN_POINT ( 'NONE',  ( -0.6823417656250212460, 2.363541667008084435, 1.181850606188767472 ) ) ;
#37949 = CARTESIAN_POINT ( 'NONE',  ( 5.148345644887269756, 7.029489223833707001, -1.599625672291256295 ) ) ;
#37951 = CARTESIAN_POINT ( 'NONE',  ( -4.964471428385745178, 6.642511170548884181, 1.245120630419704888 ) ) ;
#37952 = CARTESIAN_POINT ( 'NONE',  ( 10.14529669463207640, -6.681160345271552892, 9.269928574751062911E-15 ) ) ;
#37953 = CARTESIAN_POINT ( 'NONE',  ( 6.408651779211167465, 0.6141799454031526828, 1.863335524608072502 ) ) ;
#37954 = CARTESIAN_POINT ( 'NONE',  ( -8.369460898337653276, 8.658792557682392754, 0.7998128361456462443 ) ) ;
#37955 = CARTESIAN_POINT ( 'NONE',  ( -5.707619481228834779, 5.761236937629489852, -0.7216878364870197293 ) ) ;
#37956 = CARTESIAN_POINT ( 'NONE',  ( 5.085172837459294826, 1.651341431264556014, 1.157102043685846793 ) ) ;
#37957 = CARTESIAN_POINT ( 'NONE',  ( 1.270828881381684150, -1.433710284283566949, 1.750253757905173124 ) ) ;
#37959 = VERTEX_POINT ( 'NONE', #171088 ) ;
#37958 = CARTESIAN_POINT ( 'NONE',  ( -6.905180308061733996, 6.950465202360470052, 0.7998128361456341429 ) ) ;
#37960 = CARTESIAN_POINT ( 'NONE',  ( 1.499999999999987566, -0.9437499993171851731, 0.000000000000000000 ) ) ;
#37961 = CARTESIAN_POINT ( 'NONE',  ( 1.862360739135361376, -1.326353699019737098, 1.319252464149045734 ) ) ;
#37962 = CARTESIAN_POINT ( 'NONE',  ( 0.5626190647941519130, -0.9651924803987484980, 1.440457774218842690 ) ) ;
#37964 = CARTESIAN_POINT ( 'NONE',  ( 4.722331747100577459, 2.097238624054961864, 0.6360808509995665716 ) ) ;
#37963 = CARTESIAN_POINT ( 'NONE',  ( 1.360316468749963592, 1.286458333674704191, -0.7853790794158961308 ) ) ;
#37965 = CARTESIAN_POINT ( 'NONE',  ( 5.491387719013633983, 2.038315193044057505, -1.081779828593228521 ) ) ;
#37966 = CARTESIAN_POINT ( 'NONE',  ( 6.485628570817172367, 1.417799985879987901, 1.495801911481582813 ) ) ;
#37967 = CARTESIAN_POINT ( 'NONE',  ( 3.099484260031000193, -1.939694849350329431, 0.09605879933238459234 ) ) ;
#37968 = CARTESIAN_POINT ( 'NONE',  ( -4.026408433134269771, 6.680931691089825541, 1.082531754730560403 ) ) ;
#37969 = FACE_OUTER_BOUND ( 'NONE', #60819, .T. ) ;
#37970 = CARTESIAN_POINT ( 'NONE',  ( 4.638297949650961982, 5.544340708415133712, -1.082531754730548412 ) ) ;
#37971 = CARTESIAN_POINT ( 'NONE',  ( 1.360316468749983576, 0.5156250003414062366, -5.204170427930421283E-15 ) ) ;
#37972 = CARTESIAN_POINT ( 'NONE',  ( 4.711564657724523819, 1.930417226389494090, 0.5826574956761670920 ) ) ;
#37973 = CARTESIAN_POINT ( 'NONE',  ( -4.785665035499573783, 5.645992631913323123, 1.082531754730558626 ) ) ;
#37974 = CARTESIAN_POINT ( 'NONE',  ( -4.633854640820660009, 8.628190524257904670, -0.7998128361456362523 ) ) ;
#37975 = CARTESIAN_POINT ( 'NONE',  ( 9.206149998879153529, 10.69926207256923689, 1.199719254218453823 ) ) ;
#37977 = CARTESIAN_POINT ( 'NONE',  ( -6.956254272497635505, -6.713678229394818509, 6.457408393014306469 ) ) ;
#37976 = CARTESIAN_POINT ( 'NONE',  ( 0.8557438351849018243, 1.823752217391808372, -0.08689656109241167270 ) ) ;
#37978 = CARTESIAN_POINT ( 'NONE',  ( -4.634908411025374875, 6.500755460986618495, 1.599625672291263179 ) ) ;
#37979 = CARTESIAN_POINT ( 'NONE',  ( -8.724804694929160327E-15, -6.594478602028689629, -10.23203630735469893 ) ) ;
#37980 = CARTESIAN_POINT ( 'NONE',  ( -11.25356361929547688, 4.972433335311166935, 5.839389443199928920 ) ) ;
#37981 = ORIENTED_EDGE ( 'NONE', *, *, #119819, .T. ) ;
#37982 = CARTESIAN_POINT ( 'NONE',  ( 6.209851105358469958, -2.045643633555578766, 0.2495701479476707119 ) ) ;
#37983 = CARTESIAN_POINT ( 'NONE',  ( -6.577113915960841162, 7.806292669110006521, -1.082531754730549967 ) ) ;
#37984 = CARTESIAN_POINT ( 'NONE',  ( -2.279742385392243165, 5.811449882932888222, -0.7998128361456281477 ) ) ;
#37985 = CARTESIAN_POINT ( 'NONE',  ( 8.499999999999980460, 6.200000000000038369, 2.900000000000013678 ) ) ;
#37986 = CARTESIAN_POINT ( 'NONE',  ( 5.426427855750480589, -0.9099042507111715361, -1.803185865349592021 ) ) ;
#37988 = ORIENTED_EDGE ( 'NONE', *, *, #15314, .T. ) ;
#37987 = CARTESIAN_POINT ( 'NONE',  ( 5.988988838570013407, -2.108473666775429134, -0.6992015888120094447 ) ) ;
#37989 = CARTESIAN_POINT ( 'NONE',  ( -3.492107083971660586, 6.231819477012331632, 1.199719254218452935 ) ) ;
#37990 = CARTESIAN_POINT ( 'NONE',  ( 5.494078562035752178, 7.432844293840273231, -1.599625672291262513 ) ) ;
#37991 = STYLED_ITEM ( 'NONE', ( #177906 ), #24912 ) ;
#37992 = CARTESIAN_POINT ( 'NONE',  ( 5.752824481226431530, -1.626044790292068498, 1.266090340377580947 ) ) ;
#37993 = CARTESIAN_POINT ( 'NONE',  ( 4.342422763466713853, 0.4390309838058319425, -1.967887491402267486 ) ) ;
#37994 = VERTEX_POINT ( 'NONE', #42184 ) ;
#37995 = ORIENTED_EDGE ( 'NONE', *, *, #204332, .F. ) ;
#37996 = CARTESIAN_POINT ( 'NONE',  ( 3.246287715468270108, 5.874753870433235825, 1.199719254218450271 ) ) ;
#37998 = ORIENTED_EDGE ( 'NONE', *, *, #70571, .F. ) ;
#37997 = CARTESIAN_POINT ( 'NONE',  ( -5.271087860662956537, 9.371629280740593870, 0.000000000000000000 ) ) ;
#37999 = CARTESIAN_POINT ( 'NONE',  ( 4.650542599771462449, 8.421518672640367242, 0.4769741307986720136 ) ) ;
#38000 = CARTESIAN_POINT ( 'NONE',  ( 3.813827237909522605, -1.649828814528127907, 1.158511658058670957 ) ) ;
#38001 = CARTESIAN_POINT ( 'NONE',  ( 3.486116527793288178, -0.3603757036649730128, -1.805346353211812804 ) ) ;
#38002 = CARTESIAN_POINT ( 'NONE',  ( -0.005207807541490402925, 15.44298311167088755, 11.94812393301963915 ) ) ;
#38003 = CARTESIAN_POINT ( 'NONE',  ( 2.403307275528394626, 1.852421531443759539, -1.376039175078101806 ) ) ;
#38004 = CARTESIAN_POINT ( 'NONE',  ( 5.435893244436359240, 5.306573304789342416, -0.7998128361456481317 ) ) ;
#38005 = CARTESIAN_POINT ( 'NONE',  ( 4.552137767457805850, 2.161219302129935738, -0.04802546048104232301 ) ) ;
#38006 = CARTESIAN_POINT ( 'NONE',  ( 7.476431642932036326, 10.80992178580769014, 1.199719254218460707 ) ) ;
#38007 = CARTESIAN_POINT ( 'NONE',  ( 6.603072989126265391, -0.3962418105841297722, 1.804722624154910360 ) ) ;
#38008 = CARTESIAN_POINT ( 'NONE',  ( -4.574986769607567894, 7.424902766929059261, 1.199719254218464037 ) ) ;
#38009 = AXIS2_PLACEMENT_3D ( 'NONE', #75246, #57922, #207372 ) ;
#38010 = CARTESIAN_POINT ( 'NONE',  ( 4.112918304081806475, 0.7786346584819616723, -2.162581562504022337 ) ) ;
#38011 = CARTESIAN_POINT ( 'NONE',  ( -9.421119846345563431, 14.56525804660669898, -7.432612890530830185 ) ) ;
#38012 = DIRECTION ( 'NONE',  ( -0.6507913734559650498, 0.7592566023652995710, 0.000000000000000000 ) ) ;
#38013 = CARTESIAN_POINT ( 'NONE',  ( 2.254581950620972997, -1.447608085528677480, 1.184820545849271767 ) ) ;
#38014 = CARTESIAN_POINT ( 'NONE',  ( 6.614144449397460157, -0.9292204182751627739, -1.738729380627493049 ) ) ;
#38016 = DIRECTION ( 'NONE',  ( -0.05727394217551152328, -1.062425134715125641E-15, -0.9983585005135562351 ) ) ;
#38015 = CARTESIAN_POINT ( 'NONE',  ( -0.7500000000000249800, -1.027083332650516212, 1.299038105676659116 ) ) ;
#38017 = CARTESIAN_POINT ( 'NONE',  ( 2.121956728516772639, -2.140194184088719531, 0.5379336890513550795 ) ) ;
#38018 = ORIENTED_EDGE ( 'NONE', *, *, #31446, .F. ) ;
#38019 = B_SPLINE_CURVE_WITH_KNOTS ( 'NONE', 3,
 ( #72736, #25054, #108516, #8808, #74886, #122664 ),
 .UNSPECIFIED., .F., .F.,
 ( 4, 2, 4 ),
 ( 0.000000000000000000, 0.0001363166885564070553, 0.0002726333771128141106 ),
 .UNSPECIFIED. ) ;
#38020 = CARTESIAN_POINT ( 'NONE',  ( 3.923301836239755147, 8.994671190470434397, -0.7749999999999996891 ) ) ;
#38021 = CARTESIAN_POINT ( 'NONE',  ( 3.194917754314666514, 6.879154480009089134, 0.7998128361456321445 ) ) ;
#38022 = CARTESIAN_POINT ( 'NONE',  ( -5.773074481320628948, 5.629675071162500544, 0.000000000000000000 ) ) ;
#38023 = CARTESIAN_POINT ( 'NONE',  ( -7.860745937262166194, -5.389939693150854971, 7.694877102302390526 ) ) ;
#38024 = CARTESIAN_POINT ( 'NONE',  ( 6.684453674706574589, -1.933370886519528264, -0.3848441959667763257 ) ) ;
#38025 = CARTESIAN_POINT ( 'NONE',  ( 6.024106105913028308, -1.276746162841462695, -1.922164112325924989 ) ) ;
#38026 = CARTESIAN_POINT ( 'NONE',  ( 0.5374593765826127800, 1.831924746014142791, -0.7026076897959919743 ) ) ;
#38027 = CARTESIAN_POINT ( 'NONE',  ( 4.135635188098309101, 1.943850041002512352, -0.6901024340064102480 ) ) ;
#38028 = CARTESIAN_POINT ( 'NONE',  ( 6.046573322014824114, 7.117052299514516456, -1.082531754730543083 ) ) ;
#38029 = CARTESIAN_POINT ( 'NONE',  ( 3.464990776744291345, 6.200183785247111778, 1.199719254218452047 ) ) ;
#38030 =( BOUNDED_CURVE ( )  B_SPLINE_CURVE ( 2, ( #13815, #209877, #48482, #80960, #115647 ),
 .UNSPECIFIED., .F., .T. ) 
 B_SPLINE_CURVE_WITH_KNOTS ( ( 3, 2, 3 ),
 ( 0.02117536257016233020, 0.02500000000000000139, 0.02833227121364267215 ),
 .UNSPECIFIED. ) 
 CURVE ( )  GEOMETRIC_REPRESENTATION_ITEM ( )  RATIONAL_B_SPLINE_CURVE ( ( 0.9334640809516798754, 0.9385114893599890706, 1.000000000000000000, 0.9464272371605781942, 0.9356990284279831371 ) ) 
 REPRESENTATION_ITEM ( '' )  );
#38031 = CARTESIAN_POINT ( 'NONE',  ( 7.524412065460039933, 10.76193592880331984, -1.082531754730537976 ) ) ;
#38032 = CARTESIAN_POINT ( 'NONE',  ( -1.201851678989727383E-14, 4.009375000341416140, -1.575800808251660134 ) ) ;
#38033 = CARTESIAN_POINT ( 'NONE',  ( 1.419999999999990603, 6.120000000000041851, 2.500000000000000444 ) ) ;
#38034 = CARTESIAN_POINT ( 'NONE',  ( 4.894130264408854458, 6.732904613275549899, -1.443375672974051449 ) ) ;
#38035 = CARTESIAN_POINT ( 'NONE',  ( 6.777770921962916972, -2.107754466287181661, 0.5206637005944132479 ) ) ;
#38036 = APPLICATION_CONTEXT ( 'automotive_design' ) ;
#38038 = CARTESIAN_POINT ( 'NONE',  ( 4.950658015114751009, -1.558304906039936988, -0.9804572199803849308 ) ) ;
#38037 = DIRECTION ( 'NONE',  ( 0.000000000000000000, 1.000000000000000000, 0.000000000000000000 ) ) ;
#38039 = CARTESIAN_POINT ( 'NONE',  ( 11.84668729035180590, 12.59481419982586914, 1.399999999999998357 ) ) ;
#38040 = CARTESIAN_POINT ( 'NONE',  ( -2.493461049780994365, 3.507114751586604129, 11.73081193161140590 ) ) ;
#38041 = CARTESIAN_POINT ( 'NONE',  ( 0.4560483712790652233, 0.7097975879313439540, 1.730851494400275747 ) ) ;
#38043 = ADVANCED_FACE ( 'NONE', ( #189476 ), #27732, .T. ) ;
#38042 = CARTESIAN_POINT ( 'NONE',  ( -5.120997767102647202, 6.698429628811411796, 1.435921996857256300 ) ) ;
#38044 = CARTESIAN_POINT ( 'NONE',  ( -0.4000000000000243916, 3.000000000000566214, -2.023857702507757317 ) ) ;
#38045 = CARTESIAN_POINT ( 'NONE',  ( 5.713240515264599750, 7.403118591225121392, -1.316831503761767719 ) ) ;
#38046 = CARTESIAN_POINT ( 'NONE',  ( -1.264911064067348656, 3.850000000000018296, 0.5000000000000064393 ) ) ;
#38047 = CARTESIAN_POINT ( 'NONE',  ( 2.131405713275540847, -1.153620894759581184, -1.342296593837268848 ) ) ;
#38048 = CARTESIAN_POINT ( 'NONE',  ( 6.235026786510912800, 1.879206351595325231, 0.7223523585505615685 ) ) ;
#38050 = CARTESIAN_POINT ( 'NONE',  ( 4.517137023955775099, -1.749796063449124084, 0.7800368752974867759 ) ) ;
#38049 = CARTESIAN_POINT ( 'NONE',  ( -8.455481356417053007, 13.01647868246193518, 0.7998128361456341429 ) ) ;
#38051 = CARTESIAN_POINT ( 'NONE',  ( -0.1409997244346088141, 1.357410162930408504, -2.254437325861287533 ) ) ;
#38052 = CARTESIAN_POINT ( 'NONE',  ( 4.967230218399325103, 1.712698785223613740, 0.9724057732015491951 ) ) ;
#38054 = EDGE_CURVE ( 'NONE', #31895, #129718, #118327, .T. ) ;
#38053 = CARTESIAN_POINT ( 'NONE',  ( 6.310808155552376952, -0.5427901682961560059, -1.945386456709609524 ) ) ;
#38055 = CARTESIAN_POINT ( 'NONE',  ( 1.173530994449854870, -3.042800438942089514, 3.270848514539542506 ) ) ;
#38056 = CARTESIAN_POINT ( 'NONE',  ( 2.518242125168220102, 1.223528130051700025, -1.415109699333151561 ) ) ;
#38058 = ORIENTED_EDGE ( 'NONE', *, *, #89670, .T. ) ;
#38057 = CARTESIAN_POINT ( 'NONE',  ( 6.076716319674939193, -1.640139352550730401, -0.5342243915677049593 ) ) ;
#38060 = CARTESIAN_POINT ( 'NONE',  ( 4.202664430556261266, 4.005456045178151570, 0.7216878364870317197 ) ) ;
#38059 = CARTESIAN_POINT ( 'NONE',  ( 3.352369063006555905, 2.207063162671081713, 4.936380160885933677E-05 ) ) ;
#38061 = AXIS2_PLACEMENT_3D ( 'NONE', #788, #32270, #49578 ) ;
#38062 = CARTESIAN_POINT ( 'NONE',  ( 0.6823417656249899377, 3.155208333674754062, 1.181850606188765695 ) ) ;
#38063 = CARTESIAN_POINT ( 'NONE',  ( 0.8540550061131615411, -0.7440666694851668650, 1.923960566027690833 ) ) ;
#38065 = EDGE_CURVE ( 'NONE', #35700, #54210, #124420, .T. ) ;
#38064 = CARTESIAN_POINT ( 'NONE',  ( 7.396136491454752715, 8.587579647240744407, 1.199719254218462483 ) ) ;
#38066 = CARTESIAN_POINT ( 'NONE',  ( -8.503988664269602538, 10.94440607977979063, 1.599625672291269396 ) ) ;
#38067 = DIRECTION ( 'NONE',  ( 0.000000000000000000, 0.000000000000000000, -1.000000000000000000 ) ) ;
#38068 = CARTESIAN_POINT ( 'NONE',  ( -3.421105596467043153, -0.02305168933490822636, -0.4127856329643360134 ) ) ;
#38069 = CARTESIAN_POINT ( 'NONE',  ( -7.505515594164280380, -6.699677480913956096, -8.042162931142907922 ) ) ;
#38070 = CARTESIAN_POINT ( 'NONE',  ( 3.648938843998358106, -0.4010542052625790110, -2.030977206718207473 ) ) ;
#38071 = CARTESIAN_POINT ( 'NONE',  ( -0.7500000000000215383, 3.941666666666690411, 1.299038105676671107 ) ) ;
#38072 = CARTESIAN_POINT ( 'NONE',  ( 5.229694566569264680, 7.124396299129368337, 1.599625672291267398 ) ) ;
#38073 = CARTESIAN_POINT ( 'NONE',  ( -6.065932567686177279, 7.134227558401057934, 1.164772332933713184 ) ) ;
#38074 = CARTESIAN_POINT ( 'NONE',  ( 0.8033855960881201019, 1.780198652630104794, -0.9539489498650125521 ) ) ;
#38075 = CARTESIAN_POINT ( 'NONE',  ( 1.364683531249990311, 3.384375000341416140, 1.214306433183764966E-14 ) ) ;
#38076 = ORIENTED_EDGE ( 'NONE', *, *, #175553, .F. ) ;
#38078 = CARTESIAN_POINT ( 'NONE',  ( 9.747949258545622442, 10.47495501116581984, 0.000000000000000000 ) ) ;
#38077 = CARTESIAN_POINT ( 'NONE',  ( 0.1745949693968875116, 2.894395776691494060, -2.244452406707102110 ) ) ;
#38079 = CARTESIAN_POINT ( 'NONE',  ( 6.872432811717262169, -0.4447407475622888740, 1.973694069355651282 ) ) ;
#38080 = CARTESIAN_POINT ( 'NONE',  ( 6.315652784560811916, -1.257152391787072387, -1.445590397462018117 ) ) ;
#38081 = CARTESIAN_POINT ( 'NONE',  ( 6.639320575229288757, 4.694344378759712555, 2.565881548192010975 ) ) ;
#38082 = CARTESIAN_POINT ( 'NONE',  ( 3.280998142716429200, 1.980384277226649559, -0.9389412094223739125 ) ) ;
#38083 = CARTESIAN_POINT ( 'NONE',  ( 1.499999999999989120, 1.806250000682817269, 0.000000000000000000 ) ) ;
#38084 = CARTESIAN_POINT ( 'NONE',  ( 2.302860652515531292, -0.3306829512400177862, -1.883434002855538081 ) ) ;
#38085 = CARTESIAN_POINT ( 'NONE',  ( -6.227272627378437342, 6.159572908229946187, -0.7998128361456291469 ) ) ;
#38087 = CARTESIAN_POINT ( 'NONE',  ( 3.823036128929238942, 7.404033217152015567, 1.040834085586084257E-14 ) ) ;
#38086 = B_SPLINE_CURVE_WITH_KNOTS ( 'NONE', 3,
 ( #1328, #118371, #35981, #38130, #121593, #102062, #186499 ),
 .UNSPECIFIED., .F., .F.,
 ( 4, 3, 4 ),
 ( 0.0001126021369344445543, 0.001503110988946918273, 0.002006790696425510192 ),
 .UNSPECIFIED. ) ;
#38089 = CARTESIAN_POINT ( 'NONE',  ( 1.511342449054883241, -1.897691915346022329, 0.6820157586827847451 ) ) ;
#38088 = CARTESIAN_POINT ( 'NONE',  ( 3.558982665580148641, 7.338500189690928543, -0.2527556040902705359 ) ) ;
#38090 = CARTESIAN_POINT ( 'NONE',  ( 0.6823417656249969321, 10.58854166700806587, -1.181850606188757036 ) ) ;
#38092 = CARTESIAN_POINT ( 'NONE',  ( -4.655245641445871385, 6.524482229810530498, 1.599625672291263179 ) ) ;
#38091 = CARTESIAN_POINT ( 'NONE',  ( 5.759372899636661991, 2.159370146098410714, -0.3733810082120898044 ) ) ;
#38094 = ORIENTED_EDGE ( 'NONE', *, *, #179894, .T. ) ;
#38093 = CARTESIAN_POINT ( 'NONE',  ( 2.678358392608829686, -1.649718294651691730, -0.5031959223205755283 ) ) ;
#38095 = CARTESIAN_POINT ( 'NONE',  ( -0.1399997263889611598, 6.947783040739049731, -2.595329734540325006 ) ) ;
#38096 = CARTESIAN_POINT ( 'NONE',  ( 6.283314124929436417, 9.417951348137970413, -1.199719254218440723 ) ) ;
#38097 = CARTESIAN_POINT ( 'NONE',  ( 5.522248639467795428, 5.337044922334209573, -0.7998128361456231517 ) ) ;
#38098 = CARTESIAN_POINT ( 'NONE',  ( -1.360607927818985541, 13.37576698399828778, 0.2084529114367693059 ) ) ;
#38099 = CARTESIAN_POINT ( 'NONE',  ( 1.029656018189710309, 1.891699080040713410, -0.5197978237033785698 ) ) ;
#38100 = CARTESIAN_POINT ( 'NONE',  ( 1.123270288250308280, 2.922697346350005887, 0.7749999999993786304 ) ) ;
#38101 = CARTESIAN_POINT ( 'NONE',  ( 4.761938266897790761, 6.578680616179308771, 1.599625672291267398 ) ) ;
#38102 = CARTESIAN_POINT ( 'NONE',  ( 2.093037498677865482, 1.000000000000000888, -11.70868840297833025 ) ) ;
#38103 = CARTESIAN_POINT ( 'NONE',  ( -2.331034670843834533E-15, -5.530538574611992608, 11.29689844398642684 ) ) ;
#38104 = AXIS2_PLACEMENT_3D ( 'NONE', #64329, #195400, #63255 ) ;
#38105 = ORIENTED_EDGE ( 'NONE', *, *, #91274, .T. ) ;
#38106 = CARTESIAN_POINT ( 'NONE',  ( 3.633306742369224462, -0.1297899475344466980, 1.806866856981071967 ) ) ;
#38107 = ORIENTED_EDGE ( 'NONE', *, *, #146747, .T. ) ;
#38108 = CARTESIAN_POINT ( 'NONE',  ( 9.565441069641300587, 11.11843498845840905, -1.199719254218440723 ) ) ;
#38109 = CARTESIAN_POINT ( 'NONE',  ( 5.246079093845007257, 5.085123462432798114, 0.7998128361456352531 ) ) ;
#38110 = CARTESIAN_POINT ( 'NONE',  ( 4.582537834466095639, -1.179681096148448738, 1.374793604838970396 ) ) ;
#38111 = CARTESIAN_POINT ( 'NONE',  ( 5.682275777458829502, 9.643422483761748154, 0.7216878364870317197 ) ) ;
#38112 = CARTESIAN_POINT ( 'NONE',  ( -6.729185404178093854, -6.864242587301021103, -6.701130199342132165 ) ) ;
#38113 = CARTESIAN_POINT ( 'NONE',  ( 5.890517129559706078, 5.978185313570312687, -0.07684424279984919393 ) ) ;
#38115 = CARTESIAN_POINT ( 'NONE',  ( 0.6823417656249969321, 15.02604166700806410, -1.181850606188757036 ) ) ;
#38114 = CARTESIAN_POINT ( 'NONE',  ( 5.371493315669001234, -0.2729949515532895110, 1.840801060123838706 ) ) ;
#38116 = CARTESIAN_POINT ( 'NONE',  ( 2.354979200267411255, 0.09147625538302081583, -1.913532508166473800 ) ) ;
#38117 = DIRECTION ( 'NONE',  ( 5.578564026256490882E-16, 1.000000000000000000, 9.066213480720158442E-32 ) ) ;
#38118 = CARTESIAN_POINT ( 'NONE',  ( -4.392478581147607031, 7.108013530438723748, 1.082531754730560403 ) ) ;
#38119 = CARTESIAN_POINT ( 'NONE',  ( 7.592810154713589835E-16, -3.600000000000005862, -6.200000000000000178 ) ) ;
#38120 = CARTESIAN_POINT ( 'NONE',  ( -1.402160292154681736E-14, -1.178124999658576311, 1.575800808251672791 ) ) ;
#38121 = CARTESIAN_POINT ( 'NONE',  ( 7.619319141200072920, 7.991553207595983643, 0.7216878364870317197 ) ) ;
#38122 = CARTESIAN_POINT ( 'NONE',  ( -2.927671105547157371, 5.503034492191895666, 1.199719254218462483 ) ) ;
#38123 = CARTESIAN_POINT ( 'NONE',  ( -1.333315192109695957, 8.250054423670803772, 10.85938449304425468 ) ) ;
#38124 = CARTESIAN_POINT ( 'NONE',  ( 1.236401392562349155, 0.4093969531599008227, 2.049976805931138735 ) ) ;
#38125 = CARTESIAN_POINT ( 'NONE',  ( 6.554440917563797875, 6.611545590104705994, -0.7998128361456481317 ) ) ;
#38126 = CARTESIAN_POINT ( 'NONE',  ( 0.09436191691250192526, -0.3928898508825870439, -1.789253991261535726 ) ) ;
#38127 = CARTESIAN_POINT ( 'NONE',  ( -5.525111292768871252, 6.404716915440499037, -1.199719254218446718 ) ) ;
#38128 = CARTESIAN_POINT ( 'NONE',  ( 2.133574855335911291, -1.190200692204022470, -1.384352166806518625 ) ) ;
#38129 = ADVANCED_FACE ( 'NONE', ( #121452 ), #167982, .T. ) ;
#38130 = CARTESIAN_POINT ( 'NONE',  ( 10.56178662260467682, -8.763419982614969683, -0.1843566712554992049 ) ) ;
#38131 = CARTESIAN_POINT ( 'NONE',  ( 2.056764645581514728, 0.4224895836346024280, 1.864965418913032913 ) ) ;
#38132 = CARTESIAN_POINT ( 'NONE',  ( 1.943746065852373972, 1.356001085411572049, 1.428673526509681047 ) ) ;
#38133 = CARTESIAN_POINT ( 'NONE',  ( 3.333474266508968054, 0.8707927262202612706, -1.735945723835415677 ) ) ;
#38134 = EDGE_LOOP ( 'NONE', ( #213338, #5000 ) ) ;
#38135 = CARTESIAN_POINT ( 'NONE',  ( 1.084637062511528693, 3.273878807974804683, 1.105835307554807301 ) ) ;
#38136 = CARTESIAN_POINT ( 'NONE',  ( -4.142898457427624415, 6.991076079377632091, 1.199719254218452935 ) ) ;
#38138 = CARTESIAN_POINT ( 'NONE',  ( 3.814780496183818315, -0.6684712460508880350, -2.012520831323429515 ) ) ;
#38137 = CARTESIAN_POINT ( 'NONE',  ( 3.736153849017632922, 6.516540702899320081, -1.199719254218453823 ) ) ;
#38139 = CARTESIAN_POINT ( 'NONE',  ( 6.645879322773626363, -6.896483513897670115, 6.785280070212115433 ) ) ;
#38140 = CARTESIAN_POINT ( 'NONE',  ( 8.585337585951586803, 11.03931315507545108, -1.599625672291255185 ) ) ;
#38141 = CARTESIAN_POINT ( 'NONE',  ( -5.936491157937300756, 8.019268665717216749, 1.599625672291263179 ) ) ;
#38142 = PLANE ( 'NONE',  #97876 ) ;
#38143 = CARTESIAN_POINT ( 'NONE',  ( 5.417364897112183719, 8.477953592343014932, 1.199719254218451159 ) ) ;
#38144 = LINE ( 'NONE', #87957, #2659 ) ;
#38147 = EDGE_CURVE ( 'NONE', #138513, #156724, #208790, .T. ) ;
#38146 = CARTESIAN_POINT ( 'NONE',  ( 6.122279814772176643, 1.995267444086584296, 0.2910868170948808786 ) ) ;
#38145 = CARTESIAN_POINT ( 'NONE',  ( 3.668406916800326822, -1.225078373119499187, 1.353803248016255178 ) ) ;
#38148 = DIRECTION ( 'NONE',  ( 0.000000000000000000, 0.000000000000000000, -1.000000000000000000 ) ) ;
#38149 = CARTESIAN_POINT ( 'NONE',  ( -10.00555417720528872, 10.77549408293541866, 0.7216878364870438212 ) ) ;
#38150 = CARTESIAN_POINT ( 'NONE',  ( -4.589286827423546100, 8.493149336607261901, 0.1385767598228414277 ) ) ;
#38151 = CARTESIAN_POINT ( 'NONE',  ( 6.925078400183575233, 7.629137130509070275, 2.455651831298297338 ) ) ;
#38152 = CARTESIAN_POINT ( 'NONE',  ( 4.328871119428026049, 0.09166491666120352155, 1.868520897946590598 ) ) ;
#38153 = CARTESIAN_POINT ( 'NONE',  ( 6.753933077901968396, 11.03133902419432566, 0.7998128361456462443 ) ) ;
#38154 = CARTESIAN_POINT ( 'NONE',  ( 1.734862838405337060, 0.1885825406544305305, 1.917253122483292715 ) ) ;
#38155 = CARTESIAN_POINT ( 'NONE',  ( -0.02374884625625755044, 2.800000000000025135, 1.413344025506580337 ) ) ;
#38156 = CARTESIAN_POINT ( 'NONE',  ( -1.364683531250014514, 8.651041667008065872, -0.7879004041258335089 ) ) ;
#38157 = CARTESIAN_POINT ( 'NONE',  ( -6.901263884555985051, 8.010228272525461435, 1.199719254218450271 ) ) ;
#38158 = CARTESIAN_POINT ( 'NONE',  ( 3.551346171775753735, 6.230655402791975384, 1.199719254218462483 ) ) ;
#38159 = CARTESIAN_POINT ( 'NONE',  ( -4.082413651046300274, 6.816547455312373494, 1.082531754730549967 ) ) ;
#38160 = CARTESIAN_POINT ( 'NONE',  ( 0.8962975493561256002, -0.9559892387472949116, -1.889204697816506240 ) ) ;
#38161 = CARTESIAN_POINT ( 'NONE',  ( 10.21336978979620191, 10.81001959771741205, 0.7998128361456462443 ) ) ;
#38162 = CARTESIAN_POINT ( 'NONE',  ( 0.3697396242580934245, 6.943430631093202798, 3.891240841457444866 ) ) ;
#38163 = CARTESIAN_POINT ( 'NONE',  ( 4.803616497939601437, -1.596918191575155133, -1.317456641179854726 ) ) ;
#38165 = CARTESIAN_POINT ( 'NONE',  ( 4.499659979152191625, 7.015106111828595559, -1.153029749421132566 ) ) ;
#38164 = CARTESIAN_POINT ( 'NONE',  ( 0.2570343420702363435, 1.821350608449383124, -0.2692129421619017804 ) ) ;
#38166 = CARTESIAN_POINT ( 'NONE',  ( 5.256544959696739738, 2.216068975266134000, -0.6104820095701003480 ) ) ;
#38167 = CARTESIAN_POINT ( 'NONE',  ( 5.666945020832167224, 8.594891043404107478, 1.082531754730558626 ) ) ;
#38169 = CARTESIAN_POINT ( 'NONE',  ( 1.500000000000001332, 9.656250000682799595, 0.000000000000000000 ) ) ;
#38168 = CARTESIAN_POINT ( 'NONE',  ( 4.177320726786311056, 5.966903162707725805, -1.443375672974068769 ) ) ;
#38170 = CARTESIAN_POINT ( 'NONE',  ( 1.711265200625663008, -0.2773638578843647950, 2.275360193931966535 ) ) ;
#38172 = EDGE_CURVE ( 'NONE', #83910, #154420, #58803, .T. ) ;
#38171 = CARTESIAN_POINT ( 'NONE',  ( -0.001932266794912151702, -9.922538451904662438, -9.579662758527177857 ) ) ;
#38173 = CARTESIAN_POINT ( 'NONE',  ( -6.099189001301292379, 8.209082816308541197, 1.599625672291263179 ) ) ;
#38174 = CARTESIAN_POINT ( 'NONE',  ( 5.999939506776140519, -0.7010436009657755596, -1.811167765765375526 ) ) ;
#38175 = ORIENTED_EDGE ( 'NONE', *, *, #178570, .F. ) ;
#38176 = CARTESIAN_POINT ( 'NONE',  ( 7.415946836550712185, 10.63539316174243865, 1.082531754730558626 ) ) ;
#38177 = ADVANCED_FACE ( 'NONE', ( #75813 ), #58620, .T. ) ;
#38178 = CARTESIAN_POINT ( 'NONE',  ( -0.07006079923273231258, -1.973546630392996493, 0.3967976802892440036 ) ) ;
#38179 = CARTESIAN_POINT ( 'NONE',  ( 5.841029835422532734, -1.731992920607817288, -1.032484497598872064 ) ) ;
#38181 = CYLINDRICAL_SURFACE ( 'NONE', #29635, 0.7499999999999997780 ) ;
#38180 = CARTESIAN_POINT ( 'NONE',  ( -8.552495972122143186, 8.872333477097637200, 0.7998128361456462443 ) ) ;
#38182 = CARTESIAN_POINT ( 'NONE',  ( 3.285556943749998737, -2.442708332855375364, -1.896917185911906500 ) ) ;
#38184 = CARTESIAN_POINT ( 'NONE',  ( 0.9886869571070689977, 1.563518247070281086, -0.8293041508813036033 ) ) ;
#38183 = CARTESIAN_POINT ( 'NONE',  ( 2.994169869935947137, -0.6075897704641713970, -2.000389221998987832 ) ) ;
#38185 = CARTESIAN_POINT ( 'NONE',  ( 6.451795992440088057, -1.844709169062180409, -0.8146298745319994206 ) ) ;
#38187 = CARTESIAN_POINT ( 'NONE',  ( 3.767766022312348362, 1.272560033980062455, 1.906398719306565681 ) ) ;
#38186 = CARTESIAN_POINT ( 'NONE',  ( 4.411198876399872404, 6.239761003923544713, -1.599625672291273171 ) ) ;
#38188 = CARTESIAN_POINT ( 'NONE',  ( 3.609068157710407565, -1.714216318138677808, 0.2993142247325294991 ) ) ;
#38189 = CARTESIAN_POINT ( 'NONE',  ( 2.758194185376297902, 5.305311418659259814, 1.199719254218452047 ) ) ;
#38190 = CARTESIAN_POINT ( 'NONE',  ( -2.680920047035027842, -0.4882345588269855763, -0.09999999999999592548 ) ) ;
#38191 = CARTESIAN_POINT ( 'NONE',  ( 1.915017753259074862, 0.5389909111754992432, 1.648018863455216643 ) ) ;
#38192 = CARTESIAN_POINT ( 'NONE',  ( 3.912682095371947444, 0.7780703539225676257, 2.027152283489948026 ) ) ;
#38193 = CARTESIAN_POINT ( 'NONE',  ( 5.359550796103802028, 5.147230771742885125, -0.7998128361456231517 ) ) ;
#38194 = CARTESIAN_POINT ( 'NONE',  ( 4.118375227313908482, 1.978554835517082555, 0.3886342876525810119 ) ) ;
#38195 = CARTESIAN_POINT ( 'NONE',  ( 2.593750000000001776, -1.895863743164140525, -0.7852924748298559798 ) ) ;
#38196 = CARTESIAN_POINT ( 'NONE',  ( -1.499999999999997780, 2.181250000682817713, 1.214306433183764966E-14 ) ) ;
#38197 = CARTESIAN_POINT ( 'NONE',  ( 0.9559316444634465837, 1.924326902252432081, -0.09161688492189544453 ) ) ;
#38198 = CARTESIAN_POINT ( 'NONE',  ( 0.7500000000000006661, 8.614583334016129967, 1.299038105676657340 ) ) ;
#38199 = CARTESIAN_POINT ( 'NONE',  ( 4.605860659110106781, 1.647066397540638993, 1.490795591097130002 ) ) ;
#38200 = VERTEX_POINT ( 'NONE', #79004 ) ;
#38201 = CARTESIAN_POINT ( 'NONE',  ( -0.1106856583840877539, 4.089587022985669229, -2.551888050631024640 ) ) ;
#38202 = CARTESIAN_POINT ( 'NONE',  ( 0.7499999999999902300, 1.733333333333357595, 1.299038105676657340 ) ) ;
#38203 = CARTESIAN_POINT ( 'NONE',  ( 8.288111976655649471, 8.563885482386732306, -0.7998128361456291469 ) ) ;
#38204 = CARTESIAN_POINT ( 'NONE',  ( 4.650083499362875017, 5.487814173087225633, 1.082531754730560403 ) ) ;
#38205 = CARTESIAN_POINT ( 'NONE',  ( 3.285556943749998737, -0.9552083328553737651, -1.896917185911906722 ) ) ;
#38206 = CARTESIAN_POINT ( 'NONE',  ( 1.049838644336478000, -2.005893928647552116, 0.9545428114200222858 ) ) ;
#38208 = CARTESIAN_POINT ( 'NONE',  ( 5.353941776413853937, -0.7077614321437855072, 1.829919609802006741 ) ) ;
#38207 = CIRCLE ( 'NONE', #72675, 0.8299999999999999600 ) ;
#38209 = CARTESIAN_POINT ( 'NONE',  ( 8.242994207428692377, 12.56065097540143327, -0.7216878364870328300 ) ) ;
#38210 = SURFACE_STYLE_USAGE ( .BOTH. , #149836 ) ;
#38211 = CARTESIAN_POINT ( 'NONE',  ( 0.2105424042340813540, -0.9235240298187572527, -1.952328634516012684 ) ) ;
#38212 = CARTESIAN_POINT ( 'NONE',  ( -4.150204419558982671, 7.856005899545188242, 0.7216878364870338292 ) ) ;
#38213 = CARTESIAN_POINT ( 'NONE',  ( 3.736832797123919025, -1.987151705994869344, -0.5527697292582544053 ) ) ;
#38214 = CARTESIAN_POINT ( 'NONE',  ( -3.906720819032141190, 7.709591388846142479, -0.7998128361456281477 ) ) ;
#38215 = CARTESIAN_POINT ( 'NONE',  ( -1.201851678989727383E-14, 3.743750000682817269, 1.732050807568877637 ) ) ;
#38216 = CARTESIAN_POINT ( 'NONE',  ( -0.6823417656250212460, 5.613541667008087543, 1.181850606188767472 ) ) ;
#38217 = CARTESIAN_POINT ( 'NONE',  ( 4.534354090784907143, 1.834037221929617711, 0.3668691113338993226 ) ) ;
#38218 = CARTESIAN_POINT ( 'NONE',  ( 3.621445620172254021, 0.2585195360361118300, 1.714627356041095840 ) ) ;
#38219 = CARTESIAN_POINT ( 'NONE',  ( 3.069568678616676927, -1.034394858748697743, 1.399543075413912430 ) ) ;
#38220 = CARTESIAN_POINT ( 'NONE',  ( 0.9434182766495626815, -1.811351811004081158, -1.404917595322150659 ) ) ;
#38221 = CARTESIAN_POINT ( 'NONE',  ( 0.6823417656249899377, 4.488541667008086655, -1.181850606188754593 ) ) ;
#38222 = CARTESIAN_POINT ( 'NONE',  ( 4.441018442196864591, -1.617167385086373033, -1.325159661343593420 ) ) ;
#38223 = CARTESIAN_POINT ( 'NONE',  ( 0.4800843290509413386, -0.2225996465644273503, -1.827572303103291551 ) ) ;
#38224 = CARTESIAN_POINT ( 'NONE',  ( 0.08058962652511190983, -9.910877166163974294, 10.99970478295254850 ) ) ;
#38225 = CARTESIAN_POINT ( 'NONE',  ( 1.863907939170056149, -0.1017519224979606118, -2.013985838549677609 ) ) ;
#38226 = CARTESIAN_POINT ( 'NONE',  ( 0.3225714733509216781, 2.098294765757203528, 0.6321472216322538973 ) ) ;
#38227 = CARTESIAN_POINT ( 'NONE',  ( 8.255390768298678239, 13.81349006448566996, -9.579378744720992600 ) ) ;
#38228 = CARTESIAN_POINT ( 'NONE',  ( -7.771848369131641121, 10.09024240211882351, -1.599625672291263179 ) ) ;
#38229 = CARTESIAN_POINT ( 'NONE',  ( 6.819914962873951936, 7.915321197229798322, -1.199719254218446718 ) ) ;
#38230 = CARTESIAN_POINT ( 'NONE',  ( 2.543736517606724146, -1.977637755382474438, 0.7655657148115800892 ) ) ;
#38231 = FACE_OUTER_BOUND ( 'NONE', #138444, .T. ) ;
#38232 = CARTESIAN_POINT ( 'NONE',  ( 4.389149243953620605, 1.629682310347341456, -0.8231139397327084106 ) ) ;
#38233 = ADVANCED_FACE ( 'NONE', ( #59555 ), #177041, .T. ) ;
#38234 = EDGE_LOOP ( 'NONE', ( #4085, #133702, #206823, #64106 ) ) ;
#38235 = CARTESIAN_POINT ( 'NONE',  ( -5.447343857640614573, 9.577261277214532242, -0.7998128361456362523 ) ) ;
#38236 = FACE_OUTER_BOUND ( 'NONE', #195230, .T. ) ;
#38237 = CARTESIAN_POINT ( 'NONE',  ( 1.737500000000001155, -4.039583332377416625, 3.009438278150922130 ) ) ;
#38238 = CARTESIAN_POINT ( 'NONE',  ( -5.520141099058386125, 9.591915048876776595, 0.000000000000000000 ) ) ;
#38239 = CARTESIAN_POINT ( 'NONE',  ( 1.933859055862125809, -1.958050917679872160, 0.4949566823095867263 ) ) ;
#38240 = CARTESIAN_POINT ( 'NONE',  ( 6.141676493652540536, -1.594220855400224401, -1.526124331276897950 ) ) ;
#38241 = CARTESIAN_POINT ( 'NONE',  ( -3.526002468005825286, 6.271364091718859335, -1.199719254218450271 ) ) ;
#38242 = CARTESIAN_POINT ( 'NONE',  ( 4.469486699700035537, -0.3212591861478170663, 1.832842066241076040 ) ) ;
#38243 = CARTESIAN_POINT ( 'NONE',  ( 10.05067194643221207, 10.62020544712608938, 0.7998128361456462443 ) ) ;
#38244 = CARTESIAN_POINT ( 'NONE',  ( 11.43204722947019825, 9.944072459738245939, 3.649275849833181429 ) ) ;
#38245 = VERTEX_POINT ( 'NONE', #69425 ) ;
#38246 = CARTESIAN_POINT ( 'NONE',  ( -3.418627288940168096, 7.140148937072163804, -0.7998128361456281477 ) ) ;
#38247 = CARTESIAN_POINT ( 'NONE',  ( -8.505042434474312074, 8.816971016508505343, -0.7998128361456291469 ) ) ;
#38249 = ADVANCED_FACE ( 'NONE', ( #135531 ), #213062, .T. ) ;
#38248 = CARTESIAN_POINT ( 'NONE',  ( 4.951681858558426796, 0.5695450498939165218, -1.734646904759745700 ) ) ;
#38251 = CARTESIAN_POINT ( 'NONE',  ( -4.371234765837696656, 7.372762773471292164, -1.195546268109607846 ) ) ;
#38250 = CARTESIAN_POINT ( 'NONE',  ( -3.332271893908731464, 7.109677319527304640, -0.7998128361456481317 ) ) ;
#38252 = CARTESIAN_POINT ( 'NONE',  ( 1.364683531249988757, -0.6156249996585803075, 0.000000000000000000 ) ) ;
#38253 = CARTESIAN_POINT ( 'NONE',  ( 0.5086469178660666390, 1.728604602589098205, 0.1357594709466679594 ) ) ;
#38254 = CARTESIAN_POINT ( 'NONE',  ( 0.4095771458324704573, 1.203761932438538462, -1.257115261623420022 ) ) ;
#38255 = CARTESIAN_POINT ( 'NONE',  ( 5.514422467339478828, -1.033062203415137992, -2.063637023464809594 ) ) ;
#38256 = CARTESIAN_POINT ( 'NONE',  ( 6.039231080244466199, 6.010467446565510130, 0.7998128361456352531 ) ) ;
#38257 = CARTESIAN_POINT ( 'NONE',  ( 1.212264220565926198, -0.9239156619155285410, -1.842110158844072698 ) ) ;
#38258 = CARTESIAN_POINT ( 'NONE',  ( 5.952193131599331721, 6.902979060742733708, 1.199719254218462483 ) ) ;
#38259 = CARTESIAN_POINT ( 'NONE',  ( 6.661448219487969169, -0.6026422599177021500, -2.217949877449727047 ) ) ;
#38260 = LINE ( 'NONE', #171458, #165598 ) ;
#38261 = CARTESIAN_POINT ( 'NONE',  ( -5.478376588373717659, 8.549133898814758936, -1.199719254218452047 ) ) ;
#38262 = CARTESIAN_POINT ( 'NONE',  ( 5.172658500931742509, -1.761684834526537680, -0.6294727512598657926 ) ) ;
#38264 = CARTESIAN_POINT ( 'NONE',  ( -6.102578539926875933, 10.13377570664109051, 0.7216878364870267237 ) ) ;
#38263 = CARTESIAN_POINT ( 'NONE',  ( 3.849791259674230748, -1.322437695595569673, -1.381667681676468140 ) ) ;
#38265 = CARTESIAN_POINT ( 'NONE',  ( 4.899154391205060577, 1.836108854712194649, -1.224054507610386366 ) ) ;
#38266 = CARTESIAN_POINT ( 'NONE',  ( -4.957638175832625493E-14, 1.375000000682762291, 1.414508159514551444 ) ) ;
#38267 = CARTESIAN_POINT ( 'NONE',  ( -6.089020385868850305, 10.11795786024005572, -0.7216878364870338292 ) ) ;
#38268 = CARTESIAN_POINT ( 'NONE',  ( 3.729901657090948230, 6.405283462364505631, 1.082531754730549078 ) ) ;
#38269 = CARTESIAN_POINT ( 'NONE',  ( -6.251718229232867685, 6.466295153626015590, -0.7216878364870338292 ) ) ;
#38270 = CARTESIAN_POINT ( 'NONE',  ( 5.778019675193696969, 2.089136139637823852, -0.3624112956793351659 ) ) ;
#38271 = ORIENTED_EDGE ( 'NONE', *, *, #13673, .T. ) ;
#38272 = CARTESIAN_POINT ( 'NONE',  ( 3.294260915971382264, -0.9370450057796105847, 2.108945393182542372 ) ) ;
#38273 = CARTESIAN_POINT ( 'NONE',  ( 3.402741375674179114, 0.4741672551989496998, 1.903589013717405853 ) ) ;
#38274 = CARTESIAN_POINT ( 'NONE',  ( -4.285259070371116863, 7.157163461145040095, 1.199719254218452935 ) ) ;
#38275 = CARTESIAN_POINT ( 'NONE',  ( 0.5671465430379521999, 1.703994235754960451, 0.9719838849941149217 ) ) ;
#38276 = CARTESIAN_POINT ( 'NONE',  ( 9.167018891879168407, 14.15818339566316908, 7.673511198540157174 ) ) ;
#38277 = CARTESIAN_POINT ( 'NONE',  ( -9.497949338412174924, 15.41976506893289134, 7.334250928090418675 ) ) ;
#38278 = ORIENTED_EDGE ( 'NONE', *, *, #113945, .F. ) ;
#38279 = CARTESIAN_POINT ( 'NONE',  ( 5.788296071918774821, -0.7303023681345042206, -1.879805717804765353 ) ) ;
#38280 = CARTESIAN_POINT ( 'NONE',  ( -7.635213062790267458, 12.05949900656400686, 0.000000000000000000 ) ) ;
#38281 = FILL_AREA_STYLE_COLOUR ( '', #161727 ) ;
#38282 = CARTESIAN_POINT ( 'NONE',  ( 3.520551232162504540, 0.9717998864677798165, 1.941468132180910189 ) ) ;
#38283 = CARTESIAN_POINT ( 'NONE',  ( 4.420840606507738357, 7.315341919971147355, 1.199719254218451159 ) ) ;
#38284 = CARTESIAN_POINT ( 'NONE',  ( 1.125412309253082332, 1.872817075645373697, 0.9946839901537674056 ) ) ;
#38285 = CARTESIAN_POINT ( 'NONE',  ( -0.7500000000000215383, 1.222916667349485564, 1.299038105676659116 ) ) ;
#38286 = CARTESIAN_POINT ( 'NONE',  ( 10.05353459973327368, 11.68787744023238417, -1.199719254218440723 ) ) ;
#38287 = CARTESIAN_POINT ( 'NONE',  ( 11.97302537858606897, 13.79875989808017778, -0.8111997896467577629 ) ) ;
#38288 = CARTESIAN_POINT ( 'NONE',  ( 5.260375520412221562, 7.786458765878076171, 1.288147692060326532 ) ) ;
#38289 = CARTESIAN_POINT ( 'NONE',  ( 0.5091468516268854438, 1.791808316595304040, 1.017857635437851904 ) ) ;
#38291 = CARTESIAN_POINT ( 'NONE',  ( 6.827182134110200806, 4.698030009824885056, 2.473619993765368008 ) ) ;
#38290 = DIRECTION ( 'NONE',  ( 0.000000000000000000, 1.000000000000000000, 0.000000000000000000 ) ) ;
#38292 = CARTESIAN_POINT ( 'NONE',  ( 1.364683531249988757, 1.384375000341421469, 0.000000000000000000 ) ) ;
#38293 = CARTESIAN_POINT ( 'NONE',  ( 0.000000000000000000, -0.4330127018922214077, -6.200000000000000178 ) ) ;
#38294 = ORIENTED_EDGE ( 'NONE', *, *, #56710, .T. ) ;
#38295 = CARTESIAN_POINT ( 'NONE',  ( 4.934190575774549892, -1.026228162776990249, -1.613408319405706504 ) ) ;
#38296 = CARTESIAN_POINT ( 'NONE',  ( 5.278098682986631651, -0.9809853834585824384, 1.472868624863521880 ) ) ;
#38297 = CARTESIAN_POINT ( 'NONE',  ( 5.875479466675786355, 7.948088359245467416, -1.599625672291283607 ) ) ;
#38298 = CARTESIAN_POINT ( 'NONE',  ( -2.754277761870538299, 6.365074488824250309, 1.040834085586084257E-14 ) ) ;
#38299 = CARTESIAN_POINT ( 'NONE',  ( 0.6854714705560975840, 1.745592605935637920, -0.4840870370880663853 ) ) ;
#38301 = CARTESIAN_POINT ( 'NONE',  ( 0.9717394072371825509, -0.8581575513351351603, 1.712793540333819919 ) ) ;
#38300 = CARTESIAN_POINT ( 'NONE',  ( -6.781144757626070607, -7.161464053357452286, 6.776370306708066060 ) ) ;
#38302 = CARTESIAN_POINT ( 'NONE',  ( 2.260293373024503616, -2.069953001785612479, 0.04851313490940312168 ) ) ;
#38303 = CARTESIAN_POINT ( 'NONE',  ( 1.364683531249988757, -0.05312499965857975237, 0.000000000000000000 ) ) ;
#38304 = EDGE_CURVE ( 'NONE', #98224, #81410, #33100, .T. ) ;
#38305 = CARTESIAN_POINT ( 'NONE',  ( 0.1277242839827036902, -1.211146277544056460, -1.556326691921037675 ) ) ;
#38306 = CARTESIAN_POINT ( 'NONE',  ( 2.560947663861262491, -1.588335953301520220, -0.9000364273514869229 ) ) ;
#38308 = CARTESIAN_POINT ( 'NONE',  ( 6.365646016822680942, 6.829858545691475769, 0.5939985411197836740 ) ) ;
#38307 = CARTESIAN_POINT ( 'NONE',  ( -0.004676085075996058368, -0.5178430341337829645, -2.257629771169813448 ) ) ;
#38309 = CARTESIAN_POINT ( 'NONE',  ( -1.402160292154681736E-14, 0.5718750003414239114, 1.575800808251672791 ) ) ;
#38310 = CARTESIAN_POINT ( 'NONE',  ( 3.965324414628346172, 1.767556376804786611, 1.063002922270523953 ) ) ;
#38311 = CARTESIAN_POINT ( 'NONE',  ( -6.307567778855718288, 8.381915046796901692, -1.599625672291263179 ) ) ;
#38312 = CARTESIAN_POINT ( 'NONE',  ( 7.456094412511537151, 10.78619501698377370, 1.199719254218460707 ) ) ;
#38313 = CARTESIAN_POINT ( 'NONE',  ( 4.168242161197552420, 6.950367390450747251, -1.199719254218452047 ) ) ;
#38314 = AXIS2_PLACEMENT_3D ( 'NONE', #100026, #3557, #54477 ) ;
#38315 = CARTESIAN_POINT ( 'NONE',  ( 6.030679399980265920, 5.930214142932100252, -0.7998128361456281477 ) ) ;
#38316 = CARTESIAN_POINT ( 'NONE',  ( 1.499999999999989120, 4.004166666666685970, 0.8660254037844524744 ) ) ;
#38317 = CARTESIAN_POINT ( 'NONE',  ( 6.760220206081136496, -2.069995208266177666, 0.04663682477341199450 ) ) ;
#38318 = CARTESIAN_POINT ( 'NONE',  ( -1.402160292154681736E-14, 1.009375000341417916, -1.575800808251659024 ) ) ;
#38319 = CARTESIAN_POINT ( 'NONE',  ( 3.251412196806032995, -1.765091617811213931, -1.247493029685270649 ) ) ;
#38320 = CARTESIAN_POINT ( 'NONE',  ( 4.178382104804970076, 0.9538709814062135139, 1.780240436319034503 ) ) ;
#38321 = CARTESIAN_POINT ( 'NONE',  ( 6.720655732516655156, 7.629137130509086262, 2.873739711112702544 ) ) ;
#38322 = EDGE_CURVE ( 'NONE', #70347, #185939, #159703, .T. ) ;
#38325 = CARTESIAN_POINT ( 'NONE',  ( 6.805829924380108586, 8.963220883242035697, 1.443375672974076540 ) ) ;
#38324 = CARTESIAN_POINT ( 'NONE',  ( -3.285556943750000070, -3.259374999522044014, 0.000000000000000000 ) ) ;
#38323 = LINE ( 'NONE', #37255, #97546 ) ;
#38326 = CARTESIAN_POINT ( 'NONE',  ( -4.294900800479008574, 8.232744377192641849, 0.000000000000000000 ) ) ;
#38327 = CARTESIAN_POINT ( 'NONE',  ( 2.448454179885679149, -1.387098808145654560, 1.463928423225707931 ) ) ;
#38328 = CARTESIAN_POINT ( 'NONE',  ( -7.389357414647957256, 8.579670724299436557, 1.199719254218450271 ) ) ;
#38329 = CARTESIAN_POINT ( 'NONE',  ( -5.251085567194491155, 5.020688004682002159, -0.7998128361456221525 ) ) ;
#38330 = CARTESIAN_POINT ( 'NONE',  ( 0.000000000000000000, -3.600000000000005862, 0.000000000000000000 ) ) ;
#38331 = CARTESIAN_POINT ( 'NONE',  ( 5.941656858135132779, -1.798430535887390658, 0.6506349336675710804 ) ) ;
#38332 = DIRECTION ( 'NONE',  ( 1.000000000000000000, -7.771561172376096769E-16, -4.440892098500627148E-16 ) ) ;
#38334 = CARTESIAN_POINT ( 'NONE',  ( 4.429314653828757109, -1.560513098751922900, -1.277029310785951388 ) ) ;
#38333 = CARTESIAN_POINT ( 'NONE',  ( -9.151390499099978371, 9.778969791812544443, 0.7216878364870438212 ) ) ;
#38335 = CARTESIAN_POINT ( 'NONE',  ( -0.7499999999999972244, 5.358333333333353821, -1.299038105676652011 ) ) ;
#38336 = B_SPLINE_CURVE_WITH_KNOTS ( 'NONE', 3,
 ( #212304, #100696, #133236, #49820, #33565, #183010 ),
 .UNSPECIFIED., .F., .F.,
 ( 4, 2, 4 ),
 ( 0.000000000000000000, 0.001225895755212360379, 0.002451791510424721193 ),
 .UNSPECIFIED. ) ;
#38337 = CARTESIAN_POINT ( 'NONE',  ( -1.364683531250014514, 15.15104166700806587, -0.7879004041258335089 ) ) ;
#38338 = CARTESIAN_POINT ( 'NONE',  ( 6.493153095729292446, 1.497681883954028237, -0.8552637798607003461 ) ) ;
#38339 = CARTESIAN_POINT ( 'NONE',  ( 6.225128807330042591, 7.291680359087043151, -1.199719254218452047 ) ) ;
#38340 = CARTESIAN_POINT ( 'NONE',  ( 9.910647101909615841, 10.66476916175714607, 0.000000000000000000 ) ) ;
#38341 = STYLED_ITEM ( 'NONE', ( #79887 ), #169543 ) ;
#38342 = CARTESIAN_POINT ( 'NONE',  ( 10.91962425643211709, -9.999999999999998224, -0.09058751758337030280 ) ) ;
#38343 = CARTESIAN_POINT ( 'NONE',  ( 5.342975940791072631, -1.604858128155508101, 0.9606422304059699657 ) ) ;
#38344 = CARTESIAN_POINT ( 'NONE',  ( 6.170187344554162401, 2.007508049254663529, -0.1525455265532823512 ) ) ;
#38345 = CARTESIAN_POINT ( 'NONE',  ( 2.641538584800803502, 1.894577224340647792, -0.8349662684224224973 ) ) ;
#38346 = CARTESIAN_POINT ( 'NONE',  ( 0.4019237886466816012, 12.45758545099816850, -1.499999999999998668 ) ) ;
#38347 = ORIENTED_EDGE ( 'NONE', *, *, #164350, .F. ) ;
#38348 = CARTESIAN_POINT ( 'NONE',  ( 9.693716643646590470, 12.33242205571964512, 1.443375672974076540 ) ) ;
#38349 = CARTESIAN_POINT ( 'NONE',  ( 0.5093889453341126083, -1.913797760093600919, 0.6352206787166372326 ) ) ;
#38350 = CARTESIAN_POINT ( 'NONE',  ( 4.597623488365603528, 5.496887170248887067, -1.082531754730548412 ) ) ;
#38351 = PLANE ( 'NONE',  #173358 ) ;
#38352 = CARTESIAN_POINT ( 'NONE',  ( 9.205623113554628034, 9.842241175342985926, 0.7216878364870458196 ) ) ;
#38353 = CARTESIAN_POINT ( 'NONE',  ( 8.288111976655649471, 8.563885482386732306, -0.7998128361456291469 ) ) ;
#38355 = CARTESIAN_POINT ( 'NONE',  ( 5.694928174475800908, 1.691819642972839599, 0.8984594094828317612 ) ) ;
#38354 = CARTESIAN_POINT ( 'NONE',  ( -6.715366157470410435, 6.729015360003925750, -0.7998128361456291469 ) ) ;
#38356 = CARTESIAN_POINT ( 'NONE',  ( 1.499999999999990896, 5.025000000000022560, 1.214306433183765124E-14 ) ) ;
#38357 = CARTESIAN_POINT ( 'NONE',  ( 0.2999999999999860556, 3.999999999999996447, 0.9782388782688545836 ) ) ;
#38358 = CARTESIAN_POINT ( 'NONE',  ( 1.364683531249988757, -0.5531249996585801965, 0.000000000000000000 ) ) ;
#38360 = ORIENTED_EDGE ( 'NONE', *, *, #4172, .T. ) ;
#38359 = CARTESIAN_POINT ( 'NONE',  ( 2.250290310188348464, 5.569163095287620990, 0.7216878364870438212 ) ) ;
#38361 = CARTESIAN_POINT ( 'NONE',  ( -2.625475302540713152, 6.214804952939456228, -0.7998128361456281477 ) ) ;
#38362 = CARTESIAN_POINT ( 'NONE',  ( 2.465889518630470789, 2.120156730345585938, -0.4209195040108040797 ) ) ;
#38363 = CARTESIAN_POINT ( 'NONE',  ( -3.984117037569407938, 5.741498858621315371, 1.599625672291270506 ) ) ;
#38364 = CARTESIAN_POINT ( 'NONE',  ( 7.200788982633824276, 7.573544365927161515, 0.000000000000000000 ) ) ;
#38365 = CARTESIAN_POINT ( 'NONE',  ( 0.6332531790259123827, 1.961634380476449335, 0.8060562103610890983 ) ) ;
#38366 = CARTESIAN_POINT ( 'NONE',  ( 5.245057492501287832, -1.564903486862476489, 0.9398553879134128319 ) ) ;
#38367 = EDGE_CURVE ( 'NONE', #60619, #98073, #86282, .T. ) ;
#38368 = CARTESIAN_POINT ( 'NONE',  ( 2.126188665331921079, 1.138154612934966670, -1.609425365540081865 ) ) ;
#38369 = CARTESIAN_POINT ( 'NONE',  ( 4.377155534175989793, -1.710687068321177007, -0.8549628122409487219 ) ) ;
#38370 = ORIENTED_EDGE ( 'NONE', *, *, #152161, .F. ) ;
#38371 = CARTESIAN_POINT ( 'NONE',  ( -11.48784849554596121, 9.769504728180656628, -3.469614872287748231 ) ) ;
#38372 = CARTESIAN_POINT ( 'NONE',  ( 4.580490420436008847, 1.213483934061266201, -1.551205257841874241 ) ) ;
#38373 = CARTESIAN_POINT ( 'NONE',  ( -0.01194524340117873729, -0.4266214822964596309, -1.901745140312367521 ) ) ;
#38374 = EDGE_LOOP ( 'NONE', ( #62520, #191794, #113837, #98613 ) ) ;
#38375 = CARTESIAN_POINT ( 'NONE',  ( -4.990283058281743678, 7.979691447040783814, -1.199719254218453823 ) ) ;
#38377 = CARTESIAN_POINT ( 'NONE',  ( -0.3914079065635818755, 3.043201908700303715, 0.4248930002254263094 ) ) ;
#38376 = CARTESIAN_POINT ( 'NONE',  ( -4.390861645979385663, 6.216034235099629157, -1.599625672291271394 ) ) ;
#38379 = CARTESIAN_POINT ( 'NONE',  ( 6.509323147892504657, 6.766834225395614411, 0.000000000000000000 ) ) ;
#38378 = CARTESIAN_POINT ( 'NONE',  ( 7.958799866421889746, 9.244020251369077457, -1.199719254218441611 ) ) ;
#38381 = VERTEX_POINT ( 'NONE', #138735 ) ;
#38380 = CARTESIAN_POINT ( 'NONE',  ( 4.881465217424630687, 0.1836680969147831965, -1.903426456924644183 ) ) ;
#38382 = CARTESIAN_POINT ( 'NONE',  ( 0.4994150495197279827, 1.833458848295946186, -1.227822027206024957 ) ) ;
#38383 = CARTESIAN_POINT ( 'NONE',  ( -1.284279953904152949, 2.952889714876734573, 0.7750000000000152323 ) ) ;
#38384 = CARTESIAN_POINT ( 'NONE',  ( 6.604166866988625095, -0.8575501651001187220, 1.819208590218702071 ) ) ;
#38385 = CARTESIAN_POINT ( 'NONE',  ( 0.07661050522431847587, 7.629137130509112907, -2.310792076560589603 ) ) ;
#38386 = CARTESIAN_POINT ( 'NONE',  ( 5.349643074071059878, 2.189064600896481139, -0.1049423877047955811 ) ) ;
#38387 = CARTESIAN_POINT ( 'NONE',  ( 0.000000000000000000, -0.02876672507444788529, 3.432849766368870181 ) ) ;
#38388 = CARTESIAN_POINT ( 'NONE',  ( -6.531918710724228916, -6.583723166013396799, -7.057683771862738986 ) ) ;
#38389 = CARTESIAN_POINT ( 'NONE',  ( 3.332542965736586371, -1.235447621225284287, 1.661183390374972646 ) ) ;
#38390 = CARTESIAN_POINT ( 'NONE',  ( -4.889686956022917919, 8.856385215335397021, 1.214306433183764966E-14 ) ) ;
#38391 = CIRCLE ( 'NONE', #3879, 11.09999999999999964 ) ;
#38392 = CARTESIAN_POINT ( 'NONE',  ( -4.675522092136524144, 8.294237829558845476, 0.5223692772225538850 ) ) ;
#38394 = CARTESIAN_POINT ( 'NONE',  ( 1.129994055010040022, -1.371941552271437770, -1.670562328977095445 ) ) ;
#38393 = CARTESIAN_POINT ( 'NONE',  ( -3.903858165731105778, 6.641919395739846799, 1.199719254218464037 ) ) ;
#38395 = AXIS2_PLACEMENT_3D ( 'NONE', #70239, #19368, #133173 ) ;
#38396 = CARTESIAN_POINT ( 'NONE',  ( -11.56018411499319853, 8.213217331593577697, 3.229764516336100399 ) ) ;
#38397 = CARTESIAN_POINT ( 'NONE',  ( 5.736508392357904107, 5.865217010605237924, 0.000000000000000000 ) ) ;
#38398 = CARTESIAN_POINT ( 'NONE',  ( 0.03636482241361622264, -7.019129742887146861, 9.500587730661987251 ) ) ;
#38399 = CARTESIAN_POINT ( 'NONE',  ( 1.364683531250000303, 13.06770833367473728, -0.7879004041258355073 ) ) ;
#38401 = CARTESIAN_POINT ( 'NONE',  ( -5.281783360975562225, 8.319775133516907673, 1.199719254218452935 ) ) ;
#38400 = CARTESIAN_POINT ( 'NONE',  ( 6.925078400183546812, 2.074047572655359328, 2.163550030515603684 ) ) ;
#38402 = CARTESIAN_POINT ( 'NONE',  ( 2.641814858895009444, 2.006371511526034546, -0.2024640970367599380 ) ) ;
#38403 = CARTESIAN_POINT ( 'NONE',  ( 4.324694450628805420, 0.7358571774197277815, -1.570421820497726051 ) ) ;
#38404 = CARTESIAN_POINT ( 'NONE',  ( -2.754277761870538299, 6.365074488824250309, 1.040834085586084257E-14 ) ) ;
#38405 = CARTESIAN_POINT ( 'NONE',  ( 4.047765473330780850, 1.496028175931501947, 1.431257568052332729 ) ) ;
#38406 = CARTESIAN_POINT ( 'NONE',  ( 4.060252369235962888, -1.217431538915053180, 1.732033588162092297 ) ) ;
#38407 = CARTESIAN_POINT ( 'NONE',  ( 6.238723240582662477, 10.43026088065513513, -0.7998128361456291469 ) ) ;
#38408 = CARTESIAN_POINT ( 'NONE',  ( -1.364683531250012516, 4.988541667008084879, -0.7879004041258300672 ) ) ;
#38409 = CARTESIAN_POINT ( 'NONE',  ( 1.973436150528505406, -0.2460485697947655814, 1.953970194506114755 ) ) ;
#38410 = CARTESIAN_POINT ( 'NONE',  ( 0.7910927259777954523, -0.04954035392716604758, -1.911929172785244102 ) ) ;
#38411 = CARTESIAN_POINT ( 'NONE',  ( 5.279328977631358555, 1.536242920967767711, 1.701453964730540447 ) ) ;
#38413 = ADVANCED_FACE ( 'NONE', ( #204753 ), #20754, .T. ) ;
#38412 = CARTESIAN_POINT ( 'NONE',  ( 2.349991895876184511, 1.825291697999480434, 0.04531359951509549705 ) ) ;
#38414 = CARTESIAN_POINT ( 'NONE',  ( 4.016958651398847557, 7.908478536599129249, -0.7998128361456362523 ) ) ;
#38415 = CARTESIAN_POINT ( 'NONE',  ( 6.331294547457450683, 7.449227062530913379, -1.082531754730543083 ) ) ;
#38416 = CARTESIAN_POINT ( 'NONE',  ( -8.993135964566285168, 9.386413468282476913, -0.7998128361456291469 ) ) ;
#38417 = CARTESIAN_POINT ( 'NONE',  ( 2.355728993131640525, -1.494696414742059387, -1.348868867694212881 ) ) ;
#38418 =( BOUNDED_CURVE ( )  B_SPLINE_CURVE ( 2, ( #190798, #39231, #71704, #187604, #172443, #142103, #123778 ),
 .UNSPECIFIED., .F., .T. ) 
 B_SPLINE_CURVE_WITH_KNOTS ( ( 3, 2, 2, 3 ),
 ( 0.1428571428571429880, 0.1488095238095238637, 0.1547619047619047394, 0.1607142857142856152 ),
 .UNSPECIFIED. ) 
 CURVE ( )  GEOMETRIC_REPRESENTATION_ITEM ( )  RATIONAL_B_SPLINE_CURVE ( ( 0.9999999999999968914, 0.8660254037844418162, 1.000000000000000000, 0.8660254037844387076, 1.000000000000000000, 0.8660254037844412611, 0.9999999999999974465 ) ) 
 REPRESENTATION_ITEM ( '' )  );
#38419 = CARTESIAN_POINT ( 'NONE',  ( 3.590630163336411051, 1.912927474663427496, 0.4342120235502828773 ) ) ;
#38420 = CARTESIAN_POINT ( 'NONE',  ( -6.507023659554960204, 9.678945805201045971, 1.199719254218452047 ) ) ;
#38421 = CARTESIAN_POINT ( 'NONE',  ( -4.737684612971557740, 7.614716917520386374, 1.199719254218464037 ) ) ;
#38423 = EDGE_CURVE ( 'NONE', #61589, #74349, #206106, .T. ) ;
#38422 = CARTESIAN_POINT ( 'NONE',  ( 0.07556134207196538166, 0.2286499876833356648, -2.278112926217394030 ) ) ;
#38425 = CARTESIAN_POINT ( 'NONE',  ( 4.733122822409558950, -1.617543599503493468, 0.7186682867280795861 ) ) ;
#38424 = CARTESIAN_POINT ( 'NONE',  ( 6.017543284830850325, -1.160447301756668104, -1.738784508216392855 ) ) ;
#38426 = CARTESIAN_POINT ( 'NONE',  ( -2.334365499475838046, 5.399177108899520405, -0.7827922733892430651 ) ) ;
#38427 = CARTESIAN_POINT ( 'NONE',  ( 0.5334774086375413393, -1.552487152004313087, -1.546944964277228607 ) ) ;
#38428 = CARTESIAN_POINT ( 'NONE',  ( 6.386628771994263154, 1.510377909004370522, -0.8644441249686038997 ) ) ;
#38429 = CARTESIAN_POINT ( 'NONE',  ( 7.344766530301147789, 9.591980256816594164, 1.599625672291281386 ) ) ;
#38430 = DIRECTION ( 'NONE',  ( 0.000000000000000000, 0.000000000000000000, -1.000000000000000000 ) ) ;
#38431 = CARTESIAN_POINT ( 'NONE',  ( 0.2635768167446932986, -2.297931531924101822, -0.05306211189425556751 ) ) ;
#38432 =( BOUNDED_CURVE ( )  B_SPLINE_CURVE ( 2, ( #59468, #155918, #160174, #125627, #11774, #74661, #208899 ),
 .UNSPECIFIED., .F., .T. ) 
 B_SPLINE_CURVE_WITH_KNOTS ( ( 3, 2, 2, 3 ),
 ( 0.03571428571428574700, 0.04166666666666662272, 0.04761904761904750538, 0.05357142857142838110 ),
 .UNSPECIFIED. ) 
 CURVE ( )  GEOMETRIC_REPRESENTATION_ITEM ( )  RATIONAL_B_SPLINE_CURVE ( ( 0.9999999999999992228, 0.8660254037844394848, 1.000000000000000000, 0.8660254037844387076, 1.000000000000000000, 0.8660254037844429265, 0.9999999999999957812 ) ) 
 REPRESENTATION_ITEM ( '' )  );
#38433 = DIRECTION ( 'NONE',  ( 5.551115123125764829E-17, 0.000000000000000000, -1.000000000000000000 ) ) ;
#38434 = CARTESIAN_POINT ( 'NONE',  ( 1.647397727484143592, -1.863059487452220386, 1.182652941231487453 ) ) ;
#38435 = CARTESIAN_POINT ( 'NONE',  ( 0.7433368588017514877, -0.2641965325859591540, -2.154838077344235714 ) ) ;
#38436 = FACE_OUTER_BOUND ( 'NONE', #3197, .T. ) ;
#38437 = CARTESIAN_POINT ( 'NONE',  ( 1.007203092032255665, -0.04580389244966718426, 2.116997601370627091 ) ) ;
#38438 = CARTESIAN_POINT ( 'NONE',  ( 3.187500000000002665, -1.451031289060985330, 1.451031289061251117 ) ) ;
#38439 = CARTESIAN_POINT ( 'NONE',  ( 6.727182134110200273, 0.5640974741700152117, 2.241195997201197443 ) ) ;
#38440 = CARTESIAN_POINT ( 'NONE',  ( 4.243131921826915232, -1.676359970754065731, 0.9489593035170663660 ) ) ;
#38441 = VERTEX_POINT ( 'NONE', #43369 ) ;
#38443 = CARTESIAN_POINT ( 'NONE',  ( 0.7499999999999920064, 5.733333333333353821, 1.299038105676669330 ) ) ;
#38442 = CARTESIAN_POINT ( 'NONE',  ( 1.699181366971340701, 1.908771516627869147, 1.269207382326368316 ) ) ;
#38444 = CARTESIAN_POINT ( 'NONE',  ( 4.364835388595708743, 7.179726155748598515, 1.199719254218462483 ) ) ;
#38445 = CARTESIAN_POINT ( 'NONE',  ( 6.979750152936881058, 7.037463354714830643, 0.7998128361456341429 ) ) ;
#38446 = CARTESIAN_POINT ( 'NONE',  ( 4.143395664610330265, 0.1093779850947790705, 2.218736840405158173 ) ) ;
#38447 = CARTESIAN_POINT ( 'NONE',  ( -8.514157279702027736, 10.95626946445095307, -1.443375672974059665 ) ) ;
#38448 = LINE ( 'NONE', #88270, #156679 ) ;
#38449 = CARTESIAN_POINT ( 'NONE',  ( 5.639828713604826405, 9.523624565940227882, -0.7216878364870267237 ) ) ;
#38450 = CARTESIAN_POINT ( 'NONE',  ( -8.798878505144665851, 9.367705798864669475, -0.7216878364870267237 ) ) ;
#38452 = EDGE_CURVE ( 'NONE', #31691, #124513, #207343, .T. ) ;
#38451 = CIRCLE ( 'NONE', #180396, 0.07999999999999998779 ) ;
#38453 = CARTESIAN_POINT ( 'NONE',  ( 5.234856708652222856, 8.161064355852680308, 1.082531754730549078 ) ) ;
#38454 = EDGE_LOOP ( 'NONE', ( #141487, #80237, #109650, #50695 ) ) ;
#38455 = CARTESIAN_POINT ( 'NONE',  ( 1.354138928560550292, 0.1455316553338575902, -2.011204400906742240 ) ) ;
#38457 = CARTESIAN_POINT ( 'NONE',  ( 6.760222218534770455, -2.062298699534569124, 0.04672293413533928907 ) ) ;
#38456 = CARTESIAN_POINT ( 'NONE',  ( 7.426115451983150706, 9.686887332112256388, -1.599625672291262513 ) ) ;
#38458 = CARTESIAN_POINT ( 'NONE',  ( -11.00039779440762899, -6.304807775344881904, 0.01400375819670464893 ) ) ;
#38459 = CARTESIAN_POINT ( 'NONE',  ( 6.387299765369506055, 7.584842826753462219, -1.082531754730548412 ) ) ;
#38460 = CARTESIAN_POINT ( 'NONE',  ( -0.04178991631376138827, -1.644041690304678616, -0.8291446804715857377 ) ) ;
#38461 = CARTESIAN_POINT ( 'NONE',  ( -3.894033820048823813, 8.999999999999998224, 0.7749999999999996891 ) ) ;
#38462 = CARTESIAN_POINT ( 'NONE',  ( -1.364683531250012516, 2.280208333674751842, 0.7879004041258379498 ) ) ;
#38464 = CARTESIAN_POINT ( 'NONE',  ( 1.827073579719180163, -1.668441312418825095, 0.5905873696427661468 ) ) ;
#38463 = B_SPLINE_CURVE_WITH_KNOTS ( 'NONE', 3,
 ( #132217, #80231, #115989, #95453, #30431, #161503, #195049, #13083 ),
 .UNSPECIFIED., .F., .F.,
 ( 4, 2, 2, 4 ),
 ( 0.000000000000000000, 0.003117338238615241595, 0.004676007357922863476, 0.006234676477230485792 ),
 .UNSPECIFIED. ) ;
#38465 = CARTESIAN_POINT ( 'NONE',  ( 0.5103889644224939293, -1.913802852362625151, 0.6352017490645140985 ) ) ;
#38466 = CARTESIAN_POINT ( 'NONE',  ( 0.4328342922346357646, -1.301571265828086688, -1.302605208699902928 ) ) ;
#38467 = CARTESIAN_POINT ( 'NONE',  ( 4.564210359040954401, -1.498010274845029244, 1.735314277699088858 ) ) ;
#38468 = CARTESIAN_POINT ( 'NONE',  ( 3.679498877186979211, -0.9061679144062879665, 1.602619060095414216 ) ) ;
#38469 = CARTESIAN_POINT ( 'NONE',  ( 8.127223016387999266, 11.56917838817298616, 1.199719254218460707 ) ) ;
#38470 = CARTESIAN_POINT ( 'NONE',  ( 9.367496997597600128, 3.999999999999994671, 7.500000000000004441 ) ) ;
#38471 = CARTESIAN_POINT ( 'NONE',  ( 3.750846114953470867, -1.492790808496821775, 1.050590184284278861 ) ) ;
#38472 = CARTESIAN_POINT ( 'NONE',  ( 4.553361389630797618, -1.314998166741452090, 1.528740011303417745 ) ) ;
#38473 = CARTESIAN_POINT ( 'NONE',  ( -7.831806290188425557, 12.28885777186185990, -0.7998128361456281477 ) ) ;
#38475 = CARTESIAN_POINT ( 'NONE',  ( -7.781453819600577582, 8.043060642480948985, 0.000000000000000000 ) ) ;
#38474 = CARTESIAN_POINT ( 'NONE',  ( 3.116390431409152395, -1.113901014592171723, -1.969235179105185640 ) ) ;
#38476 = CARTESIAN_POINT ( 'NONE',  ( 6.229533133763371922, -1.984190613765562494, 0.7061325270490863559 ) ) ;
#38477 =( LENGTH_UNIT ( ) NAMED_UNIT ( * ) SI_UNIT ( .MILLI., .METRE. ) );
#38478 = CARTESIAN_POINT ( 'NONE',  ( 3.930184216435282707, 1.147649575447948100, 1.722966636330313550 ) ) ;
#38479 = CARTESIAN_POINT ( 'NONE',  ( 3.192055101013606233, 5.811482486902795230, -1.199719254218446718 ) ) ;
#38480 = CARTESIAN_POINT ( 'NONE',  ( 1.360316468749963592, 1.317708333674712184, -0.7853790794158981292 ) ) ;
#38481 = CARTESIAN_POINT ( 'NONE',  ( 5.936213163351175659, -1.177816969253571155, -1.763093882214488817 ) ) ;
#38482 = ITEM_DEFINED_TRANSFORMATION ( 'NONE', 'NONE', #197335,  #200407 ) ;
#38484 = CARTESIAN_POINT ( 'NONE',  ( 1.963383859451812041, 0.3296633872902128282, -1.897934821152784446 ) ) ;
#38483 = CARTESIAN_POINT ( 'NONE',  ( -9.398826802771548472, 11.98838390803207865, -1.599625672291263179 ) ) ;
#38485 = CARTESIAN_POINT ( 'NONE',  ( -2.830620210203090181, 6.524417021870718258, 0.000000000000000000 ) ) ;
#38486 = CARTESIAN_POINT ( 'NONE',  ( 6.596547011414190642, 1.947522214285227760, 0.2922974700911728507 ) ) ;
#38487 = CARTESIAN_POINT ( 'NONE',  ( 5.858531774436539052, 6.007577623030311287, 0.000000000000000000 ) ) ;
#38488 = CARTESIAN_POINT ( 'NONE',  ( 5.890592889100787488, 5.978139607520936316, 0.07745371066007235294 ) ) ;
#38489 = CARTESIAN_POINT ( 'NONE',  ( -3.391510981712833939, 7.108513245306943062, 0.7998128361456341429 ) ) ;
#38490 = CARTESIAN_POINT ( 'NONE',  ( 1.090412635922506368, 1.328748260410139492, 1.780047631856091606 ) ) ;
#38491 = CARTESIAN_POINT ( 'NONE',  ( 2.907361098931018795, 1.778370309693329210, 1.127733957892971484 ) ) ;
#38492 = CARTESIAN_POINT ( 'NONE',  ( -4.625266680917477835, 5.425174544939014964, -1.199719254218453823 ) ) ;
#38493 = CARTESIAN_POINT ( 'NONE',  ( 7.721532178182734185, 8.967207948423393304, 1.199719254218462483 ) ) ;
#38494 = CARTESIAN_POINT ( 'NONE',  ( 1.099803389655891195, 0.7588869020343449456, -1.699499299819209108 ) ) ;
#38495 = CARTESIAN_POINT ( 'NONE',  ( 6.908042961362778733, 8.018137195466769285, 1.199719254218462483 ) ) ;
#38496 = CARTESIAN_POINT ( 'NONE',  ( 3.472859903394816872, 7.203420320602605287, -0.7998128361456291469 ) ) ;
#38497 = CARTESIAN_POINT ( 'NONE',  ( -7.458393901293492334, 7.874083437696761223, 0.7216878364870317197 ) ) ;
#38498 = CARTESIAN_POINT ( 'NONE',  ( -8.188761592974046266, 10.57664116326830595, -1.443375672974059665 ) ) ;
#38499 =( BOUNDED_CURVE ( )  B_SPLINE_CURVE ( 3, ( #88407, #71049, #202108, #86262 ),
 .UNSPECIFIED., .F., .T. ) 
 B_SPLINE_CURVE_WITH_KNOTS ( ( 4, 4 ),
 ( 0.000000000000000000, 0.5000000000000022204 ),
 .UNSPECIFIED. ) 
 CURVE ( )  GEOMETRIC_REPRESENTATION_ITEM ( )  RATIONAL_B_SPLINE_CURVE ( ( 1.000000000000000222, 0.3333333333333304838, 0.3333333333333334259, 1.000000000000003109 ) ) 
 REPRESENTATION_ITEM ( '' )  );
#38500 = CARTESIAN_POINT ( 'NONE',  ( 1.494549364340029163, -1.129948290531690658, 1.794289463044356436 ) ) ;
#38501 = CARTESIAN_POINT ( 'NONE',  ( -7.449279056065764237, 7.655523418356991350, 0.7998128361456341429 ) ) ;
#38503 = CARTESIAN_POINT ( 'NONE',  ( 3.086327779807009009, 1.092107249913790712, -1.629585102321646328 ) ) ;
#38502 = CARTESIAN_POINT ( 'NONE',  ( 1.224999999999967004, 0.1041666666667366015, 0.7072540797572677285 ) ) ;
#38504 = CARTESIAN_POINT ( 'NONE',  ( 1.850665834824256173, 0.6780317805383448970, 2.052694239800388676 ) ) ;
#38505 = CARTESIAN_POINT ( 'NONE',  ( 1.469984750362408610, -1.748608032326857353, -0.5769476384821782267 ) ) ;
#38507 = CARTESIAN_POINT ( 'NONE',  ( -4.684235067853224521, 6.877467941869524815, -1.224209591347114046 ) ) ;
#38506 = CARTESIAN_POINT ( 'NONE',  ( -5.147255595043616516, 6.034161611419515125, 1.199719254218452935 ) ) ;
#38508 = CARTESIAN_POINT ( 'NONE',  ( 3.907932343763017347, 1.228949333998660798, -1.232512660115521408 ) ) ;
#38509 = CARTESIAN_POINT ( 'NONE',  ( 6.155038550924150087, 7.243595066575396757, 1.082531754730558626 ) ) ;
#38510 = CARTESIAN_POINT ( 'NONE',  ( -10.48267169704037727, 5.268073273308885973, 5.153989745587932880 ) ) ;
#38511 = CIRCLE ( 'NONE', #149198, 10.97656854249491687 ) ;
#38512 = CARTESIAN_POINT ( 'NONE',  ( 0.6026772488060898603, -0.7295331166810551382, -2.035022307366324945 ) ) ;
#38513 = CARTESIAN_POINT ( 'NONE',  ( 3.145861080134567000, -0.1455099638626895786, -2.010896398064919488 ) ) ;
#38514 = CARTESIAN_POINT ( 'NONE',  ( 1.500000000000001332, 12.90625000068279604, 0.000000000000000000 ) ) ;
#38515 = CARTESIAN_POINT ( 'NONE',  ( 0.4620835240300471547, 2.137967531602209981, -0.3185850937674692407 ) ) ;
#38516 = CARTESIAN_POINT ( 'NONE',  ( 2.412907133309648788, 1.760172955399338823, 0.8881188249313717309 ) ) ;
#38517 = CARTESIAN_POINT ( 'NONE',  ( 6.609000000000047947, 2.032467779867861868, 2.404707446487294842 ) ) ;
#38518 = CARTESIAN_POINT ( 'NONE',  ( 2.823698466604074309, 1.076742338344888639, -1.616048498441272407 ) ) ;
#38521 = ORIENTED_EDGE ( 'NONE', *, *, #189935, .T. ) ;
#38520 = CARTESIAN_POINT ( 'NONE',  ( -4.340018570150309785, 7.117086527600392287, -1.082531754730551743 ) ) ;
#38519 = CARTESIAN_POINT ( 'NONE',  ( 6.363533315466952445, -1.540175188624912650, -1.133462061071670579 ) ) ;
#38522 = CARTESIAN_POINT ( 'NONE',  ( -4.841670253411603397, 5.781608396135871075, 1.082531754730549078 ) ) ;
#38523 = CARTESIAN_POINT ( 'NONE',  ( -0.1106856583841086261, 2.025759259886884323, -2.413105898545636840 ) ) ;
#38524 = CARTESIAN_POINT ( 'NONE',  ( 4.875038752565570732, 7.845239757038595663, -1.199719254218452047 ) ) ;
#38525 = CARTESIAN_POINT ( 'NONE',  ( -5.712781623311813384, 7.758274208654143855, -1.599625672291271394 ) ) ;
#38526 = CARTESIAN_POINT ( 'NONE',  ( -7.605197822622922210, 7.837428646007010613, -0.7998128361456362523 ) ) ;
#38527 = CARTESIAN_POINT ( 'NONE',  ( -6.448443555175264130, 6.863647322328955802, -0.7618168508180013232 ) ) ;
#38528 = CARTESIAN_POINT ( 'NONE',  ( 0.4466624375424713689, 2.201045718399210038, 0.1599725512250807224 ) ) ;
#38529 = CARTESIAN_POINT ( 'NONE',  ( 0.000000000000000000, 8.999999999999998224, 0.000000000000000000 ) ) ;
#38530 = CARTESIAN_POINT ( 'NONE',  ( 4.170719094083116474, 1.390339895272204362, -1.384257141873693087 ) ) ;
#38531 = CARTESIAN_POINT ( 'NONE',  ( 7.771848369131631351, 10.09024240211882351, -1.599625672291262513 ) ) ;
#38532 = CARTESIAN_POINT ( 'NONE',  ( 1.617814789376757156, 0.2004366740697149929, 2.006445999502483257 ) ) ;
#38533 = ORIENTED_EDGE ( 'NONE', *, *, #194571, .T. ) ;
#38534 = CARTESIAN_POINT ( 'NONE',  ( 2.307945874296753797, -1.223308491024234224, -1.728006348806595316 ) ) ;
#38535 = CARTESIAN_POINT ( 'NONE',  ( -1.500000000000013101, 1.410416667349486008, -0.8660254037844313801 ) ) ;
#38537 = CARTESIAN_POINT ( 'NONE',  ( -6.555530967407501741, 7.606873202518897870, 1.199719254218450271 ) ) ;
#38536 = CARTESIAN_POINT ( 'NONE',  ( -4.457933580795036654, 4.095344020549286590, -0.7998128361456221525 ) ) ;
#38538 = CARTESIAN_POINT ( 'NONE',  ( 2.976309490518674217, -0.1360139883382974202, -1.836174483004118674 ) ) ;
#38539 = ORIENTED_EDGE ( 'NONE', *, *, #185325, .T. ) ;
#38540 = CARTESIAN_POINT ( 'NONE',  ( -10.29471871147821282, 10.90492667301307605, -0.7998128361456291469 ) ) ;
#38541 = CARTESIAN_POINT ( 'NONE',  ( 5.361566827843168070, 4.701484413405860430, 2.440314516401218548 ) ) ;
#38542 = CARTESIAN_POINT ( 'NONE',  ( 3.744478000529617656, 1.131475959888720295, -1.793321066073015224 ) ) ;
#38543 = CARTESIAN_POINT ( 'NONE',  ( 0.3570341529223716726, 1.821527202347131169, -0.2672101559373847857 ) ) ;
#38544 = CARTESIAN_POINT ( 'NONE',  ( -1.499999999999997780, 5.681250000682820378, 1.214306433183764966E-14 ) ) ;
#38545 = CARTESIAN_POINT ( 'NONE',  ( 7.396136491454752715, 8.587579647240744407, 1.199719254218462483 ) ) ;
#38546 = CARTESIAN_POINT ( 'NONE',  ( 4.341127749375134570, -1.794969056106166860, 1.012190969697931209 ) ) ;
#38548 = CARTESIAN_POINT ( 'NONE',  ( 1.575478407343299692, -0.9843019613302635973, 1.555867251595323353 ) ) ;
#38547 = CARTESIAN_POINT ( 'NONE',  ( -7.576308911938196999, 7.733448573549685179, 0.7998128361456462443 ) ) ;
#38549 = CARTESIAN_POINT ( 'NONE',  ( 0.6823417656249899377, 5.426041667008087543, -1.181850606188754593 ) ) ;
#38550 = CARTESIAN_POINT ( 'NONE',  ( 1.284279953904121641, 3.253360285806104812, 0.7750000000000135669 ) ) ;
#38551 = CARTESIAN_POINT ( 'NONE',  ( -1.519536625744598579, 8.761901799250109590, 2.483436355453746192 ) ) ;
#38552 = CARTESIAN_POINT ( 'NONE',  ( 10.99943592145024951, -8.241816521215563185, -0.1113975309864851937 ) ) ;
#38553 = AXIS2_PLACEMENT_3D ( 'NONE', #43203, #142844, #174271 ) ;
#38554 = CARTESIAN_POINT ( 'NONE',  ( 2.385638622766753425, 2.017150886971270651, -0.8956362484653990208 ) ) ;
#38555 = CARTESIAN_POINT ( 'NONE',  ( 3.849113346294403382, -1.852342442990447813, 1.298737409825992062 ) ) ;
#38556 = CIRCLE ( 'NONE', #159620, 0.09999999999999976963 ) ;
#38557 = CARTESIAN_POINT ( 'NONE',  ( -7.592202833972775622, 8.920286730132099606, 1.082531754730558626 ) ) ;
#38558 = CARTESIAN_POINT ( 'NONE',  ( 4.078215212670958323, 0.8593412415473808963, 1.594818892651229891 ) ) ;
#38559 = CARTESIAN_POINT ( 'NONE',  ( 3.977677156295666538, -0.7278633372749753194, 1.772268029184346227 ) ) ;
#38560 = CARTESIAN_POINT ( 'NONE',  ( 5.230950013807261101, -1.948248037745937022, -0.7008574099531189594 ) ) ;
#38561 = CARTESIAN_POINT ( 'NONE',  ( -1.201851678989727383E-14, 4.759375000341419693, -1.575800808251660134 ) ) ;
#38562 = EDGE_CURVE ( 'NONE', #132409, #17367, #42943, .T. ) ;
#38563 = CARTESIAN_POINT ( 'NONE',  ( 4.153168997088651615, -1.638446398916657776, -1.096151307749502868 ) ) ;
#38564 = CARTESIAN_POINT ( 'NONE',  ( 1.483290174073574441, 1.780938433730950621, -0.7347945396837353149 ) ) ;
#38565 = CARTESIAN_POINT ( 'NONE',  ( 3.660894226558962128, -1.649352935060313552, -0.8826137995501317501 ) ) ;
#38566 = CARTESIAN_POINT ( 'NONE',  ( 3.106426088690077858, -2.305020500623474522, 0.1135576804369240328 ) ) ;
#38567 = CARTESIAN_POINT ( 'NONE',  ( 3.982723974049819482, 1.766592268715084790, 0.5855280163863920695 ) ) ;
#38568 = CARTESIAN_POINT ( 'NONE',  ( 1.364683531249990311, 4.634375000341417916, 1.214306433183764966E-14 ) ) ;
#38569 = CARTESIAN_POINT ( 'NONE',  ( 6.396834479292349052, -8.176568542494905500, 7.055228938194280985 ) ) ;
#38570 = CARTESIAN_POINT ( 'NONE',  ( 1.506614580823143701, -0.7594792294695625889, -1.964545455775383642 ) ) ;
#38571 = B_SPLINE_CURVE_WITH_KNOTS ( 'NONE', 3,
 ( #169452, #53571, #168390, #40540, #202997, #19986, #104468, #23177 ),
 .UNSPECIFIED., .F., .F.,
 ( 4, 2, 2, 4 ),
 ( 0.000000000000000000, 0.0004970278158210180916, 0.0007455417237315293058, 0.0009940556316420405200 ),
 .UNSPECIFIED. ) ;
#38572 = CARTESIAN_POINT ( 'NONE',  ( 2.860407222358963608, 5.320596945185329218, 1.082531754730548412 ) ) ;
#38574 = DIRECTION ( 'NONE',  ( 0.000000000000000000, 0.000000000000000000, -1.000000000000000000 ) ) ;
#38573 = CARTESIAN_POINT ( 'NONE',  ( 0.6823417656249917140, 5.405208333674749177, 1.181850606188765695 ) ) ;
#38575 = CARTESIAN_POINT ( 'NONE',  ( 2.707414796094851361, 1.816601298730673220, -1.093838055662835096 ) ) ;
#38576 = CARTESIAN_POINT ( 'NONE',  ( 6.392116398764381202, 6.567141947923786027, -2.438447736780795072 ) ) ;
#38577 = CARTESIAN_POINT ( 'NONE',  ( 0.2112021888033519534, 1.676852382702203714, -1.125601893279993160 ) ) ;
#38578 = CARTESIAN_POINT ( 'NONE',  ( 1.364683531249988757, 0.8843750003414210248, 0.000000000000000000 ) ) ;
#38579 = CARTESIAN_POINT ( 'NONE',  ( -2.657034918598338180, 6.043698471765932112, -0.7216878364870267237 ) ) ;
#38580 = CARTESIAN_POINT ( 'NONE',  ( 5.769158057814842699, 6.689438141327490150, 1.199719254218462483 ) ) ;
#38581 = CARTESIAN_POINT ( 'NONE',  ( 2.477987356985793088, 1.327747062846416526, 1.705691702009938915 ) ) ;
#38582 = CARTESIAN_POINT ( 'NONE',  ( 1.387358672533454351, 7.315968950353815892, -4.254625267138348654 ) ) ;
#38585 = CARTESIAN_POINT ( 'NONE',  ( 4.053524740805938720, 3.831459740469437936, 1.214306433183764966E-14 ) ) ;
#38584 = CARTESIAN_POINT ( 'NONE',  ( 6.825078400183544503, 2.075476428726834577, 2.163873318353096931 ) ) ;
#38583 = CARTESIAN_POINT ( 'NONE',  ( 5.306037014901791693, 7.283738832175834510, 1.599625672291269396 ) ) ;
#38586 = CARTESIAN_POINT ( 'NONE',  ( -1.326716514427061987E-15, 2.999999999999988454, -1.225000000000003864 ) ) ;
#38587 = CARTESIAN_POINT ( 'NONE',  ( 6.333220217719927270, -1.622483202430196725, -1.197309987464048486 ) ) ;
#38588 = CARTESIAN_POINT ( 'NONE',  ( -7.782016984564068096, 10.10210578678999482, 1.443375672974090751 ) ) ;
#38589 = CARTESIAN_POINT ( 'NONE',  ( 6.339408610606328764, 0.7995911543839243629, -1.932009116241965252 ) ) ;
#38590 = CARTESIAN_POINT ( 'NONE',  ( -0.4000000000000236144, -3.469446951953614189E-14, -3.989863994746656317E-14 ) ) ;
#38592 = CARTESIAN_POINT ( 'NONE',  ( 1.364683531249997417, 12.23437500034139980, 2.602085213965210642E-15 ) ) ;
#38591 = CARTESIAN_POINT ( 'NONE',  ( 0.7258825447220511595, -2.147484179761431022, 0.7124928158122600941 ) ) ;
#38593 = CARTESIAN_POINT ( 'NONE',  ( -9.969323024750229578, 10.52529837183042716, -0.7998128361456291469 ) ) ;
#38594 = CARTESIAN_POINT ( 'NONE',  ( -5.707619481228832115, 6.721606151930833661, -1.082531754730543971 ) ) ;
#38595 = CARTESIAN_POINT ( 'NONE',  ( -1.364683531250012516, 1.842708333674749843, 0.7879004041258379498 ) ) ;
#38596 = CARTESIAN_POINT ( 'NONE',  ( 3.982994815507484354, 7.308283119008860851, -0.9368446653362592080 ) ) ;
#38597 = CARTESIAN_POINT ( 'NONE',  ( -0.7500000000000179856, 10.04166666666667140, 1.299038105676658228 ) ) ;
#38598 = CARTESIAN_POINT ( 'NONE',  ( 2.543205433794017978, -1.277680944696883092, -1.158960206811429750 ) ) ;
#38599 = CARTESIAN_POINT ( 'NONE',  ( 4.878955176071345434, 6.785476686873604280, -1.599625672291269396 ) ) ;
#38600 = CARTESIAN_POINT ( 'NONE',  ( 2.495042215028328236, 1.364832443287033570, 1.126547774882515673 ) ) ;
#38601 = CARTESIAN_POINT ( 'NONE',  ( 2.578773234406753101, -1.386572882437474341, 1.459666011457598556 ) ) ;
#38602 = CARTESIAN_POINT ( 'NONE',  ( 5.368293279414073638, 1.083412401764087374, 1.922438065789177308 ) ) ;
#38603 = ORIENTED_EDGE ( 'NONE', *, *, #156207, .T. ) ;
#38604 = CARTESIAN_POINT ( 'NONE',  ( 4.412371012857700947, -2.019438640443659505, -0.04532404540058888875 ) ) ;
#38605 = CARTESIAN_POINT ( 'NONE',  ( -5.803772275101700906, 8.928762199997411386, -1.199719254218452047 ) ) ;
#38607 = CARTESIAN_POINT ( 'NONE',  ( 4.007435537932837910, -1.928747227692016564, 0.5880391185724976877 ) ) ;
#38606 = CARTESIAN_POINT ( 'NONE',  ( 4.406960118137589255, -0.4655763551070742912, -2.068578822641816473 ) ) ;
#38609 = ORIENTED_EDGE ( 'NONE', *, *, #70817, .F. ) ;
#38608 = CARTESIAN_POINT ( 'NONE',  ( 4.060681591697304249, 0.4892206165460743494, 1.744179128828279302 ) ) ;
#38610 = CARTESIAN_POINT ( 'NONE',  ( 4.213551878797002992, 8.137837301896977849, 0.000000000000000000 ) ) ;
#38611 = ORIENTED_EDGE ( 'NONE', *, *, #109273, .F. ) ;
#38612 = CARTESIAN_POINT ( 'NONE',  ( 1.604156678829884886, -0.6703249191640224813, -1.746612230856612769 ) ) ;
#38613 = CIRCLE ( 'NONE', #21257, 3.017800438942085606 ) ;
#38614 = CARTESIAN_POINT ( 'NONE',  ( 6.709597972018079837, -0.3944863986210072060, 1.789098616620278470 ) ) ;
#38615 = CARTESIAN_POINT ( 'NONE',  ( 5.742768220754598474, 1.747532268389985433, 0.4768009125176131957 ) ) ;
#38616 = CARTESIAN_POINT ( 'NONE',  ( -1.445103857048130047, 8.688264192037886247, 2.625611233228264840 ) ) ;
#38617 = CARTESIAN_POINT ( 'NONE',  ( -11.19531657929523583, 4.806608400964729633, -5.951317567608690240 ) ) ;
#38618 = CARTESIAN_POINT ( 'NONE',  ( -1.499999999999997780, 4.650000000000022560, 1.214306433183764966E-14 ) ) ;
#38619 = CARTESIAN_POINT ( 'NONE',  ( -1.364683531249997417, 3.571875000341423245, 1.214306433183764966E-14 ) ) ;
#38620 = CARTESIAN_POINT ( 'NONE',  ( 0.6153073421325053749, 1.564839666810373231, 1.099065937236625157 ) ) ;
#38621 = EDGE_LOOP ( 'NONE', ( #204291, #58740, #185288, #207827 ) ) ;
#38622 = CARTESIAN_POINT ( 'NONE',  ( 7.214347136247488912, 7.589362211809770997, -0.7216878364870317197 ) ) ;
#38623 = CARTESIAN_POINT ( 'NONE',  ( 1.275752070009423367, -1.914805681740685106, 0.4264308320794732432 ) ) ;
#38624 = CARTESIAN_POINT ( 'NONE',  ( -4.394251184604987870, 5.259619482528146150, 1.082531754730549078 ) ) ;
#38625 = CARTESIAN_POINT ( 'NONE',  ( -5.152980901645737077, 8.169505597632108262, -1.199719254218453823 ) ) ;
#38626 = CARTESIAN_POINT ( 'NONE',  ( 4.517907016363444939, -0.5628432189327194912, 2.044499502628312371 ) ) ;
#38628 = CARTESIAN_POINT ( 'NONE',  ( -10.50660484223216606, 5.359830900411396648, 5.105327592218940502 ) ) ;
#38627 = CARTESIAN_POINT ( 'NONE',  ( -0.02988540731096045455, 2.895077309840556445, -2.215427197800499570 ) ) ;
#38629 = CARTESIAN_POINT ( 'NONE',  ( 5.993430986175369846, 1.491191765471042041, 1.289477300995988118 ) ) ;
#38630 = CARTESIAN_POINT ( 'NONE',  ( -1.364683531250014514, 0.7385416670080887647, -0.7879004041258289570 ) ) ;
#38631 = CARTESIAN_POINT ( 'NONE',  ( 0.6506401683969212923, 1.984111478139438667, 0.3401018483101604928 ) ) ;
#38632 = ORIENTED_EDGE ( 'NONE', *, *, #127735, .T. ) ;
#38633 = CARTESIAN_POINT ( 'NONE',  ( 6.421125127611838401, -1.890376142121247494, 0.9539971363903186896 ) ) ;
#38634 = CARTESIAN_POINT ( 'NONE',  ( 11.39089125540332148, 7.472230595314081292, 3.799964780113331830 ) ) ;
#38635 = CARTESIAN_POINT ( 'NONE',  ( 1.996617168637443429, 2.047528291220417351, 0.3059219562495316125 ) ) ;
#38636 = CARTESIAN_POINT ( 'NONE',  ( 3.854260808034858155, 7.718664386007802136, -0.7998128361456362523 ) ) ;
#38637 = CARTESIAN_POINT ( 'NONE',  ( 5.845500506147374153, 6.848780674373954547, 1.199719254218453823 ) ) ;
#38638 = ORIENTED_EDGE ( 'NONE', *, *, #206116, .F. ) ;
#38640 = CARTESIAN_POINT ( 'NONE',  ( 4.493637847925535667, 7.329995691633395261, -1.199719254218452047 ) ) ;
#38639 = CARTESIAN_POINT ( 'NONE',  ( 4.892568727727841349, 1.738426232616798295, -1.160983500135639890 ) ) ;
#38643 = ORIENTED_EDGE ( 'NONE', *, *, #161384, .T. ) ;
#38642 = CARTESIAN_POINT ( 'NONE',  ( 1.980848084912645524, -1.656539610615878955, -0.7334085510423118404 ) ) ;
#38641 = CARTESIAN_POINT ( 'NONE',  ( 3.522295995157864290, 1.158834602800838498, -1.410599190884161969 ) ) ;
#38644 = CARTESIAN_POINT ( 'NONE',  ( 6.217417563691929772, -0.2743312036321900460, 2.189694890431858276 ) ) ;
#38645 = CARTESIAN_POINT ( 'NONE',  ( -0.08000000000000194456, -9.900000000000005684, -10.91970695577494865 ) ) ;
#38646 = MECHANICAL_DESIGN_GEOMETRIC_PRESENTATION_REPRESENTATION (  '', ( #4134 ), #10952 ) ;
#38647 = CARTESIAN_POINT ( 'NONE',  ( 4.577303723630254062, 0.003709267837189236805, -2.206952907291927168 ) ) ;
#38648 = CARTESIAN_POINT ( 'NONE',  ( 6.109920781252839994, 10.27999134477033216, 1.040834085586084257E-14 ) ) ;
#38649 = CARTESIAN_POINT ( 'NONE',  ( -0.6823417656250003738, 9.213541667008065872, 1.181850606188754593 ) ) ;
#38650 = CARTESIAN_POINT ( 'NONE',  ( 2.455592584850064153, -1.418247937500687561, -1.282927761235647335 ) ) ;
#38651 = CARTESIAN_POINT ( 'NONE',  ( 7.747594715205354809, 11.12627870345989756, -1.199719254218446718 ) ) ;
#38652 = CARTESIAN_POINT ( 'NONE',  ( 6.004363041306050697, 2.067815565686380364, 0.1054426792976848049 ) ) ;
#38653 = CARTESIAN_POINT ( 'NONE',  ( -1.500000000000001110, 10.30208333401612997, 0.8660254037844418162 ) ) ;
#38654 = CARTESIAN_POINT ( 'NONE',  ( 6.251546423958431298, 2.185849743821382862, -0.1592787069685035195 ) ) ;
#38655 = CARTESIAN_POINT ( 'NONE',  ( 5.120401779693986910, 7.917229619699595489, -1.217862772375446712 ) ) ;
#38656 = CARTESIAN_POINT ( 'NONE',  ( -9.481437597266051398, -6.708819892820502950, 0.4299312922663448555 ) ) ;
#38657 = ORIENTED_EDGE ( 'NONE', *, *, #43201, .T. ) ;
#38658 = EDGE_LOOP ( 'NONE', ( #52487, #153062, #209789, #9955, #196764, #38533 ) ) ;
#38659 = STYLED_ITEM ( 'NONE', ( #205943 ), #167773 ) ;
#38660 = CARTESIAN_POINT ( 'NONE',  ( 0.3999999999999889200, 0.000000000000000000, -5.204170427930421283E-15 ) ) ;
#38661 = CARTESIAN_POINT ( 'NONE',  ( 3.233525009082056201, -1.253693836546897700, -1.388425355430204622 ) ) ;
#38662 = CARTESIAN_POINT ( 'NONE',  ( -1.642778471875000035, -1.305208332855377407, -2.845375778867859751 ) ) ;
#38663 = CARTESIAN_POINT ( 'NONE',  ( 6.211043768836151280, 6.418841616496627545, 0.7216878364870578100 ) ) ;
#38664 = CARTESIAN_POINT ( 'NONE',  ( -6.995644074971465010, 10.14503993989993091, 1.082531754730549967 ) ) ;
#38665 = CARTESIAN_POINT ( 'NONE',  ( 3.413620815590684199, 7.204584394822967752, 0.7998128361456281477 ) ) ;
#38666 = CARTESIAN_POINT ( 'NONE',  ( 6.754741982670550371, -0.5462536098296210119, -1.996853278248729824 ) ) ;
#38667 = CARTESIAN_POINT ( 'NONE',  ( 0.7730648107450198703, 1.777001872080404166, -0.9530316558409923644 ) ) ;
#38668 = CARTESIAN_POINT ( 'NONE',  ( -7.974166903131914452, 12.45494515362926435, -0.7998128361456281477 ) ) ;
#38669 = CARTESIAN_POINT ( 'NONE',  ( 4.435452530326143616, 5.203724702582467998, -1.199719254218452047 ) ) ;
#38670 = FILL_AREA_STYLE ('',( #84208 ) ) ;
#38671 = CARTESIAN_POINT ( 'NONE',  ( 1.342011898504836820, 2.189069585219292957, 0.1046993245200772138 ) ) ;
#38672 = CARTESIAN_POINT ( 'NONE',  ( 4.723181480036696023, -0.08661695748878039947, 1.823760500460340550 ) ) ;
#38673 = CARTESIAN_POINT ( 'NONE',  ( -3.113568832632681360, 6.784247404713427798, -0.7998128361456281477 ) ) ;
#38674 = CARTESIAN_POINT ( 'NONE',  ( 6.400857919427532572, 6.640291458853147866, -0.7216878364870458196 ) ) ;
#38675 = CARTESIAN_POINT ( 'NONE',  ( 10.73535870392234237, 11.41900666419791399, 0.000000000000000000 ) ) ;
#38676 = CARTESIAN_POINT ( 'NONE',  ( -5.306037014901836990, 7.283738832175834510, 1.599625672291263179 ) ) ;
#38677 = CARTESIAN_POINT ( 'NONE',  ( 2.354312230267378236, 5.898448035287240820, -0.7998128361456281477 ) ) ;
#38678 = CARTESIAN_POINT ( 'NONE',  ( 5.239300017038202917, 5.077214539491492928, 0.000000000000000000 ) ) ;
#38679 = ORIENTED_EDGE ( 'NONE', *, *, #121920, .F. ) ;
#38681 = CARTESIAN_POINT ( 'NONE',  ( -0.1047997906430510606, -0.1421793342430139606, -1.981047221590222840 ) ) ;
#38680 = CARTESIAN_POINT ( 'NONE',  ( 3.350949008998193257, 0.4442310927498266948, -1.786741727165648497 ) ) ;
#38682 = CARTESIAN_POINT ( 'NONE',  ( 1.792731522490832230, -2.164186313916468762, 0.7742391241713635353 ) ) ;
#38684 = CARTESIAN_POINT ( 'NONE',  ( 6.473494419632052299, -0.2434444386649399217, 1.946554233954982172 ) ) ;
#38683 = CARTESIAN_POINT ( 'NONE',  ( 3.551873057100287223, 5.166937871415542283, 1.443375672974062551 ) ) ;
#38685 = CARTESIAN_POINT ( 'NONE',  ( -4.391951695823077984, 7.211361847513815704, 1.199719254218464037 ) ) ;
#38686 = DIRECTION ( 'NONE',  ( 0.7592566023653005702, -0.6507913734559639396, 0.000000000000000000 ) ) ;
#38687 = CARTESIAN_POINT ( 'NONE',  ( 3.392734571251673881, -1.844325299564765652, -0.5055192353106837677 ) ) ;
#38688 = CARTESIAN_POINT ( 'NONE',  ( -8.784793466650835825, 12.33634391347959713, 1.199719254218462483 ) ) ;
#38690 = EDGE_CURVE ( 'NONE', #97371, #180616, #51193, .T. ) ;
#38689 = CARTESIAN_POINT ( 'NONE',  ( 6.455362170788604637, 6.771378801287749383, -0.3290997004737963860 ) ) ;
#38691 = CARTESIAN_POINT ( 'NONE',  ( -3.797165540279144214, 6.587721009371067638, 1.199719254218452935 ) ) ;
#38693 = CARTESIAN_POINT ( 'NONE',  ( 1.287742131874554552, -0.8442722623961744777, 1.669378388412197767 ) ) ;
#38692 = CARTESIAN_POINT ( 'NONE',  ( 2.841443172333203204, 0.7501175549536406306, -1.951742197369815912 ) ) ;
#38694 = CARTESIAN_POINT ( 'NONE',  ( 2.179064334209149578, -0.9478932651061505732, -1.779355105811925020 ) ) ;
#38695 = CARTESIAN_POINT ( 'NONE',  ( 8.595506201384020883, 9.130438111143927671, 0.7216878364870438212 ) ) ;
#38696 = CARTESIAN_POINT ( 'NONE',  ( 1.364683531249988535, 4.467708333674754506, -0.7879004041258300672 ) ) ;
#38697 = CARTESIAN_POINT ( 'NONE',  ( 2.823474877308090214, 0.9648067800103199421, -1.448311861076934104 ) ) ;
#38698 = CARTESIAN_POINT ( 'NONE',  ( 5.281064527722868718, 6.119995689553514140, 1.199719254218462483 ) ) ;
#38700 = CARTESIAN_POINT ( 'NONE',  ( 0.000000000000000000, 13.49999999999999822, 0.000000000000000000 ) ) ;
#38699 = DIRECTION ( 'NONE',  ( 0.000000000000000000, 0.000000000000000000, 1.000000000000000000 ) ) ;
#38701 = CARTESIAN_POINT ( 'NONE',  ( 3.844159338287247429, 1.716807015663003311, 0.1666082703000223986 ) ) ;
#38702 = CARTESIAN_POINT ( 'NONE',  ( 3.825867475279482566, 1.171244075711602051, -1.852137614134836907 ) ) ;
#38703 = DIRECTION ( 'NONE',  ( 0.000000000000000000, -9.023263958591316185E-17, 1.000000000000000000 ) ) ;
#38704 = CARTESIAN_POINT ( 'NONE',  ( -11.16206481669071415, 4.728763190537430994, -6.013947724923736082 ) ) ;
#38705 = CARTESIAN_POINT ( 'NONE',  ( 3.485384773837760353, 0.04839624821431457585, 2.170676210889192603 ) ) ;
#38706 = CARTESIAN_POINT ( 'NONE',  ( 2.385134503015675200, 1.669401249834654433, -0.7394980648879890817 ) ) ;
#38707 = CARTESIAN_POINT ( 'NONE',  ( 0.4019237886466847653, 12.32366454968463287, 1.499999999999997113 ) ) ;
#38708 = CARTESIAN_POINT ( 'NONE',  ( 4.979753661315234226, -0.7591050579739184734, 1.976773538454196677 ) ) ;
#38709 = CARTESIAN_POINT ( 'NONE',  ( 6.539320575229232269, 1.262224698349242669, 2.111181586620724637 ) ) ;
#38710 = ORIENTED_EDGE ( 'NONE', *, *, #76837, .T. ) ;
#38712 = CARTESIAN_POINT ( 'NONE',  ( 0.6823417656249882723, 2.988541667008084879, -1.181850606188754593 ) ) ;
#38711 = CARTESIAN_POINT ( 'NONE',  ( 5.267208303392540536, 2.209927380382335826, -0.6089511437187348220 ) ) ;
#38713 = CARTESIAN_POINT ( 'NONE',  ( 6.620655732516652847, 2.468432086671234149, 2.210906647470804565 ) ) ;
#38714 = CARTESIAN_POINT ( 'NONE',  ( 2.758194185376297902, 5.305311418659259814, 1.199719254218452047 ) ) ;
#38715 = CARTESIAN_POINT ( 'NONE',  ( 0.4168467196605326053, -0.7183999135813922132, -1.995210048009891102 ) ) ;
#38716 = CARTESIAN_POINT ( 'NONE',  ( -5.504247177468192476, 7.444707678511436555, 1.443375672974064550 ) ) ;
#38717 = CARTESIAN_POINT ( 'NONE',  ( 3.606105671554957759, 4.269840040644637291, -1.082531754730543083 ) ) ;
#38718 = CARTESIAN_POINT ( 'NONE',  ( -6.534666851662457532, 6.726125536468730459, 1.040834085586084257E-14 ) ) ;
#38719 = ADVANCED_FACE ( 'NONE', ( #124687 ), #199139, .F. ) ;
#38720 = FACE_OUTER_BOUND ( 'NONE', #117786, .T. ) ;
#38721 = ORIENTED_EDGE ( 'NONE', *, *, #59183, .F. ) ;
#38722 = CARTESIAN_POINT ( 'NONE',  ( 5.555314621531947772, -1.277044735018734833, 1.560499014526220307 ) ) ;
#38724 = CARTESIAN_POINT ( 'NONE',  ( 2.870046724737782995, -2.040761436538469198, 0.2982335875671269787 ) ) ;
#38723 = CARTESIAN_POINT ( 'NONE',  ( 4.123651276850781144, 7.962676922967908411, -0.7998128361456221525 ) ) ;
#38726 = CARTESIAN_POINT ( 'NONE',  ( -0.2408018239684278916, 6.947782644136219155, -2.695524888730389090 ) ) ;
#38725 = CARTESIAN_POINT ( 'NONE',  ( 7.614839552730775729, 8.913009562054615031, 1.199719254218452047 ) ) ;
#38727 = CARTESIAN_POINT ( 'NONE',  ( 7.849244587668864348, 8.122149871893999062, 0.7998128361456291469 ) ) ;
#38728 = CARTESIAN_POINT ( 'NONE',  ( -1.642778471874998480, -1.801041666188708090, 2.845375778867863303 ) ) ;
#38729 = CYLINDRICAL_SURFACE ( 'NONE', #123781, 0.08000000000000020983 ) ;
#38730 = CARTESIAN_POINT ( 'NONE',  ( 6.193348084369689310, -0.7418380161853586063, 2.062208804312585020 ) ) ;
#38731 = CARTESIAN_POINT ( 'NONE',  ( 3.762342404062005041, 1.897698010425369786, -0.6819954029829021769 ) ) ;
#38732 = CARTESIAN_POINT ( 'NONE',  ( 3.140019216317342376, 0.4501627324021878485, 1.785233193441162491 ) ) ;
#38733 = CARTESIAN_POINT ( 'NONE',  ( 6.817052309572890323, 6.847649204123507083, 0.7998128361456341429 ) ) ;
#38734 = CARTESIAN_POINT ( 'NONE',  ( 0.4458014021226979207, 1.719615392401403708, 0.1342584403209358679 ) ) ;
#38735 = CARTESIAN_POINT ( 'NONE',  ( -3.735435015764967837, 4.316761258935923884, -1.199719254218452047 ) ) ;
#38736 = CARTESIAN_POINT ( 'NONE',  ( 1.090962482291182312, -0.5517420707249369727, 2.231415953587682299 ) ) ;
#38737 = CARTESIAN_POINT ( 'NONE',  ( -5.388475986427523345, 8.373973519885682393, 1.199719254218452047 ) ) ;
#38738 = CARTESIAN_POINT ( 'NONE',  ( 6.455986150183742112, 2.257016316038124693, -0.1587017259171065731 ) ) ;
#38739 = CARTESIAN_POINT ( 'NONE',  ( 3.457739842999438817, 0.5116738510754537117, -2.042838612040797752 ) ) ;
#38740 = CARTESIAN_POINT ( 'NONE',  ( -4.553559489343377287, 6.405848385690952718, -1.599625672291271394 ) ) ;
#38741 = CARTESIAN_POINT ( 'NONE',  ( 7.287671262545424966, 8.461036880179857889, -1.199719254218451159 ) ) ;
#38742 = CARTESIAN_POINT ( 'NONE',  ( 5.628043163004202931, 8.619781885929965526, -1.082531754730548412 ) ) ;
#38743 = CARTESIAN_POINT ( 'NONE',  ( -7.250913225210214641, 7.353820272367037170, 0.7998128361456341429 ) ) ;
#38744 = B_SPLINE_CURVE_WITH_KNOTS ( 'NONE', 3,
 ( #189860, #158439, #76114, #139003, #8977, #208232 ),
 .UNSPECIFIED., .F., .F.,
 ( 4, 2, 4 ),
 ( 0.000000000000000000, 0.0003172254002810710651, 0.0006344508005621421302 ),
 .UNSPECIFIED. ) ;
#38745 = CARTESIAN_POINT ( 'NONE',  ( 6.114364089638786304, 8.156510742710487705, 1.443375672974076540 ) ) ;
#38746 = CARTESIAN_POINT ( 'NONE',  ( 4.602920755658417740, 7.148668813305413039, 1.337190490212318839 ) ) ;
#38747 = CARTESIAN_POINT ( 'NONE',  ( -4.737684612971557740, 7.614716917520386374, 1.199719254218464037 ) ) ;
#38748 = CARTESIAN_POINT ( 'NONE',  ( 4.430067838210618447, -2.178247905445731103, 0.4349904863075284567 ) ) ;
#38749 = CARTESIAN_POINT ( 'NONE',  ( 2.642740014504705304, -1.821389600533461994, 1.218302608185666491 ) ) ;
#38750 = CARTESIAN_POINT ( 'NONE',  ( -6.901263884555985051, 8.010228272525461435, 1.199719254218450271 ) ) ;
#38751 = AXIS2_PLACEMENT_3D ( 'NONE', #143897, #74592, #140695 ) ;
#38752 = CARTESIAN_POINT ( 'NONE',  ( -4.122561227007127016, 6.967349310553715647, 1.199719254218452935 ) ) ;
#38753 = CARTESIAN_POINT ( 'NONE',  ( 5.318788500806308051, -1.422220495204097546, 1.351624447685224162 ) ) ;
#38754 = CARTESIAN_POINT ( 'NONE',  ( 0.6823417656249882723, 1.676041667008083769, -1.181850606188749264 ) ) ;
#38755 = CARTESIAN_POINT ( 'NONE',  ( 6.610000000000042952, 4.702635990354799844, 2.282722937023287102 ) ) ;
#38756 = CARTESIAN_POINT ( 'NONE',  ( -5.083944415444539899, 8.875092884753202682, 0.000000000000000000 ) ) ;
#38757 = CARTESIAN_POINT ( 'NONE',  ( 4.342108446431157454, -1.306982937058022820, -1.669832246961988176 ) ) ;
#38758 = CARTESIAN_POINT ( 'NONE',  ( -3.149236820124241110, 6.896136400112061970, -0.7998128361456481317 ) ) ;
#38759 = ORIENTED_EDGE ( 'NONE', *, *, #21974, .T. ) ;
#38760 = CARTESIAN_POINT ( 'NONE',  ( 5.700121470611750674, -2.161883445634639411, -0.004416275431240455560 ) ) ;
#38761 = CARTESIAN_POINT ( 'NONE',  ( 6.331821432781979730, 7.345878745455822312, -1.199719254218445830 ) ) ;
#38762 = CARTESIAN_POINT ( 'NONE',  ( 4.985823801847525161, -1.827980399782932697, -0.2200341325891697619 ) ) ;
#38763 = CARTESIAN_POINT ( 'NONE',  ( -5.890076507333620981, 6.013243542187837853, -0.2543948676220365024 ) ) ;
#38764 = CARTESIAN_POINT ( 'NONE',  ( 1.364683531249986537, 0.9677083336747538400, -0.7879004041258239610 ) ) ;
#38765 = CARTESIAN_POINT ( 'NONE',  ( 0.2393033055489251493, 1.735545043620636996, 0.1309560527960016429 ) ) ;
#38766 = CARTESIAN_POINT ( 'NONE',  ( 6.727182134110222478, 3.706444386917655986, 2.325533714637216143 ) ) ;
#38767 = CARTESIAN_POINT ( 'NONE',  ( -1.402160292154681736E-14, -0.7406249996585823059, -1.575800808251665908 ) ) ;
#38768 = CARTESIAN_POINT ( 'NONE',  ( -1.225000000000044276, 1.770833333333392545, 0.7072540797572737237 ) ) ;
#38769 = CARTESIAN_POINT ( 'NONE',  ( 3.872077330825273389, 1.198917189070296541, 1.798566189592496034 ) ) ;
#38770 = CARTESIAN_POINT ( 'NONE',  ( -5.057354993097396445, 5.859001232490445688, -1.199719254218446718 ) ) ;
#38771 = CIRCLE ( 'NONE', #101060, 0.08000000000000020983 ) ;
#38772 = CARTESIAN_POINT ( 'NONE',  ( -7.659993601596726265, 8.039006744725394782, -0.7216878364870267237 ) ) ;
#38773 = CARTESIAN_POINT ( 'NONE',  ( 3.327187652246216931, 0.05129554954072869377, 2.161254785723889515 ) ) ;
#38774 = CARTESIAN_POINT ( 'NONE',  ( 4.534422775129973715, 1.932726017421485976, 0.3875534085790635630 ) ) ;
#38775 = CARTESIAN_POINT ( 'NONE',  ( 3.602662725270942445, 0.7809228151291653930, -1.548105009325143833 ) ) ;
#38776 = CARTESIAN_POINT ( 'NONE',  ( 1.136565065649897344, 0.4323997850379875385, 2.148315308122191514 ) ) ;
#38777 = CARTESIAN_POINT ( 'NONE',  ( 1.360874125193665130, 0.9374058560891560532, 2.108772699047257948 ) ) ;
#38778 = CARTESIAN_POINT ( 'NONE',  ( 3.479809507395460244, 1.304684485917747994, 1.595210877418812956 ) ) ;
#38779 = CARTESIAN_POINT ( 'NONE',  ( 5.390160969041248862, -0.4756269310413098750, -1.882793909387857179 ) ) ;
#38781 = VERTEX_POINT ( 'NONE', #65952 ) ;
#38780 = CARTESIAN_POINT ( 'NONE',  ( -7.659993601596713830, 9.959745173328078849, -1.443375672974058777 ) ) ;
#38782 = CARTESIAN_POINT ( 'NONE',  ( -4.145761110728687804, 8.058748072483927771, -0.7998128361456481317 ) ) ;
#38783 = SURFACE_STYLE_USAGE ( .BOTH. , #57167 ) ;
#38784 = CARTESIAN_POINT ( 'NONE',  ( -4.462568837553487100, 5.235360394347691404, -1.199719254218453823 ) ) ;
#38785 = CARTESIAN_POINT ( 'NONE',  ( -8.500599125644013654, 9.019713189447241319, 0.7216878364870438212 ) ) ;
#38786 = CARTESIAN_POINT ( 'NONE',  ( 3.874219531129017291, 1.223701582695544854, 1.836212042189053761 ) ) ;
#38787 = CARTESIAN_POINT ( 'NONE',  ( -3.285556943750000514, -3.726041666188710799, -1.896917185911906500 ) ) ;
#38788 = ORIENTED_EDGE ( 'NONE', *, *, #29409, .T. ) ;
#38789 = CARTESIAN_POINT ( 'NONE',  ( 1.234942694251008000, -0.03850059531256519452, -1.860717468297488297 ) ) ;
#38790 = CARTESIAN_POINT ( 'NONE',  ( -0.1291982275798807533, 5.720674304969967316, -2.668085245563474484 ) ) ;
#38791 = CARTESIAN_POINT ( 'NONE',  ( 0.7499999999999920064, 5.514583334016151639, 1.299038105676669330 ) ) ;
#38792 = CARTESIAN_POINT ( 'NONE',  ( 4.298292216229534723, 7.460037067547172107, -1.072071942351945584 ) ) ;
#38794 = CARTESIAN_POINT ( 'NONE',  ( 6.925078400183590333, 2.001873123210990535, 2.545813127278444998 ) ) ;
#38793 = FACE_OUTER_BOUND ( 'NONE', #43723, .T. ) ;
#38795 = DIRECTION ( 'NONE',  ( 0.000000000000000000, 1.000000000000000000, 0.000000000000000000 ) ) ;
#38796 = ORIENTED_EDGE ( 'NONE', *, *, #43620, .T. ) ;
#38797 = CARTESIAN_POINT ( 'NONE',  ( 2.747006664573675039, -1.714185755289293622, 1.143718651939158670 ) ) ;
#38798 = CARTESIAN_POINT ( 'NONE',  ( -1.552391752028397856E-14, -0.04687499965855816686, 1.570758158831750295 ) ) ;
#38799 = CARTESIAN_POINT ( 'NONE',  ( -6.287230548435221777, 8.358188277972981695, -1.599625672291263179 ) ) ;
#38800 = CARTESIAN_POINT ( 'NONE',  ( 10.91962425643199985, -9.999999999999994671, -0.09058751758333170867 ) ) ;
#38801 = CARTESIAN_POINT ( 'NONE',  ( 3.310162060030825248, 7.013606170011280838, -0.7998128361456291469 ) ) ;
#38802 = COLOUR_RGB ( '', 0.09019608, 0.27058824, 0.51372549) ;
#38803 = CARTESIAN_POINT ( 'NONE',  ( 1.041951191326966342, 0.8359002368949167705, -1.883948988615320896 ) ) ;
#38805 = CARTESIAN_POINT ( 'NONE',  ( -0.6823417656250039265, 13.31770833367473195, -1.181850606188755259 ) ) ;
#38804 = CARTESIAN_POINT ( 'NONE',  ( 4.882711408206717785, 4.933808380148556161, 0.6288647573781755984 ) ) ;
#38806 = CARTESIAN_POINT ( 'NONE',  ( 5.656776405399742025, 7.622658444431597680, -1.599625672291262513 ) ) ;
#38807 = CARTESIAN_POINT ( 'NONE',  ( 5.830760709146560750, 2.125890151018691832, 0.5921790101122563765 ) ) ;
#38808 = CARTESIAN_POINT ( 'NONE',  ( 6.591137597455673180, 1.973280021476801149, -1.106527213950120547 ) ) ;
#38809 = CARTESIAN_POINT ( 'NONE',  ( -5.599154252763867134, 5.634694171087028636, 0.000000000000000000 ) ) ;
#38810 = CARTESIAN_POINT ( 'NONE',  ( 6.504213119055646253, -0.7662104867102972339, 1.640237621407932167 ) ) ;
#38811 = CARTESIAN_POINT ( 'NONE',  ( 0.9015777671340443611, -1.966303774932298021, 0.4465067697373495403 ) ) ;
#38812 = CARTESIAN_POINT ( 'NONE',  ( 6.821160681006781523, 9.051383109298340557, 1.443375672974063439 ) ) ;
#38813 = CARTESIAN_POINT ( 'NONE',  ( 1.370962024642598864, -0.5571102548348834116, 2.229726662508556778 ) ) ;
#38814 = ADVANCED_FACE ( 'NONE', ( #113751 ), #65039, .T. ) ;
#38815 = CARTESIAN_POINT ( 'NONE',  ( -4.218512253981381299, 3.978430757497701364, -0.5307291018261834914 ) ) ;
#38816 = CARTESIAN_POINT ( 'NONE',  ( -0.4359479416626658721, -6.334709917115479705, -9.855659161987901484 ) ) ;
#38817 = B_SPLINE_CURVE_WITH_KNOTS ( 'NONE', 3,
 ( #53665, #52595, #88307, #187916 ),
 .UNSPECIFIED., .F., .F.,
 ( 4, 4 ),
 ( 1.113895019748840813E-15, 8.505390839970735750E-05 ),
 .UNSPECIFIED. ) ;
#38818 = CARTESIAN_POINT ( 'NONE',  ( 1.844031106778964535, 8.927559574663328945, -0.7749999999999996891 ) ) ;
#38819 = CARTESIAN_POINT ( 'NONE',  ( 1.463515404423965105, 1.843522461416190250, -0.3164952454337774390 ) ) ;
#38820 = CARTESIAN_POINT ( 'NONE',  ( 2.202361591730035428, 1.313542931311746598, -1.530159205979222170 ) ) ;
#38822 = CARTESIAN_POINT ( 'NONE',  ( 11.41381678389397614, 13.52879418241072074, 3.704697885617693753 ) ) ;
#38821 = CARTESIAN_POINT ( 'NONE',  ( -0.6823417656250003738, 0.7177083336747519526, -1.181850606188749264 ) ) ;
#38824 = CARTESIAN_POINT ( 'NONE',  ( 5.022148466640797615, -1.125808720090130111, -1.779717422886097244 ) ) ;
#38823 = CARTESIAN_POINT ( 'NONE',  ( -7.153898609505128015, 11.49796547773133604, 0.7998128361456481317 ) ) ;
#38825 = CARTESIAN_POINT ( 'NONE',  ( 7.934546212495622086, 10.28005655271014795, -1.599625672291262513 ) ) ;
#38827 = CARTESIAN_POINT ( 'NONE',  ( -6.906989191158078079, 10.14557225873805812, -1.199719254218440723 ) ) ;
#38826 = CARTESIAN_POINT ( 'NONE',  ( 3.711900195091365262, 7.552577004240394132, -0.7998128361456362523 ) ) ;
#38828 = CARTESIAN_POINT ( 'NONE',  ( -0.03636482241158912887, -7.019129742886503820, -9.500587730666937958 ) ) ;
#38829 = CARTESIAN_POINT ( 'NONE',  ( 4.465106368662499214, -1.619631974074808412, 1.206539259511850259 ) ) ;
#38830 = CARTESIAN_POINT ( 'NONE',  ( -1.364683531249997417, 4.759375000341424133, 1.214306433183764966E-14 ) ) ;
#38831 = EDGE_CURVE ( 'NONE', #62825, #17090, #135887, .T. ) ;
#38832 = CARTESIAN_POINT ( 'NONE',  ( 6.355934510867760956, -0.6984221382469282258, 1.940952099462374569 ) ) ;
#38833 = CARTESIAN_POINT ( 'NONE',  ( 8.703971430293332645, 12.13808852110884118, -1.082531754730543083 ) ) ;
#38834 = CARTESIAN_POINT ( 'NONE',  ( 5.061884429210019576, 2.138887713127162638, -0.3115965683029159883 ) ) ;
#38835 = CARTESIAN_POINT ( 'NONE',  ( 5.956828388357757298, 8.042995434541133193, 1.599625672291269396 ) ) ;
#38836 = CARTESIAN_POINT ( 'NONE',  ( 1.364683531249986537, -0.2822916663252520997, -0.7879004041258309554 ) ) ;
#38838 = CARTESIAN_POINT ( 'NONE',  ( 9.367496997597598352, 4.518459255872631530, -7.500000000000005329 ) ) ;
#38837 = CARTESIAN_POINT ( 'NONE',  ( 4.830447868218803897, 8.857549289555754157, -0.7998128361456481317 ) ) ;
#38839 = CARTESIAN_POINT ( 'NONE',  ( 6.602457619730749627, 10.64669162308715222, 0.7216878364870438212 ) ) ;
#38841 = CARTESIAN_POINT ( 'NONE',  ( -0.3532572990641859034, -7.666862990898835051, 10.99465531782957939 ) ) ;
#38840 = CARTESIAN_POINT ( 'NONE',  ( 1.961612892103332229, 1.804449789391232795, 1.207184914618843807 ) ) ;
#38843 = CARTESIAN_POINT ( 'NONE',  ( 1.575478407343299692, -0.9843019613302635973, 1.555867251595323353 ) ) ;
#38842 = CARTESIAN_POINT ( 'NONE',  ( -5.829642864196175722, 7.824335979694092558, 1.443375672974064550 ) ) ;
#38844 = CARTESIAN_POINT ( 'NONE',  ( -1.364683531250012516, 2.780208333674754506, 0.7879004041258379498 ) ) ;
#38845 = CARTESIAN_POINT ( 'NONE',  ( 2.999763140970078901, -2.188934734890151113, 0.1099877568606702771 ) ) ;
#38846 = CARTESIAN_POINT ( 'NONE',  ( 6.983263157960365675, 7.052158404629149224, 2.651961988451009944 ) ) ;
#38847 = CARTESIAN_POINT ( 'NONE',  ( 4.223666230214691453, -2.166182250408314580, 0.6532043330096364286 ) ) ;
#38848 = CARTESIAN_POINT ( 'NONE',  ( -6.555530967407501741, 7.606873202518897870, 1.199719254218450271 ) ) ;
#38849 = CARTESIAN_POINT ( 'NONE',  ( -1.874158809982179319, 3.299964346911585356, 0.3999999999999993006 ) ) ;
#38850 = CARTESIAN_POINT ( 'NONE',  ( 5.969043672405669909, 7.102642550806028687, -1.084880274121432064 ) ) ;
#38851 = CARTESIAN_POINT ( 'NONE',  ( -1.500000000000015099, 13.22916666666667140, -0.8660254037844309360 ) ) ;
#38852 = CARTESIAN_POINT ( 'NONE',  ( 6.726253606155519371, 7.019919760035800316, -0.7216878364870458196 ) ) ;
#38853 = CARTESIAN_POINT ( 'NONE',  ( 5.729715491186369469, -1.123817246201250786, -1.367138390065870457 ) ) ;
#38854 = CIRCLE ( 'NONE', #4327, 11.09999999999999964 ) ;
#38855 = CARTESIAN_POINT ( 'NONE',  ( 6.923409998072794558, 11.22906209772695618, 1.040834085586084257E-14 ) ) ;
#38856 = CARTESIAN_POINT ( 'NONE',  ( 1.536301591958776802, 1.038269187514633485, -1.832158284056581543 ) ) ;
#38859 = EDGE_CURVE ( 'NONE', #115710, #191004, #213351, .T. ) ;
#38858 = CARTESIAN_POINT ( 'NONE',  ( -1.201851678989727383E-14, 2.712500000000023892, 1.732050807568877637 ) ) ;
#38857 = CARTESIAN_POINT ( 'NONE',  ( -0.6823417656250039265, 11.56770833367473017, -1.181850606188755259 ) ) ;
#38860 = CARTESIAN_POINT ( 'NONE',  ( 0.8890313061419883311, 0.1412731933134198092, 1.964529561086136189 ) ) ;
#38861 = CARTESIAN_POINT ( 'NONE',  ( -3.135678666510573365, 6.880318554229450712, 0.000000000000000000 ) ) ;
#38862 = CARTESIAN_POINT ( 'NONE',  ( 0.2034672893990868703, -1.513989045467616146, -1.247398002513319781 ) ) ;
#38864 = ORIENTED_EDGE ( 'NONE', *, *, #171794, .F. ) ;
#38863 = CARTESIAN_POINT ( 'NONE',  ( 6.170143040141627289, 1.806061762467878751, -0.1426304505553182556 ) ) ;
#38865 = CARTESIAN_POINT ( 'NONE',  ( 5.178851490740187913, 8.985817805931475277, 0.7216878364870438212 ) ) ;
#38866 = CARTESIAN_POINT ( 'NONE',  ( 0.6823417656249864960, -0.7614583329919113464, -1.181850606188749264 ) ) ;
#38867 = CARTESIAN_POINT ( 'NONE',  ( 5.155093292349416600, -1.580716073637401076, -1.000049079914612449 ) ) ;
#38868 = CARTESIAN_POINT ( 'NONE',  ( 6.104363016364067640, 2.067617457866403718, 0.1074407263862015016 ) ) ;
#38869 = CARTESIAN_POINT ( 'NONE',  ( 0.6124999999999932720, 1.666666666666712038, -1.060881119635983083 ) ) ;
#38870 = CARTESIAN_POINT ( 'NONE',  ( -3.960390268523300339, 7.634556056670224855, 1.214306433183764966E-14 ) ) ;
#38871 = CARTESIAN_POINT ( 'NONE',  ( 2.668637133679951035, -0.9572936134980876144, 2.114570777442663640 ) ) ;
#38872 = CARTESIAN_POINT ( 'NONE',  ( -0.7500000000000249800, -0.8083333333333136972, 1.299038105676659116 ) ) ;
#38873 = CARTESIAN_POINT ( 'NONE',  ( 7.775764792637399836, 9.030479331953833011, -1.199719254218441611 ) ) ;
#38874 = CARTESIAN_POINT ( 'NONE',  ( -9.515124878692420296, 9.995400534762978850, 1.040834085586084257E-14 ) ) ;
#38875 = CARTESIAN_POINT ( 'NONE',  ( 7.354371980770088690, 7.544798497178720531, 0.000000000000000000 ) ) ;
#38876 = EDGE_CURVE ( 'NONE', #84144, #157271, #68715, .T. ) ;
#38877 = CARTESIAN_POINT ( 'NONE',  ( -1.364683531250014514, 0.03020833367475737191, 0.7879004041258379498 ) ) ;
#38878 = CARTESIAN_POINT ( 'NONE',  ( -1.500000000000013101, 1.629166666666691077, -0.8660254037844313801 ) ) ;
#38880 = CARTESIAN_POINT ( 'NONE',  ( 5.497994985541524215, 6.373081223675282736, -1.199719254218445830 ) ) ;
#38879 = CARTESIAN_POINT ( 'NONE',  ( 5.600043156098196917, 0.7966083592686534764, -1.793046234938546757 ) ) ;
#38881 = CARTESIAN_POINT ( 'NONE',  ( 2.231795861093866851, -1.842164517099669441, -0.8196493499348647127 ) ) ;
#38882 = DIRECTION ( 'NONE',  ( -0.000000000000000000, -1.000000000000000000, -0.000000000000000000 ) ) ;
#38883 = CARTESIAN_POINT ( 'NONE',  ( 0.7147126110796617748, 2.027027023440019171, 0.8336157706642086662 ) ) ;
#38884 = DIRECTION ( 'NONE',  ( -0.000000000000000000, -1.000000000000000000, -0.000000000000000000 ) ) ;
#38885 = CARTESIAN_POINT ( 'NONE',  ( 2.126040175964475143, 1.080828230516362121, -1.526477596812993553 ) ) ;
#38886 = CARTESIAN_POINT ( 'NONE',  ( 1.364683531249988535, 4.905208333674756283, -0.7879004041258300672 ) ) ;
#38887 = CARTESIAN_POINT ( 'NONE',  ( 3.849861664782163739, -1.391318219759619002, -1.455273641467175860 ) ) ;
#38888 = CARTESIAN_POINT ( 'NONE',  ( -8.670602931139386627, 10.07445716020612103, 1.199719254218462483 ) ) ;
#38890 = CARTESIAN_POINT ( 'NONE',  ( 3.972345043000875098, -2.094467101900459483, -0.3087697250930310222 ) ) ;
#38889 = CARTESIAN_POINT ( 'NONE',  ( -5.639828713604883248, 6.642516923036197340, 1.082531754730548412 ) ) ;
#38891 = DIRECTION ( 'NONE',  ( 0.000000000000000000, -1.000000000000000000, 0.000000000000000000 ) ) ;
#38892 = CARTESIAN_POINT ( 'NONE',  ( 6.074686117427479992, 1.393331124738606652, -1.531503843499823381 ) ) ;
#38894 = CARTESIAN_POINT ( 'NONE',  ( 6.720655732516648051, 2.039834428248034293, 2.379457109286802208 ) ) ;
#38893 = CARTESIAN_POINT ( 'NONE',  ( 0.8903107040577078468, -0.5117213476562210150, -2.027015703535272717 ) ) ;
#38896 = ORIENTED_EDGE ( 'NONE', *, *, #208458, .T. ) ;
#38895 = CARTESIAN_POINT ( 'NONE',  ( 6.809597967592865508, -0.3964169337347979161, 1.788522171948719874 ) ) ;
#38897 = CARTESIAN_POINT ( 'NONE',  ( 7.293396569147545527, 10.59638086639245280, 1.199719254218460707 ) ) ;
#38898 = CARTESIAN_POINT ( 'NONE',  ( 7.749822179018763357, -6.479141885268237644, -7.806953216197509704 ) ) ;
#38900 = VECTOR ( 'NONE', #86605, 1000.000000000000000 ) ;
#38899 =( NAMED_UNIT ( * ) PLANE_ANGLE_UNIT ( ) SI_UNIT ( $, .RADIAN. ) );
#38901 = CARTESIAN_POINT ( 'NONE',  ( -10.82858503610327894, 5.585649091226504659, 6.509997993261127824 ) ) ;
#38902 = CARTESIAN_POINT ( 'NONE',  ( 7.632877294369377452, 8.967740267261513409, -1.082531754730537976 ) ) ;
#38903 = CARTESIAN_POINT ( 'NONE',  ( -1.402160292154681736E-14, 12.73437500034139980, 1.575800808251682339 ) ) ;
#38904 = CARTESIAN_POINT ( 'NONE',  ( 6.270165159132718991, 1.906809857242173445, -0.1455798257045255728 ) ) ;
#38905 = CARTESIAN_POINT ( 'NONE',  ( -6.970863535720637216, 11.28442455831609337, 0.7998128361456481317 ) ) ;
#38906 = CARTESIAN_POINT ( 'NONE',  ( 5.952193131599331721, 6.902979060742733708, 1.199719254218462483 ) ) ;
#38908 = B_SPLINE_CURVE_WITH_KNOTS ( 'NONE', 3,
 ( #12906, #124639, #109440, #112633 ),
 .UNSPECIFIED., .F., .F.,
 ( 4, 4 ),
 ( 0.000000000000000000, 8.505390838610257180E-05 ),
 .UNSPECIFIED. ) ;
#38907 = DIRECTION ( 'NONE',  ( -1.000000000000000000, -1.224646799147353454E-16, 0.000000000000000000 ) ) ;
#38909 = CARTESIAN_POINT ( 'NONE',  ( -2.081668171172168513E-14, 5.868705557303649734, 4.125226524755077229 ) ) ;
#38910 = CARTESIAN_POINT ( 'NONE',  ( 2.510230996824538430, 6.080353262937265413, 0.000000000000000000 ) ) ;
#38911 = ORIENTED_EDGE ( 'NONE', *, *, #51077, .T. ) ;
#38912 = CARTESIAN_POINT ( 'NONE',  ( 6.292592244351721043, 1.492246071875057423, -1.356311808412967723 ) ) ;
#38913 = CARTESIAN_POINT ( 'NONE',  ( 0.5047332052380922862, -2.104974169346077506, -0.2554120829242333968 ) ) ;
#38914 = CARTESIAN_POINT ( 'NONE',  ( 1.253848497529134409, -2.775557561562891351E-14, 0.5275650105875644424 ) ) ;
#38915 = AXIS2_PLACEMENT_3D ( 'NONE', #135616, #6645, #184337 ) ;
#38916 = CARTESIAN_POINT ( 'NONE',  ( 2.273753298029672187, 5.671309185932734032, 0.4822658753677200871 ) ) ;
#38917 = CARTESIAN_POINT ( 'NONE',  ( -4.284013352238255301, 6.981470763377843447, -1.082531754730549967 ) ) ;
#38918 = CARTESIAN_POINT ( 'NONE',  ( 2.737856954955798727, 5.281584649835344258, 1.199719254218452047 ) ) ;
#38919 = CARTESIAN_POINT ( 'NONE',  ( 3.836728334651629879, -1.896773656598240709, -0.5296851528490874594 ) ) ;
#38920 = CARTESIAN_POINT ( 'NONE',  ( 4.763296089436113157, 1.880429982106451181, -0.7283946704290320540 ) ) ;
#38921 = CARTESIAN_POINT ( 'NONE',  ( -5.693534442735004752, 8.729875052244421951, 1.199719254218452047 ) ) ;
#38922 = CARTESIAN_POINT ( 'NONE',  ( -9.486581398170532253, -9.006862915010220405, 0.5116190538792247944 ) ) ;
#38923 = CARTESIAN_POINT ( 'NONE',  ( 4.910206770677443266, 1.512653250323254817, -1.585896273577400706 ) ) ;
#38924 = PLANE ( 'NONE',  #126355 ) ;
#38925 = CARTESIAN_POINT ( 'NONE',  ( 3.627879330711426320, -1.146429500678107116, -1.547990911671823566 ) ) ;
#38926 = CARTESIAN_POINT ( 'NONE',  ( -7.426115451983156923, 9.686887332112256388, -1.599625672291263179 ) ) ;
#38927 = CARTESIAN_POINT ( 'NONE',  ( -0.02948999725181991258, 7.629137130509059617, -2.526318448094333480 ) ) ;
#38928 = CARTESIAN_POINT ( 'NONE',  ( 0.1181803206181560040, -2.163391993613572151, 0.4351206515559591370 ) ) ;
#38929 = FACE_OUTER_BOUND ( 'NONE', #211277, .T. ) ;
#38930 = CARTESIAN_POINT ( 'NONE',  ( -4.385389099566589621, 14.48107117044276571, 11.17888682965734937 ) ) ;
#38931 = CARTESIAN_POINT ( 'NONE',  ( 5.996784015946103885, 5.890669528225568996, 1.040834085586084257E-14 ) ) ;
#38932 = ORIENTED_EDGE ( 'NONE', *, *, #169477, .F. ) ;
#38933 = CARTESIAN_POINT ( 'NONE',  ( 5.560252395380222090, 5.659585014131299552, 0.7216878364870328300 ) ) ;
#38934 = ORIENTED_EDGE ( 'NONE', *, *, #41175, .F. ) ;
#38935 = CARTESIAN_POINT ( 'NONE',  ( 4.873860229706322933, -1.932217566332248282, 0.3801659098390720581 ) ) ;
#38936 = EDGE_LOOP ( 'NONE', ( #126806, #64979, #135951, #92013, #28125, #12586 ) ) ;
#38938 = CARTESIAN_POINT ( 'NONE',  ( 4.195951375888273382, 1.316525029674735947, 1.522990447314742424 ) ) ;
#38937 = CARTESIAN_POINT ( 'NONE',  ( 0.8900594323104525918, -0.4731300603538539096, -1.883416623991182481 ) ) ;
#38939 = CARTESIAN_POINT ( 'NONE',  ( 5.677245700908649439, -1.026343684741271023, -2.056567161392281129 ) ) ;
#38941 = CARTESIAN_POINT ( 'NONE',  ( 3.608110912359719258, 1.861131631771815842, 0.004268880383616681894 ) ) ;
#38940 = CARTESIAN_POINT ( 'NONE',  ( -6.084577077482911101, 10.32070003369722144, 0.000000000000000000 ) ) ;
#38942 = CARTESIAN_POINT ( 'NONE',  ( 3.285556943750000514, -0.6635416661887083567, 1.896917185911906500 ) ) ;
#38943 = CARTESIAN_POINT ( 'NONE',  ( 1.220146605508150803E-14, 11.43749999999999822, -1.499999999999998446 ) ) ;
#38944 = CARTESIAN_POINT ( 'NONE',  ( -8.044065211609668253, 8.279164256499745633, 0.7998128361456602331 ) ) ;
#38945 = EDGE_CURVE ( 'NONE', #152917, #195805, #137407, .T. ) ;
#38946 = CARTESIAN_POINT ( 'NONE',  ( -4.502716413514301408, 7.306900678191715848, -1.082531754730549967 ) ) ;
#38947 = CARTESIAN_POINT ( 'NONE',  ( 6.233939691744167177, 2.068093053085200417, 0.3059697267470474769 ) ) ;
#38948 = CARTESIAN_POINT ( 'NONE',  ( 5.016153647376201619, 7.835634441038803466, 1.082531754730558626 ) ) ;
#38949 = ORIENTED_EDGE ( 'NONE', *, *, #27652, .T. ) ;
#38950 = AXIS2_PLACEMENT_3D ( 'NONE', #50550, #199982, #51629 ) ;
#38951 = CARTESIAN_POINT ( 'NONE',  ( 10.96964784646768010, -7.712340523144908921, -0.6288774950739197678 ) ) ;
#38952 = CARTESIAN_POINT ( 'NONE',  ( 4.713352964544355039, 8.277509442901161307, 0.6665495596407186030 ) ) ;
#38953 = CARTESIAN_POINT ( 'NONE',  ( -0.01727558406095473439, -0.1313277740116538805, -1.795991579427682616 ) ) ;
#38954 = CARTESIAN_POINT ( 'NONE',  ( -5.773074481320628948, 5.629675071162500544, 0.000000000000000000 ) ) ;
#38955 = CARTESIAN_POINT ( 'NONE',  ( 3.023724745236521017, -1.528101708971361106, 0.8198667277116710173 ) ) ;
#38956 = CARTESIAN_POINT ( 'NONE',  ( 6.902720145097976712, 15.44736672593543148, 9.761920446463514978 ) ) ;
#38957 = CARTESIAN_POINT ( 'NONE',  ( 6.509000000000016328, 7.053097208480951785, 2.498154145070859311 ) ) ;
#38958 = CARTESIAN_POINT ( 'NONE',  ( -7.230575994789712801, 7.330093503543126054, 0.7998128361456341429 ) ) ;
#38959 = CYLINDRICAL_SURFACE ( 'NONE', #39586, 2.750000000000008438 ) ;
#38960 = CARTESIAN_POINT ( 'NONE',  ( 6.965710887581792576, -0.4882203796070741508, 2.123536573467856403 ) ) ;
#38961 = CARTESIAN_POINT ( 'NONE',  ( 5.549374350267230582, -1.441814640532925074, -1.119852386600270533 ) ) ;
#38962 = CARTESIAN_POINT ( 'NONE',  ( 3.344534541303633368, -1.931932779036081183, -0.3399374921491463142 ) ) ;
#38963 = CARTESIAN_POINT ( 'NONE',  ( 0.6124999999999793943, -0.8541666659838200726, 1.060881119635887604 ) ) ;
#38964 = CARTESIAN_POINT ( 'NONE',  ( -9.664264568442742842, 10.16939683947169115, -0.7998128361456291469 ) ) ;
#38965 = CARTESIAN_POINT ( 'NONE',  ( 7.949158136313996259, 8.168439335321471262, 1.040834085586084257E-14 ) ) ;
#38966 = CARTESIAN_POINT ( 'NONE',  ( 4.125719030757846184, -0.3612518283466863434, 2.089324717668067599 ) ) ;
#38967 = DIRECTION ( 'NONE',  ( 1.000000000000000000, -0.000000000000000000, 1.224646799147353207E-16 ) ) ;
#38968 = CARTESIAN_POINT ( 'NONE',  ( -10.62011439820619429, 11.28455497419572318, -0.7998128361456221525 ) ) ;
#38969 = CARTESIAN_POINT ( 'NONE',  ( 1.832961912758425349, -1.964510197511709189, -0.6532998099852762586 ) ) ;
#38971 = CARTESIAN_POINT ( 'NONE',  ( -1.364683531250014514, -1.157291666325248158, 0.7879004041258379498 ) ) ;
#38970 = CARTESIAN_POINT ( 'NONE',  ( -11.89204169242383102, 11.29999999999999893, 0.8046421800351404308 ) ) ;
#38973 = EDGE_LOOP ( 'NONE', ( #133862, #116237 ) ) ;
#38972 = CARTESIAN_POINT ( 'NONE',  ( 4.530067796519579026, -2.178530490643998174, 0.4330045798939685109 ) ) ;
#38974 = CARTESIAN_POINT ( 'NONE',  ( 2.215865853697509102, 2.230823145726851475, 0.5541181435367804609 ) ) ;
#38976 = CARTESIAN_POINT ( 'NONE',  ( 6.666849506214659549, 1.532398756413049457, -1.380780335402414849 ) ) ;
#38975 = CARTESIAN_POINT ( 'NONE',  ( 9.164948653157988900, 11.71552606681625619, -1.443375672974057666 ) ) ;
#38978 = CARTESIAN_POINT ( 'NONE',  ( 1.737500000000001155, -0.9333333333333346804, 3.009438278150922130 ) ) ;
#38977 = CARTESIAN_POINT ( 'NONE',  ( 6.780486220610169035, 9.003929572168926754, -1.443375672974078761 ) ) ;
#38979 = CARTESIAN_POINT ( 'NONE',  ( 6.515202330376022921, -1.784155196879381622, 0.4545711315065634195 ) ) ;
#38980 = VERTEX_POINT ( 'NONE', #201294 ) ;
#38981 = CARTESIAN_POINT ( 'NONE',  ( -10.56178662260468393, -8.763419982614969683, 0.1843566712555078646 ) ) ;
#38982 = EDGE_CURVE ( 'NONE', #897, #16835, #119071, .T. ) ;
#38983 = CARTESIAN_POINT ( 'NONE',  ( 3.410326831400651404, -1.910418641682644969, -0.08914582809275289899 ) ) ;
#38984 = CARTESIAN_POINT ( 'NONE',  ( -0.2214363961139278192, 7.035828811087419865, -3.928328033908623507 ) ) ;
#38985 = CARTESIAN_POINT ( 'NONE',  ( 3.592533753846867128, -0.3360022577178176650, -1.691527450499834995 ) ) ;
#38986 = CARTESIAN_POINT ( 'NONE',  ( 2.061732777098632230, 1.244387006429502396, 1.586668050434843158 ) ) ;
#38987 = CARTESIAN_POINT ( 'NONE',  ( 3.973462176510922816, -2.273730406356341049, -0.3370867821424743949 ) ) ;
#38988 = CARTESIAN_POINT ( 'NONE',  ( 4.024925711125073136, 2.146699088035211922, 0.7144036547655304714 ) ) ;
#38989 = CARTESIAN_POINT ( 'NONE',  ( 0.1005910224048736229, -2.206496634663042133, -0.04943112074598519229 ) ) ;
#38990 = CARTESIAN_POINT ( 'NONE',  ( -5.478903473698255588, 7.485416367438324059, -1.443375672974066548 ) ) ;
#38991 = ORIENTED_EDGE ( 'NONE', *, *, #78185, .T. ) ;
#38992 = CARTESIAN_POINT ( 'NONE',  ( 5.237463280334829996, -1.251769750873907849, -1.251277626909578222 ) ) ;
#38994 = CARTESIAN_POINT ( 'NONE',  ( 0.9730957290566042417, -0.06121152481648738097, -2.291606990885884265 ) ) ;
#38993 = CARTESIAN_POINT ( 'NONE',  ( 7.472478939787284169, 8.746922180287201698, 1.199719254218452935 ) ) ;
#38995 = CARTESIAN_POINT ( 'NONE',  ( 5.226429366918344144, 0.1390423275269437320, 1.835946739075666745 ) ) ;
#38996 = CARTESIAN_POINT ( 'NONE',  ( -4.471491734408701291, 4.111161866431900513, 1.214306433183764966E-14 ) ) ;
#38997 = CARTESIAN_POINT ( 'NONE',  ( 5.349643074071059878, 2.189064600896481139, -0.1049423877047955811 ) ) ;
#38998 = CARTESIAN_POINT ( 'NONE',  ( -4.132202957115018727, 8.042930226601317401, 0.000000000000000000 ) ) ;
#38999 = CARTESIAN_POINT ( 'NONE',  ( -2.761056838677368397, 6.372983411765559048, 0.7998128361456341429 ) ) ;
#39000 = CARTESIAN_POINT ( 'NONE',  ( -9.716492259128738596, -7.972382850425317358, 0.4652101495396395170 ) ) ;
#39001 = CARTESIAN_POINT ( 'NONE',  ( 6.180147188013234150, -1.146869210499700920, -1.723488058659912392 ) ) ;
#39002 = CARTESIAN_POINT ( 'NONE',  ( 1.077361674225948418, 1.530160568918725872, 1.313541346884481209 ) ) ;
#39003 = CIRCLE ( 'NONE', #70207, 0.1999999999999996503 ) ;
#39004 = CARTESIAN_POINT ( 'NONE',  ( -0.6823417656250212460, 5.551041667008087543, 1.181850606188767472 ) ) ;
#39005 = CARTESIAN_POINT ( 'NONE',  ( 4.477124871421138685, -0.001476069148669684195, -1.926676517386548992 ) ) ;
#39006 = CARTESIAN_POINT ( 'NONE',  ( 1.364683531249996529, 9.713541667008064096, 0.7879004041258405033 ) ) ;
#39007 = CARTESIAN_POINT ( 'NONE',  ( 1.195894564581518660, 2.049875489592466238, -0.8564406981130603391 ) ) ;
#39009 = ORIENTED_EDGE ( 'NONE', *, *, #29854, .F. ) ;
#39008 = CARTESIAN_POINT ( 'NONE',  ( 0.000000000000000000, 1.500000000000001332, 0.000000000000000000 ) ) ;
#39011 = DIRECTION ( 'NONE',  ( -1.000000000000000000, 0.000000000000000000, 0.000000000000000000 ) ) ;
#39010 =( NAMED_UNIT ( * ) PLANE_ANGLE_UNIT ( ) SI_UNIT ( $, .RADIAN. ) );
#39012 = CARTESIAN_POINT ( 'NONE',  ( 9.541187415715040032, 12.15447128979948310, -1.599625672291262513 ) ) ;
#39013 = DIRECTION ( 'NONE',  ( -0.7592566023652994600, -0.6507913734559651608, -0.000000000000000000 ) ) ;
#39014 = FACE_OUTER_BOUND ( 'NONE', #176919, .T. ) ;
#39015 = CARTESIAN_POINT ( 'NONE',  ( 11.28604769787390616, 8.703668910516690005, 3.930664473729216901 ) ) ;
#39016 = CARTESIAN_POINT ( 'NONE',  ( 2.576550507925364109, 1.283677811227203147, -1.483670167215108693 ) ) ;
#39018 = CARTESIAN_POINT ( 'NONE',  ( -0.6823417656250212460, 2.613541667008084879, 1.181850606188767472 ) ) ;
#39017 = CARTESIAN_POINT ( 'NONE',  ( 5.986088515633498197, 6.942523675449257858, -1.199719254218446718 ) ) ;
#39019 = EDGE_CURVE ( 'NONE', #174805, #124865, #30480, .T. ) ;
#39020 = DIRECTION ( 'NONE',  ( 0.000000000000000000, 0.7071067811865445751, 0.7071067811865504593 ) ) ;
#39021 = CARTESIAN_POINT ( 'NONE',  ( 6.672321430365630412, -0.9237476215336395402, -1.730755693189582667 ) ) ;
#39022 = CARTESIAN_POINT ( 'NONE',  ( -7.537443334193545397, 10.88110209227943770, -1.199719254218446718 ) ) ;
#39023 = CARTESIAN_POINT ( 'NONE',  ( -5.219525951136856357, 6.152163700156858539, -1.082531754730543971 ) ) ;
#39024 = CARTESIAN_POINT ( 'NONE',  ( 6.807524309086420367, -0.4794501827766698421, 2.115671360755105646 ) ) ;
#39026 = EDGE_LOOP ( 'NONE', ( #144721, #36221, #199608, #162500 ) ) ;
#39025 = CARTESIAN_POINT ( 'NONE',  ( -6.715366157470410435, 6.729015360003925750, -0.7998128361456291469 ) ) ;
#39027 = CARTESIAN_POINT ( 'NONE',  ( -1.500000000000015099, -1.047916665983845919, 0.8660254037844403729 ) ) ;
#39028 = CARTESIAN_POINT ( 'NONE',  ( 1.106479506788549116, 1.420293003395491693, -1.217391549091076275 ) ) ;
#39029 = CARTESIAN_POINT ( 'NONE',  ( -0.1054646484276201696, -0.7404878594409001202, -1.567598555697255369 ) ) ;
#39031 = CARTESIAN_POINT ( 'NONE',  ( 3.667680160636753506, 1.218766932906123479, 1.821211977396507198 ) ) ;
#39030 = CARTESIAN_POINT ( 'NONE',  ( -1.360316468750042862, 1.869791667008058988, -0.7853790794158961308 ) ) ;
#39032 = CARTESIAN_POINT ( 'NONE',  ( 6.106511577925135548, -0.8227651472764373475, -2.156109995086146647 ) ) ;
#39033 = CARTESIAN_POINT ( 'NONE',  ( 6.503207061003255518, 1.710746398682884140, 1.148667516769467767 ) ) ;
#39034 = CARTESIAN_POINT ( 'NONE',  ( 2.378764330827160212, 1.775374922424903801, -0.7872989649762071052 ) ) ;
#39035 = CARTESIAN_POINT ( 'NONE',  ( -6.371969008298464132, 6.536311385877402458, 1.040834085586084257E-14 ) ) ;
#39036 = DIRECTION ( 'NONE',  ( 0.000000000000000000, 0.000000000000000000, 1.000000000000000000 ) ) ;
#39037 = CARTESIAN_POINT ( 'NONE',  ( 5.126391479742934187, 6.113783160189109722, -1.082531754730548412 ) ) ;
#39038 = CARTESIAN_POINT ( 'NONE',  ( -1.360316468750008667, 0.1197916670080665519, -0.7853790794159001276 ) ) ;
#39039 = CARTESIAN_POINT ( 'NONE',  ( 2.918592439375994552, -1.356299846568160827, -1.492255409411530120 ) ) ;
#39040 = CARTESIAN_POINT ( 'NONE',  ( -5.558479791478509568, 5.587240632920778438, 0.000000000000000000 ) ) ;
#39041 = CARTESIAN_POINT ( 'NONE',  ( -4.945692173934974178, 8.992000979557944973, 0.000000000000000000 ) ) ;
#39042 = CARTESIAN_POINT ( 'NONE',  ( 9.561524646135536543, 12.17819805862340310, -1.599625672291262513 ) ) ;
#39044 = DIRECTION ( 'NONE',  ( -5.578564026256490882E-16, -1.000000000000000000, -9.066213480720158442E-32 ) ) ;
#39043 = CARTESIAN_POINT ( 'NONE',  ( 0.6975366375942676500, -0.6598540886826111951, 1.702458561391326342 ) ) ;
#39045 = CARTESIAN_POINT ( 'NONE',  ( -6.261886844665283114, 8.398896966899865646, 1.599625672291269396 ) ) ;
#39046 = CARTESIAN_POINT ( 'NONE',  ( 0.000000000000000000, 0.000000000000000000, -0.5000000000000004441 ) ) ;
#39047 = CARTESIAN_POINT ( 'NONE',  ( -10.64985034906098882, 4.117567600086831980, 6.884957259278849051 ) ) ;
#39048 = ORIENTED_EDGE ( 'NONE', *, *, #202497, .F. ) ;
#39049 = CARTESIAN_POINT ( 'NONE',  ( 6.385628592921421820, 1.419324251362139133, 1.494494355598655622 ) ) ;
#39050 = CARTESIAN_POINT ( 'NONE',  ( -7.566859129758459979, 8.000626204239226880, 0.000000000000000000 ) ) ;
#39051 = CARTESIAN_POINT ( 'NONE',  ( -0.4019237886466871523, 11.72991455036742714, -1.499999999999998668 ) ) ;
#39052 = DIRECTION ( 'NONE',  ( -0.000000000000000000, -1.000000000000000000, -0.000000000000000000 ) ) ;
#39053 = CARTESIAN_POINT ( 'NONE',  ( -8.136864746495904299, 12.64475930422059768, -0.7998128361456281477 ) ) ;
#39054 = CARTESIAN_POINT ( 'NONE',  ( 5.760417579480547445, 2.017467016246987210, 0.09685271086026786547 ) ) ;
#39055 = CARTESIAN_POINT ( 'NONE',  ( 5.215582523826345351, 1.815199501411597582, 1.280085896050622507 ) ) ;
#39056 = CARTESIAN_POINT ( 'NONE',  ( -3.006876207180748217, 6.730049018344652190, -0.7998128361456481317 ) ) ;
#39057 = CARTESIAN_POINT ( 'NONE',  ( 6.440286661691305703, 7.472421512516709718, 1.199719254218462483 ) ) ;
#39058 = CARTESIAN_POINT ( 'NONE',  ( 5.260643881022500246, -1.494227509126961451, 1.419604852646045634 ) ) ;
#39059 = CARTESIAN_POINT ( 'NONE',  ( 3.779922787921150995, 1.701948043757589124, -1.081065327119046016 ) ) ;
#39060 = ORIENTED_EDGE ( 'NONE', *, *, #82886, .F. ) ;
#39061 = SPHERICAL_SURFACE ( 'NONE', #83374, 0.08000000000000000167 ) ;
#39062 = CARTESIAN_POINT ( 'NONE',  ( 3.354752944377597856, 6.001296637494123232, -1.199719254218446718 ) ) ;
#39064 = ORIENTED_EDGE ( 'NONE', *, *, #187251, .T. ) ;
#39063 = CARTESIAN_POINT ( 'NONE',  ( -7.930593509350902792, 8.217056947189661287, -0.7998128361456362523 ) ) ;
#39065 = CARTESIAN_POINT ( 'NONE',  ( 5.865087380380676230, 7.178575736046542310, -1.148900262672468475 ) ) ;
#39066 = CARTESIAN_POINT ( 'NONE',  ( 3.972029700707707445, 1.727737986437705819, 1.038833660170018769 ) ) ;
#39067 = CARTESIAN_POINT ( 'NONE',  ( 3.029072736150268952, -1.236975958831527445, -1.363863411116640334 ) ) ;
#39068 = CARTESIAN_POINT ( 'NONE',  ( 5.763039058787838620, 7.049721345481010815, 2.500000000000351719 ) ) ;
#39069 = CARTESIAN_POINT ( 'NONE',  ( 2.420946758181366842, 1.505949115154591400, -1.748677306438247703 ) ) ;
#39070 = CARTESIAN_POINT ( 'NONE',  ( 5.422335090822693715, 5.290755458906732933, 0.000000000000000000 ) ) ;
#39071 = ADVANCED_FACE ( 'NONE', ( #154718 ), #138452, .T. ) ;
#39072 = CARTESIAN_POINT ( 'NONE',  ( 3.444745247808535638, 0.5215555581963465803, 2.097624034931542703 ) ) ;
#39073 = CARTESIAN_POINT ( 'NONE',  ( 6.584456157731144899, 10.83361595066169514, -0.7998128361456291469 ) ) ;
#39074 = CARTESIAN_POINT ( 'NONE',  ( -6.261168011412601153, 6.199117522936475666, 1.040834085586084257E-14 ) ) ;
#39075 = CARTESIAN_POINT ( 'NONE',  ( 2.970384050378202634, 1.940355284992447027, 1.231690374697077095 ) ) ;
#39076 = CARTESIAN_POINT ( 'NONE',  ( -1.499999999999984901, 4.160416667349482900, -0.8660254037844477004 ) ) ;
#39077 = AXIS2_PLACEMENT_3D ( 'NONE', #13500, #178156, #144621 ) ;
#39078 = CARTESIAN_POINT ( 'NONE',  ( 2.184254540302111636, -1.834043650784190405, -0.3674020703766100460 ) ) ;
#39079 = CARTESIAN_POINT ( 'NONE',  ( 0.3683541893860732275, -1.290952873633111953, 1.489922359098810878 ) ) ;
#39081 = CARTESIAN_POINT ( 'NONE',  ( -5.738844160334429567, 9.917344963690652548, 0.000000000000000000 ) ) ;
#39080 = CARTESIAN_POINT ( 'NONE',  ( -1.201851678989727383E-14, 4.446875000341417916, -1.575800808251660134 ) ) ;
#39083 = CARTESIAN_POINT ( 'NONE',  ( 1.858336453454629611, 2.200810804183956026, -0.1644699235988852648 ) ) ;
#39082 = CARTESIAN_POINT ( 'NONE',  ( -4.401593425930945713, 8.286942763561420122, 1.040834085586084257E-14 ) ) ;
#39084 = ORIENTED_EDGE ( 'NONE', *, *, #170552, .F. ) ;
#39085 = CARTESIAN_POINT ( 'NONE',  ( -2.680963302752293664, 0.4788041664877169534, -0.1016165050528608921 ) ) ;
#39086 = CARTESIAN_POINT ( 'NONE',  ( 4.306686350635271054, 8.176217842383143974, -0.7998128361456221525 ) ) ;
#39087 = CARTESIAN_POINT ( 'NONE',  ( -4.599240423533815125, 6.388866465587984322, 1.599625672291267398 ) ) ;
#39088 = CARTESIAN_POINT ( 'NONE',  ( 11.94650005372637835, 13.65102700337638275, 1.135399707157307203 ) ) ;
#39089 = CARTESIAN_POINT ( 'NONE',  ( 5.858272006539261056, 0.7985356142178706707, 1.802671990260945156 ) ) ;
#39090 = CARTESIAN_POINT ( 'NONE',  ( 5.936188932989287181, 1.142819166849334378, -2.004778302753240649 ) ) ;
#39092 = ADVANCED_FACE ( 'NONE', ( #72374 ), #57215, .F. ) ;
#39091 = CARTESIAN_POINT ( 'NONE',  ( 6.531710587413017244, 1.780498168465095787, -0.5416703039235416517 ) ) ;
#39093 = CARTESIAN_POINT ( 'NONE',  ( 2.571201674526869763, 1.840362857814400455, 0.9314759700368970829 ) ) ;
#39094 = CARTESIAN_POINT ( 'NONE',  ( 4.989037340148863464, 8.764367963574922982, -0.7216878364870257245 ) ) ;
#39095 = AXIS2_PLACEMENT_3D ( 'NONE', #147197, #13955, #193784 ) ;
#39096 = CARTESIAN_POINT ( 'NONE',  ( 5.643937085038755797, 9.806620042512378177, -0.7998128361456481317 ) ) ;
#39097 = CARTESIAN_POINT ( 'NONE',  ( 5.938108092661121162, 9.871617174839238729, 1.040834085586084257E-14 ) ) ;
#39098 = CARTESIAN_POINT ( 'NONE',  ( -1.364683531250012516, 3.342708333674756727, 0.7879004041258379498 ) ) ;
#39099 = CARTESIAN_POINT ( 'NONE',  ( -9.604686356149274573, 3.481548657788671619, -7.193747284969077782 ) ) ;
#39100 = CARTESIAN_POINT ( 'NONE',  ( 6.114364089638798738, 6.235772314107808079, 0.7216878364870317197 ) ) ;
#39101 = CARTESIAN_POINT ( 'NONE',  ( 6.092256315220226703, 1.075607590566488803, -1.885974292122821527 ) ) ;
#39103 = CARTESIAN_POINT ( 'NONE',  ( 5.108874002337426390, -0.2646564886703614006, 1.822002613180016883 ) ) ;
#39102 = CARTESIAN_POINT ( 'NONE',  ( -11.33772463945036968, 10.19999999999999929, -3.600000000000000977 ) ) ;
#39104 = CARTESIAN_POINT ( 'NONE',  ( 7.065207446497155708, 9.336104335703744539, 0.000000000000000000 ) ) ;
#39105 = CARTESIAN_POINT ( 'NONE',  ( 6.620655732516651071, -0.002413161512292844035, 2.173887093218453082 ) ) ;
#39106 = CARTESIAN_POINT ( 'NONE',  ( 0.2450992160058732550, -1.441561472518913867, -1.191725768352129622 ) ) ;
#39108 = CARTESIAN_POINT ( 'NONE',  ( -4.243318646243602998, 7.513047557524930475, 1.036732258902311354 ) ) ;
#39107 = CIRCLE ( 'NONE', #87503, 0.07999999999999998779 ) ;
#39109 = CARTESIAN_POINT ( 'NONE',  ( 1.499999999999959588, 7.750000000000000000, -10.86128356754324820 ) ) ;
#39110 = CARTESIAN_POINT ( 'NONE',  ( 6.468016842275610578, 6.857101109195174793, 0.6445861549769070775 ) ) ;
#39111 = CARTESIAN_POINT ( 'NONE',  ( 0.06490398442321809735, -1.535895564731554863, 1.139000086266952705 ) ) ;
#39112 =( BOUNDED_CURVE ( )  B_SPLINE_CURVE ( 2, ( #210015, #31301, #46484, #15013, #130991 ),
 .UNSPECIFIED., .F., .T. ) 
 B_SPLINE_CURVE_WITH_KNOTS ( ( 3, 2, 3 ),
 ( 0.2238897612321706643, 0.2250000000000000056, 0.2266653943240793667 ),
 .UNSPECIFIED. ) 
 CURVE ( )  GEOMETRIC_REPRESENTATION_ITEM ( )  RATIONAL_B_SPLINE_CURVE ( ( 0.9690575545878401531, 0.9821507451252642351, 1.000000000000000000, 0.9732255361470136812, 0.9571526819254749796 ) ) 
 REPRESENTATION_ITEM ( '' )  );
#39113 = CARTESIAN_POINT ( 'NONE',  ( 2.271989177565427287, -1.091335633969382490, 1.393213513506918133 ) ) ;
#39114 = CARTESIAN_POINT ( 'NONE',  ( -0.005422908085399994089, -1.854866876809873943, -0.4647201794698225252 ) ) ;
#39116 = CARTESIAN_POINT ( 'NONE',  ( 3.884325381594720739, -0.6044542036256529416, -1.817792542802825428 ) ) ;
#39115 = CARTESIAN_POINT ( 'NONE',  ( -8.805130697071332335, 12.36007068230351358, 1.199719254218462483 ) ) ;
#39117 = CARTESIAN_POINT ( 'NONE',  ( -2.974934349810927525, 6.692942428052418791, -0.01217162047775656973 ) ) ;
#39118 = CARTESIAN_POINT ( 'NONE',  ( 5.178159682156908694, -1.051918566972683600, -1.664904379343169705 ) ) ;
#39119 = CARTESIAN_POINT ( 'NONE',  ( 0.0004480315400831600455, -0.9938866557669153723, 1.873244595478529728 ) ) ;
#39120 = CARTESIAN_POINT ( 'NONE',  ( -2.123823618835070537, 5.629544655282869847, 1.040834085586084257E-14 ) ) ;
#39121 = CARTESIAN_POINT ( 'NONE',  ( 3.274138816734498025, -1.115311402298941656, 1.501645261301733481 ) ) ;
#39123 = ORIENTED_EDGE ( 'NONE', *, *, #191685, .F. ) ;
#39122 = CARTESIAN_POINT ( 'NONE',  ( 6.692093555742618882, -0.7303567666399125580, 1.561414089659449944 ) ) ;
#39125 = CARTESIAN_POINT ( 'NONE',  ( 3.226477370372302644, 5.747678784534228313, 1.082531754730546636 ) ) ;
#39124 = CARTESIAN_POINT ( 'NONE',  ( 1.805583701156989518, 1.836052299496168771, 1.224139149458243425 ) ) ;
#39126 = CARTESIAN_POINT ( 'NONE',  ( -0.6823417656249969321, 3.780208333674754506, -1.181850606188749264 ) ) ;
#39127 = CARTESIAN_POINT ( 'NONE',  ( 0.5200786239168513347, 2.040466299037096309, -0.3010312105025755303 ) ) ;
#39128 = CARTESIAN_POINT ( 'NONE',  ( 7.721532178182734185, 8.967207948423393304, 1.199719254218462483 ) ) ;
#39129 = DIRECTION ( 'NONE',  ( 0.000000000000000000, 0.000000000000000000, -1.000000000000000000 ) ) ;
#39130 = CARTESIAN_POINT ( 'NONE',  ( 1.566537053174811955, 8.754671357082440153, 2.463935854687016480 ) ) ;
#39131 = CARTESIAN_POINT ( 'NONE',  ( -4.253507506385334480, 5.985511395581417204, 1.599625672291267175 ) ) ;
#39132 = CARTESIAN_POINT ( 'NONE',  ( 1.000000000000003553, 6.120000000000020535, 1.214306433183764966E-14 ) ) ;
#39133 = ORIENTED_EDGE ( 'NONE', *, *, #93452, .F. ) ;
#39134 = CARTESIAN_POINT ( 'NONE',  ( 3.437997351728830697, 1.311287738946330439, 1.602184970737066116 ) ) ;
#39135 = CARTESIAN_POINT ( 'NONE',  ( -1.201851678989727383E-14, 4.587500000000025224, -1.732050807568863648 ) ) ;
#39136 = CARTESIAN_POINT ( 'NONE',  ( 4.904298879841284098, 6.744767997946721216, 1.599625672291267398 ) ) ;
#39137 = CARTESIAN_POINT ( 'NONE',  ( -6.616720264197946122, 6.757059058146986708, -0.05018984082068300712 ) ) ;
#39139 = EDGE_CURVE ( 'NONE', #64100, #79124, #82401, .T. ) ;
#39138 = CARTESIAN_POINT ( 'NONE',  ( 0.7682301616282152246, 2.017272972751768645, -0.1012717401170943471 ) ) ;
#39140 =( NAMED_UNIT ( * ) SI_UNIT ( $, .STERADIAN. ) SOLID_ANGLE_UNIT ( ) );
#39141 = CARTESIAN_POINT ( 'NONE',  ( -1.001543065824772872E-14, 4.571875000341418804, 1.575800808251672791 ) ) ;
#39142 = ORIENTED_EDGE ( 'NONE', *, *, #107850, .F. ) ;
#39143 = EDGE_CURVE ( 'NONE', #126275, #194519, #25764, .T. ) ;
#39145 = CARTESIAN_POINT ( 'NONE',  ( 9.300530189294644146, 10.91333531134101165, -1.082531754730543083 ) ) ;
#39144 = CARTESIAN_POINT ( 'NONE',  ( 0.1749903794560228876, 5.724274800596795387, -2.549334106949477263 ) ) ;
#39146 = CARTESIAN_POINT ( 'NONE',  ( 5.677111188754776272, -0.9039728708103295096, -1.802140534545144890 ) ) ;
#39147 = CARTESIAN_POINT ( 'NONE',  ( 5.911341210168471250, -1.801345639624308381, 0.6523577827844198040 ) ) ;
#39148 = CARTESIAN_POINT ( 'NONE',  ( -1.500000000000039524, 7.750000000000000000, -10.86128356754322688 ) ) ;
#39149 = CARTESIAN_POINT ( 'NONE',  ( 3.316156725143477146, 1.388770557483296697, -1.695381604771596606 ) ) ;
#39150 = CARTESIAN_POINT ( 'NONE',  ( 1.499999999999989120, 1.785416667349487563, 0.8660254037844524744 ) ) ;
#39151 = CARTESIAN_POINT ( 'NONE',  ( 2.232540727315056373, 1.246330492051262784, -1.450604739030990187 ) ) ;
#39152 = CARTESIAN_POINT ( 'NONE',  ( -7.054319997812058318, 7.124461507069184130, 1.040834085586084257E-14 ) ) ;
#39153 = CARTESIAN_POINT ( 'NONE',  ( 4.975479186090857375, 5.867442474269873642, 1.082531754730560403 ) ) ;
#39154 = CARTESIAN_POINT ( 'NONE',  ( 1.159780049612362030, 1.203373692603469935, 1.617804775344060308 ) ) ;
#39155 = CARTESIAN_POINT ( 'NONE',  ( -1.402160292154681736E-14, 10.73437500034139802, 1.575800808251682339 ) ) ;
#39157 = CARTESIAN_POINT ( 'NONE',  ( -6.252245114557387851, 7.323316050852266557, -1.199719254218453823 ) ) ;
#39156 = CARTESIAN_POINT ( 'NONE',  ( 5.970311429539967740, -2.080533979117826782, -0.6889730390344513955 ) ) ;
#39159 = ORIENTED_EDGE ( 'NONE', *, *, #155782, .F. ) ;
#39158 = CARTESIAN_POINT ( 'NONE',  ( 2.871755265489631448, 0.9208624611983186048, 1.458155879698035395 ) ) ;
#39160 = CARTESIAN_POINT ( 'NONE',  ( 0.07999999999999327094, -9.746166700180788567, 9.579665964948873125 ) ) ;
#39161 = CARTESIAN_POINT ( 'NONE',  ( 8.444030743212801227, 8.745790710036752458, 0.7998128361456462443 ) ) ;
#39162 = CARTESIAN_POINT ( 'NONE',  ( 4.202137545231717120, 6.989912005157271402, 1.199719254218462483 ) ) ;
#39163 = CARTESIAN_POINT ( 'NONE',  ( -3.475000000000000533, -2.435416665710753215, -2.006292185433948827 ) ) ;
#39164 = CARTESIAN_POINT ( 'NONE',  ( 11.41108574530281494, 9.841631446223743751, -3.405883542057589253 ) ) ;
#39165 = CARTESIAN_POINT ( 'NONE',  ( 6.166260936116925606, 6.088392601758203071, 0.7998128361456341429 ) ) ;
#39166 = CARTESIAN_POINT ( 'NONE',  ( 3.834746474454188013E-15, 10.81250000000000355, 1.500000000000001554 ) ) ;
#39167 = ORIENTED_EDGE ( 'NONE', *, *, #168889, .F. ) ;
#39168 = AXIS2_PLACEMENT_3D ( 'NONE', #210544, #91493, #124062 ) ;
#39169 = ORIENTED_EDGE ( 'NONE', *, *, #154979, .T. ) ;
#39170 = CARTESIAN_POINT ( 'NONE',  ( 3.598146505595464006, -0.8898571075792599538, 1.577739831003275084 ) ) ;
#39171 = ORIENTED_EDGE ( 'NONE', *, *, #100675, .T. ) ;
#39172 = CARTESIAN_POINT ( 'NONE',  ( 10.07778825365955733, 10.65184113889131012, -0.7998128361456281477 ) ) ;
#39173 = MECHANICAL_DESIGN_GEOMETRIC_PRESENTATION_REPRESENTATION (  '', ( #194849 ), #49514 ) ;
#39174 = CARTESIAN_POINT ( 'NONE',  ( 5.273195401072370281, 5.116759154198018855, -0.7998128361456481317 ) ) ;
#39175 = CARTESIAN_POINT ( 'NONE',  ( 4.230988290566616072, 1.657980831523006460, 0.7301630082575115699 ) ) ;
#39176 = CARTESIAN_POINT ( 'NONE',  ( 6.983858524370772258, 9.241197259889668558, 1.443375672974063439 ) ) ;
#39177 = CARTESIAN_POINT ( 'NONE',  ( 5.228900738148710481, 6.411469580122314049, 1.161126877744517838 ) ) ;
#39179 = CARTESIAN_POINT ( 'NONE',  ( 1.364683531249996529, 14.96354166700806410, 0.7879004041258405033 ) ) ;
#39178 = CARTESIAN_POINT ( 'NONE',  ( 5.424199618621329044, 0.9171840495176122321, 1.619240327305818683 ) ) ;
#39180 = CARTESIAN_POINT ( 'NONE',  ( 3.145994354733801845, 0.8638979756431870438, 1.709836580976647813 ) ) ;
#39181 = CARTESIAN_POINT ( 'NONE',  ( 4.807927017778164114, 8.120258031035326951, 0.8434019511586322571 ) ) ;
#39182 = CARTESIAN_POINT ( 'NONE',  ( -10.57232898948313604, 5.599354254162436817, 4.968808419985093039 ) ) ;
#39183 = CARTESIAN_POINT ( 'NONE',  ( -1.284279953904152949, 3.171639714193937198, 0.7750000000000152323 ) ) ;
#39184 = CARTESIAN_POINT ( 'NONE',  ( 5.653386867218496370, 9.539442411822841805, 1.040834085586084257E-14 ) ) ;
#39185 = CARTESIAN_POINT ( 'NONE',  ( -4.440459003675619520, 5.139289244831666714, 1.199719254218462483 ) ) ;
#39186 = CARTESIAN_POINT ( 'NONE',  ( 1.710996362105126511, -0.2544465352872951613, 2.075019263894110733 ) ) ;
#39187 = CARTESIAN_POINT ( 'NONE',  ( 6.313256805818848960, 7.394496357324014113, 1.199719254218452047 ) ) ;
#39188 = CARTESIAN_POINT ( 'NONE',  ( 6.317406038308035043, -0.2352959436980571473, 1.911917130847824886 ) ) ;
#39189 = CARTESIAN_POINT ( 'NONE',  ( -6.240830780992103755, 6.175390754112560110, 1.040834085586084257E-14 ) ) ;
#39190 = CARTESIAN_POINT ( 'NONE',  ( 2.291784574284541964, -0.7830779901500490858, 1.649245556672715773 ) ) ;
#39191 = CARTESIAN_POINT ( 'NONE',  ( 0.7500000000000006661, 9.947916667349469222, -1.299038105676657340 ) ) ;
#39192 = CARTESIAN_POINT ( 'NONE',  ( 1.627339542692422869, 0.1479755015179542166, -1.964067387968527312 ) ) ;
#39193 = CARTESIAN_POINT ( 'NONE',  ( 3.931145062177692218, -1.341491907185809795, -1.404491712913302104 ) ) ;
#39194 = ORIENTED_EDGE ( 'NONE', *, *, #66840, .F. ) ;
#39196 = CARTESIAN_POINT ( 'NONE',  ( 6.930517489306616596, -1.145039166549733922, 1.467359839328785664 ) ) ;
#39195 = CARTESIAN_POINT ( 'NONE',  ( -4.197131071882288289, 7.054347462908075350, -1.199719254218455378 ) ) ;
#39198 = CARTESIAN_POINT ( 'NONE',  ( 3.709332143218791789, 1.789599998243587731, -1.137392358348317201 ) ) ;
#39197 = CARTESIAN_POINT ( 'NONE',  ( 3.627688620108284745, 6.389997935838436227, 1.199719254218452047 ) ) ;
#39199 = CARTESIAN_POINT ( 'NONE',  ( 6.392587740394325202, -6.532648833121162291, 6.999862025037000279 ) ) ;
#39200 = CARTESIAN_POINT ( 'NONE',  ( 10.07100917685271035, 10.64393221595000938, 0.7998128361456462443 ) ) ;
#39201 = CARTESIAN_POINT ( 'NONE',  ( -6.611536185319534908, 7.742488966741438716, 1.199719254218452047 ) ) ;
#39202 =( NAMED_UNIT ( * ) PLANE_ANGLE_UNIT ( ) SI_UNIT ( $, .RADIAN. ) );
#39203 = ORIENTED_EDGE ( 'NONE', *, *, #190382, .F. ) ;
#39204 = AXIS2_PLACEMENT_3D ( 'NONE', #78254, #124962, #209295 ) ;
#39205 = CARTESIAN_POINT ( 'NONE',  ( 6.200875153403774043, 8.327716660428123419, -1.599625672291283607 ) ) ;
#39206 = CARTESIAN_POINT ( 'NONE',  ( -15.75000000000000000, 10.19999999999999929, -1.100000000000000311 ) ) ;
#39207 = CARTESIAN_POINT ( 'NONE',  ( 3.896943178251357054, 1.541351720387572843, -0.9781566455248569270 ) ) ;
#39208 = CARTESIAN_POINT ( 'NONE',  ( 3.484082288587600384, 7.008587070086744752, -0.7216878364870351614 ) ) ;
#39209 = CARTESIAN_POINT ( 'NONE',  ( -8.175203439360366531, 12.48156174598837787, 1.040834085586084257E-14 ) ) ;
#39210 = CARTESIAN_POINT ( 'NONE',  ( -4.986341270546564175, 8.046800470007955397, 1.126807992560383331 ) ) ;
#39211 = DIRECTION ( 'NONE',  ( 0.000000000000000000, -1.000000000000000000, 0.000000000000000000 ) ) ;
#39212 = CARTESIAN_POINT ( 'NONE',  ( 4.258574955689950592, -1.386304660245713860, 1.256184814050688603 ) ) ;
#39213 = CARTESIAN_POINT ( 'NONE',  ( 9.250740883225924804, 9.686952540052077509, 1.040834085586084257E-14 ) ) ;
#39214 = CARTESIAN_POINT ( 'NONE',  ( 2.104012753913253153, -1.926084867047285654, 0.04718631861246740111 ) ) ;
#39215 = CARTESIAN_POINT ( 'NONE',  ( -0.6385288935052398918, 2.800000000000018474, 1.214618717626907207 ) ) ;
#39216 = CARTESIAN_POINT ( 'NONE',  ( 0.6823417656249934904, 9.005208333674726617, 1.181850606188764807 ) ) ;
#39217 = CARTESIAN_POINT ( 'NONE',  ( -7.088215381846223906, 7.164006121775713609, 0.7998128361456341429 ) ) ;
#39218 = CARTESIAN_POINT ( 'NONE',  ( 4.416205349749311004, 6.175325546172740765, 1.599625672291267398 ) ) ;
#39219 = CARTESIAN_POINT ( 'NONE',  ( -5.167065940139584868, 6.161236697318522637, 1.082531754730549078 ) ) ;
#39220 = VECTOR ( 'NONE', #204091, 1000.000000000000000 ) ;
#39221 = MECHANICAL_DESIGN_GEOMETRIC_PRESENTATION_REPRESENTATION (  '', ( #143015 ), #122191 ) ;
#39222 = CARTESIAN_POINT ( 'NONE',  ( 0.05257324754554763141, -1.379058229334565455, 1.606613856852637356 ) ) ;
#39223 = CARTESIAN_POINT ( 'NONE',  ( 8.367353357928214663, 12.91366268422496688, 1.040834085586084257E-14 ) ) ;
#39224 = CARTESIAN_POINT ( 'NONE',  ( -1.492729907964628788, 4.434594525010058241, 0.1664789471928727893 ) ) ;
#39225 = CARTESIAN_POINT ( 'NONE',  ( 4.750872686184268723, -0.4484009487188305165, -2.020967519627144604 ) ) ;
#39227 = CARTESIAN_POINT ( 'NONE',  ( -0.6823417656250003738, 2.530208333674753618, -1.181850606188749264 ) ) ;
#39226 = CARTESIAN_POINT ( 'NONE',  ( 0.9074547957551477584, -0.8278116715597811925, -1.644758345054016191 ) ) ;
#39228 = CARTESIAN_POINT ( 'NONE',  ( 4.957821946367388932, -2.163970343481158132, -0.7757635736431248707 ) ) ;
#39229 = CARTESIAN_POINT ( 'NONE',  ( 6.860062538834778678, 8.066123052471139587, -1.082531754730543083 ) ) ;
#39231 = CARTESIAN_POINT ( 'NONE',  ( -1.499999999999990896, 4.660416667349485564, -0.8660254037844429265 ) ) ;
#39230 = CARTESIAN_POINT ( 'NONE',  ( 5.085717018901939390, 5.105960408239938353, 0.000000000000000000 ) ) ;
#39232 = CARTESIAN_POINT ( 'NONE',  ( 0.4809653258567511691, -0.2865729554843428062, -2.274222260372929405 ) ) ;
#39233 = CARTESIAN_POINT ( 'NONE',  ( 1.224999999999967004, 0.3958333333333378667, -0.7072540797573017013 ) ) ;
#39234 = CARTESIAN_POINT ( 'NONE',  ( -5.803772275101700906, 8.928762199997411386, -1.199719254218452047 ) ) ;
#39235 = CARTESIAN_POINT ( 'NONE',  ( 4.593657693847520207, -1.941558278569108120, -0.04622955632663238584 ) ) ;
#39236 = ORIENTED_EDGE ( 'NONE', *, *, #49632, .T. ) ;
#39237 = CARTESIAN_POINT ( 'NONE',  ( 8.229436053370669413, 10.62409470039771442, 1.443375672974076540 ) ) ;
#39238 = CIRCLE ( 'NONE', #4566, 0.08000000000000020983 ) ;
#39239 = ORIENTED_EDGE ( 'NONE', *, *, #50950, .T. ) ;
#39240 = CARTESIAN_POINT ( 'NONE',  ( -0.2047996464942871964, -0.1441562275304847374, -1.980932652848297115 ) ) ;
#39241 = CARTESIAN_POINT ( 'NONE',  ( 5.999232488047271161, -0.2420365156972601739, 2.001857322483958423 ) ) ;
#39243 = DIRECTION ( 'NONE',  ( -0.9885327375000381167, 0.000000000000000000, -0.1510067114093955609 ) ) ;
#39242 = CARTESIAN_POINT ( 'NONE',  ( -8.910733272679575379, 11.41894145625809820, -1.599625672291263179 ) ) ;
#39244 = CARTESIAN_POINT ( 'NONE',  ( -3.285556943749998737, -1.217708332855376607, 1.896917185911908499 ) ) ;
#39246 = CARTESIAN_POINT ( 'NONE',  ( 0.8129392405988710157, -0.2653805273100506290, 1.749707594005883937 ) ) ;
#39245 = CARTESIAN_POINT ( 'NONE',  ( 2.748082359423655419, 0.7051493092682534769, 1.968258087557398284 ) ) ;
#39247 = CARTESIAN_POINT ( 'NONE',  ( -1.500000000000008216, 8.281250000682797818, 3.469446951953614189E-15 ) ) ;
#39249 = CARTESIAN_POINT ( 'NONE',  ( 4.699361189290715224, -0.6141998521675575695, 2.208390280175839049 ) ) ;
#39248 = CARTESIAN_POINT ( 'NONE',  ( 0.000000000000000000, 8.500000000000000000, 0.000000000000000000 ) ) ;
#39250 = CARTESIAN_POINT ( 'NONE',  ( 2.026944798790380364, -1.135751832872053058, -1.318713242574782507 ) ) ;
#39251 = CARTESIAN_POINT ( 'NONE',  ( 3.018661757337009810, 6.673522483535157868, 0.000000000000000000 ) ) ;
#39252 = CARTESIAN_POINT ( 'NONE',  ( 6.008198349511364000, 7.038594824965278995, 1.199719254218453823 ) ) ;
#39253 = CARTESIAN_POINT ( 'NONE',  ( 2.196291916443537939, -1.129096229514385819, -1.315908775350557169 ) ) ;
#39254 = CARTESIAN_POINT ( 'NONE',  ( -0.6801582343750282034, 1.963541667008045222, 1.178068619123803451 ) ) ;
#39255 = CARTESIAN_POINT ( 'NONE',  ( 1.979201191301533047, 2.025398335218126622, 0.7825711269493199618 ) ) ;
#39256 = CARTESIAN_POINT ( 'NONE',  ( 5.311043488251262268, 7.219303374425030562, -1.599625672291256295 ) ) ;
#39257 = CARTESIAN_POINT ( 'NONE',  ( 5.137907791644652278, 2.014008302827663854, -0.1037760698975112861 ) ) ;
#39258 = CARTESIAN_POINT ( 'NONE',  ( 2.250000000000001776, 1.285947368876626068E-13, 2.052068128417949389 ) ) ;
#39259 = CARTESIAN_POINT ( 'NONE',  ( -0.7500000000000006661, 2.639583334016156080, -1.299038105676652011 ) ) ;
#39260 = CARTESIAN_POINT ( 'NONE',  ( 1.078981819582014445, -0.04439612541052954248, -1.926037623753373618 ) ) ;
#39261 = CARTESIAN_POINT ( 'NONE',  ( 0.6823417656249934904, 14.69270833367473195, 1.181850606188764807 ) ) ;
#39262 = CARTESIAN_POINT ( 'NONE',  ( 4.676165968894677505, 2.197079021736783044, -0.3272799971512970196 ) ) ;
#39263 = VERTEX_POINT ( 'NONE', #61475 ) ;
#39264 = DIRECTION ( 'NONE',  ( -1.000000000000000000, 7.771561172376096769E-16, 4.440892098500627148E-16 ) ) ;
#39265 = CARTESIAN_POINT ( 'NONE',  ( -0.7500000000000215383, 0.9416666666666878571, 1.299038105676659116 ) ) ;
#39266 = CARTESIAN_POINT ( 'NONE',  ( 8.260995669428309540, 8.532249790621511565, 0.7998128361456481317 ) ) ;
#39267 = CARTESIAN_POINT ( 'NONE',  ( -1.364683531250014514, -0.4697916663252449943, 0.7879004041258379498 ) ) ;
#39268 = EDGE_CURVE ( 'NONE', #140877, #59046, #165429, .T. ) ;
#39269 = CARTESIAN_POINT ( 'NONE',  ( 0.1709645942036420174, 0.8561845417300646410, 2.049862257243968422 ) ) ;
#39270 = CARTESIAN_POINT ( 'NONE',  ( 5.301206097546149465, -1.683542251207278628, 1.007010407901312465 ) ) ;
#39271 = CARTESIAN_POINT ( 'NONE',  ( 9.734391104931955141, 10.45913716528321125, 0.7216878364870438212 ) ) ;
#39272 = EDGE_CURVE ( 'NONE', #73634, #37563, #74535, .T. ) ;
#39273 = CARTESIAN_POINT ( 'NONE',  ( 0.6323695665565836066, 1.111747700424435159, -1.853661729306683936 ) ) ;
#39274 = CARTESIAN_POINT ( 'NONE',  ( -4.502716413514310290, 6.346531463890372926, -1.443375672974066548 ) ) ;
#39275 = CARTESIAN_POINT ( 'NONE',  ( 3.420431513525914902, 0.9250737872015384333, 1.843656989716379035 ) ) ;
#39276 = CARTESIAN_POINT ( 'NONE',  ( -5.473741331615264549, 7.409117525016355010, -1.599625672291256295 ) ) ;
#39277 = CARTESIAN_POINT ( 'NONE',  ( 1.499999999999989120, 2.535416667349483344, 0.8660254037844524744 ) ) ;
#39278 = CARTESIAN_POINT ( 'NONE',  ( -0.6823417656249969321, 5.530208333674756283, -1.181850606188749264 ) ) ;
#39279 = CARTESIAN_POINT ( 'NONE',  ( 4.674985431947434655, 0.001863223488791227334, -1.870726058175266715 ) ) ;
#39280 = CARTESIAN_POINT ( 'NONE',  ( 3.709331991548686425, 1.648016779243220320, 0.5399856063554776542 ) ) ;
#39281 = CARTESIAN_POINT ( 'NONE',  ( 3.438731153704393417, -1.320290108414169605, -1.134124902983554062 ) ) ;
#39282 = CARTESIAN_POINT ( 'NONE',  ( 0.9785521075769167965, -2.238008663356937156, -0.4956820494700850399 ) ) ;
#39283 = CARTESIAN_POINT ( 'NONE',  ( -0.6823417656250212460, 4.613541667008086655, 1.181850606188767472 ) ) ;
#39285 = CARTESIAN_POINT ( 'NONE',  ( 4.247661304151585604, 2.090252499381782147, -0.05307422152340918187 ) ) ;
#39284 = B_SPLINE_CURVE_WITH_KNOTS ( 'NONE', 3,
 ( #130056, #178737, #196050, #96436, #145200, #209062, #60699, #47682, #176597, #211206 ),
 .UNSPECIFIED., .F., .F.,
 ( 4, 2, 2, 2, 4 ),
 ( 0.0001025101613542923196, 0.0005630481886794980444, 0.001023586216004703647, 0.001484124243329909250, 0.001944662270655115070 ),
 .UNSPECIFIED. ) ;
#39286 = CARTESIAN_POINT ( 'NONE',  ( 6.333930032320489900, 1.921166581771537318, 0.2825802787540276917 ) ) ;
#39288 = VERTEX_POINT ( 'NONE', #45247 ) ;
#39287 = CARTESIAN_POINT ( 'NONE',  ( 8.398252340528729931, 15.16388421002588593, 8.572949304411110916 ) ) ;
#39289 = CARTESIAN_POINT ( 'NONE',  ( 0.7389079861009685279, 2.013985778099684154, -0.1017531103126300962 ) ) ;
#39290 = CARTESIAN_POINT ( 'NONE',  ( 0.6508261300204335464, 2.090236094481153550, 0.3566229023672163878 ) ) ;
#39291 =( LENGTH_UNIT ( ) NAMED_UNIT ( * ) SI_UNIT ( .MILLI., .METRE. ) );
#39292 = CARTESIAN_POINT ( 'NONE',  ( -11.41267819554183127, 4.000000000000003553, 3.708203932499423150 ) ) ;
#39293 = CARTESIAN_POINT ( 'NONE',  ( -7.340850106795412167, 10.65174332698158643, 1.199719254218453823 ) ) ;
#39294 =( BOUNDED_CURVE ( )  B_SPLINE_CURVE ( 3, ( #155075, #38123, #187558, #22905 ),
 .UNSPECIFIED., .F., .T. ) 
 B_SPLINE_CURVE_WITH_KNOTS ( ( 4, 4 ),
 ( 4.683789229004537091, 4.706575325518645769 ),
 .UNSPECIFIED. ) 
 CURVE ( )  GEOMETRIC_REPRESENTATION_ITEM ( )  RATIONAL_B_SPLINE_CURVE ( ( 1.000000000000000000, 0.9999567332851475587, 0.9999567332851475587, 1.000000000000000000 ) ) 
 REPRESENTATION_ITEM ( '' )  );
#39295 = CARTESIAN_POINT ( 'NONE',  ( 5.147291874682557555, 9.156924287104992288, 0.7998128361456462443 ) ) ;
#39296 = CARTESIAN_POINT ( 'NONE',  ( 2.420699464796825850, -0.8139657014685426351, -1.958238820914718792 ) ) ;
#39297 = FILL_AREA_STYLE_COLOUR ( '', #167127 ) ;
#39298 = CARTESIAN_POINT ( 'NONE',  ( 4.178209475066913647, -1.049361115903378883, 1.493786327181771068 ) ) ;
#39299 = ORIENTED_EDGE ( 'NONE', *, *, #29742, .F. ) ;
#39300 = CARTESIAN_POINT ( 'NONE',  ( -4.380693030546956912, 6.204170850428461392, 1.443375672974065660 ) ) ;
#39301 = CARTESIAN_POINT ( 'NONE',  ( 1.972527975918452161E-16, -7.473374494045017968, -9.500331257164628340 ) ) ;
#39302 = CARTESIAN_POINT ( 'NONE',  ( 3.475000000000000533, -3.981249999044082610, 0.000000000000000000 ) ) ;
#39303 = CARTESIAN_POINT ( 'NONE',  ( -5.994676475536691029, 10.14553965476814845, 0.7998128361456481317 ) ) ;
#39304 = CARTESIAN_POINT ( 'NONE',  ( 1.810812951734928511, -0.5429070200502202903, -1.945354291398709412 ) ) ;
#39305 = CARTESIAN_POINT ( 'NONE',  ( 5.491335294905154818, 1.948586811899848614, -1.035780281143129811 ) ) ;
#39306 = CARTESIAN_POINT ( 'NONE',  ( -5.984998465789844069, 5.947196063035064206, 0.7998128361456281477 ) ) ;
#39307 = CARTESIAN_POINT ( 'NONE',  ( 3.256551146222384396, -0.5358571751262303229, -1.782154170384263603 ) ) ;
#39308 = CARTESIAN_POINT ( 'NONE',  ( 3.379006598303866848, 4.965260336153046516, -1.599625672291262513 ) ) ;
#39309 = CARTESIAN_POINT ( 'NONE',  ( 0.000000000000000000, 9.999999999999998224, 0.000000000000000000 ) ) ;
#39310 = ORIENTED_EDGE ( 'NONE', *, *, #12006, .F. ) ;
#39311 = CARTESIAN_POINT ( 'NONE',  ( -5.199715606040888005, 6.025088614257851027, -1.199719254218446718 ) ) ;
#39312 = AXIS2_PLACEMENT_3D ( 'NONE', #20649, #3327, #201527 ) ;
#39313 = CARTESIAN_POINT ( 'NONE',  ( -7.648771216403934758, 12.07531685244661723, -0.7998128361456291469 ) ) ;
#39314 = CARTESIAN_POINT ( 'NONE',  ( 4.828627627824715773, 1.747987318788373656, 0.5269492854979712648 ) ) ;
#39316 = CARTESIAN_POINT ( 'NONE',  ( -4.127707017443506210, 7.650024674618332021, -0.8198546088712642677 ) ) ;
#39315 = CARTESIAN_POINT ( 'NONE',  ( -3.383641855062333281, 6.105276709951447778, -1.199719254218452047 ) ) ;
#39317 = CARTESIAN_POINT ( 'NONE',  ( 5.348589505275513467, 7.707351500233518671, -1.315919829448284784 ) ) ;
#39318 = CARTESIAN_POINT ( 'NONE',  ( 1.088703816646944267, 1.038853075768126910, -1.387971508864824788 ) ) ;
#39319 = CARTESIAN_POINT ( 'NONE',  ( 6.421814705521882161, 1.055779539018763646, -1.508159643570324393 ) ) ;
#39320 = CARTESIAN_POINT ( 'NONE',  ( 5.444061505814771884, 0.9398705156117830306, -2.107803560374045038 ) ) ;
#39321 = CARTESIAN_POINT ( 'NONE',  ( 3.691562964670865199, 7.528850235416478576, -0.7998128361456362523 ) ) ;
#39322 = CARTESIAN_POINT ( 'NONE',  ( 6.925078400183550364, -0.007619068086212391067, 2.144148427808051594 ) ) ;
#39323 = CARTESIAN_POINT ( 'NONE',  ( 4.984594031318565932, 8.967110136513669616, 0.7998128361456462443 ) ) ;
#39324 = CARTESIAN_POINT ( 'NONE',  ( 5.923294579110739200, 0.9235710928677911546, 2.104827929701275302 ) ) ;
#39325 = CARTESIAN_POINT ( 'NONE',  ( -9.499668754385629299, -7.215597533182398493, -0.07933194154558173561 ) ) ;
#39326 = CARTESIAN_POINT ( 'NONE',  ( -6.882699257592852504, 8.058845884393651460, -1.199719254218452047 ) ) ;
#39327 = VECTOR ( 'NONE', #62489, 1000.000000000000000 ) ;
#39328 = CARTESIAN_POINT ( 'NONE',  ( 5.946149726614579301, 1.868617323842229894, 0.09011704611043556967 ) ) ;
#39330 = CARTESIAN_POINT ( 'NONE',  ( -4.472210567661380587, 6.310941310395290493, 1.599625672291270506 ) ) ;
#39329 = CARTESIAN_POINT ( 'NONE',  ( 3.023589307540079041, -0.3687504995396119201, 1.876329818327879817 ) ) ;
#39331 = CARTESIAN_POINT ( 'NONE',  ( 5.039771180630152614, -1.558841386063321455, -1.562417271110942307 ) ) ;
#39332 = CARTESIAN_POINT ( 'NONE',  ( 4.223895228407223534, 0.9020499113536835090, -1.915681561053275139 ) ) ;
#39333 = CARTESIAN_POINT ( 'NONE',  ( 1.224999999999976108, 1.187500000682802037, -3.469446951953614189E-14 ) ) ;
#39334 = CARTESIAN_POINT ( 'NONE',  ( 6.883263157960399781, 2.038134514454426505, 2.350812138539408735 ) ) ;
#39335 = CARTESIAN_POINT ( 'NONE',  ( 3.228249973385329596, 6.780392379009261283, -1.734723475976807094E-15 ) ) ;
#39336 = CARTESIAN_POINT ( 'NONE',  ( -4.950135482320926705, 6.868520377498098739, -1.443375672974066548 ) ) ;
#39337 = CARTESIAN_POINT ( 'NONE',  ( 6.164709077089638001, 0.6648188651474650213, 2.013622499735030491 ) ) ;
#39338 = CARTESIAN_POINT ( 'NONE',  ( 1.852963337694241819, 0.7249817717532834882, 2.190821962643316301 ) ) ;
#39340 = EDGE_CURVE ( 'NONE', #169237, #136644, #16682, .T. ) ;
#39339 = CARTESIAN_POINT ( 'NONE',  ( 3.894932841003693191, 0.2855096342280309396, 1.940843471192068570 ) ) ;
#39341 = CARTESIAN_POINT ( 'NONE',  ( -5.798046968499580345, 6.793418213784815585, 1.199719254218452935 ) ) ;
#39342 = CARTESIAN_POINT ( 'NONE',  ( 0.2331563151865486683, 0.005903526429595904942, -1.945944850731482934 ) ) ;
#39343 = CARTESIAN_POINT ( 'NONE',  ( 9.348381460497192208, 13.52536904890506797, 7.450314784081282227 ) ) ;
#39344 = CARTESIAN_POINT ( 'NONE',  ( 5.011674058906918638, 5.875983152593414971, 1.199719254218452047 ) ) ;
#39345 = ORIENTED_EDGE ( 'NONE', *, *, #135974, .T. ) ;
#39346 = CARTESIAN_POINT ( 'NONE',  ( 5.577361344084559747, 1.530155114678043660, 1.313547687611632764 ) ) ;
#39347 = CARTESIAN_POINT ( 'NONE',  ( 0.05820987927622478519, -1.643049995186950829, -0.8308948761173093889 ) ) ;
#39348 = CARTESIAN_POINT ( 'NONE',  ( -10.71030397718323890, 6.055815897892919075, -4.668189396100475008 ) ) ;
#39349 = CARTESIAN_POINT ( 'NONE',  ( 3.116274269780743733, 2.161009848182334991, -0.2084346501036362376 ) ) ;
#39350 = CARTESIAN_POINT ( 'NONE',  ( 5.041653019435334393, 6.975290837464928728, -1.599625672291269396 ) ) ;
#39351 = CARTESIAN_POINT ( 'NONE',  ( 0.9144942500491148873, -2.120778211678171488, 0.005759991200282587286 ) ) ;
#39352 = CARTESIAN_POINT ( 'NONE',  ( 0.7499999999999885647, 2.347916667349486453, -1.299038105676652899 ) ) ;
#39353 = CARTESIAN_POINT ( 'NONE',  ( -4.930951480464074166E-10, 14.48154074412735426, -12.00000000000003553 ) ) ;
#39354 = CARTESIAN_POINT ( 'NONE',  ( -3.189213936345698830, 2.817530495244580102, 2.450448857954578230 ) ) ;
#39355 = CARTESIAN_POINT ( 'NONE',  ( 5.141188686642438554, 7.897460914975725998, 1.230089993873971999 ) ) ;
#39356 = CARTESIAN_POINT ( 'NONE',  ( 0.7552377862659557239, -1.739527406477459515, -1.104632168941059867 ) ) ;
#39358 = CARTESIAN_POINT ( 'NONE',  ( -3.294945724223601768, 7.655198976062505878, -2.499999999999995115 ) ) ;
#39357 = CARTESIAN_POINT ( 'NONE',  ( -9.022061154889962964, 12.61315621642528129, -1.199719254218446718 ) ) ;
#39359 = CARTESIAN_POINT ( 'NONE',  ( 0.6823417656249899377, 1.342708333674752508, 1.181850606188755259 ) ) ;
#39360 = DIRECTION ( 'NONE',  ( -0.9667253911244640951, 0.2558163758543454125, 0.000000000000000000 ) ) ;
#39361 = ADVANCED_FACE ( 'NONE', ( #109239 ), #87182, .T. ) ;
#39362 = ORIENTED_EDGE ( 'NONE', *, *, #212165, .F. ) ;
#39363 = CARTESIAN_POINT ( 'NONE',  ( 2.912652942483742180, -0.5572119909246497915, -1.829279355302193544 ) ) ;
#39364 = CARTESIAN_POINT ( 'NONE',  ( 5.629715507205930614, -1.125428185119830005, -1.365942169508828741 ) ) ;
#39365 = CARTESIAN_POINT ( 'NONE',  ( 7.049313524462606395, 7.188896964819984525, 0.000000000000000000 ) ) ;
#39366 = CARTESIAN_POINT ( 'NONE',  ( -4.090809663021341969, 5.795697244990093644, 1.599625672291267398 ) ) ;
#39367 = CARTESIAN_POINT ( 'NONE',  ( 0.4745106373920011666, -1.311730567922615665, 1.249698552857400946 ) ) ;
#39369 = CARTESIAN_POINT ( 'NONE',  ( 0.4619447194890722308, -1.061692323622511536, 1.594387217869216888 ) ) ;
#39368 = CARTESIAN_POINT ( 'NONE',  ( 7.591565991045856165, -6.646943093534003033, 7.792125355486806626 ) ) ;
#39370 = CARTESIAN_POINT ( 'NONE',  ( 2.330607996690749140, -1.275545549462468120, 1.630658604070814199 ) ) ;
#39371 = CARTESIAN_POINT ( 'NONE',  ( 0.6823417656249882723, 0.7385416670080829915, -1.181850606188749264 ) ) ;
#39372 = CARTESIAN_POINT ( 'NONE',  ( 6.315307248462690204, -0.2269180964024133385, 1.856785020699961875 ) ) ;
#39373 = CARTESIAN_POINT ( 'NONE',  ( 2.349991895876184511, 1.825291697999480434, 0.04531359951509549705 ) ) ;
#39375 = CARTESIAN_POINT ( 'NONE',  ( 6.233692552841108458, 6.917895963632635592, 0.8214459722771473293 ) ) ;
#39374 = CARTESIAN_POINT ( 'NONE',  ( 6.568967528192747096, -2.015767819289843388, -0.8987472251835016968 ) ) ;
#39376 = CARTESIAN_POINT ( 'NONE',  ( -1.402160292154681736E-14, 0.6968750003414164729, -1.575800808251659024 ) ) ;
#39377 = CARTESIAN_POINT ( 'NONE',  ( 4.070800801938780467, 1.460776800910084994, -1.456535598646004237 ) ) ;
#39379 = CARTESIAN_POINT ( 'NONE',  ( -7.283754839039664475, 9.520799950344851936, -1.599625672291263179 ) ) ;
#39378 = CIRCLE ( 'NONE', #160438, 0.6500000000000000222 ) ;
#39380 = CARTESIAN_POINT ( 'NONE',  ( 9.511208455186636712, 11.05516360492796935, 1.199719254218453823 ) ) ;
#39381 = DIRECTION ( 'NONE',  ( -1.000000000000000000, 0.000000000000000000, 0.000000000000000000 ) ) ;
#39382 = CARTESIAN_POINT ( 'NONE',  ( 0.8081717762262634608, -2.151237856378166224, 0.2110218573620133986 ) ) ;
#39383 = CARTESIAN_POINT ( 'NONE',  ( 6.672334155782003506, -0.9722939650993901450, -1.827837255792996718 ) ) ;
#39384 = CARTESIAN_POINT ( 'NONE',  ( -1.201851678989727383E-14, 0.8843750003414173610, 1.575800808251672791 ) ) ;
#39385 = CARTESIAN_POINT ( 'NONE',  ( 3.919328646192806520, -0.1633067429045453600, 2.155504054270485970 ) ) ;
#39387 = ADVANCED_FACE ( 'NONE', ( #26835 ), #92938, .T. ) ;
#39386 = CARTESIAN_POINT ( 'NONE',  ( 3.774085898144818874, 2.004173781823472833, -0.2492677732841129534 ) ) ;
#39388 = CARTESIAN_POINT ( 'NONE',  ( 0.000000000000000000, 3.079999999999999183, 0.000000000000000000 ) ) ;
#39389 = EDGE_CURVE ( 'NONE', #84082, #7772, #172355, .T. ) ;
#39392 = CARTESIAN_POINT ( 'NONE',  ( 6.805829924380114804, 8.002851668940699881, 1.082531754730558626 ) ) ;
#39391 = CARTESIAN_POINT ( 'NONE',  ( -3.475000000000000533, -0.02916666666666653876, -2.006292185433948827 ) ) ;
#39390 = FACE_OUTER_BOUND ( 'NONE', #145990, .T. ) ;
#39393 = CARTESIAN_POINT ( 'NONE',  ( -5.986807348886189040, 9.142303119412650503, -1.199719254218452047 ) ) ;
#39394 = CARTESIAN_POINT ( 'NONE',  ( 2.729704159269104924, 0.7212915320151757070, -1.883313052590728454 ) ) ;
#39395 = CARTESIAN_POINT ( 'NONE',  ( -7.335124800193271177, 8.516399340768996851, -1.199719254218452935 ) ) ;
#39397 = CARTESIAN_POINT ( 'NONE',  ( -4.858757509019083543, 5.629766575900002401, -2.420000000000000373 ) ) ;
#39396 = CARTESIAN_POINT ( 'NONE',  ( -4.090809663021341969, 5.795697244990093644, 1.599625672291267398 ) ) ;
#39398 = FACE_OUTER_BOUND ( 'NONE', #83528, .T. ) ;
#39399 = CARTESIAN_POINT ( 'NONE',  ( 5.256085721135645095, 0.7693902824621422498, -1.750971482026221437 ) ) ;
#39401 = CARTESIAN_POINT ( 'NONE',  ( -2.428882075142555497, 5.985446187641602300, 1.040834085586084257E-14 ) ) ;
#39400 = B_SPLINE_CURVE_WITH_KNOTS ( 'NONE', 3,
 ( #171032, #204576, #122387, #89817, #200318, #51969 ),
 .UNSPECIFIED., .F., .F.,
 ( 4, 2, 4 ),
 ( 0.000000000000000000, 0.0002835903134653135075, 0.0005671806269306270149 ),
 .UNSPECIFIED. ) ;
#39402 = CARTESIAN_POINT ( 'NONE',  ( 6.277061933002788585, 6.425586464699131639, 0.7216878364870317197 ) ) ;
#39404 = CARTESIAN_POINT ( 'NONE',  ( 4.851185501729457172, 0.1948232160459452411, -2.006962824030594561 ) ) ;
#39403 = CARTESIAN_POINT ( 'NONE',  ( -7.144783764277399030, 11.27940545839156528, 0.7216878364870458196 ) ) ;
#39405 = CARTESIAN_POINT ( 'NONE',  ( -1.201851678989727383E-14, 4.337500000000023448, -1.732050807568863648 ) ) ;
#39406 = CARTESIAN_POINT ( 'NONE',  ( 1.364683531250000303, 15.06770833367473017, -0.7879004041258355073 ) ) ;
#39407 = CARTESIAN_POINT ( 'NONE',  ( 6.141572722362285575, -1.252861708448499201, -1.185644778512841002 ) ) ;
#39408 = CARTESIAN_POINT ( 'NONE',  ( 4.362691568547328202, 8.311833606605697256, -0.7998128361456381397 ) ) ;
#39409 = CARTESIAN_POINT ( 'NONE',  ( 8.053180056837369705, 11.37883191874353805, -1.082531754730543083 ) ) ;
#39410 = CARTESIAN_POINT ( 'NONE',  ( 4.973830807571049561, 1.075732564348480746, 1.530087412091485799 ) ) ;
#39411 = CARTESIAN_POINT ( 'NONE',  ( -4.036671995544492297, 7.285761072467114019, 0.7944190476826870073 ) ) ;
#39412 = CARTESIAN_POINT ( 'NONE',  ( 2.342711862795249012, -2.029470198211943632, -0.4080651701656515251 ) ) ;
#39413 = CARTESIAN_POINT ( 'NONE',  ( 0.4019237886466847653, 12.35491455036742892, 1.499999999999997113 ) ) ;
#39414 = ORIENTED_EDGE ( 'NONE', *, *, #19442, .F. ) ;
#39415 = CARTESIAN_POINT ( 'NONE',  ( 3.902768115887398803, 5.646591783325653147, -1.599625672291269396 ) ) ;
#39416 = CARTESIAN_POINT ( 'NONE',  ( 0.6675924852559200762, 1.356316336250670496, 1.492241973137248934 ) ) ;
#39417 = CARTESIAN_POINT ( 'NONE',  ( 1.248006495514828895, 0.8912474588982389756, -1.577060073313638622 ) ) ;
#39418 = CARTESIAN_POINT ( 'NONE',  ( 5.085717018457579286, 6.066329622022862189, -1.082531754730548412 ) ) ;
#39419 = DIRECTION ( 'NONE',  ( 0.6507913734559627184, -0.7592566023653016805, 0.000000000000000000 ) ) ;
#39420 = CARTESIAN_POINT ( 'NONE',  ( 8.893785580440313865, 9.478430720042945623, 1.040834085586084257E-14 ) ) ;
#39421 = CARTESIAN_POINT ( 'NONE',  ( 8.263858322729371153, 9.599921783727809910, -1.199719254218446718 ) ) ;
#39423 = CARTESIAN_POINT ( 'NONE',  ( 5.589432567506730010, -0.4607417488133085381, 1.859251224981002482 ) ) ;
#39422 = CARTESIAN_POINT ( 'NONE',  ( -4.720210035852093533, 8.658662141802762946, -0.7998128361456281477 ) ) ;
#39424 = CARTESIAN_POINT ( 'NONE',  ( -3.673896439623302257, 4.156855427197417185, -0.9999999999999991118 ) ) ;
#39425 = DIRECTION ( 'NONE',  ( 0.000000000000000000, 0.000000000000000000, 1.000000000000000000 ) ) ;
#39426 = CARTESIAN_POINT ( 'NONE',  ( 6.033015167956792268, 8.061603667414825480, -1.443375672974057666 ) ) ;
#39427 = CARTESIAN_POINT ( 'NONE',  ( 1.364683531249986537, -0.5739583329919174526, 0.7879004041258500513 ) ) ;
#39429 = ORIENTED_EDGE ( 'NONE', *, *, #82785, .F. ) ;
#39428 = CARTESIAN_POINT ( 'NONE',  ( 3.050221373394638835, 6.502416002361635528, 0.000000000000000000 ) ) ;
#39430 = CARTESIAN_POINT ( 'NONE',  ( -7.537970219518083326, 9.817384560903001045, -1.443375672974059665 ) ) ;
#39431 = CARTESIAN_POINT ( 'NONE',  ( 3.098656953246520906, -0.6260995091542167490, -2.069055637940686143 ) ) ;
#39432 = CARTESIAN_POINT ( 'NONE',  ( -5.804299160426224624, 9.785783097223662352, -0.7216878364870338292 ) ) ;
#39433 = CARTESIAN_POINT ( 'NONE',  ( 6.699137298928153683, 7.948653282571920720, 1.082531754730549967 ) ) ;
#39434 = CARTESIAN_POINT ( 'NONE',  ( 1.002369745560643510, -0.9483682245385971488, 1.896766750748935415 ) ) ;
#39435 = CARTESIAN_POINT ( 'NONE',  ( 6.299803673773761936, -0.6120917497752301761, 1.720027978493202436 ) ) ;
#39436 = CARTESIAN_POINT ( 'NONE',  ( 2.354701247847644119, -1.526412939949482128, 1.247560610424301109 ) ) ;
#39437 = VERTEX_POINT ( 'NONE', #161117 ) ;
#39438 = CARTESIAN_POINT ( 'NONE',  ( -7.817327168174091234, 14.48014722064626802, -9.115250753896237512 ) ) ;
#39439 = CARTESIAN_POINT ( 'NONE',  ( 4.422284282497963126, 0.9263432559908044706, 1.738082477136545956 ) ) ;
#39440 = CARTESIAN_POINT ( 'NONE',  ( 0.5154417807694658960, -1.038215432012145056, -1.640949389817857984 ) ) ;
#39441 = ORIENTED_EDGE ( 'NONE', *, *, #131051, .F. ) ;
#39442 = CARTESIAN_POINT ( 'NONE',  ( -5.611095471209320174, 7.639640364534566075, 1.599625672291263179 ) ) ;
#39444 = CARTESIAN_POINT ( 'NONE',  ( 1.500000000000007105, 10.64264068711930733, 1.214306433183764966E-14 ) ) ;
#39443 = CARTESIAN_POINT ( 'NONE',  ( -4.659162064951642535, 5.464719159645540003, 1.199719254218452935 ) ) ;
#39446 = CARTESIAN_POINT ( 'NONE',  ( 5.790741006368192778, 8.809596036521288198, -1.082531754730548412 ) ) ;
#39445 = CARTESIAN_POINT ( 'NONE',  ( 7.609150525767641504, 9.900428251527500834, -1.599625672291262513 ) ) ;
#39448 = EDGE_LOOP ( 'NONE', ( #27454, #140514, #80589, #48999, #161355 ) ) ;
#39447 = CARTESIAN_POINT ( 'NONE',  ( 5.285773936917006921, 1.841837585529454202, -0.5139651673399318055 ) ) ;
#39449 = CARTESIAN_POINT ( 'NONE',  ( 1.184930176456780337, -2.153272645635353033, -0.4822455307981614592 ) ) ;
#39450 = CARTESIAN_POINT ( 'NONE',  ( 7.808923410443484592, -5.575271019048062549, 7.747753938335146806 ) ) ;
#39451 = CARTESIAN_POINT ( 'NONE',  ( -0.05814382529654647802, -1.176414490726215734, -1.508152472379259867 ) ) ;
#39452 = CARTESIAN_POINT ( 'NONE',  ( 0.07661050522433666965, 0.7707917844542893082, -1.796988219766264550 ) ) ;
#39453 = CARTESIAN_POINT ( 'NONE',  ( -5.623011108385752799, 7.471940032223963968, 1.349922804658145292 ) ) ;
#39454 = DIRECTION ( 'NONE',  ( 0.000000000000000000, 1.000000000000000000, 0.000000000000000000 ) ) ;
#39455 = CARTESIAN_POINT ( 'NONE',  ( 2.805202726412972414, -1.722705984639979482, 1.148039668612794051 ) ) ;
#39456 = CARTESIAN_POINT ( 'NONE',  ( -6.226218857173722476, 8.287007971501239467, 1.599625672291283607 ) ) ;
#39457 = EDGE_CURVE ( 'NONE', #37010, #148901, #206648, .T. ) ;
#39458 = CARTESIAN_POINT ( 'NONE',  ( -4.969355510774519757, 7.965585441469681172, -1.036248007939699178 ) ) ;
#39460 = CARTESIAN_POINT ( 'NONE',  ( 1.059701713109785670, 0.4209238396889224965, -2.120155868012041811 ) ) ;
#39459 = CARTESIAN_POINT ( 'NONE',  ( -4.608882153641705059, 7.464447381635583412, -1.199719254218452047 ) ) ;
#39461 = DIRECTION ( 'NONE',  ( -0.000000000000000000, 1.000000000000000000, 0.000000000000000000 ) ) ;
#39462 = CARTESIAN_POINT ( 'NONE',  ( 5.573810548993915148, 5.675402860013913475, 0.000000000000000000 ) ) ;
#39463 = CARTESIAN_POINT ( 'NONE',  ( 7.720982897393566802, -6.134628647623485698, -7.834948825496929281 ) ) ;
#39464 = CARTESIAN_POINT ( 'NONE',  ( 1.364683531249997417, 12.79687500034139980, 2.602085213965210642E-15 ) ) ;
#39466 = CARTESIAN_POINT ( 'NONE',  ( -6.981522756394290319, 7.109807735406931783, 0.7998128361456341429 ) ) ;
#39465 = CARTESIAN_POINT ( 'NONE',  ( 6.825078400183572036, 4.699117039843025090, 2.418333817060664526 ) ) ;
#39467 = CARTESIAN_POINT ( 'NONE',  ( 4.992643705478089444, -1.725105917503889641, 0.1769386724924902066 ) ) ;
#39468 = CARTESIAN_POINT ( 'NONE',  ( -5.088387723830502196, 4.830873854090670605, -0.7998128361456221525 ) ) ;
#39469 = CARTESIAN_POINT ( 'NONE',  ( 2.905202624773518316, -1.723727875341171778, 1.146311801414557241 ) ) ;
#39470 = CARTESIAN_POINT ( 'NONE',  ( 4.763340612834221943, 1.975027209670917161, -0.7632558447715469541 ) ) ;
#39471 = CARTESIAN_POINT ( 'NONE',  ( 7.019370843573166319, 9.212351955633947043, 1.599625672291281386 ) ) ;
#39472 = CARTESIAN_POINT ( 'NONE',  ( -0.6823417656249969321, 3.717708333674754506, -1.181850606188749264 ) ) ;
#39473 = CARTESIAN_POINT ( 'NONE',  ( 1.463649477047322733, -0.4837646206634453883, 1.908952741056660685 ) ) ;
#39474 = CARTESIAN_POINT ( 'NONE',  ( 5.756168354352870331, 6.246635012430203027, 1.018728318139457523 ) ) ;
#39475 = CARTESIAN_POINT ( 'NONE',  ( 0.1758378621803426134, 1.891278220088285833, -0.2826890867150752551 ) ) ;
#39476 = CARTESIAN_POINT ( 'NONE',  ( 4.541174964560028116, -1.770302748489580358, -1.456204954804733998 ) ) ;
#39477 = CARTESIAN_POINT ( 'NONE',  ( 2.226930044512597906, -0.0006860120723567450030, 1.825872481329051444 ) ) ;
#39478 = CARTESIAN_POINT ( 'NONE',  ( 4.258142763143749399, 7.125527769379820242, 1.199719254218451159 ) ) ;
#39479 = CARTESIAN_POINT ( 'NONE',  ( 5.951666246274803562, 7.006327377817825663, 1.082531754730558626 ) ) ;
#39480 = CARTESIAN_POINT ( 'NONE',  ( -7.182068686937172153, 9.402166106225269715, 1.599625672291283607 ) ) ;
#39481 = ADVANCED_FACE ( 'NONE', ( #108165 ), #14836, .F. ) ;
#39482 = CARTESIAN_POINT ( 'NONE',  ( 3.357684704777043283, -1.527344908821237635, -1.311707263431096671 ) ) ;
#39483 = CARTESIAN_POINT ( 'NONE',  ( 2.905073028004667712, -1.633678134795817360, 1.085783093053994453 ) ) ;
#39484 = CARTESIAN_POINT ( 'NONE',  ( -8.565000355531095622, 11.01558638625153286, -1.599625672291263179 ) ) ;
#39485 = CARTESIAN_POINT ( 'NONE',  ( -6.250472511100020334, 7.250971670160158311, 1.199719254218450271 ) ) ;
#39486 = LINE ( 'NONE', #206247, #199362 ) ;
#39488 = CARTESIAN_POINT ( 'NONE',  ( 4.944116541256327935, 1.765280609655010879, 0.1280878748119110566 ) ) ;
#39487 = CARTESIAN_POINT ( 'NONE',  ( 5.665992906516797767, -1.327130266483244059, 1.615391119202228332 ) ) ;
#39489 = CARTESIAN_POINT ( 'NONE',  ( 4.903883154387664867, 4.836367890058183683, 0.6143738762558150768 ) ) ;
#39490 = CARTESIAN_POINT ( 'NONE',  ( 0.2170718473699268514, -0.1031819972749977166, 2.189145592210713698 ) ) ;
#39491 = CARTESIAN_POINT ( 'NONE',  ( 5.947135546971048292, 0.4987507408355364991, -1.667328318302605528 ) ) ;
#39492 = ADVANCED_FACE ( 'NONE', ( #32176 ), #114562, .F. ) ;
#39493 = CARTESIAN_POINT ( 'NONE',  ( 7.242026607993941489, 11.60078147596829901, 0.7998128361456462443 ) ) ;
#39494 = CARTESIAN_POINT ( 'NONE',  ( -5.275531169048911728, 6.287779464379406491, -1.082531754730549967 ) ) ;
#39495 = CARTESIAN_POINT ( 'NONE',  ( 6.363951117287210302, -0.1083456013219602776, -2.296273276487709847 ) ) ;
#39496 = CARTESIAN_POINT ( 'NONE',  ( 0.000000000000000000, 13.87999999999998302, 0.000000000000000000 ) ) ;
#39497 = CARTESIAN_POINT ( 'NONE',  ( 5.606719662199564524, 0.7002562906495370942, -1.586348028144116462 ) ) ;
#39498 = CARTESIAN_POINT ( 'NONE',  ( 2.104404934925046877, -2.206339196854599116, 0.05594281105186085790 ) ) ;
#39499 = CARTESIAN_POINT ( 'NONE',  ( 6.285609470618021888, -2.046568710056245965, 0.7253697862827021003 ) ) ;
#39500 = DIRECTION ( 'NONE',  ( -0.7431448254774005724, 0.000000000000000000, -0.6691306063588511321 ) ) ;
#39501 = CARTESIAN_POINT ( 'NONE',  ( 1.182980447155062453, 1.727502145113229970, -1.224025170244628757 ) ) ;
#39502 = CARTESIAN_POINT ( 'NONE',  ( 3.843750000000002220, 1.895863743164162063, 0.7852924748297951396 ) ) ;
#39503 = CARTESIAN_POINT ( 'NONE',  ( 6.727182134110202938, 2.016807574165893513, 2.492494991173601182 ) ) ;
#39504 = CARTESIAN_POINT ( 'NONE',  ( 4.629859910813647339, -1.184627732843917647, -1.519026826222178661 ) ) ;
#39505 = CARTESIAN_POINT ( 'NONE',  ( 1.664984172775041182, 0.7006824767318786673, 2.107951039278654015 ) ) ;
#39506 = ORIENTED_EDGE ( 'NONE', *, *, #189032, .T. ) ;
#39508 = CARTESIAN_POINT ( 'NONE',  ( -1.500000000000011324, 4.629166666666689522, -0.8660254037844313801 ) ) ;
#39507 = CARTESIAN_POINT ( 'NONE',  ( 1.787097420474514031, 1.992035690054320574, -1.134270899834391999 ) ) ;
#39509 = CARTESIAN_POINT ( 'NONE',  ( 4.334856428067313416, 6.080418470877079429, -1.599625672291256295 ) ) ;
#39510 = CARTESIAN_POINT ( 'NONE',  ( 6.681470773436232413, 6.689470745297396270, -0.7998128361456281477 ) ) ;
#39511 = ADVANCED_FACE ( 'NONE', ( #145961 ), #199985, .T. ) ;
#39512 = CARTESIAN_POINT ( 'NONE',  ( 3.967602866622577107, -1.847128000506767176, -1.233534119358855152 ) ) ;
#39513 = CARTESIAN_POINT ( 'NONE',  ( -7.022760382198764084, 11.13704484596649635, 0.7216878364870458196 ) ) ;
#39514 = CARTESIAN_POINT ( 'NONE',  ( 5.178851490740187913, 8.985817805931475277, 0.7216878364870438212 ) ) ;
#39515 = CARTESIAN_POINT ( 'NONE',  ( -8.148087131688683371, 11.48955683940339867, -1.082531754730543083 ) ) ;
#39516 = TOROIDAL_SURFACE ( 'NONE', #160596, 11.92000000000000171, 0.08000000000000000167 ) ;
#39517 = CARTESIAN_POINT ( 'NONE',  ( 5.885648082108177803, 9.880690172519326353, 0.7216878364870317197 ) ) ;
#39518 = CARTESIAN_POINT ( 'NONE',  ( 2.145157927413956944, 0.8647252629472859109, 1.821741647932619390 ) ) ;
#39520 = CARTESIAN_POINT ( 'NONE',  ( 6.197729521560835231, -1.491448369540880670, -1.425081351520232964 ) ) ;
#39519 = CARTESIAN_POINT ( 'NONE',  ( 7.588813295347141441, 9.876701482703580837, -1.599625672291262513 ) ) ;
#39521 = CARTESIAN_POINT ( 'NONE',  ( -10.98997987423604172, -6.893137084989856334, 0.4694063952341883672 ) ) ;
#39522 = CARTESIAN_POINT ( 'NONE',  ( 5.831415467209187575, 9.817418788470464008, 0.000000000000000000 ) ) ;
#39523 = CIRCLE ( 'NONE', #136483, 11.00000000000000000 ) ;
#39524 = CARTESIAN_POINT ( 'NONE',  ( 0.09881949811249221560, -0.4921898920670075839, 1.774194203830472993 ) ) ;
#39525 = PLANE ( 'NONE',  #36873 ) ;
#39526 = CARTESIAN_POINT ( 'NONE',  ( 1.364683531249986537, 2.655208333674754062, -0.7879004041258239610 ) ) ;
#39527 = CARTESIAN_POINT ( 'NONE',  ( 1.053533388295304629, 1.768092659605845052, -0.07913920300933743879 ) ) ;
#39528 = CARTESIAN_POINT ( 'NONE',  ( 0.2291389764034670318, 2.011204493129043591, 0.1455304468792120720 ) ) ;
#39529 = CARTESIAN_POINT ( 'NONE',  ( 0.3273695209934923689, 0.9472894719858866441, -1.578709817245539604 ) ) ;
#39530 = CARTESIAN_POINT ( 'NONE',  ( 4.072042370276293788, -1.319783315292190284, 1.874172932857321339 ) ) ;
#39531 = CARTESIAN_POINT ( 'NONE',  ( 3.134520880496123318, -1.623366475481220261, 0.8686021547102340534 ) ) ;
#39532 = CARTESIAN_POINT ( 'NONE',  ( 8.609591239877852686, 10.00327685373437347, -1.199719254218445830 ) ) ;
#39533 = CARTESIAN_POINT ( 'NONE',  ( 2.836711209001481659, 0.2215568149019596367, 1.812007907362273018 ) ) ;
#39534 = CARTESIAN_POINT ( 'NONE',  ( 4.272111401563948085, 1.799923229630392640, -0.9091438646662284295 ) ) ;
#39535 = CARTESIAN_POINT ( 'NONE',  ( -10.16591625214838679, 10.75465713712827487, 1.040834085586084257E-14 ) ) ;
#39537 = CARTESIAN_POINT ( 'NONE',  ( -5.745623237141265882, 9.925253886631958622, 0.7998128361456291469 ) ) ;
#39536 = CARTESIAN_POINT ( 'NONE',  ( 3.379979430277161079, 1.433683275776801214, 1.750306659111708463 ) ) ;
#39538 = CARTESIAN_POINT ( 'NONE',  ( 5.561587576256037835, 0.4139992630615954572, -2.064685544603379608 ) ) ;
#39539 = CARTESIAN_POINT ( 'NONE',  ( -1.919777701841220319, 3.227564709615637462, -0.4000000000000281664 ) ) ;
#39540 = CARTESIAN_POINT ( 'NONE',  ( 3.350112325975619587, -0.8415805752714689003, 1.891790567983504312 ) ) ;
#39541 = CARTESIAN_POINT ( 'NONE',  ( 10.70146331988817323, 11.37946204949139251, 0.7998128361456341429 ) ) ;
#39542 = CARTESIAN_POINT ( 'NONE',  ( 0.6801582343749970061, 2.505208333674749266, 1.178068619123801675 ) ) ;
#39543 = CARTESIAN_POINT ( 'NONE',  ( 6.182307711929101224, 1.089732742074623006, 1.818925385317768928 ) ) ;
#39544 = ITEM_DEFINED_TRANSFORMATION ( 'NONE', 'NONE', #186969,  #200407 ) ;
#39546 = CARTESIAN_POINT ( 'NONE',  ( 0.9965603196819513565, -0.4670424642401714288, -1.868911657674779958 ) ) ;
#39545 = CARTESIAN_POINT ( 'NONE',  ( -10.16591625214838679, 10.75465713712827487, 1.040834085586084257E-14 ) ) ;
#39547 = CARTESIAN_POINT ( 'NONE',  ( 4.816116650875026828, 5.094466954826537552, -0.7651464576672448725 ) ) ;
#39548 = CARTESIAN_POINT ( 'NONE',  ( 9.206149998879153529, 10.69926207256923689, 1.199719254218453823 ) ) ;
#39549 = CARTESIAN_POINT ( 'NONE',  ( 3.404505970362959655, 6.986024375483197879, 0.7216878364870257245 ) ) ;
#39550 = CARTESIAN_POINT ( 'NONE',  ( 5.869075745953527878, 5.991122463535357490, 0.2593076673842714119 ) ) ;
#39551 = CARTESIAN_POINT ( 'NONE',  ( 1.203941962966152968, 3.258481847795084541, -0.7749999999999840350 ) ) ;
#39552 = CARTESIAN_POINT ( 'NONE',  ( -4.090809663021341969, 5.795697244990093644, 1.599625672291267398 ) ) ;
#39553 = CARTESIAN_POINT ( 'NONE',  ( 0.8794853950937852050, -2.011299634806243741, -0.9433073274909502537 ) ) ;
#39554 = CARTESIAN_POINT ( 'NONE',  ( 2.538226622342924177, 0.9936286567288643568, -1.856823529840909481 ) ) ;
#39555 = CARTESIAN_POINT ( 'NONE',  ( -5.164730172163054966, 4.990216387137135889, -0.7998128361456362523 ) ) ;
#39556 = CARTESIAN_POINT ( 'NONE',  ( 6.740374924288304648, 11.01552117831172062, 1.040834085586084257E-14 ) ) ;
#39557 = CARTESIAN_POINT ( 'NONE',  ( 6.948144928891270666, -0.7966579434352799582, 1.680504273975716334 ) ) ;
#39558 = CARTESIAN_POINT ( 'NONE',  ( 6.205881626753210867, 8.263281202677319470, 1.599625672291281386 ) ) ;
#39559 = CARTESIAN_POINT ( 'NONE',  ( 0.000000000000000000, 1.016439536705160407E-16, 2.080000000000000071 ) ) ;
#39560 = CARTESIAN_POINT ( 'NONE',  ( -7.282137904315833410, 7.668451441222825515, 0.000000000000000000 ) ) ;
#39561 = CARTESIAN_POINT ( 'NONE',  ( -8.514157279702027736, 10.95626946445095307, -1.443375672974059665 ) ) ;
#39562 = CARTESIAN_POINT ( 'NONE',  ( 0.1762450972803019933, 2.096614079038420897, -0.3174041833761130360 ) ) ;
#39563 = CARTESIAN_POINT ( 'NONE',  ( -8.100070429521727178, 8.414780020722290033, 0.7998128361456341429 ) ) ;
#39565 = CARTESIAN_POINT ( 'NONE',  ( 3.473055881322492322, 1.772541284497713976, 0.8411618914155660764 ) ) ;
#39564 = CARTESIAN_POINT ( 'NONE',  ( -1.225000000000034284, -0.7708333333333156068, -0.7072540797573237947 ) ) ;
#39566 = CARTESIAN_POINT ( 'NONE',  ( 2.571340117545738657, 0.1069729528509130723, -2.159185227005658181 ) ) ;
#39567 = CARTESIAN_POINT ( 'NONE',  ( 1.663359199420410883, 0.9473472845980964729, 1.578708189602283873 ) ) ;
#39569 = CARTESIAN_POINT ( 'NONE',  ( -5.552734181323573992, 6.223089306236814444, -0.9332588772281782408 ) ) ;
#39568 = CARTESIAN_POINT ( 'NONE',  ( -3.610214042988883598, 7.433943160120816351, 0.7998128361456352531 ) ) ;
#39570 = CARTESIAN_POINT ( 'NONE',  ( 3.169568575122613918, -1.035934168062458971, 1.398253053441183891 ) ) ;
#39571 = CARTESIAN_POINT ( 'NONE',  ( 6.480434237652124452, 8.583592582059388576, 1.443375672974076540 ) ) ;
#39572 = CARTESIAN_POINT ( 'NONE',  ( -11.83624332731381124, 4.942650230196960592, 4.855242260347336192 ) ) ;
#39573 = CARTESIAN_POINT ( 'NONE',  ( 0.7081719773709761467, -2.151164098719647200, 0.2130325561137471624 ) ) ;
#39574 = CARTESIAN_POINT ( 'NONE',  ( 3.655624903986275154, -0.3905385215352343287, -1.977747697055858955 ) ) ;
#39575 = DIRECTION ( 'NONE',  ( -3.451266460341926649E-31, -5.200010849845536803E-32, 1.000000000000000000 ) ) ;
#39576 = CARTESIAN_POINT ( 'NONE',  ( 0.1456854043008250221, -1.672057201651616642, -1.369741535119282982 ) ) ;
#39577 = CARTESIAN_POINT ( 'NONE',  ( 2.606273030088624765, -0.7529636864501542126, -1.822200628222752972 ) ) ;
#39578 = TOROIDAL_SURFACE ( 'NONE', #150146, 10.92000000000000171, 0.08000000000000000167 ) ;
#39579 = CARTESIAN_POINT ( 'NONE',  ( 6.609000000000047947, 7.052356515605485932, 2.698153947863399793 ) ) ;
#39580 = CARTESIAN_POINT ( 'NONE',  ( 2.489705217443307195, -1.937006489018164190, -0.1406711297040150188 ) ) ;
#39583 = EDGE_LOOP ( 'NONE', ( #177873, #57526, #34491, #106577, #75822, #72338, #10286, #202055 ) ) ;
#39582 = CARTESIAN_POINT ( 'NONE',  ( -5.668717624289589807, 5.786127781192186958, 0.7216878364870257245 ) ) ;
#39581 = CARTESIAN_POINT ( 'NONE',  ( 9.333041836227126353, 3.553052365627043407, 7.472413793103448221 ) ) ;
#39584 = CARTESIAN_POINT ( 'NONE',  ( -5.451787166026575981, 5.533042246551999277, 0.000000000000000000 ) ) ;
#39585 = CARTESIAN_POINT ( 'NONE',  ( 4.386945222473598527, 7.275797305264619652, -1.199719254218452047 ) ) ;
#39586 = AXIS2_PLACEMENT_3D ( 'NONE', #107219, #37889, #7497 ) ;
#39587 = CARTESIAN_POINT ( 'NONE',  ( -6.493429226302317225, 6.540365283632955773, 0.7998128361456341429 ) ) ;
#39588 = CARTESIAN_POINT ( 'NONE',  ( -5.824109505522200081, 8.952488968821326054, -1.199719254218452047 ) ) ;
#39589 = CARTESIAN_POINT ( 'NONE',  ( 5.473738792520003393, 2.225791634824420218, -0.6087584347118053518 ) ) ;
#39591 = ADVANCED_FACE ( 'NONE', ( #196805 ), #115611, .T. ) ;
#39590 = CARTESIAN_POINT ( 'NONE',  ( 0.000000000000000000, 9.799999999999982947, 0.000000000000000000 ) ) ;
#39592 = CARTESIAN_POINT ( 'NONE',  ( 3.660947809037872425, 1.549288415169544963, -1.203348422379519667 ) ) ;
#39593 = CARTESIAN_POINT ( 'NONE',  ( 6.988338112840064120, 10.24047933403371502, 1.199719254218460707 ) ) ;
#39594 = CARTESIAN_POINT ( 'NONE',  ( 0.7916389524552719381, 1.525042296397002062, -1.319230309296010706 ) ) ;
#39595 = ORIENTED_EDGE ( 'NONE', *, *, #171411, .F. ) ;
#39596 = CARTESIAN_POINT ( 'NONE',  ( 2.729822841111886333, 0.7574698553451510996, -1.977403127767562552 ) ) ;
#39597 = CARTESIAN_POINT ( 'NONE',  ( 0.7499999999999902300, 1.014583334016154526, 1.299038105676657340 ) ) ;
#39598 = CARTESIAN_POINT ( 'NONE',  ( -5.357443255694392725, 9.402100898285455699, 0.000000000000000000 ) ) ;
#39599 = CARTESIAN_POINT ( 'NONE',  ( 3.240019139272034110, 0.4481936114588759845, 1.785621944311803100 ) ) ;
#39600 = ORIENTED_EDGE ( 'NONE', *, *, #157816, .T. ) ;
#39601 = CARTESIAN_POINT ( 'NONE',  ( -10.13488352141530768, 11.78278451552804817, 1.199719254218462483 ) ) ;
#39602 = CARTESIAN_POINT ( 'NONE',  ( 4.465154236216789307, -1.701427117168831549, 1.265499569954648962 ) ) ;
#39603 = CARTESIAN_POINT ( 'NONE',  ( 0.5679803739370090643, -1.732728882149033645, -0.6228371021387222317 ) ) ;
#39604 = DIRECTION ( 'NONE',  ( -0.000000000000000000, 1.000000000000000000, 0.000000000000000000 ) ) ;
#39605 = CARTESIAN_POINT ( 'NONE',  ( 8.111855979677986994, 8.358253485912799263, 1.040834085586084257E-14 ) ) ;
#39606 = CARTESIAN_POINT ( 'NONE',  ( 5.905458427204159477, 9.047396044116986502, 1.199719254218452047 ) ) ;
#39607 = ORIENTED_EDGE ( 'NONE', *, *, #40880, .T. ) ;
#39608 = CARTESIAN_POINT ( 'NONE',  ( 4.516905262009872857, 1.882569317753344240, 0.8387543118332175807 ) ) ;
#39610 = CARTESIAN_POINT ( 'NONE',  ( 1.118424870118275738, -0.04499623084481922664, 1.840855209834332928 ) ) ;
#39609 = CARTESIAN_POINT ( 'NONE',  ( -7.039708073993679704, 9.236078724457858158, 1.599625672291283607 ) ) ;
#39611 = CARTESIAN_POINT ( 'NONE',  ( 1.364683531249988535, 4.405208333674754506, -0.7879004041258300672 ) ) ;
#39612 = CARTESIAN_POINT ( 'NONE',  ( 0.000000000000000000, 2.999999999999999112, -11.00000000000000000 ) ) ;
#39613 = CARTESIAN_POINT ( 'NONE',  ( 0.000000000000000000, -1.500000000000001332, 0.000000000000000000 ) ) ;
#39614 = CARTESIAN_POINT ( 'NONE',  ( 1.506762622594171930, -0.7967928049063888185, -2.058199171410409978 ) ) ;
#39615 = CARTESIAN_POINT ( 'NONE',  ( 4.165478197628463164, 0.2823181557158191968, -2.244685958880874743 ) ) ;
#39616 = CARTESIAN_POINT ( 'NONE',  ( -7.036318535812428721, 11.15286269184909784, 0.000000000000000000 ) ) ;
#39617 = CARTESIAN_POINT ( 'NONE',  ( 3.515680188161012687, -0.5209108127710823100, 1.735096886039680930 ) ) ;
#39618 = CARTESIAN_POINT ( 'NONE',  ( 4.751152363292252545, 0.1813030634821456710, -1.907091066879146757 ) ) ;
#39619 = CARTESIAN_POINT ( 'NONE',  ( 4.967269779104159788, 1.799668380515653920, 1.023422521214325309 ) ) ;
#39620 = CARTESIAN_POINT ( 'NONE',  ( -1.364683531249997417, 4.821875000341417916, 1.214306433183764966E-14 ) ) ;
#39621 = CARTESIAN_POINT ( 'NONE',  ( 2.729320057108883368, -1.840128979258702557, 0.7079907272262278006 ) ) ;
#39622 = CARTESIAN_POINT ( 'NONE',  ( 0.9383530073892000223, 1.897354475554638320, 0.3323884044314562858 ) ) ;
#39623 = CARTESIAN_POINT ( 'NONE',  ( 4.434354141042872399, 1.834536173243521917, 0.3649259964926266364 ) ) ;
#39624 = CARTESIAN_POINT ( 'NONE',  ( 3.950101280099535650, 0.7789643570827823327, -2.172381230931414109 ) ) ;
#39625 = CARTESIAN_POINT ( 'NONE',  ( 3.525696930263744200, 1.816150354290571034, -0.4055864600542318232 ) ) ;
#39626 = CARTESIAN_POINT ( 'NONE',  ( 1.364683531249988535, 3.655208333674750509, -0.7879004041258239610 ) ) ;
#39627 = CLOSED_SHELL ( 'NONE', ( #108625, #13250, #118798, #106672, #171398, #57973, #56911, #114876 ) ) ;
#39628 = CARTESIAN_POINT ( 'NONE',  ( 5.182959862174088883, 9.268813282503625572, 0.7998128361456331437 ) ) ;
#39629 = CARTESIAN_POINT ( 'NONE',  ( 1.067171494879548987, -1.904794536548588546, -0.8987870243707897222 ) ) ;
#39630 = CARTESIAN_POINT ( 'NONE',  ( 3.755245360860917536, 5.404205559136275205, -1.443375672974051449 ) ) ;
#39632 = CYLINDRICAL_SURFACE ( 'NONE', #42440, 0.1000000000000000472 ) ;
#39631 = CARTESIAN_POINT ( 'NONE',  ( 1.364683531249988535, 5.217708333674750065, -0.7879004041258300672 ) ) ;
#39633 = CARTESIAN_POINT ( 'NONE',  ( 6.749309733681256418, -1.731629633356733589, -1.293610171197785652 ) ) ;
#39634 = CARTESIAN_POINT ( 'NONE',  ( 1.951583061186522583, -1.892041120407188304, 0.9578705467366486204 ) ) ;
#39635 = CARTESIAN_POINT ( 'NONE',  ( 4.492294583947371578, 8.028511867739082319, -2.500000000000000000 ) ) ;
#39637 = EDGE_CURVE ( 'NONE', #206340, #197886, #175824, .T. ) ;
#39636 = CARTESIAN_POINT ( 'NONE',  ( 1.195576078702242473, 1.864576247583774160, -0.7769579012074608881 ) ) ;
#39638 = CARTESIAN_POINT ( 'NONE',  ( -1.364683531250012516, 1.030208333674754062, 0.7879004041258379498 ) ) ;
#39639 = CARTESIAN_POINT ( 'NONE',  ( -3.416291520963659512, 5.969128626890772615, 1.082531754730560403 ) ) ;
#39640 = CARTESIAN_POINT ( 'NONE',  ( 4.202137545231717120, 6.989912005157271402, 1.199719254218462483 ) ) ;
#39641 = VERTEX_POINT ( 'NONE', #130815 ) ;
#39642 = CARTESIAN_POINT ( 'NONE',  ( 1.300320450452172594, -2.161773191439372965, -0.001381507821696103871 ) ) ;
#39643 = CARTESIAN_POINT ( 'NONE',  ( -1.500000000000001332, -1.099999999999982991, 0.000000000000000000 ) ) ;
#39646 = CARTESIAN_POINT ( 'NONE',  ( 5.043269954603547767, 4.986162489899998995, -0.7216878364870197293 ) ) ;
#39645 = CARTESIAN_POINT ( 'NONE',  ( 6.925078400183562799, 2.053856789352814793, 2.261525409452989965 ) ) ;
#39644 = CARTESIAN_POINT ( 'NONE',  ( 5.923986774528332333, 5.876015756563318426, -0.7998128361456481317 ) ) ;
#39647 = DIRECTION ( 'NONE',  ( 0.000000000000000000, 0.000000000000000000, 1.000000000000000000 ) ) ;
#39648 = CARTESIAN_POINT ( 'NONE',  ( 6.350795928397162449, -1.845624747684541989, -0.8128223418941012968 ) ) ;
#39649 = CARTESIAN_POINT ( 'NONE',  ( -7.199016379176422120, 11.34267684244042584, 0.000000000000000000 ) ) ;
#39650 = EDGE_CURVE ( 'NONE', #57181, #139360, #141372, .T. ) ;
#39651 = CARTESIAN_POINT ( 'NONE',  ( 0.3807642395799659130, -0.2741851280289032688, -2.174293136291181483 ) ) ;
#39652 = CARTESIAN_POINT ( 'NONE',  ( -10.54982673430220608, -8.131911363926706215, 0.6210660986541721718 ) ) ;
#39654 = CARTESIAN_POINT ( 'NONE',  ( -1.364683531250000748, 10.85937500034139802, 0.000000000000000000 ) ) ;
#39653 = CARTESIAN_POINT ( 'NONE',  ( 0.5501786683353731000, 0.7064523498505774768, -2.149447411369388217 ) ) ;
#39655 = CARTESIAN_POINT ( 'NONE',  ( -8.350932551013499960, 11.83017284523606172, -1.199719254218446718 ) ) ;
#39656 = PRESENTATION_LAYER_ASSIGNMENT (  '', '', ( #91471 ) ) ;
#39658 = CARTESIAN_POINT ( 'NONE',  ( 1.142033650006045731, 0.7776438622074226537, 1.750858609485239192 ) ) ;
#39657 = CARTESIAN_POINT ( 'NONE',  ( -4.541618270453545492, 8.242379048930368768, 0.7216878364870458196 ) ) ;
#39659 = CARTESIAN_POINT ( 'NONE',  ( 1.364683531249986537, 0.2177083336747502595, -0.7879004041258309554 ) ) ;
#39660 = CARTESIAN_POINT ( 'NONE',  ( 1.499999999999996891, 9.395833333333332149, -0.8660254037844378194 ) ) ;
#39661 = CARTESIAN_POINT ( 'NONE',  ( 1.499999999999997113, 9.395833333333332149, -0.8660254037844378194 ) ) ;
#39662 = CARTESIAN_POINT ( 'NONE',  ( 2.683889919492283394, -0.8868522494023568514, 1.479262710868123110 ) ) ;
#39663 = CARTESIAN_POINT ( 'NONE',  ( 5.740951700743842423, 5.662474837148078421, -0.7998128361456481317 ) ) ;
#39664 = CARTESIAN_POINT ( 'NONE',  ( 1.686396851806533315, -0.2532433360125495025, -1.751381468886082038 ) ) ;
#39665 = CARTESIAN_POINT ( 'NONE',  ( 5.016741729952475914, 1.524926965779101140, -1.595359541877178877 ) ) ;
#39666 = VERTEX_POINT ( 'NONE', #48448 ) ;
#39667 = CARTESIAN_POINT ( 'NONE',  ( 4.078382194585396192, 0.9556978891391977315, 1.779404116599448082 ) ) ;
#39668 = CARTESIAN_POINT ( 'NONE',  ( -7.099629715411508890, 8.311931418515415615, 1.199719254218452047 ) ) ;
#39670 = CARTESIAN_POINT ( 'NONE',  ( 3.954703970953522774, -1.882481274494081980, -0.7231244775810635739 ) ) ;
#39669 = CARTESIAN_POINT ( 'NONE',  ( 4.846395287928321416, 1.089488137594313510, -1.819044145143506208 ) ) ;
#39672 = ORIENTED_EDGE ( 'NONE', *, *, #65893, .T. ) ;
#39671 = CARTESIAN_POINT ( 'NONE',  ( 4.341949102618557710, -1.119799544600053265, -1.423922225892548354 ) ) ;
#39673 = CARTESIAN_POINT ( 'NONE',  ( 5.761288931164342486, 5.686201605971993978, -0.7998128361456481317 ) ) ;
#39674 = ORIENTED_EDGE ( 'NONE', *, *, #34390, .T. ) ;
#39675 = CARTESIAN_POINT ( 'NONE',  ( 1.322894217037653863, -0.04941562205608431707, 1.870173573632450736 ) ) ;
#39676 = VECTOR ( 'NONE', #156181, 1000.000000000000000 ) ;
#39677 = ADVANCED_FACE ( 'NONE', ( #83041 ), #214076, .F. ) ;
#39678 = DIRECTION ( 'NONE',  ( 1.000000000000000000, 0.000000000000000000, 0.000000000000000000 ) ) ;
#39679 = CARTESIAN_POINT ( 'NONE',  ( 6.340474544234134591, 1.036764729950395258, -1.485249760763515114 ) ) ;
#39680 = CARTESIAN_POINT ( 'NONE',  ( -4.790108344329849110, 4.482881244673243337, 0.7998128361456341429 ) ) ;
#39681 = FACE_OUTER_BOUND ( 'NONE', #194083, .T. ) ;
#39682 = CIRCLE ( 'NONE', #74325, 8.500000000000000000 ) ;
#39683 = CARTESIAN_POINT ( 'NONE',  ( -1.364683531249997417, 3.321875000341423245, 1.214306433183764966E-14 ) ) ;
#39684 = VERTEX_POINT ( 'NONE', #30048 ) ;
#39685 = CARTESIAN_POINT ( 'NONE',  ( 7.078765600110826561, 8.391552967285011988, -1.082531754730548412 ) ) ;
#39686 = CARTESIAN_POINT ( 'NONE',  ( -3.851925040058337579, 6.547644075826416277, -1.082531754730546636 ) ) ;
#39687 = CARTESIAN_POINT ( 'NONE',  ( -4.911796789900812144, 8.952456364851418158, 0.7998128361456291469 ) ) ;
#39688 = CARTESIAN_POINT ( 'NONE',  ( 4.131183091185314460, 1.940096312829143299, 0.8565103500411813675 ) ) ;
#39690 = CARTESIAN_POINT ( 'NONE',  ( -12.15542830485202153, 9.245334104615434256, -2.757920875862237775 ) ) ;
#39689 = CARTESIAN_POINT ( 'NONE',  ( -5.436182321379713578, 6.108390213082993903, 1.083092214668917919 ) ) ;
#39691 = CARTESIAN_POINT ( 'NONE',  ( 5.712177144062582812, -0.8841330711255364072, -1.762019952394773936 ) ) ;
#39692 = CARTESIAN_POINT ( 'NONE',  ( 0.6823417656249899377, 0.8427083336747520637, 1.181850606188755259 ) ) ;
#39694 = CARTESIAN_POINT ( 'NONE',  ( 0.5803383592409648850, 0.9960403410373251942, 1.749501224816521816 ) ) ;
#39693 = AXIS2_PLACEMENT_3D ( 'NONE', #19481, #72495, #170001 ) ;
#39695 = ORIENTED_EDGE ( 'NONE', *, *, #154536, .T. ) ;
#39696 = CARTESIAN_POINT ( 'NONE',  ( 6.456269881894531437, -1.301449686459619226, 1.670992065744638433 ) ) ;
#39697 = CARTESIAN_POINT ( 'NONE',  ( 8.900812118921299643, 12.80989862106750543, 8.049590783350238254 ) ) ;
#39698 = CARTESIAN_POINT ( 'NONE',  ( 1.223191768902037957, -1.870915810643185795, -0.8869332102946840823 ) ) ;
#39699 = EDGE_LOOP ( 'NONE', ( #172075, #28360, #69322, #173038 ) ) ;
#39700 = CARTESIAN_POINT ( 'NONE',  ( 5.879395890181562834, 6.888325289080478697, -1.199719254218452047 ) ) ;
#39701 = CARTESIAN_POINT ( 'NONE',  ( 6.235824307642648279, 6.239826211863360506, 0.000000000000000000 ) ) ;
#39703 = CARTESIAN_POINT ( 'NONE',  ( 5.250031796989762967, 7.148123067953287446, 1.599625672291267398 ) ) ;
#39702 = CARTESIAN_POINT ( 'NONE',  ( 4.646477879911859787, -1.679251869332079483, 1.245118527403435094 ) ) ;
#39704 = CARTESIAN_POINT ( 'NONE',  ( 7.862802741282558294, 8.137967717776607657, 0.000000000000000000 ) ) ;
#39707 = ORIENTED_EDGE ( 'NONE', *, *, #187404, .T. ) ;
#39706 = CARTESIAN_POINT ( 'NONE',  ( 1.822642882514250218, 1.341887823972046201, -1.217030898042359643 ) ) ;
#39705 = CARTESIAN_POINT ( 'NONE',  ( 2.819161699164650869, -0.1809198688003388622, 1.816599095187728219 ) ) ;
#39708 = CARTESIAN_POINT ( 'NONE',  ( 6.674453038267287752, -1.361800985140369402, 1.737325302230605661 ) ) ;
#39709 = CARTESIAN_POINT ( 'NONE',  ( 0.000000000000000000, 0.000000000000000000, -0.09999999999999592548 ) ) ;
#39710 = CARTESIAN_POINT ( 'NONE',  ( 4.014836333542094238, 1.562590183666903165, -1.558512549626612342 ) ) ;
#39711 = CARTESIAN_POINT ( 'NONE',  ( 7.579171565239241737, 8.801120566655981747, 1.199719254218462483 ) ) ;
#39713 =( BOUNDED_SURFACE ( )  B_SPLINE_SURFACE ( 3, 3, ( 
 ( #66028, #133234, #185126, #199238, #186198, #36751, #184069, #49817, #20496, #181932, #117008, #102837, #86581, #70301, #120224, #37832 ),
 ( #103909, #169955, #21542, #35688, #3164, #166772, #69235, #83366, #33563, #118082, #2096, #183008, #136417, #34625, #101764, #18368 ),
 ( #17290, #152646, #149452, #1034, #84445, #19430, #68169, #174259, #175312, #109303, #204570, #121299, #22622, #38901, #57285, #56218 ),
 ( #41052, #9590, #107161, #5291, #7442, #73523, #75666, #171026, #139625, #55152, #43190, #189410, #205648, #123448, #108235, #173186 ),
 ( #206720, #155856, #24766, #91940, #90869, #207781, #23701, #156932, #8521, #25831, #89811, #74602, #140706, #93003, #58348, #39977 ),
 ( #6375, #187273, #124504, #137485, #104985, #190463, #158001, #188338, #141774, #59408, #71369, #42122, #125565, #191525, #106085, #26899 ),
 ( #203499, #72445, #88732, #154788, #138546, #122381, #172108, #46370, #29049, #212031, #77787, #129827, #142833, #79912, #162249, #48504 ) ),
 .UNSPECIFIED., .T., .F., .F. ) 
 B_SPLINE_SURFACE_WITH_KNOTS ( ( 4, 3, 4 ),
 ( 4, 2, 2, 2, 2, 2, 2, 4 ),
 ( 0.000000000000000000, 0.5000000000000000000, 1.000000000000000000 ),
 ( 0.3501333200791456046, 0.3551713324458994903, 0.3602093448126533759, 0.3702853695461611472, 0.3803518226137216351, 0.3853850491475018791, 0.3879016624143920011, 0.3904182756812821231 ),
 .UNSPECIFIED. ) 
 GEOMETRIC_REPRESENTATION_ITEM ( )  RATIONAL_B_SPLINE_SURFACE ( (
 ( 1.000000000000000000, 1.000000000000000000, 1.000000000000000000, 1.000000000000000000, 1.000000000000000000, 1.000000000000000000, 1.000000000000000000, 1.000000000000000000, 1.000000000000000000, 1.000000000000000000, 1.000000000000000000, 1.000000000000000000, 1.000000000000000000, 1.000000000000000000, 1.000000000000000000, 1.000000000000000000),
 ( 0.3333333333333333703, 0.3333333333333333703, 0.3333333333333333703, 0.3333333333333333703, 0.3333333333333333703, 0.3333333333333333703, 0.3333333333333333703, 0.3333333333333333703, 0.3333333333333333703, 0.3333333333333333703, 0.3333333333333333703, 0.3333333333333333703, 0.3333333333333333703, 0.3333333333333333703, 0.3333333333333333703, 0.3333333333333333703),
 ( 0.3333333333333333703, 0.3333333333333333703, 0.3333333333333333703, 0.3333333333333333703, 0.3333333333333333703, 0.3333333333333333703, 0.3333333333333333703, 0.3333333333333333703, 0.3333333333333333703, 0.3333333333333333703, 0.3333333333333333703, 0.3333333333333333703, 0.3333333333333333703, 0.3333333333333333703, 0.3333333333333333703, 0.3333333333333333703),
 ( 1.000000000000000000, 1.000000000000000000, 1.000000000000000000, 1.000000000000000000, 1.000000000000000000, 1.000000000000000000, 1.000000000000000000, 1.000000000000000000, 1.000000000000000000, 1.000000000000000000, 1.000000000000000000, 1.000000000000000000, 1.000000000000000000, 1.000000000000000000, 1.000000000000000000, 1.000000000000000000),
 ( 0.3333333333333333703, 0.3333333333333333703, 0.3333333333333333703, 0.3333333333333333703, 0.3333333333333333703, 0.3333333333333333703, 0.3333333333333333703, 0.3333333333333333703, 0.3333333333333333703, 0.3333333333333333703, 0.3333333333333333703, 0.3333333333333333703, 0.3333333333333333703, 0.3333333333333333703, 0.3333333333333333703, 0.3333333333333333703),
 ( 0.3333333333333333703, 0.3333333333333333703, 0.3333333333333333703, 0.3333333333333333703, 0.3333333333333333703, 0.3333333333333333703, 0.3333333333333333703, 0.3333333333333333703, 0.3333333333333333703, 0.3333333333333333703, 0.3333333333333333703, 0.3333333333333333703, 0.3333333333333333703, 0.3333333333333333703, 0.3333333333333333703, 0.3333333333333333703),
 ( 1.000000000000000000, 1.000000000000000000, 1.000000000000000000, 1.000000000000000000, 1.000000000000000000, 1.000000000000000000, 1.000000000000000000, 1.000000000000000000, 1.000000000000000000, 1.000000000000000000, 1.000000000000000000, 1.000000000000000000, 1.000000000000000000, 1.000000000000000000, 1.000000000000000000, 1.000000000000000000) ) ) 
 REPRESENTATION_ITEM ( '' )  SURFACE ( )  );
#39712 = CARTESIAN_POINT ( 'NONE',  ( -8.012344526598182026E-15, 9.109375000341396245, -1.575800808251669460 ) ) ;
#39714 = CARTESIAN_POINT ( 'NONE',  ( 3.035702773332124238, -1.842316306609870891, 0.5122265333450183311 ) ) ;
#39715 = CARTESIAN_POINT ( 'NONE',  ( 7.771848369131631351, 10.09024240211882351, -1.599625672291262513 ) ) ;
#39716 = CARTESIAN_POINT ( 'NONE',  ( 6.408651866624735405, 0.6456447432892989946, 1.967203394946090755 ) ) ;
#39717 = TOROIDAL_SURFACE ( 'NONE', #157400, 9.559451093910102060, 0.08000000000000000167 ) ;
#39718 = CARTESIAN_POINT ( 'NONE',  ( 1.527007413433539407, 8.693555224946434734, -2.520068491016797196 ) ) ;
#39719 = CARTESIAN_POINT ( 'NONE',  ( 6.110890996357365879, -0.2699588104537915534, 2.174781792473476472 ) ) ;
#39720 = CARTESIAN_POINT ( 'NONE',  ( 5.178155719255617129, 7.862379301422712352, -1.251444257556088457 ) ) ;
#39721 = CARTESIAN_POINT ( 'NONE',  ( -3.531379752551939699, 15.51966450444894008, -11.47742190998778788 ) ) ;
#39722 = ORIENTED_EDGE ( 'NONE', *, *, #15800, .F. ) ;
#39723 = ORIENTED_EDGE ( 'NONE', *, *, #89254, .F. ) ;
#39724 = CARTESIAN_POINT ( 'NONE',  ( 6.343551558972093218, 6.506286488053501849, -2.500000000000000444 ) ) ;
#39725 = CARTESIAN_POINT ( 'NONE',  ( 3.250922972226694352, 7.014770244231638863, 0.7998128361456281477 ) ) ;
#39726 = CARTESIAN_POINT ( 'NONE',  ( -3.285556943749998737, -1.567708332855375142, 1.896917185911908721 ) ) ;
#39727 = CARTESIAN_POINT ( 'NONE',  ( -0.2409995289980246258, 1.355929887833319469, -2.254219809973062816 ) ) ;
#39729 = CARTESIAN_POINT ( 'NONE',  ( -8.839552966430023417, 9.415159337030921449, -0.7216878364870267237 ) ) ;
#39728 = STYLED_ITEM ( 'NONE', ( #151478 ), #86557 ) ;
#39730 = CARTESIAN_POINT ( 'NONE',  ( 3.250922972226694352, 7.014770244231638863, 0.7998128361456281477 ) ) ;
#39731 = CARTESIAN_POINT ( 'NONE',  ( 5.998901810315326877, 0.3981486965325408134, 2.031442706791640074 ) ) ;
#39732 = CARTESIAN_POINT ( 'NONE',  ( 4.565017902933249161, -1.721472425840556930, -0.8649740032428044900 ) ) ;
#39733 = CARTESIAN_POINT ( 'NONE',  ( 0.6148615108944045504, 0.1511614643284354409, 2.010825953887733775 ) ) ;
#39734 = CARTESIAN_POINT ( 'NONE',  ( -9.053093885623068715, 11.58502883802551153, -1.599625672291263179 ) ) ;
#39735 = CARTESIAN_POINT ( 'NONE',  ( 7.991605200612358573, 8.288237253661408843, 0.7998128361456281477 ) ) ;
#39736 = CARTESIAN_POINT ( 'NONE',  ( 11.86145016429272836, 12.69999999999999929, -1.100000000000000311 ) ) ;
#39737 = CARTESIAN_POINT ( 'NONE',  ( 1.675987266036529366, -1.170314894790158933, 1.852603040092117848 ) ) ;
#39738 = CARTESIAN_POINT ( 'NONE',  ( 5.602125774977974260, -1.825872481414937853, 0.004271240736861136277 ) ) ;
#39739 = CARTESIAN_POINT ( 'NONE',  ( -4.843287188579803448, 6.673587691474970107, -1.599625672291256295 ) ) ;
#39740 = VECTOR ( 'NONE', #65806, 1000.000000000000227 ) ;
#39741 = CARTESIAN_POINT ( 'NONE',  ( 5.966997003790217136, 8.054858819212300958, -1.443375672974078761 ) ) ;
#39742 = CARTESIAN_POINT ( 'NONE',  ( 8.886479618753304166, 12.45497775759917758, -1.199719254218446718 ) ) ;
#39743 = CARTESIAN_POINT ( 'NONE',  ( -6.154475385960665790, 6.144919136567696505, 0.000000000000000000 ) ) ;
#39744 = CARTESIAN_POINT ( 'NONE',  ( 4.924636110261782385, 6.768494766770632332, 1.599625672291267398 ) ) ;
#39745 = CARTESIAN_POINT ( 'NONE',  ( 5.225741863424510747, 5.061396693608882558, 0.7998128361456352531 ) ) ;
#39746 = ORIENTED_EDGE ( 'NONE', *, *, #157187, .T. ) ;
#39748 = CARTESIAN_POINT ( 'NONE',  ( 5.836195099138038245, -1.121959161234881819, -1.671398195203987136 ) ) ;
#39747 = CARTESIAN_POINT ( 'NONE',  ( 2.858754248528099229, 0.2676582106064147593, -1.821554178878769470 ) ) ;
#39749 = CARTESIAN_POINT ( 'NONE',  ( 2.179500908114082591, -1.083194949601238521, -2.027108130913716444 ) ) ;
#39751 = CARTESIAN_POINT ( 'NONE',  ( 6.420756404446519738, -1.389671697431221542, 1.384925340169262054 ) ) ;
#39750 = CARTESIAN_POINT ( 'NONE',  ( 3.877268743828276243, 4.586196958296845594, 1.082531754730560403 ) ) ;
#39752 = CARTESIAN_POINT ( 'NONE',  ( -4.232116505760120440, 8.089219690028791376, -0.7998128361456281477 ) ) ;
#39753 = CARTESIAN_POINT ( 'NONE',  ( 11.25751254300906723, -6.452016313277396442, 9.269928574751062911E-15 ) ) ;
#39754 = CARTESIAN_POINT ( 'NONE',  ( 3.111475685156277038, 1.510342251817019532, 1.173009309769344588 ) ) ;
#39755 = CARTESIAN_POINT ( 'NONE',  ( -8.839026081105473054, 12.39961529701003684, -1.199719254218446718 ) ) ;
#39756 = CARTESIAN_POINT ( 'NONE',  ( 0.8716356842100521085, -0.3054578492302991721, 2.047597563663336118 ) ) ;
#39757 = CARTESIAN_POINT ( 'NONE',  ( -3.526002468005825286, 6.271364091718859335, -1.199719254218450271 ) ) ;
#39759 = CARTESIAN_POINT ( 'NONE',  ( 1.305301652190330675, -0.4579020413679709689, 1.813615928118620380 ) ) ;
#39758 = CARTESIAN_POINT ( 'NONE',  ( 2.138330579027637679, 0.4610650599585190967, 2.039099516977191495 ) ) ;
#39760 = CARTESIAN_POINT ( 'NONE',  ( 2.091172504846372959, 1.163092143266548639, -1.646586049616038494 ) ) ;
#39761 = CARTESIAN_POINT ( 'NONE',  ( 6.941411460516762943, 11.04213777067082702, -0.7216878364870267237 ) ) ;
#39762 = ORIENTED_EDGE ( 'NONE', *, *, #116366, .T. ) ;
#39763 = CARTESIAN_POINT ( 'NONE',  ( -0.6823417656249969321, 4.780208333674755394, -1.181850606188749264 ) ) ;
#39764 = CARTESIAN_POINT ( 'NONE',  ( 3.702475415089864441, 1.494950309154385426, 0.8909294612347866682 ) ) ;
#39765 = CARTESIAN_POINT ( 'NONE',  ( 3.876741858503734761, 6.610283703974623393, 1.199719254218462483 ) ) ;
#39767 = CARTESIAN_POINT ( 'NONE',  ( 0.2949160023044670731, 2.710037616963835827, -2.050670093719204168 ) ) ;
#39766 = SURFACE_STYLE_USAGE ( .BOTH. , #190264 ) ;
#39768 = CARTESIAN_POINT ( 'NONE',  ( 2.859633459980165160, 1.716568739768107532, -0.1690650336269062803 ) ) ;
#39769 = CARTESIAN_POINT ( 'NONE',  ( 2.700927432832851860, 1.852951201923001223, 1.169960570980829839 ) ) ;
#39770 = CARTESIAN_POINT ( 'NONE',  ( 0.05276861106134726059, -1.135576942788417254, 1.310739833803043819 ) ) ;
#39771 = CARTESIAN_POINT ( 'NONE',  ( 5.057340365224886725, -1.863002784048470639, -1.182737378625432489 ) ) ;
#39772 = CARTESIAN_POINT ( 'NONE',  ( -10.10707714348148301, 4.359868340440408829, -5.857196085253971063 ) ) ;
#39773 =( BOUNDED_SURFACE ( )  B_SPLINE_SURFACE ( 3, 3, ( 
 ( #106127, #173227, #91983, #190505, #44286, #60509, #42162, #75705, #207822, #59451, #125607, #22662, #191567, #43231, #109348, #175358, #93046, #88773, #154831, #138588, #204611, #172150, #81031, #113602, #147118, #130915, #30152, #214179, #65807, #96240, #212073, #61583, #63712, #161224, #177476, #196908, #178542, #48548, #162291, #163360, #131954, #160156, #47493, #82085, #78884, #213144, #114666, #94115, #79957, #176411, #29091, #14935, #13878, #148178, #97301, #95175, #197964, #111471, #146059, #64774, #180660, #129869, #145007, #110407, #62635, #12811, #32285, #211013, #98350, #46413, #164416, #128794, #45352, #16000, #112529, #195853, #179606, #28017, #127751, #31227, #11754, #77828, #194776, #143949, #209944, #193708, #51742, #151379, #117865, #37614, #84226, #116787, #102622, #53871, #100474, #120004, #182784, #133016, #83149, #166549, #66871, #199015, #167616, #87439, #34402, #118931, #103694, #18137, #67940, #50661, #49595, #33339, #183856, #150314, #1880, #99421, #71152, #134084, #200093, #69020, #35469, #169744, #202217, #101546, #181709, #19214, #85293, #2948, #21333, #135137, #201153, #152436, #52792, #803, #185980, #184911, #36535, #165475, #17071, #168677, #153507, #5077, #115719, #20281, #86365, #4015, #70084, #136199, #149228, #137269, #122155, #171885, #88515, #210510, #127231, #11239, #79454, #203289, #109895, #154577, #27498, #7222, #77318, #175907, #170815, #188123, #13379, #61072, #143431, #45913, #209427, #29651, #54936, #193201, #112031, #44848, #176961, #121088, #187055, #139400, #38687, #159642, #110954, #93598, #23482, #62146, #161788, #104766, #28577, #78382, #94665, #22406, #144503, #138330, #56004, #95736, #39754, #6153, #105859, #155638, #160708, #12302, #128305, #194267, #72223, #178033, #204346, #89589, #73297, #192117, #205433, #60001, #43781, #126154, #181211, #98915, #115220, #166037, #80521, #82642, #16559, #130422, #15497, #146619, #148726, #81585, #48054, #147668, #296, #32838, #66366, #132513, #213685, #17622, #83707, #65308, #131457, #30721, #197458, #212636, #64277, #198511, #97859, #50157, #163921, #164967, #149796, #49100, #1370, #116279, #195345, #145571, #211569, #14432, #182269, #33894, #114167, #99972, #63203, #129367, #96804, #46977, #162853, #196409, #180160, #113093, #179099, #31786, #111652, #175533, #210128, #78011, #192813, #9807, #93228, #60691, #177664, #27122, #144135, #30344, #110587, #94295, #92166, #109526, #125786, #160335, #46599, #193890, #59629, #42342, #43403, #208003, #127938, #158218, #10861, #96429, #190683, #162480, #29272, #159260, #14052, #191748, #176589, #79074, #211198, #44471, #76934, #80141, #143060, #209055, #145192, #126855, #161414, #28201, #62824, #11939, #61770, #95364, #45538, #12998, #128984, #124723, #75882, #194963, #112717, #178729, #146244, #212260, #108457, #174477, #26053, #141989, #65986, #51920, #98533, #131098, #116971, #68127, #114839, #134262, #197087, #147293, #97483, #180837, #81213, #213324, #181887, #101724, #48725, #133194, #118043, #32464, #82264, #64946, #63894, #47676, #132136, #164594, #16180, #113787, #85469, #148357, #214356, #83325, #198143, #184029, #2054, #49775, #196042, #115902, #33523, #99595, #35645, #165661, #17248, #166733, #149412, #15125, #200268, #994, #67058, #179789, #31409, #199196, #167795, #19390, #130049 ),
 ( #50844, #182968, #151557, #163540, #34583, #100655, #18324, #84407, #150495, #187234, #185087, #136376, #24728, #72407, #22585, #52967, #154751, #189372, #186161, #39938, #89773, #201329, #38863, #69194, #70262, #122341, #55115, #205611, #37794, #202395, #56180, #7403, #54047, #73484, #120184, #86541, #36711, #103869, #20458, #152606, #121261, #41015, #169918, #138507, #57248, #21504, #87613, #4192, #3125, #119105, #71329, #153684, #5252, #102797, #90831, #137444, #203461, #88691, #104946, #123408, #155819, #170986, #135315, #6335, #204530, #188298, #107124, #106046, #172069, #23663, #139584, #168855, #173147, #59374, #159015, #140667, #75633, #191490, #156893, #8481, #74568, #143875, #10609, #142801, #60435, #126595, #110333, #29013, #176336, #11679, #196835, #84147, #83069, #181634, #212001, #129797, #214104, #32205, #165395, #116705, #182705, #34324, #2869, #168598, #101466, #104686, #54858, #85212, #186976, #7148, #3933, #72147, #122080, #19135, #4996, #151298, #20198, #154498, #153427, #139326, #22321, #86287, #201073, #36460, #137190, #204269, #39671, #103611, #70003, #118848, #202132, #152358, #55922, #136117, #105782, #185899, #171807, #119924, #184830, #88434, #21252, #203212, #38608, #121009, #170735, #23399, #89512, #155566, #190181, #207498, #10359, #76436, #191239, #142544, #42902, #208550, #109011, #157708, #192303, #175030, #12494, #90580, #160898, #24467, #156640, #25547, #27688, #26617, #62328, #176090, #91655, #60184, #126343, #92718, #74315, #9305, #125277, #93787, #75378, #43962, #94847, #158764, #110078, #8232, #173973, #41836, #159823, #111146, #11426, #124219, #106865, #107947, #58054, #77502, #140412, #141492, #78567, #40759, #28763, #143621, #144687, #189124, #209616, #210698, #61258, #127416, #172892, #206430, #193388, #59120, #45032, #177146, #164102, #163040, #198695, #83889, #194453, #15685, #479, #197643, #128487, #66545, #63395, #195531, #166213, #113284, #149980, #179290, #80716, #31966, #115406, #131640, #213870, #145757, #132688, #129549, #14620, #65493, #114348, #1551, #34080, #180345, #181399, #49288, #33023, #99100, #17806, #47170, #165153, #16744, #96989, #98049, #30914, #82829, #81772, #146806, #147852, #148905, #50339, #116459, #182452, #48235, #46098, #112214, #100149, #178223, #79638, #29838, #212824, #64460, #95922, #196593, #161976, #13566, #211757, #130604, #53531, #155306, #136932, #117531, #105511, #23137, #151052, #55662, #5814, #201881, #199766, #135860, #52468, #84963, #187788, #184583, #69756, #170474, #134812, #18879, #71889, #118593, #19946, #51411, #183525, #102276, #39417, #137998, #67612, #186723, #36201, #152107, #2619, #68690, #167292, #104427, #200817, #3677, #37281, #204016, #202959, #87097, #133757, #103352, #169416, #21000, #4741, #70816, #22060, #154241, #89255, #140148, #28505, #76182, #26355, #56737, #158509, #193131, #189929, #43710, #93528, #205096, #190982, #72966, #74056, #126086, #58867, #44780, #208301, #206172, #110886, #7965, #125025, #175838, #159570, #75124, #41575, #176892, #173717, #57802, #27430, #123961, #109828, #157455, #11167, #25293, #156383, #59931, #9049, #42646, #10109, #6888, #172634, #141233, #77244, #207242, #107689, #91394, #108756, #174780, #92471, #142289, #192047, #209358, #143361, #61003, #127160, #94594, #139071, #122905, #188863 ),
 ( #40501, #106605, #24209, #144436, #14366, #13314, #79387, #210438, #182204, #30654, #177967, #180095, #161722, #96740, #95669, #29581, #45845, #131396, #145506, #129303, #111964, #164902, #81523, #31719, #33830, #160638, #64214, #211504, #196346, #179036, #97794, #130354, #128236, #63141, #12238, #15434, #163854, #62079, #147601, #132451, #195280, #197393, #32772, #194199, #47988, #78312, #46912, #65246, #212575, #198449, #213619, #113030, #50095, #162788, #114104, #115155, #98851, #80457, #146555, #116216, #49035, #181150, #16495, #82576, #148664, #230, #66302, #118351, #34883, #152920, #35962, #151867, #37024, #99909, #51159, #168109, #136686, #19708, #100956, #184339, #135618, #201638, #102040, #53286, #85787, #87920, #134575, #167046, #4499, #104182, #150805, #170231, #18638, #183279, #133510, #2369, #117281, #84717, #3442, #137756, #68446, #169166, #153994, #200576, #69509, #52223, #165970, #83641, #119419, #185406, #103108, #149728, #121573, #20761, #86855, #70567, #202711, #5563, #38110, #54362, #17555, #120503, #186474, #21816, #71643, #203775, #55419, #187544, #1306, #67366, #199514, #23969, #205925, #22890, #89007, #73800, #159316, #109580, #39175, #26107, #7716, #9859, #59679, #173461, #143116, #209107, #25041, #140980, #204840, #206989, #90071, #106357, #125839, #107437, #191797, #91142, #92219, #60745, #157198, #126907, #108506, #155059, #76989, #105258, #122651, #58618, #8795, #139894, #42396, #74874, #171299, #6646, #10913, #72725, #138819, #156134, #158270, #124774, #56493, #75935, #57558, #190733, #174529, #142036, #188614, #123716, #189677, #208052, #41327, #43459, #40246, #175584, #27174, #172380, #93278, #193942, #14103, #117821, #50613, #127988, #110639, #111705, #61821, #198969, #11988, #145244, #167569, #44522, #35421, #116738, #19169, #68972, #182737, #101499, #34356, #166500, #192866, #176641, #129041, #28253, #757, #100429, #80193, #13049, #51699, #151331, #94346, #66823, #67895, #18091, #160388, #134040, #45589, #177714, #85243, #29323, #2899, #95417, #211249, #96484, #84179, #150268, #132966, #210181, #200048, #161469, #62874, #1836, #178784, #78064, #144189, #30398, #183811, #195018, #46650, #112773, #162531, #202168, #105815, #171841, #103647, #121044, #53826, #23434, #187011, #87393, #38642, #89545, #138288, #155596, #7181, #118879, #104721, #201105, #119956, #39706, #170769, #172926, #122112, #185931, #106900, #136151, #22358, #73252, #139359, #203246, #169699, #24503, #153460, #37567, #205390, #21287, #57028, #71108, #123195, #5033, #70035, #188077, #137226, #88470, #72179, #135091, #86317, #54890, #189156, #154530, #6109, #204303, #55959, #40795, #90613, #156672, #8264, #52745, #184865, #36492, #102569, #168629, #20232, #152389, #3967, #157742, #107979, #125310, #91689, #9339, #192336, #112247, #59152, #143657, #128519, #191269, #92751, #75412, #74348, #58090, #142576, #141525, #207533, #124251, #95955, #158795, #42935, #93818, #109044, #62358, #12528, #208583, #206463, #60218, #175063, #26650, #194487, #10392, #76467, #177181, #126377, #25578, #78600, #43995, #110113, #190209, #41869, #176124, #46130, #144720, #140452, #61292, #27724, #159859, #11462, #77535, #174007, #45068, #209651, #127453, #193424, #210732, #111179, #28797, #162009, #94881, #160933, #178258, #29871, #32000, #33057 ),
 ( #197675, #195567, #212856, #14655, #49319, #150012, #82862, #163074, #145787, #146837, #97020, #16778, #47203, #114381, #199798, #79672, #67643, #148938, #51443, #101240, #511, #133790, #66578, #198725, #13598, #211790, #164136, #63428, #181427, #132720, #115436, #48268, #83922, #183557, #129580, #99135, #100183, #50371, #113318, #166248, #80749, #64493, #117562, #130635, #35164, #196627, #180376, #131673, #116494, #182483, #165184, #30945, #17838, #98081, #15720, #34111, #213904, #179325, #81805, #65527, #1582, #147888, #88202, #104461, #205125, #19979, #138030, #204044, #135893, #153199, #86063, #55694, #4770, #119698, #70849, #121849, #170508, #187820, #39447, #87129, #56769, #122935, #136963, #54630, #118627, #120777, #3708, #152140, #105542, #21031, #171575, #202991, #5850, #188892, #186757, #40533, #22090, #2648, #167323, #18909, #36231, #38380, #154275, #201911, #71921, #23172, #84993, #68721, #139098, #134843, #200846, #53564, #155336, #6919, #151084, #72996, #185681, #184613, #102309, #168383, #37310, #103384, #169446, #93559, #157489, #59966, #77282, #75157, #92503, #25326, #143395, #158542, #58906, #10139, #209392, #109859, #61036, #127197, #26391, #210473, #62111, #76214, #208334, #57832, #126120, #9083, #173749, #193164, #174815, #44814, #142324, #159603, #128270, #192080, #194232, #175873, #156412, #144469, #106637, #189961, #43746, #27461, #141267, #11201, #110918, #172665, #7999, #78346, #74091, #140183, #207275, #176924, #28539, #24242, #94631, #125059, #160674, #12270, #90343, #206204, #191015, #42682, #123993, #108789, #41611, #107723, #91427, #15464, #13345, #30686, #46943, #81550, #182234, #115185, #195312, #95700, #179067, #129336, #49065, #79420, #64243, #17586, #111998, #166001, #181180, #83670, #133539, #32805, #149760, #98880, #16524, #45876, #161754, #48018, #145537, #213651, #164933, #147633, #80488, #116245, #1337, #211535, #65277, #132477, #82607, #63170, #50124, #113061, #96769, #67398, #162821, #114134, #180126, #31752, #163889, #148692, #262, #131423, #97824, #33858, #197423, #66331, #210383, #44722, #14305, #178983, #110831, #111909, #62024, #194141, #128180, #96684, #126029, #29524, #58816, #145450, #208246, #191992, #162733, #43657, #80400, #109774, #11113, #176836, #45790, #177910, #144383, #76131, #211447, #59879, #159514, #95616, #28450, #146496, #30597, #94542, #161666, #13260, #79332, #63081, #124969, #175783, #129249, #195221, #27375, #160581, #93476, #46858, #12188, #77188, #78259, #112971, #190931, #42595, #108700, #193071, #174729, #26301, #92415, #158455, #10054, #142234, #143310, #209302, #60949, #127106, #150747, #132389, #51097, #168046, #198390, #85721, #67308, #47933, #35901, #19648, #81468, #17499, #50031, #181093, #1248, #116156, #101977, #114046, #184276, #180040, #31662, #48978, #117223, #182142, #212514, #199455, #115097, #83586, #165914, #66240, #97739, #32710, #148604, #183220, #98792, #149668, #118290, #33773, #99852, #163797, #197337, #213566, #133450, #134514, #34826, #147545, #130298, #131342, #65188, #100900, #15374, #164846, #64156, #196286, #52163, #166989, #16438, #82517, #18580, #173, #84658, #2308, #68385, #200518, #87862, #201580, #105197, #138760, #187484, #186411, #7655, #107375, #3381, #39114, #23908, #6583, #4438, #56431, #203712, #189620, #204777 ),
 ( #172318, #70508, #188552, #153934, #90012, #170166, #86793, #122590, #5503, #55360, #88944, #151808, #103050, #71583, #40184, #137692, #152860, #21754, #171234, #22830, #121512, #154998, #72662, #139836, #38048, #136623, #106297, #156068, #202650, #73739, #54299, #20700, #185345, #120437, #169103, #104119, #205864, #41267, #57498, #123657, #173398, #24979, #69450, #135556, #53226, #119357, #36967, #158209, #9798, #140916, #112708, #175523, #108447, #110578, #92156, #79064, #29263, #10852, #8735, #159251, #75873, #174467, #145182, #207994, #93220, #193880, #141980, #42333, #95355, #59621, #43394, #74816, #206930, #125777, #211188, #161405, #91082, #78002, #191738, #27113, #26043, #109516, #190672, #61760, #76925, #143051, #209046, #12989, #11931, #176580, #178719, #157142, #60682, #126846, #192803, #44462, #28190, #94286, #58559, #160326, #124712, #144126, #210119, #127928, #45528, #62813, #111643, #177655, #128974, #194953, #46589, #96419, #16171, #214347, #212251, #15115, #31399, #65977, #166723, #99587, #179780, #162469, #163530, #113778, #33515, #63885, #131090, #2045, #14043, #84398, #165653, #68116, #118033, #17240, #150486, #83315, #984, #30334, #80130, #180829, #146234, #198136, #149402, #132127, #64939, #100646, #200259, #130040, #49767, #116961, #67049, #196033, #182959, #97474, #81204, #134252, #147283, #51910, #213315, #197079, #148347, #133186, #199186, #115893, #47667, #34574, #48716, #114830, #181878, #82255, #32454, #98523, #50834, #18314, #164585, #154743, #204522, #73475, #102790, #56171, #122333, #54039, #21498, #103860, #188290, #5246, #137436, #203452, #39930, #139576, #35636, #101715, #55107, #167786, #19382, #3116, #69186, #185079, #50577, #114586, #180578, #46336, #136109, #138249, #202125, #121002, #35385, #53784, #151292, #71065, #2863, #105773, #135054, #201066, #153419, #119917, #36454, #4989, #37527, #52708, #118840, #102529, #168591, #20192, #86279, #186970, #103603, #152350, #203205, #3927, #137182, #169660, #38601, #104679, #22313, #204263, #55914, #122073, #109003, #61250, #76425, #92708, #193379, #8223, #126334, #192293, #124212, #141484, #74307, #43953, #207490, #107941, #59110, #110069, #158755, #176081, #27679, #75370, #45023, #111134, #125269, #42894, #106856, #175020, #206422, #140403, #93775, #9297, #159814, #191231, #208542, #28754, #26607, #155559, #10349, #205348, #7140, #73211, #24459, #142534, #60177, #190174, #11418, #77493, #139318, #56984, #127406, #189115, #40749, #58046, #143612, #209605, #172884, #90572, #41828, #156633, #173966, #25540, #91648, #157700, #30905, #81763, #145747, #48228, #471, #80708, #64451, #62318, #79628, #95913, #130596, #16736, #164095, #29829, #12484, #13557, #178213, #98042, #128478, #195522, #66540, #160889, #148898, #15677, #132681, #182444, #147844, #198687, #213863, #65484, #94838, #78558, #96980, #144676, #114340, #131633, #196585, #129541, #165145, #50332, #210690, #180336, #181391, #197632, #194445, #33014, #161966, #211748, #116450, #63386, #46088, #47159, #113275, #212814, #49277, #115398, #31958, #112206, #99093, #179280, #163029, #82822, #146798, #14611, #154234, #19941, #87091, #37275, #1543, #167286, #58596, #103345, #53524, #83883, #185643, #5805, #2613, #70811, #120742, #17795, #3672, #100142, #101198, #153161, #86027, #71882, #20995 ),
 ( #54595, #18871, #136924, #184576, #186716, #52462, #183518, #4736, #36195, #152101, #169410, #34071, #199760, #102271, #202951, #168346, #35126, #118588, #69748, #135854, #201876, #119658, #38344, #22054, #68682, #84955, #104420, #170468, #151044, #88164, #134806, #117524, #67605, #200812, #51404, #137991, #204009, #124751, #166206, #149973, #133751, #175561, #209083, #191777, #190711, #174507, #44500, #43433, #109557, #26083, #212287, #60720, #208030, #210155, #27152, #178760, #129014, #110617, #108483, #176617, #93256, #59658, #30372, #159290, #192841, #79102, #10889, #142015, #194991, #76964, #143091, #92198, #158248, #126883, #96459, #46625, #42372, #177688, #28229, #94322, #125815, #160363, #75912, #161444, #11966, #78039, #144163, #112748, #111681, #61797, #63921, #9836, #127966, #193918, #45564, #29299, #95393, #13025, #145220, #211226, #62852, #162509, #14080, #80170, #146276, #148385, #131126, #214386, #181918, #100681, #88718, #70288, #57272, #7428, #203486, #201355, #137472, #54075, #152632, #123434, #186185, #71356, #23687, #136404, #20483, #73509, #120210, #21528, #52996, #119132, #103895, #189396, #139612, #69222, #122367, #37818, #153710, #4219, #202420, #168879, #39963, #169943, #87639, #5279, #205634, #204555, #154777, #156919, #135341, #187260, #55139, #104972, #121284, #6361, #38887, #36738, #171013, #90855, #138532, #72430, #185112, #188323, #41038, #22610, #106071, #107148, #102824, #89797, #24753, #75653, #127692, #60456, #46357, #209888, #141760, #194718, #9576, #126613, #177418, #95119, #76702, #43177, #112477, #175300, #207768, #29036, #59395, #45294, #159034, #161168, #26886, #157988, #61526, #10627, #192576, #160097, #8508, #174246, #142819, #111414, #208826, #125551, #92989, #44231, #110352, #176355, #27963, #94056, #210955, #109290, #191512, #193652, #12754, #11700, #78828, #77774, #91928, #42108, #143894, #25818, #144949, #62582, #178486, #128744, #30096, #96186, #74589, #206708, #58335, #140692, #124491, #190450, #108221, #149169, #48492, #32226, #97245, #179551, #47433, #132955, #80973, #114610, #113548, #166489, #83090, #181655, #35409, #162237, #65752, #31172, #197906, #180601, #33281, #131898, #129814, #147064, #183799, #17014, #99366, #212016, #165418, #134028, #98298, #198958, #34345, #146006, #49535, #13823, #14880, #66812, #214123, #200035, #746, #213084, #51687, #163299, #115661, #116726, #100418, #15945, #164361, #117809, #82029, #64715, #182726, #148122, #50601, #18080, #84168, #150256, #1824, #67882, #79897, #63660, #195795, #101487, #52734, #169687, #138276, #21275, #102557, #119944, #137213, #203235, #103635, #54879, #87381, #89533, #136139, #168618, #154518, #105804, #152377, #171828, #20220, #184854, #135080, #3956, #118868, #70023, #5022, #139347, #202156, #170757, #155585, #53815, #185920, #37555, #167558, #85231, #153449, #71096, #121033, #151320, #123184, #187000, #38631, #104708, #22346, #7170, #39694, #88458, #19158, #6099, #72168, #204290, #73240, #55947, #122100, #188064, #23422, #205377, #57015, #189144, #2888, #68960, #201093, #25567, #58077, #94868, #157731, #42922, #143645, #107967, #206449, #193412, #91679, #207521, #24489, #90600, #75400, #160922, #111167, #40782, #27712, #9327, #125299, #190199, #124239, #140438, #11450, #173995, #141513, #41858, #45055, #176112, #60204 ),
 ( #172914, #12516, #43982, #78587, #156660, #93807, #144709, #159847, #77524, #8252, #74336, #191257, #59140, #208571, #209639, #76456, #109032, #177168, #210721, #175051, #142564, #127441, #110101, #26637, #62348, #92738, #158783, #10380, #126365, #192324, #61279, #146825, #98068, #33043, #197662, #65513, #63416, #66566, #129568, #80736, #131659, #180364, #150000, #100171, #15706, #99121, #165171, #16765, #82849, #17826, #47192, #148925, #498, #163063, #81792, #113305, #132708, #147875, #64482, #213891, #116481, #182471, #34100, #166236, #83909, #1570, #194476, #46119, #112236, #195555, #178246, #30933, #179312, #95941, #48254, #161997, #79660, #97009, #14643, #130623, #196615, #202979, #183545, #171564, #19969, #105530, #204034, #133778, #120768, #102299, #3698, #68709, #2637, #18898, #104449, #52486, #86053, #84982, #138019, #54620, #153188, #6909, #199785, #37300, #134832, #169436, #152129, #4761, #103374, #101229, #118616, #155325, #186747, #70837, #35152, #136954, #23162, #69774, #170497, #5839, #117551, #21020, #51431, #200835, #38369, #185671, #89277, #22080, #184603, #167311, #36220, #87117, #88192, #71910, #201901, #135882, #53553, #119685, #154265, #55683, #121839, #187811, #9072, #93548, #91416, #7990, #126109, #75146, #125048, #10128, #72986, #24231, #141256, #109848, #207264, #74079, #157477, #108778, #174804, #58894, #26380, #191003, #61026, #107711, #140171, #192069, #77271, #123983, #143383, #206193, #156402, #106627, #41600, #90333, #57821, #42670, #110908, #173737, #142313, #127187, #25315, #158531, #76203, #139090, #56760, #208323, #59954, #43734, #122924, #94621, #175862, #27450, #159592, #11191, #193154, #209382, #44804, #205117, #176914, #160664, #188882, #40523, #172656, #14387, #164923, #79410, #161744, #16516, #129326, #179057, #210463, #62101, #144459, #48007, #82599, #147624, #128260, #253, #145527, #46933, #33850, #113051, #99931, #30676, #96759, #130377, #49056, #15454, #97815, #162810, #132469, #146578, #196367, #163879, #194222, #165993, #71663, #3462, #4519, #169189, #86876, #103131, #203795, #18659, #136707, #202731, #134596, #69532, #84739, #54383, #135639, #118372, #201660, #120521, #20781, #186500, #38131, #85809, #55441, #17578, #53309, #119441, #117303, #37047, #68469, #52244, #21835, #19730, #87943, #152943, #70592, #149752, #154017, #1329, #5583, #133531, #199538, #51180, #34906, #137777, #183299, #184360, #100978, #167067, #35982, #102063, #168128, #155082, #72747, #156159, #158294, #25065, #192891, #92245, #7739, #190759, #58645, #173489, #204861, #73826, #41354, #9885, #139920, #124798, #10937, #91168, #74898, #138844, #90094, #106380, #141007, #27199, #174556, #40269, #22913, #205950, #188639, #108527, #56516, #57582, #77013, #171318, #159340, #26133, #143140, #105281, #75960, #209135, #142063, #208077, #89029, #6670, #107463, #122676, #42422, #59703, #207014, #123740, #175611, #60774, #125865, #157225, #8822, #191823, #172403, #189701, #43487, #93305, #126933, #45613, #62899, #80221, #146320, #46675, #212335, #112795, #35443, #79152, #111728, #97564, #48799, #95444, #117842, #177735, #128011, #78088, #161494, #61845, #193964, #162557, #85269, #29349, #113869, #101522, #13073, #129069, #145269, #44548, #28276, #178807, #211276, #195040, #94369, #68997, #30422, #96507, #63973 ) ),
 .UNSPECIFIED., .T., .F., .T. ) 
 B_SPLINE_SURFACE_WITH_KNOTS ( ( 4, 3, 4 ),
 ( 4, 1, 1, 1, 1, 1, 1, 1, 1, 1, 1, 1, 1, 1, 1, 1, 1, 1, 1, 1, 1, 1, 1, 1, 1, 1, 1, 1, 1, 1, 1, 1, 1, 1, 1, 1, 1, 1, 1, 1, 1, 1, 1, 1, 1, 1, 1, 1, 1, 1, 1, 1, 1, 1, 1, 1, 1, 1, 1, 1, 1, 1, 1, 1, 1, 1, 1, 1, 1, 1, 1, 1, 1, 1, 1, 1, 1, 1, 1, 1, 1, 1, 1, 1, 1, 1, 1, 1, 1, 1, 1, 1, 1, 1, 1, 1, 1, 1, 1, 1, 1, 1, 1, 1, 1, 1, 1, 1, 1, 1, 1, 1, 1, 1, 1, 1, 1, 1, 1, 1, 1, 1, 1, 1, 1, 1, 1, 1, 1, 1, 1, 1, 1, 1, 1, 1, 1, 1, 1, 1, 1, 1, 1, 1, 1, 1, 1, 1, 1, 1, 1, 1, 1, 1, 1, 1, 1, 1, 1, 1, 1, 1, 1, 1, 1, 1, 1, 1, 1, 1, 1, 1, 1, 1, 1, 1, 1, 1, 1, 1, 1, 1, 1, 1, 1, 1, 1, 1, 1, 1, 1, 1, 1, 1, 1, 1, 1, 1, 1, 1, 1, 1, 1, 1, 1, 1, 1, 1, 1, 1, 1, 1, 1, 1, 1, 1, 1, 1, 1, 1, 1, 1, 1, 1, 1, 1, 1, 1, 1, 1, 1, 1, 1, 1, 1, 1, 1, 1, 1, 1, 1, 1, 1, 1, 1, 1, 1, 1, 1, 1, 1, 1, 1, 1, 1, 1, 1, 1, 1, 1, 1, 1, 1, 1, 1, 1, 1, 1, 1, 1, 1, 1, 1, 1, 1, 1, 1, 1, 1, 1, 1, 1, 1, 1, 1, 1, 1, 1, 1, 1, 1, 1, 1, 1, 1, 1, 1, 1, 1, 1, 1, 1, 1, 1, 1, 1, 1, 1, 1, 1, 1, 1, 1, 1, 1, 1, 1, 1, 1, 1, 1, 1, 1, 1, 1, 1, 1, 1, 1, 1, 1, 1, 1, 1, 1, 1, 1, 1, 1, 1, 1, 1, 1, 1, 1, 1, 1, 1, 1, 1, 1, 1, 1, 1, 1, 1, 1, 1, 1, 1, 1, 1, 1, 1, 1, 1, 1, 1, 1, 1, 1, 1, 1, 1, 1, 1, 1, 1, 1, 1, 1, 1, 1, 1, 4 ),
 ( 0.000000000000000000, 0.5000000000000000000, 1.000000000000000000 ),
 ( 0.000000000000000000, 0.002600137934918278840, 0.005208846947063642402, 0.007813284371963545236, 0.01041597565644012714, 0.01302123463190214131, 0.01562472912267370319, 0.01822934229245065652, 0.02083335053635077330, 0.02343730581734793095, 0.02604195799539401474, 0.02864545692284610826, 0.03125045498156164142, 0.03385385361191795006, 0.03645873261014952182, 0.03906243010681619693, 0.04166674480109257978, 0.04427107247243720900, 0.04687475664952634596, 0.04947964045798968619, 0.05208303702386667122, 0.05468803228817373241, 0.05729153353077973132, 0.05989618223844375006, 0.06250015876865079589, 0.06510412050499821135, 0.06770877833268285073, 0.07031227041168378045, 0.07291726700687002627, 0.07552066596874357218, 0.07812554330212571896, 0.08072923942118487295, 0.08333355289058355653, 0.08593787945419822938, 0.08854156225015286097, 0.09114644488045960113, 0.09374984019314609729, 0.09635483420994474246, 0.09895833431534489799, 0.1015629817166532611, 0.1041669571688737805, 0.1067709175595765864, 0.1093755742645453749, 0.1119790650618166516, 0.1145840604711090005, 0.1171874582687142119, 0.1197923343547293018, 0.1223960294069747767, 0.1250003415701952669, 0.1276046670722256471, 0.1302083485727723866, 0.1328132300777099817, 0.1354166241949035232, 0.1380216170238739992, 0.1406251160503516617, 0.1432297622036773077, 0.1458337366370238142, 0.1484376957407889386, 0.1510423513813509144, 0.1536458409560605698, 0.1562508352375901466, 0.1588542319300798034, 0.1614591068269417562, 0.1640628008713490293, 0.1666671117869774343, 0.1692714362859856492, 0.1718751165501164191, 0.1744799969878772505, 0.1770833899687347668, 0.1796883816679979429, 0.1822918796746371972, 0.1848965246383280081, 0.1875004981115827030, 0.1901044559872153150, 0.1927091106216977379, 0.1953125990329364348, 0.1979175922448092595, 0.2005209878913200294, 0.2031258616572126918, 0.2057295547527302204, 0.2083338644793258920, 0.2109381880338489224, 0.2135418671205281671, 0.2161467465492790951, 0.2187501384529311477, 0.2213551290805818306, 0.2239586261264417955, 0.2265632699588193688, 0.2291672425307399730, 0.2317711992370185270, 0.2343758529237242316, 0.2369793402305566954, 0.2395843324308542799, 0.2421877270904984059, 0.2447925997835804779, 0.2473962919891333490, 0.2500006005852301039, 0.2526049232537817546, 0.2552086012219486610, 0.2578134796998332035, 0.2604168705853860954, 0.2630218601994954719, 0.2656253563436123954, 0.2682299991029740149, 0.2708339708322964334, 0.2734379264279751531, 0.2760425792251849364, 0.2786460654866522724, 0.2812510567334335909, 0.2838544504653006673, 0.2864593221437078951, 0.2890630135181997962, 0.2916673210423081364, 0.2942716428833813125, 0.2968753197919519748, 0.2994801973770923054, 0.3020835873036303854, 0.3046885759622478540, 0.3072920712636373342, 0.3098967130082584398, 0.3125006839536987324, 0.3151046384975096371, 0.3177092904634842285, 0.3203127757386058927, 0.3229177660899096303, 0.3255211589530693228, 0.3281260296749167193, 0.3307297202772326306, 0.3333340267878420748, 0.3359383478599109463, 0.3385420237677806976, 0.3411469005182800607, 0.3437502895448679152, 0.3463552773060237788, 0.3489587718236830116, 0.3515634126118191150, 0.3541673828320756612, 0.3567713363827305639, 0.3593759875757128741, 0.3619794719234893932, 0.3645844614373360826, 0.3671878534908398217, 0.3697927233142242476, 0.3723964132032320795, 0.3750007187588132451, 0.3776050391203355505, 0.3802087140863810166, 0.3828135900603256703, 0.3854169782460106219, 0.3880219651677176973, 0.3906254589606275029, 0.3932300988505167960, 0.3958340684042725433, 0.3984380210204655492, 0.4010426714986830565, 0.4036461549780977487, 0.4062511437124918245, 0.4088545350153757196, 0.4114594039983773821, 0.4140630932329303349, 0.4166673978919369636, 0.4192717176013560643, 0.4218753916844373286, 0.4244802669398990425, 0.4270836543437129262, 0.4296886404839689866, 0.4322921336110964741, 0.4348967726609613837, 0.4375007416068860122, 0.4401046933472957945, 0.4427093431689624881, 0.4453128258389836835, 0.4479178138519160357, 0.4505212044632024293, 0.4531260726638874359, 0.4557297613028266636, 0.4583340651236982866, 0.4609383842394453867, 0.4635420574984087105, 0.4661469320934465421, 0.4687503187744080368, 0.4713553041911981989, 0.4739587967114984313, 0.4765634349795482838, 0.4791674033763006491, 0.4817713542995921694, 0.4843760035229108252, 0.4869794854424946973, 0.4895844727919445583, 0.4921878627706443576, 0.4947927302470669919, 0.4973964183492232127, 0.5000007213903868708, 0.5026050399708832384, 0.5052087124645624483, 0.5078135864572254077, 0.5104169724743423675, 0.5130219572256408123, 0.5156254491980594157, 0.5182300867424926016, 0.5208340546487225664, 0.5234380048135498509, 0.5260426534967141965, 0.5286461347248060383, 0.5312511214687432037, 0.5338545108738584899, 0.5364593776840630435, 0.5390630653082590928, 0.5416673676281316130, 0.5442716857317909662, 0.5468753575190105076, 0.5494802309673390006, 0.5520836163796108975, 0.5546886005233833128, 0.5572920920068584749, 0.5598967288858642810, 0.5625006963602153798, 0.5651046458252231286, 0.5677092940264200083, 0.5703127746219572858, 0.5729177608183441128, 0.5755211497088699169, 0.5781260159108934094, 0.5807297031159460721, 0.5833340047729366207, 0.5859383224581667937, 0.5885419935977430628, 0.5911468665597719996, 0.5937502514261915332, 0.5963552350203973340, 0.5989587260738620245, 0.6015633623456233536, 0.6041673294467342359, 0.6067712782705607655, 0.6093759260479724160, 0.6119794060698863225, 0.6145843917766802278, 0.6171877802116071399, 0.6197926458634805957, 0.6223963327082033814, 0.6250006337607152407, 0.6276049510859208480, 0.6302086216366651339, 0.6328134941704254279, 0.6354168785499811900, 0.6380218616525755726, 0.6406253523349600965, 0.6432299880576550777, 0.6458339548441623945, 0.6484379030854412473, 0.6510425504972472410, 0.6536460300044655281, 0.6562510152796211527, 0.6588544033179367654, 0.6614592684776883225, 0.6640629550208935195, 0.6666672555273263079, 0.6692715725509107427, 0.6718752425716313370, 0.6744801147351520143, 0.6770834986868305982, 0.6796884813557668714, 0.6822919717260003125, 0.6848966069578048543, 0.6875005734883452568, 0.6901045212057073108, 0.6927091683100871089, 0.6953126473615357517, 0.6979176322630067375, 0.7005210199636988655, 0.7031258846893556624, 0.7057295709898557812, 0.7083338710086078960, 0.7109381877889758838, 0.7135418573384794128, 0.7161467291897904985, 0.7187501127725786088, 0.7213550950658099703, 0.7239585851828231888, 0.7265632199819130888, 0.7291671863151253374, 0.7317711335672014705, 0.7343757804223364216, 0.7369792590769420615, 0.7395842436626837157, 0.7421876310847422831, 0.7447924954343322357, 0.7473961815509432283, 0.7500004811404139549, 0.7526047977359727748, 0.7552084668730677519, 0.7578133384702019359, 0.7604167217430886083, 0.7630217037185706985, 0.7656251936412983294, 0.7682298280658512724, 0.7708337942603785686, 0.7734377411058018792, 0.7760423877698768846, 0.7786458660865690495, 0.7812508504145402322, 0.7838542376169586046, 0.7864591016485131814, 0.7890627876400562180, 0.7916670868586475063, 0.7942714033278103214, 0.7968750721113085911, 0.7994799435123028930, 0.8020833265342820484, 0.8046883082499752815, 0.8072917980373575109, 0.8098964321455554005, 0.8125003982600473851, 0.8151043447574546352, 0.8177089912886614798, 0.8203124693263749156, 0.8229174534545398156, 0.8255208404963184643, 0.8281257042678743518, 0.8307293901931780411, 0.8333336890992975032, 0.8359380055004849153, 0.8385416739892034288, 0.8411465452521027508, 0.8437499280821748604, 0.8463549095960458679, 0.8489583993070312085, 0.8515630331570626099, 0.8541669992501779163, 0.8567709454582125295, 0.8593755919147509914, 0.8619790697324273276, 0.8645840537187589048, 0.8671874406589066275, 0.8697923042285079509, 0.8723959901464106714, 0.8750002887984731359, 0.8776046051901155165, 0.8802082734428797739, 0.8828131446257380111, 0.8854165273229123168, 0.8880215086929368340, 0.8906249983864840125, 0.8932296320365455955, 0.8958335981669537373, 0.8984375441442679078, 0.9010421905843485346, 0.9036456682409392815, 0.9062506521434200435, 0.9088540390409564074, 0.9114589024666573946, 0.9140625884360091824, 0.9166668868924389146, 0.9192712033329777377, 0.9218748714086243412, 0.9244797425695093773, 0.9270831251927963423, 0.9296881064769593195, 0.9322915962120889022, 0.9348962297203436966, 0.9375001959466012780, 0.9401041417521586174, 0.9427087882339971747, 0.9453122657876905643, 0.9479172496658602176, 0.9505206365780075606, 0.9531254999124115779, 0.9557291860198475764, 0.9583334843266348990, 0.9609378007344983041, 0.9635414689593263526, 0.9661463405142474148, 0.9687497214891268582, 0.9713547029754164841, 0.9739581985331400293, 0.9765628250748574768, 0.9791667834374845336, 0.9817707607320566021, 0.9843753697534296521, 0.9869788348889786400, 0.9895840831931937975, 0.9921867700316038263, 0.9947911815772807476, 0.9973998924267860611, 1.000000000000000000 ),
 .UNSPECIFIED. ) 
 GEOMETRIC_REPRESENTATION_ITEM ( )  RATIONAL_B_SPLINE_SURFACE ( (
 ( 1.000000000000000000, 1.000000000000000000, 1.000000000000000000, 1.000000000000000222, 0.9999999999999996669, 1.000000000000000222, 0.9999999999999997780, 1.000000000000000000, 0.9999999999999997780, 1.000000000000000444, 1.000000000000000000, 0.9999999999999997780, 1.000000000000000222, 1.000000000000000000, 0.9999999999999997780, 1.000000000000000222, 0.9999999999999996669, 1.000000000000000000, 1.000000000000000222, 1.000000000000000000, 1.000000000000000000, 1.000000000000000444, 0.9999999999999994449, 1.000000000000000444, 0.9999999999999996669, 1.000000000000000222, 1.000000000000000000, 1.000000000000000444, 1.000000000000000000, 0.9999999999999997780, 1.000000000000000000, 1.000000000000000222, 0.9999999999999997780, 0.9999999999999997780, 1.000000000000000444, 0.9999999999999997780, 1.000000000000000444, 1.000000000000000222, 0.9999999999999996669, 1.000000000000000222, 1.000000000000000000, 1.000000000000000444, 0.9999999999999997780, 1.000000000000000222, 1.000000000000000222, 1.000000000000000222, 0.9999999999999997780, 1.000000000000000000, 1.000000000000000000, 1.000000000000000000, 0.9999999999999994449, 1.000000000000000444, 0.9999999999999997780, 1.000000000000000444, 0.9999999999999997780, 1.000000000000000000, 1.000000000000000000, 0.9999999999999997780, 1.000000000000000444, 0.9999999999999996669, 1.000000000000000444, 0.9999999999999996669, 1.000000000000000222, 0.9999999999999994449, 1.000000000000000222, 1.000000000000000000, 1.000000000000000000, 1.000000000000000000, 1.000000000000000000, 1.000000000000000222, 1.000000000000000000, 1.000000000000000222, 0.9999999999999996669, 1.000000000000000222, 1.000000000000000000, 1.000000000000000444, 1.000000000000000000, 1.000000000000000000, 0.9999999999999997780, 1.000000000000000222, 0.9999999999999997780, 0.9999999999999997780, 1.000000000000000444, 1.000000000000000000, 1.000000000000000222, 0.9999999999999996669, 1.000000000000000444, 0.9999999999999997780, 1.000000000000000222, 0.9999999999999997780, 1.000000000000000222, 1.000000000000000000, 1.000000000000000000, 1.000000000000000000, 1.000000000000000000, 1.000000000000000222, 1.000000000000000222, 0.9999999999999997780, 1.000000000000000222, 1.000000000000000000, 1.000000000000000222, 0.9999999999999997780, 1.000000000000000222, 1.000000000000000000, 1.000000000000000000, 0.9999999999999997780, 1.000000000000000000, 1.000000000000000000, 0.9999999999999997780, 1.000000000000000222, 0.9999999999999997780, 1.000000000000000222, 0.9999999999999997780, 1.000000000000000444, 1.000000000000000000, 0.9999999999999996669, 1.000000000000000444, 1.000000000000000000, 0.9999999999999997780, 1.000000000000000000, 0.9999999999999996669, 1.000000000000000000, 1.000000000000000222, 0.9999999999999996669, 1.000000000000000222, 0.9999999999999997780, 1.000000000000000000, 1.000000000000000222, 0.9999999999999997780, 1.000000000000000222, 0.9999999999999997780, 1.000000000000000222, 1.000000000000000000, 1.000000000000000000, 1.000000000000000000, 0.9999999999999997780, 1.000000000000000222, 0.9999999999999997780, 1.000000000000000222, 1.000000000000000000, 1.000000000000000000, 1.000000000000000000, 1.000000000000000000, 1.000000000000000444, 0.9999999999999997780, 1.000000000000000444, 0.9999999999999997780, 1.000000000000000222, 1.000000000000000000, 1.000000000000000000, 1.000000000000000000, 1.000000000000000000, 0.9999999999999997780, 1.000000000000000000, 1.000000000000000222, 0.9999999999999997780, 1.000000000000000222, 1.000000000000000000, 1.000000000000000000, 1.000000000000000222, 0.9999999999999997780, 1.000000000000000222, 0.9999999999999996669, 1.000000000000000444, 0.9999999999999994449, 1.000000000000000444, 0.9999999999999997780, 0.9999999999999997780, 1.000000000000000000, 1.000000000000000000, 1.000000000000000222, 1.000000000000000000, 1.000000000000000000, 1.000000000000000000, 1.000000000000000000, 1.000000000000000222, 1.000000000000000444, 0.9999999999999997780, 1.000000000000000222, 1.000000000000000000, 0.9999999999999996669, 1.000000000000000222, 1.000000000000000222, 1.000000000000000222, 1.000000000000000222, 1.000000000000000000, 1.000000000000000000, 1.000000000000000222, 1.000000000000000000, 1.000000000000000222, 1.000000000000000000, 1.000000000000000000, 1.000000000000000000, 1.000000000000000222, 0.9999999999999997780, 1.000000000000000000, 1.000000000000000222, 1.000000000000000000, 1.000000000000000222, 1.000000000000000000, 0.9999999999999997780, 1.000000000000000444, 1.000000000000000000, 0.9999999999999996669, 1.000000000000000222, 0.9999999999999997780, 1.000000000000000222, 1.000000000000000000, 1.000000000000000000, 1.000000000000000444, 0.9999999999999996669, 1.000000000000000000, 0.9999999999999997780, 1.000000000000000000, 0.9999999999999997780, 0.9999999999999997780, 1.000000000000000000, 1.000000000000000000, 1.000000000000000000, 0.9999999999999997780, 1.000000000000000000, 1.000000000000000222, 1.000000000000000222, 1.000000000000000000, 0.9999999999999997780, 1.000000000000000222, 1.000000000000000000, 1.000000000000000000, 1.000000000000000222, 1.000000000000000222, 1.000000000000000222, 1.000000000000000000, 0.9999999999999997780, 1.000000000000000444, 0.9999999999999997780, 1.000000000000000444, 0.9999999999999997780, 1.000000000000000000, 1.000000000000000222, 0.9999999999999997780, 1.000000000000000222, 0.9999999999999997780, 1.000000000000000222, 0.9999999999999997780, 1.000000000000000222, 0.9999999999999996669, 1.000000000000000222, 0.9999999999999997780, 1.000000000000000444, 1.000000000000000000, 1.000000000000000000, 0.9999999999999997780, 1.000000000000000222, 1.000000000000000000, 0.9999999999999996669, 1.000000000000000222, 0.9999999999999997780, 1.000000000000000000, 1.000000000000000222, 1.000000000000000000, 1.000000000000000222, 0.9999999999999996669, 1.000000000000000444, 0.9999999999999996669, 1.000000000000000000, 1.000000000000000000, 1.000000000000000000, 0.9999999999999997780, 1.000000000000000444, 1.000000000000000000, 1.000000000000000000, 1.000000000000000000, 1.000000000000000000, 0.9999999999999997780, 1.000000000000000222, 1.000000000000000222, 1.000000000000000222, 1.000000000000000000, 1.000000000000000222, 1.000000000000000000, 0.9999999999999997780, 1.000000000000000444, 1.000000000000000000, 0.9999999999999997780, 1.000000000000000222, 0.9999999999999996669, 1.000000000000000222, 1.000000000000000000, 1.000000000000000444, 1.000000000000000222, 0.9999999999999996669, 1.000000000000000222, 0.9999999999999997780, 1.000000000000000222, 1.000000000000000222, 0.9999999999999997780, 1.000000000000000222, 1.000000000000000000, 1.000000000000000222, 1.000000000000000222, 0.9999999999999997780, 1.000000000000000444, 0.9999999999999996669, 1.000000000000000222, 1.000000000000000222, 1.000000000000000000, 1.000000000000000000, 1.000000000000000000, 1.000000000000000222, 1.000000000000000000, 1.000000000000000000, 1.000000000000000222, 0.9999999999999996669, 1.000000000000000444, 1.000000000000000222, 0.9999999999999997780, 1.000000000000000222, 0.9999999999999997780, 1.000000000000000444, 0.9999999999999996669, 1.000000000000000666, 0.9999999999999994449, 1.000000000000000222, 0.9999999999999997780, 1.000000000000000444, 1.000000000000000000, 1.000000000000000222, 1.000000000000000222, 1.000000000000000000, 0.9999999999999997780, 0.9999999999999997780, 1.000000000000000444, 1.000000000000000000, 1.000000000000000000, 1.000000000000000000, 0.9999999999999997780, 1.000000000000000222, 1.000000000000000222, 0.9999999999999997780, 1.000000000000000222, 1.000000000000000000, 1.000000000000000444, 0.9999999999999996669, 1.000000000000000444, 0.9999999999999997780, 1.000000000000000000, 0.9999999999999997780, 1.000000000000000444, 0.9999999999999996669, 1.000000000000000444, 1.000000000000000000, 1.000000000000000000, 1.000000000000000000, 0.9999999999999997780, 1.000000000000000444, 1.000000000000000222, 0.9999999999999997780, 1.000000000000000444, 1.000000000000000000, 0.9999999999999996669, 1.000000000000000444, 1.000000000000000000, 1.000000000000000000, 1.000000000000000000, 0.9999999999999997780, 1.000000000000000222, 0.9999999999999997780, 1.000000000000000000, 1.000000000000000222, 0.9999999999999997780, 1.000000000000000000, 1.000000000000000000, 0.9999999999999997780, 1.000000000000000444, 0.9999999999999997780, 1.000000000000000444, 0.9999999999999994449, 1.000000000000000444, 0.9999999999999997780, 1.000000000000000444, 0.9999999999999997780, 1.000000000000000000, 0.9999999999999997780, 1.000000000000000222, 1.000000000000000222, 1.000000000000000000, 1.000000000000000000),
 ( 0.3333333333333333703, 0.3333333333333333703, 0.3333333333333333703, 0.3333333333333335369, 0.3333333333333333148, 0.3333333333333333703, 0.3333333333333333703, 0.3333333333333333148, 0.3333333333333333148, 0.3333333333333334259, 0.3333333333333333703, 0.3333333333333333148, 0.3333333333333334259, 0.3333333333333333148, 0.3333333333333334259, 0.3333333333333333148, 0.3333333333333333703, 0.3333333333333333148, 0.3333333333333334814, 0.3333333333333333148, 0.3333333333333334814, 0.3333333333333334814, 0.3333333333333333148, 0.3333333333333334259, 0.3333333333333333148, 0.3333333333333333703, 0.3333333333333333148, 0.3333333333333334814, 0.3333333333333333703, 0.3333333333333333703, 0.3333333333333333703, 0.3333333333333334259, 0.3333333333333333148, 0.3333333333333333148, 0.3333333333333334259, 0.3333333333333333703, 0.3333333333333334259, 0.3333333333333334259, 0.3333333333333332038, 0.3333333333333334814, 0.3333333333333333703, 0.3333333333333334814, 0.3333333333333332593, 0.3333333333333334259, 0.3333333333333333703, 0.3333333333333334259, 0.3333333333333333148, 0.3333333333333333703, 0.3333333333333334259, 0.3333333333333333148, 0.3333333333333332038, 0.3333333333333335369, 0.3333333333333332593, 0.3333333333333334814, 0.3333333333333333148, 0.3333333333333333703, 0.3333333333333334259, 0.3333333333333333703, 0.3333333333333334814, 0.3333333333333333703, 0.3333333333333334259, 0.3333333333333333148, 0.3333333333333334814, 0.3333333333333332038, 0.3333333333333334259, 0.3333333333333333148, 0.3333333333333333703, 0.3333333333333333703, 0.3333333333333334259, 0.3333333333333333148, 0.3333333333333333703, 0.3333333333333334259, 0.3333333333333333148, 0.3333333333333333703, 0.3333333333333333703, 0.3333333333333335369, 0.3333333333333333148, 0.3333333333333333703, 0.3333333333333333703, 0.3333333333333333703, 0.3333333333333333148, 0.3333333333333333703, 0.3333333333333334814, 0.3333333333333333148, 0.3333333333333334814, 0.3333333333333333703, 0.3333333333333334259, 0.3333333333333333148, 0.3333333333333334259, 0.3333333333333333148, 0.3333333333333334259, 0.3333333333333333148, 0.3333333333333333703, 0.3333333333333333703, 0.3333333333333333703, 0.3333333333333334259, 0.3333333333333334259, 0.3333333333333332593, 0.3333333333333334259, 0.3333333333333333703, 0.3333333333333334259, 0.3333333333333333148, 0.3333333333333334259, 0.3333333333333333703, 0.3333333333333333703, 0.3333333333333333148, 0.3333333333333334259, 0.3333333333333333703, 0.3333333333333333148, 0.3333333333333334259, 0.3333333333333332038, 0.3333333333333334814, 0.3333333333333333148, 0.3333333333333335369, 0.3333333333333334259, 0.3333333333333332038, 0.3333333333333334814, 0.3333333333333333703, 0.3333333333333332593, 0.3333333333333333703, 0.3333333333333332593, 0.3333333333333333703, 0.3333333333333334814, 0.3333333333333333148, 0.3333333333333334814, 0.3333333333333333148, 0.3333333333333334259, 0.3333333333333334259, 0.3333333333333333148, 0.3333333333333334259, 0.3333333333333333148, 0.3333333333333334259, 0.3333333333333333703, 0.3333333333333333703, 0.3333333333333334259, 0.3333333333333332593, 0.3333333333333334814, 0.3333333333333333148, 0.3333333333333333703, 0.3333333333333333703, 0.3333333333333333703, 0.3333333333333334259, 0.3333333333333334259, 0.3333333333333334814, 0.3333333333333333703, 0.3333333333333334259, 0.3333333333333333703, 0.3333333333333333703, 0.3333333333333333148, 0.3333333333333333703, 0.3333333333333334259, 0.3333333333333333148, 0.3333333333333333148, 0.3333333333333333148, 0.3333333333333334259, 0.3333333333333333148, 0.3333333333333334814, 0.3333333333333333148, 0.3333333333333334259, 0.3333333333333334259, 0.3333333333333333148, 0.3333333333333334814, 0.3333333333333333148, 0.3333333333333334814, 0.3333333333333332593, 0.3333333333333335369, 0.3333333333333333148, 0.3333333333333333703, 0.3333333333333333703, 0.3333333333333334259, 0.3333333333333333703, 0.3333333333333333703, 0.3333333333333333148, 0.3333333333333333703, 0.3333333333333332593, 0.3333333333333335369, 0.3333333333333334259, 0.3333333333333333703, 0.3333333333333334259, 0.3333333333333334259, 0.3333333333333332038, 0.3333333333333334814, 0.3333333333333333703, 0.3333333333333334259, 0.3333333333333333703, 0.3333333333333333703, 0.3333333333333333148, 0.3333333333333334814, 0.3333333333333333148, 0.3333333333333334814, 0.3333333333333334259, 0.3333333333333333148, 0.3333333333333333703, 0.3333333333333333703, 0.3333333333333333703, 0.3333333333333333703, 0.3333333333333334259, 0.3333333333333333148, 0.3333333333333334814, 0.3333333333333333148, 0.3333333333333333703, 0.3333333333333334814, 0.3333333333333332593, 0.3333333333333333148, 0.3333333333333334259, 0.3333333333333332593, 0.3333333333333335369, 0.3333333333333333703, 0.3333333333333334259, 0.3333333333333335369, 0.3333333333333333148, 0.3333333333333333703, 0.3333333333333333148, 0.3333333333333333703, 0.3333333333333333148, 0.3333333333333333148, 0.3333333333333333703, 0.3333333333333333703, 0.3333333333333333703, 0.3333333333333333148, 0.3333333333333333703, 0.3333333333333333703, 0.3333333333333334259, 0.3333333333333333703, 0.3333333333333333148, 0.3333333333333333703, 0.3333333333333333703, 0.3333333333333333703, 0.3333333333333334259, 0.3333333333333334259, 0.3333333333333334814, 0.3333333333333332593, 0.3333333333333334259, 0.3333333333333334259, 0.3333333333333333148, 0.3333333333333334259, 0.3333333333333333703, 0.3333333333333333148, 0.3333333333333334814, 0.3333333333333333703, 0.3333333333333334259, 0.3333333333333332593, 0.3333333333333334259, 0.3333333333333332593, 0.3333333333333334814, 0.3333333333333332593, 0.3333333333333334259, 0.3333333333333333148, 0.3333333333333334259, 0.3333333333333333703, 0.3333333333333334259, 0.3333333333333333703, 0.3333333333333333703, 0.3333333333333333703, 0.3333333333333333148, 0.3333333333333334259, 0.3333333333333333703, 0.3333333333333333148, 0.3333333333333334259, 0.3333333333333333148, 0.3333333333333333703, 0.3333333333333333148, 0.3333333333333334814, 0.3333333333333332593, 0.3333333333333333703, 0.3333333333333333703, 0.3333333333333334259, 0.3333333333333332593, 0.3333333333333335369, 0.3333333333333333703, 0.3333333333333333703, 0.3333333333333333703, 0.3333333333333333148, 0.3333333333333333148, 0.3333333333333334259, 0.3333333333333334814, 0.3333333333333334259, 0.3333333333333333703, 0.3333333333333334259, 0.3333333333333334259, 0.3333333333333333703, 0.3333333333333334814, 0.3333333333333333148, 0.3333333333333333148, 0.3333333333333334259, 0.3333333333333332038, 0.3333333333333334814, 0.3333333333333333148, 0.3333333333333335369, 0.3333333333333334259, 0.3333333333333333148, 0.3333333333333334814, 0.3333333333333333703, 0.3333333333333333703, 0.3333333333333334259, 0.3333333333333333703, 0.3333333333333334259, 0.3333333333333333703, 0.3333333333333334259, 0.3333333333333333148, 0.3333333333333333703, 0.3333333333333335369, 0.3333333333333332038, 0.3333333333333334814, 0.3333333333333333703, 0.3333333333333333148, 0.3333333333333334259, 0.3333333333333333703, 0.3333333333333333148, 0.3333333333333334259, 0.3333333333333333703, 0.3333333333333334259, 0.3333333333333332593, 0.3333333333333335369, 0.3333333333333334814, 0.3333333333333333148, 0.3333333333333334259, 0.3333333333333333148, 0.3333333333333335369, 0.3333333333333332593, 0.3333333333333335924, 0.3333333333333332593, 0.3333333333333333703, 0.3333333333333333703, 0.3333333333333334814, 0.3333333333333333703, 0.3333333333333334814, 0.3333333333333333703, 0.3333333333333334259, 0.3333333333333332593, 0.3333333333333334259, 0.3333333333333335369, 0.3333333333333333148, 0.3333333333333334814, 0.3333333333333333148, 0.3333333333333333703, 0.3333333333333334259, 0.3333333333333334259, 0.3333333333333332593, 0.3333333333333334259, 0.3333333333333333148, 0.3333333333333335369, 0.3333333333333332593, 0.3333333333333335369, 0.3333333333333333148, 0.3333333333333333148, 0.3333333333333333703, 0.3333333333333334814, 0.3333333333333333148, 0.3333333333333334259, 0.3333333333333333148, 0.3333333333333334259, 0.3333333333333333703, 0.3333333333333333148, 0.3333333333333334259, 0.3333333333333334814, 0.3333333333333333148, 0.3333333333333334814, 0.3333333333333333703, 0.3333333333333332593, 0.3333333333333334259, 0.3333333333333333703, 0.3333333333333334259, 0.3333333333333333703, 0.3333333333333333148, 0.3333333333333334259, 0.3333333333333333703, 0.3333333333333333148, 0.3333333333333334259, 0.3333333333333333148, 0.3333333333333333148, 0.3333333333333333703, 0.3333333333333333703, 0.3333333333333334259, 0.3333333333333333148, 0.3333333333333334259, 0.3333333333333332593, 0.3333333333333334259, 0.3333333333333333703, 0.3333333333333334259, 0.3333333333333333703, 0.3333333333333333703, 0.3333333333333333148, 0.3333333333333334814, 0.3333333333333334259, 0.3333333333333333703, 0.3333333333333333703),
 ( 0.3333333333333333703, 0.3333333333333333703, 0.3333333333333333703, 0.3333333333333335369, 0.3333333333333333148, 0.3333333333333333703, 0.3333333333333333703, 0.3333333333333333148, 0.3333333333333333148, 0.3333333333333334259, 0.3333333333333333703, 0.3333333333333333148, 0.3333333333333334259, 0.3333333333333333148, 0.3333333333333334259, 0.3333333333333333148, 0.3333333333333333703, 0.3333333333333333148, 0.3333333333333334814, 0.3333333333333333148, 0.3333333333333334814, 0.3333333333333334814, 0.3333333333333333148, 0.3333333333333334259, 0.3333333333333333148, 0.3333333333333333703, 0.3333333333333333148, 0.3333333333333334814, 0.3333333333333333703, 0.3333333333333333703, 0.3333333333333333703, 0.3333333333333334259, 0.3333333333333333148, 0.3333333333333333148, 0.3333333333333334259, 0.3333333333333333703, 0.3333333333333334259, 0.3333333333333334259, 0.3333333333333332038, 0.3333333333333334814, 0.3333333333333333703, 0.3333333333333334814, 0.3333333333333332593, 0.3333333333333334259, 0.3333333333333333703, 0.3333333333333334259, 0.3333333333333333148, 0.3333333333333333703, 0.3333333333333334259, 0.3333333333333333148, 0.3333333333333332038, 0.3333333333333335369, 0.3333333333333332593, 0.3333333333333334814, 0.3333333333333333148, 0.3333333333333333703, 0.3333333333333334259, 0.3333333333333333703, 0.3333333333333334814, 0.3333333333333333703, 0.3333333333333334259, 0.3333333333333333148, 0.3333333333333334814, 0.3333333333333332038, 0.3333333333333334259, 0.3333333333333333148, 0.3333333333333333703, 0.3333333333333333703, 0.3333333333333334259, 0.3333333333333333148, 0.3333333333333333703, 0.3333333333333334259, 0.3333333333333333148, 0.3333333333333333703, 0.3333333333333333703, 0.3333333333333335369, 0.3333333333333333148, 0.3333333333333333703, 0.3333333333333333703, 0.3333333333333333703, 0.3333333333333333148, 0.3333333333333333703, 0.3333333333333334814, 0.3333333333333333148, 0.3333333333333334814, 0.3333333333333333703, 0.3333333333333334259, 0.3333333333333333148, 0.3333333333333334259, 0.3333333333333333148, 0.3333333333333334259, 0.3333333333333333148, 0.3333333333333333703, 0.3333333333333333703, 0.3333333333333333703, 0.3333333333333334259, 0.3333333333333334259, 0.3333333333333332593, 0.3333333333333334259, 0.3333333333333333703, 0.3333333333333334259, 0.3333333333333333148, 0.3333333333333334259, 0.3333333333333333703, 0.3333333333333333703, 0.3333333333333333148, 0.3333333333333334259, 0.3333333333333333703, 0.3333333333333333148, 0.3333333333333334259, 0.3333333333333332038, 0.3333333333333334814, 0.3333333333333333148, 0.3333333333333335369, 0.3333333333333334259, 0.3333333333333332038, 0.3333333333333334814, 0.3333333333333333703, 0.3333333333333332593, 0.3333333333333333703, 0.3333333333333332593, 0.3333333333333333703, 0.3333333333333334814, 0.3333333333333333148, 0.3333333333333334814, 0.3333333333333333148, 0.3333333333333334259, 0.3333333333333334259, 0.3333333333333333148, 0.3333333333333334259, 0.3333333333333333148, 0.3333333333333334259, 0.3333333333333333703, 0.3333333333333333703, 0.3333333333333334259, 0.3333333333333332593, 0.3333333333333334814, 0.3333333333333333148, 0.3333333333333333703, 0.3333333333333333703, 0.3333333333333333703, 0.3333333333333334259, 0.3333333333333334259, 0.3333333333333334814, 0.3333333333333333703, 0.3333333333333334259, 0.3333333333333333703, 0.3333333333333333703, 0.3333333333333333148, 0.3333333333333333703, 0.3333333333333334259, 0.3333333333333333148, 0.3333333333333333148, 0.3333333333333333148, 0.3333333333333334259, 0.3333333333333333148, 0.3333333333333334814, 0.3333333333333333148, 0.3333333333333334259, 0.3333333333333334259, 0.3333333333333333148, 0.3333333333333334814, 0.3333333333333333148, 0.3333333333333334814, 0.3333333333333332593, 0.3333333333333335369, 0.3333333333333333148, 0.3333333333333333703, 0.3333333333333333703, 0.3333333333333334259, 0.3333333333333333703, 0.3333333333333333703, 0.3333333333333333148, 0.3333333333333333703, 0.3333333333333332593, 0.3333333333333335369, 0.3333333333333334259, 0.3333333333333333703, 0.3333333333333334259, 0.3333333333333334259, 0.3333333333333332038, 0.3333333333333334814, 0.3333333333333333703, 0.3333333333333334259, 0.3333333333333333703, 0.3333333333333333703, 0.3333333333333333148, 0.3333333333333334814, 0.3333333333333333148, 0.3333333333333334814, 0.3333333333333334259, 0.3333333333333333148, 0.3333333333333333703, 0.3333333333333333703, 0.3333333333333333703, 0.3333333333333333703, 0.3333333333333334259, 0.3333333333333333148, 0.3333333333333334814, 0.3333333333333333148, 0.3333333333333333703, 0.3333333333333334814, 0.3333333333333332593, 0.3333333333333333148, 0.3333333333333334259, 0.3333333333333332593, 0.3333333333333335369, 0.3333333333333333703, 0.3333333333333334259, 0.3333333333333335369, 0.3333333333333333148, 0.3333333333333333703, 0.3333333333333333148, 0.3333333333333333703, 0.3333333333333333148, 0.3333333333333333148, 0.3333333333333333703, 0.3333333333333333703, 0.3333333333333333703, 0.3333333333333333148, 0.3333333333333333703, 0.3333333333333333703, 0.3333333333333334259, 0.3333333333333333703, 0.3333333333333333148, 0.3333333333333333703, 0.3333333333333333703, 0.3333333333333333703, 0.3333333333333334259, 0.3333333333333334259, 0.3333333333333334814, 0.3333333333333332593, 0.3333333333333334259, 0.3333333333333334259, 0.3333333333333333148, 0.3333333333333334259, 0.3333333333333333703, 0.3333333333333333148, 0.3333333333333334814, 0.3333333333333333703, 0.3333333333333334259, 0.3333333333333332593, 0.3333333333333334259, 0.3333333333333332593, 0.3333333333333334814, 0.3333333333333332593, 0.3333333333333334259, 0.3333333333333333148, 0.3333333333333334259, 0.3333333333333333703, 0.3333333333333334259, 0.3333333333333333703, 0.3333333333333333703, 0.3333333333333333703, 0.3333333333333333148, 0.3333333333333334259, 0.3333333333333333703, 0.3333333333333333148, 0.3333333333333334259, 0.3333333333333333148, 0.3333333333333333703, 0.3333333333333333148, 0.3333333333333334814, 0.3333333333333332593, 0.3333333333333333703, 0.3333333333333333703, 0.3333333333333334259, 0.3333333333333332593, 0.3333333333333335369, 0.3333333333333333703, 0.3333333333333333703, 0.3333333333333333703, 0.3333333333333333148, 0.3333333333333333148, 0.3333333333333334259, 0.3333333333333334814, 0.3333333333333334259, 0.3333333333333333703, 0.3333333333333334259, 0.3333333333333334259, 0.3333333333333333703, 0.3333333333333334814, 0.3333333333333333148, 0.3333333333333333148, 0.3333333333333334259, 0.3333333333333332038, 0.3333333333333334814, 0.3333333333333333148, 0.3333333333333335369, 0.3333333333333334259, 0.3333333333333333148, 0.3333333333333334814, 0.3333333333333333703, 0.3333333333333333703, 0.3333333333333334259, 0.3333333333333333703, 0.3333333333333334259, 0.3333333333333333703, 0.3333333333333334259, 0.3333333333333333148, 0.3333333333333333703, 0.3333333333333335369, 0.3333333333333332038, 0.3333333333333334814, 0.3333333333333333703, 0.3333333333333333148, 0.3333333333333334259, 0.3333333333333333703, 0.3333333333333333148, 0.3333333333333334259, 0.3333333333333333703, 0.3333333333333334259, 0.3333333333333332593, 0.3333333333333335369, 0.3333333333333334814, 0.3333333333333333148, 0.3333333333333334259, 0.3333333333333333148, 0.3333333333333335369, 0.3333333333333332593, 0.3333333333333335924, 0.3333333333333332593, 0.3333333333333333703, 0.3333333333333333703, 0.3333333333333334814, 0.3333333333333333703, 0.3333333333333334814, 0.3333333333333333703, 0.3333333333333334259, 0.3333333333333332593, 0.3333333333333334259, 0.3333333333333335369, 0.3333333333333333148, 0.3333333333333334814, 0.3333333333333333148, 0.3333333333333333703, 0.3333333333333334259, 0.3333333333333334259, 0.3333333333333332593, 0.3333333333333334259, 0.3333333333333333148, 0.3333333333333335369, 0.3333333333333332593, 0.3333333333333335369, 0.3333333333333333148, 0.3333333333333333148, 0.3333333333333333703, 0.3333333333333334814, 0.3333333333333333148, 0.3333333333333334259, 0.3333333333333333148, 0.3333333333333334259, 0.3333333333333333703, 0.3333333333333333148, 0.3333333333333334259, 0.3333333333333334814, 0.3333333333333333148, 0.3333333333333334814, 0.3333333333333333703, 0.3333333333333332593, 0.3333333333333334259, 0.3333333333333333703, 0.3333333333333334259, 0.3333333333333333703, 0.3333333333333333148, 0.3333333333333334259, 0.3333333333333333703, 0.3333333333333333148, 0.3333333333333334259, 0.3333333333333333148, 0.3333333333333333148, 0.3333333333333333703, 0.3333333333333333703, 0.3333333333333334259, 0.3333333333333333148, 0.3333333333333334259, 0.3333333333333332593, 0.3333333333333334259, 0.3333333333333333703, 0.3333333333333334259, 0.3333333333333333703, 0.3333333333333333703, 0.3333333333333333148, 0.3333333333333334814, 0.3333333333333334259, 0.3333333333333333703, 0.3333333333333333703),
 ( 1.000000000000000000, 1.000000000000000000, 1.000000000000000000, 1.000000000000000222, 0.9999999999999996669, 1.000000000000000222, 0.9999999999999997780, 1.000000000000000000, 0.9999999999999997780, 1.000000000000000444, 1.000000000000000000, 0.9999999999999997780, 1.000000000000000222, 1.000000000000000000, 0.9999999999999997780, 1.000000000000000222, 0.9999999999999996669, 1.000000000000000000, 1.000000000000000222, 1.000000000000000000, 1.000000000000000000, 1.000000000000000444, 0.9999999999999994449, 1.000000000000000444, 0.9999999999999996669, 1.000000000000000222, 1.000000000000000000, 1.000000000000000444, 1.000000000000000000, 0.9999999999999997780, 1.000000000000000000, 1.000000000000000222, 0.9999999999999997780, 0.9999999999999997780, 1.000000000000000444, 0.9999999999999997780, 1.000000000000000444, 1.000000000000000222, 0.9999999999999996669, 1.000000000000000222, 1.000000000000000000, 1.000000000000000444, 0.9999999999999997780, 1.000000000000000222, 1.000000000000000222, 1.000000000000000222, 0.9999999999999997780, 1.000000000000000000, 1.000000000000000000, 1.000000000000000000, 0.9999999999999994449, 1.000000000000000444, 0.9999999999999997780, 1.000000000000000444, 0.9999999999999997780, 1.000000000000000000, 1.000000000000000000, 0.9999999999999997780, 1.000000000000000444, 0.9999999999999996669, 1.000000000000000444, 0.9999999999999996669, 1.000000000000000222, 0.9999999999999994449, 1.000000000000000222, 1.000000000000000000, 1.000000000000000000, 1.000000000000000000, 1.000000000000000000, 1.000000000000000222, 1.000000000000000000, 1.000000000000000222, 0.9999999999999996669, 1.000000000000000222, 1.000000000000000000, 1.000000000000000444, 1.000000000000000000, 1.000000000000000000, 0.9999999999999997780, 1.000000000000000222, 0.9999999999999997780, 0.9999999999999997780, 1.000000000000000444, 1.000000000000000000, 1.000000000000000222, 0.9999999999999996669, 1.000000000000000444, 0.9999999999999997780, 1.000000000000000222, 0.9999999999999997780, 1.000000000000000222, 1.000000000000000000, 1.000000000000000000, 1.000000000000000000, 1.000000000000000000, 1.000000000000000222, 1.000000000000000222, 0.9999999999999997780, 1.000000000000000222, 1.000000000000000000, 1.000000000000000222, 0.9999999999999997780, 1.000000000000000222, 1.000000000000000000, 1.000000000000000000, 0.9999999999999997780, 1.000000000000000000, 1.000000000000000000, 0.9999999999999997780, 1.000000000000000222, 0.9999999999999997780, 1.000000000000000222, 0.9999999999999997780, 1.000000000000000444, 1.000000000000000000, 0.9999999999999996669, 1.000000000000000444, 1.000000000000000000, 0.9999999999999997780, 1.000000000000000000, 0.9999999999999996669, 1.000000000000000000, 1.000000000000000222, 0.9999999999999996669, 1.000000000000000222, 0.9999999999999997780, 1.000000000000000000, 1.000000000000000222, 0.9999999999999997780, 1.000000000000000222, 0.9999999999999997780, 1.000000000000000222, 1.000000000000000000, 1.000000000000000000, 1.000000000000000000, 0.9999999999999997780, 1.000000000000000222, 0.9999999999999997780, 1.000000000000000222, 1.000000000000000000, 1.000000000000000000, 1.000000000000000000, 1.000000000000000000, 1.000000000000000444, 0.9999999999999997780, 1.000000000000000444, 0.9999999999999997780, 1.000000000000000222, 1.000000000000000000, 1.000000000000000000, 1.000000000000000000, 1.000000000000000000, 0.9999999999999997780, 1.000000000000000000, 1.000000000000000222, 0.9999999999999997780, 1.000000000000000222, 1.000000000000000000, 1.000000000000000000, 1.000000000000000222, 0.9999999999999997780, 1.000000000000000222, 0.9999999999999996669, 1.000000000000000444, 0.9999999999999994449, 1.000000000000000444, 0.9999999999999997780, 0.9999999999999997780, 1.000000000000000000, 1.000000000000000000, 1.000000000000000222, 1.000000000000000000, 1.000000000000000000, 1.000000000000000000, 1.000000000000000000, 1.000000000000000222, 1.000000000000000444, 0.9999999999999997780, 1.000000000000000222, 1.000000000000000000, 0.9999999999999996669, 1.000000000000000222, 1.000000000000000222, 1.000000000000000222, 1.000000000000000222, 1.000000000000000000, 1.000000000000000000, 1.000000000000000222, 1.000000000000000000, 1.000000000000000222, 1.000000000000000000, 1.000000000000000000, 1.000000000000000000, 1.000000000000000222, 0.9999999999999997780, 1.000000000000000000, 1.000000000000000222, 1.000000000000000000, 1.000000000000000222, 1.000000000000000000, 0.9999999999999997780, 1.000000000000000444, 1.000000000000000000, 0.9999999999999996669, 1.000000000000000222, 0.9999999999999997780, 1.000000000000000222, 1.000000000000000000, 1.000000000000000000, 1.000000000000000444, 0.9999999999999996669, 1.000000000000000000, 0.9999999999999997780, 1.000000000000000000, 0.9999999999999997780, 0.9999999999999997780, 1.000000000000000000, 1.000000000000000000, 1.000000000000000000, 0.9999999999999997780, 1.000000000000000000, 1.000000000000000222, 1.000000000000000222, 1.000000000000000000, 0.9999999999999997780, 1.000000000000000222, 1.000000000000000000, 1.000000000000000000, 1.000000000000000222, 1.000000000000000222, 1.000000000000000222, 1.000000000000000000, 0.9999999999999997780, 1.000000000000000444, 0.9999999999999997780, 1.000000000000000444, 0.9999999999999997780, 1.000000000000000000, 1.000000000000000222, 0.9999999999999997780, 1.000000000000000222, 0.9999999999999997780, 1.000000000000000222, 0.9999999999999997780, 1.000000000000000222, 0.9999999999999996669, 1.000000000000000222, 0.9999999999999997780, 1.000000000000000444, 1.000000000000000000, 1.000000000000000000, 0.9999999999999997780, 1.000000000000000222, 1.000000000000000000, 0.9999999999999996669, 1.000000000000000222, 0.9999999999999997780, 1.000000000000000000, 1.000000000000000222, 1.000000000000000000, 1.000000000000000222, 0.9999999999999996669, 1.000000000000000444, 0.9999999999999996669, 1.000000000000000000, 1.000000000000000000, 1.000000000000000000, 0.9999999999999997780, 1.000000000000000444, 1.000000000000000000, 1.000000000000000000, 1.000000000000000000, 1.000000000000000000, 0.9999999999999997780, 1.000000000000000222, 1.000000000000000222, 1.000000000000000222, 1.000000000000000000, 1.000000000000000222, 1.000000000000000000, 0.9999999999999997780, 1.000000000000000444, 1.000000000000000000, 0.9999999999999997780, 1.000000000000000222, 0.9999999999999996669, 1.000000000000000222, 1.000000000000000000, 1.000000000000000444, 1.000000000000000222, 0.9999999999999996669, 1.000000000000000222, 0.9999999999999997780, 1.000000000000000222, 1.000000000000000222, 0.9999999999999997780, 1.000000000000000222, 1.000000000000000000, 1.000000000000000222, 1.000000000000000222, 0.9999999999999997780, 1.000000000000000444, 0.9999999999999996669, 1.000000000000000222, 1.000000000000000222, 1.000000000000000000, 1.000000000000000000, 1.000000000000000000, 1.000000000000000222, 1.000000000000000000, 1.000000000000000000, 1.000000000000000222, 0.9999999999999996669, 1.000000000000000444, 1.000000000000000222, 0.9999999999999997780, 1.000000000000000222, 0.9999999999999997780, 1.000000000000000444, 0.9999999999999996669, 1.000000000000000666, 0.9999999999999994449, 1.000000000000000222, 0.9999999999999997780, 1.000000000000000444, 1.000000000000000000, 1.000000000000000222, 1.000000000000000222, 1.000000000000000000, 0.9999999999999997780, 0.9999999999999997780, 1.000000000000000444, 1.000000000000000000, 1.000000000000000000, 1.000000000000000000, 0.9999999999999997780, 1.000000000000000222, 1.000000000000000222, 0.9999999999999997780, 1.000000000000000222, 1.000000000000000000, 1.000000000000000444, 0.9999999999999996669, 1.000000000000000444, 0.9999999999999997780, 1.000000000000000000, 0.9999999999999997780, 1.000000000000000444, 0.9999999999999996669, 1.000000000000000444, 1.000000000000000000, 1.000000000000000000, 1.000000000000000000, 0.9999999999999997780, 1.000000000000000444, 1.000000000000000222, 0.9999999999999997780, 1.000000000000000444, 1.000000000000000000, 0.9999999999999996669, 1.000000000000000444, 1.000000000000000000, 1.000000000000000000, 1.000000000000000000, 0.9999999999999997780, 1.000000000000000222, 0.9999999999999997780, 1.000000000000000000, 1.000000000000000222, 0.9999999999999997780, 1.000000000000000000, 1.000000000000000000, 0.9999999999999997780, 1.000000000000000444, 0.9999999999999997780, 1.000000000000000444, 0.9999999999999994449, 1.000000000000000444, 0.9999999999999997780, 1.000000000000000444, 0.9999999999999997780, 1.000000000000000000, 0.9999999999999997780, 1.000000000000000222, 1.000000000000000222, 1.000000000000000000, 1.000000000000000000),
 ( 0.3333333333333333703, 0.3333333333333333703, 0.3333333333333333703, 0.3333333333333335369, 0.3333333333333333148, 0.3333333333333333703, 0.3333333333333333703, 0.3333333333333333148, 0.3333333333333333148, 0.3333333333333334259, 0.3333333333333333703, 0.3333333333333333148, 0.3333333333333334259, 0.3333333333333333148, 0.3333333333333334259, 0.3333333333333333148, 0.3333333333333333703, 0.3333333333333333148, 0.3333333333333334814, 0.3333333333333333148, 0.3333333333333334814, 0.3333333333333334814, 0.3333333333333333148, 0.3333333333333334259, 0.3333333333333333148, 0.3333333333333333703, 0.3333333333333333148, 0.3333333333333334814, 0.3333333333333333703, 0.3333333333333333703, 0.3333333333333333703, 0.3333333333333334259, 0.3333333333333333148, 0.3333333333333333148, 0.3333333333333334259, 0.3333333333333333703, 0.3333333333333334259, 0.3333333333333334259, 0.3333333333333332038, 0.3333333333333334814, 0.3333333333333333703, 0.3333333333333334814, 0.3333333333333332593, 0.3333333333333334259, 0.3333333333333333703, 0.3333333333333334259, 0.3333333333333333148, 0.3333333333333333703, 0.3333333333333334259, 0.3333333333333333148, 0.3333333333333332038, 0.3333333333333335369, 0.3333333333333332593, 0.3333333333333334814, 0.3333333333333333148, 0.3333333333333333703, 0.3333333333333334259, 0.3333333333333333703, 0.3333333333333334814, 0.3333333333333333703, 0.3333333333333334259, 0.3333333333333333148, 0.3333333333333334814, 0.3333333333333332038, 0.3333333333333334259, 0.3333333333333333148, 0.3333333333333333703, 0.3333333333333333703, 0.3333333333333334259, 0.3333333333333333148, 0.3333333333333333703, 0.3333333333333334259, 0.3333333333333333148, 0.3333333333333333703, 0.3333333333333333703, 0.3333333333333335369, 0.3333333333333333148, 0.3333333333333333703, 0.3333333333333333703, 0.3333333333333333703, 0.3333333333333333148, 0.3333333333333333703, 0.3333333333333334814, 0.3333333333333333148, 0.3333333333333334814, 0.3333333333333333703, 0.3333333333333334259, 0.3333333333333333148, 0.3333333333333334259, 0.3333333333333333148, 0.3333333333333334259, 0.3333333333333333148, 0.3333333333333333703, 0.3333333333333333703, 0.3333333333333333703, 0.3333333333333334259, 0.3333333333333334259, 0.3333333333333332593, 0.3333333333333334259, 0.3333333333333333703, 0.3333333333333334259, 0.3333333333333333148, 0.3333333333333334259, 0.3333333333333333703, 0.3333333333333333703, 0.3333333333333333148, 0.3333333333333334259, 0.3333333333333333703, 0.3333333333333333148, 0.3333333333333334259, 0.3333333333333332038, 0.3333333333333334814, 0.3333333333333333148, 0.3333333333333335369, 0.3333333333333334259, 0.3333333333333332038, 0.3333333333333334814, 0.3333333333333333703, 0.3333333333333332593, 0.3333333333333333703, 0.3333333333333332593, 0.3333333333333333703, 0.3333333333333334814, 0.3333333333333333148, 0.3333333333333334814, 0.3333333333333333148, 0.3333333333333334259, 0.3333333333333334259, 0.3333333333333333148, 0.3333333333333334259, 0.3333333333333333148, 0.3333333333333334259, 0.3333333333333333703, 0.3333333333333333703, 0.3333333333333334259, 0.3333333333333332593, 0.3333333333333334814, 0.3333333333333333148, 0.3333333333333333703, 0.3333333333333333703, 0.3333333333333333703, 0.3333333333333334259, 0.3333333333333334259, 0.3333333333333334814, 0.3333333333333333703, 0.3333333333333334259, 0.3333333333333333703, 0.3333333333333333703, 0.3333333333333333148, 0.3333333333333333703, 0.3333333333333334259, 0.3333333333333333148, 0.3333333333333333148, 0.3333333333333333148, 0.3333333333333334259, 0.3333333333333333148, 0.3333333333333334814, 0.3333333333333333148, 0.3333333333333334259, 0.3333333333333334259, 0.3333333333333333148, 0.3333333333333334814, 0.3333333333333333148, 0.3333333333333334814, 0.3333333333333332593, 0.3333333333333335369, 0.3333333333333333148, 0.3333333333333333703, 0.3333333333333333703, 0.3333333333333334259, 0.3333333333333333703, 0.3333333333333333703, 0.3333333333333333148, 0.3333333333333333703, 0.3333333333333332593, 0.3333333333333335369, 0.3333333333333334259, 0.3333333333333333703, 0.3333333333333334259, 0.3333333333333334259, 0.3333333333333332038, 0.3333333333333334814, 0.3333333333333333703, 0.3333333333333334259, 0.3333333333333333703, 0.3333333333333333703, 0.3333333333333333148, 0.3333333333333334814, 0.3333333333333333148, 0.3333333333333334814, 0.3333333333333334259, 0.3333333333333333148, 0.3333333333333333703, 0.3333333333333333703, 0.3333333333333333703, 0.3333333333333333703, 0.3333333333333334259, 0.3333333333333333148, 0.3333333333333334814, 0.3333333333333333148, 0.3333333333333333703, 0.3333333333333334814, 0.3333333333333332593, 0.3333333333333333148, 0.3333333333333334259, 0.3333333333333332593, 0.3333333333333335369, 0.3333333333333333703, 0.3333333333333334259, 0.3333333333333335369, 0.3333333333333333148, 0.3333333333333333703, 0.3333333333333333148, 0.3333333333333333703, 0.3333333333333333148, 0.3333333333333333148, 0.3333333333333333703, 0.3333333333333333703, 0.3333333333333333703, 0.3333333333333333148, 0.3333333333333333703, 0.3333333333333333703, 0.3333333333333334259, 0.3333333333333333703, 0.3333333333333333148, 0.3333333333333333703, 0.3333333333333333703, 0.3333333333333333703, 0.3333333333333334259, 0.3333333333333334259, 0.3333333333333334814, 0.3333333333333332593, 0.3333333333333334259, 0.3333333333333334259, 0.3333333333333333148, 0.3333333333333334259, 0.3333333333333333703, 0.3333333333333333148, 0.3333333333333334814, 0.3333333333333333703, 0.3333333333333334259, 0.3333333333333332593, 0.3333333333333334259, 0.3333333333333332593, 0.3333333333333334814, 0.3333333333333332593, 0.3333333333333334259, 0.3333333333333333148, 0.3333333333333334259, 0.3333333333333333703, 0.3333333333333334259, 0.3333333333333333703, 0.3333333333333333703, 0.3333333333333333703, 0.3333333333333333148, 0.3333333333333334259, 0.3333333333333333703, 0.3333333333333333148, 0.3333333333333334259, 0.3333333333333333148, 0.3333333333333333703, 0.3333333333333333148, 0.3333333333333334814, 0.3333333333333332593, 0.3333333333333333703, 0.3333333333333333703, 0.3333333333333334259, 0.3333333333333332593, 0.3333333333333335369, 0.3333333333333333703, 0.3333333333333333703, 0.3333333333333333703, 0.3333333333333333148, 0.3333333333333333148, 0.3333333333333334259, 0.3333333333333334814, 0.3333333333333334259, 0.3333333333333333703, 0.3333333333333334259, 0.3333333333333334259, 0.3333333333333333703, 0.3333333333333334814, 0.3333333333333333148, 0.3333333333333333148, 0.3333333333333334259, 0.3333333333333332038, 0.3333333333333334814, 0.3333333333333333148, 0.3333333333333335369, 0.3333333333333334259, 0.3333333333333333148, 0.3333333333333334814, 0.3333333333333333703, 0.3333333333333333703, 0.3333333333333334259, 0.3333333333333333703, 0.3333333333333334259, 0.3333333333333333703, 0.3333333333333334259, 0.3333333333333333148, 0.3333333333333333703, 0.3333333333333335369, 0.3333333333333332038, 0.3333333333333334814, 0.3333333333333333703, 0.3333333333333333148, 0.3333333333333334259, 0.3333333333333333703, 0.3333333333333333148, 0.3333333333333334259, 0.3333333333333333703, 0.3333333333333334259, 0.3333333333333332593, 0.3333333333333335369, 0.3333333333333334814, 0.3333333333333333148, 0.3333333333333334259, 0.3333333333333333148, 0.3333333333333335369, 0.3333333333333332593, 0.3333333333333335924, 0.3333333333333332593, 0.3333333333333333703, 0.3333333333333333703, 0.3333333333333334814, 0.3333333333333333703, 0.3333333333333334814, 0.3333333333333333703, 0.3333333333333334259, 0.3333333333333332593, 0.3333333333333334259, 0.3333333333333335369, 0.3333333333333333148, 0.3333333333333334814, 0.3333333333333333148, 0.3333333333333333703, 0.3333333333333334259, 0.3333333333333334259, 0.3333333333333332593, 0.3333333333333334259, 0.3333333333333333148, 0.3333333333333335369, 0.3333333333333332593, 0.3333333333333335369, 0.3333333333333333148, 0.3333333333333333148, 0.3333333333333333703, 0.3333333333333334814, 0.3333333333333333148, 0.3333333333333334259, 0.3333333333333333148, 0.3333333333333334259, 0.3333333333333333703, 0.3333333333333333148, 0.3333333333333334259, 0.3333333333333334814, 0.3333333333333333148, 0.3333333333333334814, 0.3333333333333333703, 0.3333333333333332593, 0.3333333333333334259, 0.3333333333333333703, 0.3333333333333334259, 0.3333333333333333703, 0.3333333333333333148, 0.3333333333333334259, 0.3333333333333333703, 0.3333333333333333148, 0.3333333333333334259, 0.3333333333333333148, 0.3333333333333333148, 0.3333333333333333703, 0.3333333333333333703, 0.3333333333333334259, 0.3333333333333333148, 0.3333333333333334259, 0.3333333333333332593, 0.3333333333333334259, 0.3333333333333333703, 0.3333333333333334259, 0.3333333333333333703, 0.3333333333333333703, 0.3333333333333333148, 0.3333333333333334814, 0.3333333333333334259, 0.3333333333333333703, 0.3333333333333333703),
 ( 0.3333333333333333703, 0.3333333333333333703, 0.3333333333333333703, 0.3333333333333335369, 0.3333333333333333148, 0.3333333333333333703, 0.3333333333333333703, 0.3333333333333333148, 0.3333333333333333148, 0.3333333333333334259, 0.3333333333333333703, 0.3333333333333333148, 0.3333333333333334259, 0.3333333333333333148, 0.3333333333333334259, 0.3333333333333333148, 0.3333333333333333703, 0.3333333333333333148, 0.3333333333333334814, 0.3333333333333333148, 0.3333333333333334814, 0.3333333333333334814, 0.3333333333333333148, 0.3333333333333334259, 0.3333333333333333148, 0.3333333333333333703, 0.3333333333333333148, 0.3333333333333334814, 0.3333333333333333703, 0.3333333333333333703, 0.3333333333333333703, 0.3333333333333334259, 0.3333333333333333148, 0.3333333333333333148, 0.3333333333333334259, 0.3333333333333333703, 0.3333333333333334259, 0.3333333333333334259, 0.3333333333333332038, 0.3333333333333334814, 0.3333333333333333703, 0.3333333333333334814, 0.3333333333333332593, 0.3333333333333334259, 0.3333333333333333703, 0.3333333333333334259, 0.3333333333333333148, 0.3333333333333333703, 0.3333333333333334259, 0.3333333333333333148, 0.3333333333333332038, 0.3333333333333335369, 0.3333333333333332593, 0.3333333333333334814, 0.3333333333333333148, 0.3333333333333333703, 0.3333333333333334259, 0.3333333333333333703, 0.3333333333333334814, 0.3333333333333333703, 0.3333333333333334259, 0.3333333333333333148, 0.3333333333333334814, 0.3333333333333332038, 0.3333333333333334259, 0.3333333333333333148, 0.3333333333333333703, 0.3333333333333333703, 0.3333333333333334259, 0.3333333333333333148, 0.3333333333333333703, 0.3333333333333334259, 0.3333333333333333148, 0.3333333333333333703, 0.3333333333333333703, 0.3333333333333335369, 0.3333333333333333148, 0.3333333333333333703, 0.3333333333333333703, 0.3333333333333333703, 0.3333333333333333148, 0.3333333333333333703, 0.3333333333333334814, 0.3333333333333333148, 0.3333333333333334814, 0.3333333333333333703, 0.3333333333333334259, 0.3333333333333333148, 0.3333333333333334259, 0.3333333333333333148, 0.3333333333333334259, 0.3333333333333333148, 0.3333333333333333703, 0.3333333333333333703, 0.3333333333333333703, 0.3333333333333334259, 0.3333333333333334259, 0.3333333333333332593, 0.3333333333333334259, 0.3333333333333333703, 0.3333333333333334259, 0.3333333333333333148, 0.3333333333333334259, 0.3333333333333333703, 0.3333333333333333703, 0.3333333333333333148, 0.3333333333333334259, 0.3333333333333333703, 0.3333333333333333148, 0.3333333333333334259, 0.3333333333333332038, 0.3333333333333334814, 0.3333333333333333148, 0.3333333333333335369, 0.3333333333333334259, 0.3333333333333332038, 0.3333333333333334814, 0.3333333333333333703, 0.3333333333333332593, 0.3333333333333333703, 0.3333333333333332593, 0.3333333333333333703, 0.3333333333333334814, 0.3333333333333333148, 0.3333333333333334814, 0.3333333333333333148, 0.3333333333333334259, 0.3333333333333334259, 0.3333333333333333148, 0.3333333333333334259, 0.3333333333333333148, 0.3333333333333334259, 0.3333333333333333703, 0.3333333333333333703, 0.3333333333333334259, 0.3333333333333332593, 0.3333333333333334814, 0.3333333333333333148, 0.3333333333333333703, 0.3333333333333333703, 0.3333333333333333703, 0.3333333333333334259, 0.3333333333333334259, 0.3333333333333334814, 0.3333333333333333703, 0.3333333333333334259, 0.3333333333333333703, 0.3333333333333333703, 0.3333333333333333148, 0.3333333333333333703, 0.3333333333333334259, 0.3333333333333333148, 0.3333333333333333148, 0.3333333333333333148, 0.3333333333333334259, 0.3333333333333333148, 0.3333333333333334814, 0.3333333333333333148, 0.3333333333333334259, 0.3333333333333334259, 0.3333333333333333148, 0.3333333333333334814, 0.3333333333333333148, 0.3333333333333334814, 0.3333333333333332593, 0.3333333333333335369, 0.3333333333333333148, 0.3333333333333333703, 0.3333333333333333703, 0.3333333333333334259, 0.3333333333333333703, 0.3333333333333333703, 0.3333333333333333148, 0.3333333333333333703, 0.3333333333333332593, 0.3333333333333335369, 0.3333333333333334259, 0.3333333333333333703, 0.3333333333333334259, 0.3333333333333334259, 0.3333333333333332038, 0.3333333333333334814, 0.3333333333333333703, 0.3333333333333334259, 0.3333333333333333703, 0.3333333333333333703, 0.3333333333333333148, 0.3333333333333334814, 0.3333333333333333148, 0.3333333333333334814, 0.3333333333333334259, 0.3333333333333333148, 0.3333333333333333703, 0.3333333333333333703, 0.3333333333333333703, 0.3333333333333333703, 0.3333333333333334259, 0.3333333333333333148, 0.3333333333333334814, 0.3333333333333333148, 0.3333333333333333703, 0.3333333333333334814, 0.3333333333333332593, 0.3333333333333333148, 0.3333333333333334259, 0.3333333333333332593, 0.3333333333333335369, 0.3333333333333333703, 0.3333333333333334259, 0.3333333333333335369, 0.3333333333333333148, 0.3333333333333333703, 0.3333333333333333148, 0.3333333333333333703, 0.3333333333333333148, 0.3333333333333333148, 0.3333333333333333703, 0.3333333333333333703, 0.3333333333333333703, 0.3333333333333333148, 0.3333333333333333703, 0.3333333333333333703, 0.3333333333333334259, 0.3333333333333333703, 0.3333333333333333148, 0.3333333333333333703, 0.3333333333333333703, 0.3333333333333333703, 0.3333333333333334259, 0.3333333333333334259, 0.3333333333333334814, 0.3333333333333332593, 0.3333333333333334259, 0.3333333333333334259, 0.3333333333333333148, 0.3333333333333334259, 0.3333333333333333703, 0.3333333333333333148, 0.3333333333333334814, 0.3333333333333333703, 0.3333333333333334259, 0.3333333333333332593, 0.3333333333333334259, 0.3333333333333332593, 0.3333333333333334814, 0.3333333333333332593, 0.3333333333333334259, 0.3333333333333333148, 0.3333333333333334259, 0.3333333333333333703, 0.3333333333333334259, 0.3333333333333333703, 0.3333333333333333703, 0.3333333333333333703, 0.3333333333333333148, 0.3333333333333334259, 0.3333333333333333703, 0.3333333333333333148, 0.3333333333333334259, 0.3333333333333333148, 0.3333333333333333703, 0.3333333333333333148, 0.3333333333333334814, 0.3333333333333332593, 0.3333333333333333703, 0.3333333333333333703, 0.3333333333333334259, 0.3333333333333332593, 0.3333333333333335369, 0.3333333333333333703, 0.3333333333333333703, 0.3333333333333333703, 0.3333333333333333148, 0.3333333333333333148, 0.3333333333333334259, 0.3333333333333334814, 0.3333333333333334259, 0.3333333333333333703, 0.3333333333333334259, 0.3333333333333334259, 0.3333333333333333703, 0.3333333333333334814, 0.3333333333333333148, 0.3333333333333333148, 0.3333333333333334259, 0.3333333333333332038, 0.3333333333333334814, 0.3333333333333333148, 0.3333333333333335369, 0.3333333333333334259, 0.3333333333333333148, 0.3333333333333334814, 0.3333333333333333703, 0.3333333333333333703, 0.3333333333333334259, 0.3333333333333333703, 0.3333333333333334259, 0.3333333333333333703, 0.3333333333333334259, 0.3333333333333333148, 0.3333333333333333703, 0.3333333333333335369, 0.3333333333333332038, 0.3333333333333334814, 0.3333333333333333703, 0.3333333333333333148, 0.3333333333333334259, 0.3333333333333333703, 0.3333333333333333148, 0.3333333333333334259, 0.3333333333333333703, 0.3333333333333334259, 0.3333333333333332593, 0.3333333333333335369, 0.3333333333333334814, 0.3333333333333333148, 0.3333333333333334259, 0.3333333333333333148, 0.3333333333333335369, 0.3333333333333332593, 0.3333333333333335924, 0.3333333333333332593, 0.3333333333333333703, 0.3333333333333333703, 0.3333333333333334814, 0.3333333333333333703, 0.3333333333333334814, 0.3333333333333333703, 0.3333333333333334259, 0.3333333333333332593, 0.3333333333333334259, 0.3333333333333335369, 0.3333333333333333148, 0.3333333333333334814, 0.3333333333333333148, 0.3333333333333333703, 0.3333333333333334259, 0.3333333333333334259, 0.3333333333333332593, 0.3333333333333334259, 0.3333333333333333148, 0.3333333333333335369, 0.3333333333333332593, 0.3333333333333335369, 0.3333333333333333148, 0.3333333333333333148, 0.3333333333333333703, 0.3333333333333334814, 0.3333333333333333148, 0.3333333333333334259, 0.3333333333333333148, 0.3333333333333334259, 0.3333333333333333703, 0.3333333333333333148, 0.3333333333333334259, 0.3333333333333334814, 0.3333333333333333148, 0.3333333333333334814, 0.3333333333333333703, 0.3333333333333332593, 0.3333333333333334259, 0.3333333333333333703, 0.3333333333333334259, 0.3333333333333333703, 0.3333333333333333148, 0.3333333333333334259, 0.3333333333333333703, 0.3333333333333333148, 0.3333333333333334259, 0.3333333333333333148, 0.3333333333333333148, 0.3333333333333333703, 0.3333333333333333703, 0.3333333333333334259, 0.3333333333333333148, 0.3333333333333334259, 0.3333333333333332593, 0.3333333333333334259, 0.3333333333333333703, 0.3333333333333334259, 0.3333333333333333703, 0.3333333333333333703, 0.3333333333333333148, 0.3333333333333334814, 0.3333333333333334259, 0.3333333333333333703, 0.3333333333333333703),
 ( 1.000000000000000000, 1.000000000000000000, 1.000000000000000000, 1.000000000000000222, 0.9999999999999996669, 1.000000000000000222, 0.9999999999999997780, 1.000000000000000000, 0.9999999999999997780, 1.000000000000000444, 1.000000000000000000, 0.9999999999999997780, 1.000000000000000222, 1.000000000000000000, 0.9999999999999997780, 1.000000000000000222, 0.9999999999999996669, 1.000000000000000000, 1.000000000000000222, 1.000000000000000000, 1.000000000000000000, 1.000000000000000444, 0.9999999999999994449, 1.000000000000000444, 0.9999999999999996669, 1.000000000000000222, 1.000000000000000000, 1.000000000000000444, 1.000000000000000000, 0.9999999999999997780, 1.000000000000000000, 1.000000000000000222, 0.9999999999999997780, 0.9999999999999997780, 1.000000000000000444, 0.9999999999999997780, 1.000000000000000444, 1.000000000000000222, 0.9999999999999996669, 1.000000000000000222, 1.000000000000000000, 1.000000000000000444, 0.9999999999999997780, 1.000000000000000222, 1.000000000000000222, 1.000000000000000222, 0.9999999999999997780, 1.000000000000000000, 1.000000000000000000, 1.000000000000000000, 0.9999999999999994449, 1.000000000000000444, 0.9999999999999997780, 1.000000000000000444, 0.9999999999999997780, 1.000000000000000000, 1.000000000000000000, 0.9999999999999997780, 1.000000000000000444, 0.9999999999999996669, 1.000000000000000444, 0.9999999999999996669, 1.000000000000000222, 0.9999999999999994449, 1.000000000000000222, 1.000000000000000000, 1.000000000000000000, 1.000000000000000000, 1.000000000000000000, 1.000000000000000222, 1.000000000000000000, 1.000000000000000222, 0.9999999999999996669, 1.000000000000000222, 1.000000000000000000, 1.000000000000000444, 1.000000000000000000, 1.000000000000000000, 0.9999999999999997780, 1.000000000000000222, 0.9999999999999997780, 0.9999999999999997780, 1.000000000000000444, 1.000000000000000000, 1.000000000000000222, 0.9999999999999996669, 1.000000000000000444, 0.9999999999999997780, 1.000000000000000222, 0.9999999999999997780, 1.000000000000000222, 1.000000000000000000, 1.000000000000000000, 1.000000000000000000, 1.000000000000000000, 1.000000000000000222, 1.000000000000000222, 0.9999999999999997780, 1.000000000000000222, 1.000000000000000000, 1.000000000000000222, 0.9999999999999997780, 1.000000000000000222, 1.000000000000000000, 1.000000000000000000, 0.9999999999999997780, 1.000000000000000000, 1.000000000000000000, 0.9999999999999997780, 1.000000000000000222, 0.9999999999999997780, 1.000000000000000222, 0.9999999999999997780, 1.000000000000000444, 1.000000000000000000, 0.9999999999999996669, 1.000000000000000444, 1.000000000000000000, 0.9999999999999997780, 1.000000000000000000, 0.9999999999999996669, 1.000000000000000000, 1.000000000000000222, 0.9999999999999996669, 1.000000000000000222, 0.9999999999999997780, 1.000000000000000000, 1.000000000000000222, 0.9999999999999997780, 1.000000000000000222, 0.9999999999999997780, 1.000000000000000222, 1.000000000000000000, 1.000000000000000000, 1.000000000000000000, 0.9999999999999997780, 1.000000000000000222, 0.9999999999999997780, 1.000000000000000222, 1.000000000000000000, 1.000000000000000000, 1.000000000000000000, 1.000000000000000000, 1.000000000000000444, 0.9999999999999997780, 1.000000000000000444, 0.9999999999999997780, 1.000000000000000222, 1.000000000000000000, 1.000000000000000000, 1.000000000000000000, 1.000000000000000000, 0.9999999999999997780, 1.000000000000000000, 1.000000000000000222, 0.9999999999999997780, 1.000000000000000222, 1.000000000000000000, 1.000000000000000000, 1.000000000000000222, 0.9999999999999997780, 1.000000000000000222, 0.9999999999999996669, 1.000000000000000444, 0.9999999999999994449, 1.000000000000000444, 0.9999999999999997780, 0.9999999999999997780, 1.000000000000000000, 1.000000000000000000, 1.000000000000000222, 1.000000000000000000, 1.000000000000000000, 1.000000000000000000, 1.000000000000000000, 1.000000000000000222, 1.000000000000000444, 0.9999999999999997780, 1.000000000000000222, 1.000000000000000000, 0.9999999999999996669, 1.000000000000000222, 1.000000000000000222, 1.000000000000000222, 1.000000000000000222, 1.000000000000000000, 1.000000000000000000, 1.000000000000000222, 1.000000000000000000, 1.000000000000000222, 1.000000000000000000, 1.000000000000000000, 1.000000000000000000, 1.000000000000000222, 0.9999999999999997780, 1.000000000000000000, 1.000000000000000222, 1.000000000000000000, 1.000000000000000222, 1.000000000000000000, 0.9999999999999997780, 1.000000000000000444, 1.000000000000000000, 0.9999999999999996669, 1.000000000000000222, 0.9999999999999997780, 1.000000000000000222, 1.000000000000000000, 1.000000000000000000, 1.000000000000000444, 0.9999999999999996669, 1.000000000000000000, 0.9999999999999997780, 1.000000000000000000, 0.9999999999999997780, 0.9999999999999997780, 1.000000000000000000, 1.000000000000000000, 1.000000000000000000, 0.9999999999999997780, 1.000000000000000000, 1.000000000000000222, 1.000000000000000222, 1.000000000000000000, 0.9999999999999997780, 1.000000000000000222, 1.000000000000000000, 1.000000000000000000, 1.000000000000000222, 1.000000000000000222, 1.000000000000000222, 1.000000000000000000, 0.9999999999999997780, 1.000000000000000444, 0.9999999999999997780, 1.000000000000000444, 0.9999999999999997780, 1.000000000000000000, 1.000000000000000222, 0.9999999999999997780, 1.000000000000000222, 0.9999999999999997780, 1.000000000000000222, 0.9999999999999997780, 1.000000000000000222, 0.9999999999999996669, 1.000000000000000222, 0.9999999999999997780, 1.000000000000000444, 1.000000000000000000, 1.000000000000000000, 0.9999999999999997780, 1.000000000000000222, 1.000000000000000000, 0.9999999999999996669, 1.000000000000000222, 0.9999999999999997780, 1.000000000000000000, 1.000000000000000222, 1.000000000000000000, 1.000000000000000222, 0.9999999999999996669, 1.000000000000000444, 0.9999999999999996669, 1.000000000000000000, 1.000000000000000000, 1.000000000000000000, 0.9999999999999997780, 1.000000000000000444, 1.000000000000000000, 1.000000000000000000, 1.000000000000000000, 1.000000000000000000, 0.9999999999999997780, 1.000000000000000222, 1.000000000000000222, 1.000000000000000222, 1.000000000000000000, 1.000000000000000222, 1.000000000000000000, 0.9999999999999997780, 1.000000000000000444, 1.000000000000000000, 0.9999999999999997780, 1.000000000000000222, 0.9999999999999996669, 1.000000000000000222, 1.000000000000000000, 1.000000000000000444, 1.000000000000000222, 0.9999999999999996669, 1.000000000000000222, 0.9999999999999997780, 1.000000000000000222, 1.000000000000000222, 0.9999999999999997780, 1.000000000000000222, 1.000000000000000000, 1.000000000000000222, 1.000000000000000222, 0.9999999999999997780, 1.000000000000000444, 0.9999999999999996669, 1.000000000000000222, 1.000000000000000222, 1.000000000000000000, 1.000000000000000000, 1.000000000000000000, 1.000000000000000222, 1.000000000000000000, 1.000000000000000000, 1.000000000000000222, 0.9999999999999996669, 1.000000000000000444, 1.000000000000000222, 0.9999999999999997780, 1.000000000000000222, 0.9999999999999997780, 1.000000000000000444, 0.9999999999999996669, 1.000000000000000666, 0.9999999999999994449, 1.000000000000000222, 0.9999999999999997780, 1.000000000000000444, 1.000000000000000000, 1.000000000000000222, 1.000000000000000222, 1.000000000000000000, 0.9999999999999997780, 0.9999999999999997780, 1.000000000000000444, 1.000000000000000000, 1.000000000000000000, 1.000000000000000000, 0.9999999999999997780, 1.000000000000000222, 1.000000000000000222, 0.9999999999999997780, 1.000000000000000222, 1.000000000000000000, 1.000000000000000444, 0.9999999999999996669, 1.000000000000000444, 0.9999999999999997780, 1.000000000000000000, 0.9999999999999997780, 1.000000000000000444, 0.9999999999999996669, 1.000000000000000444, 1.000000000000000000, 1.000000000000000000, 1.000000000000000000, 0.9999999999999997780, 1.000000000000000444, 1.000000000000000222, 0.9999999999999997780, 1.000000000000000444, 1.000000000000000000, 0.9999999999999996669, 1.000000000000000444, 1.000000000000000000, 1.000000000000000000, 1.000000000000000000, 0.9999999999999997780, 1.000000000000000222, 0.9999999999999997780, 1.000000000000000000, 1.000000000000000222, 0.9999999999999997780, 1.000000000000000000, 1.000000000000000000, 0.9999999999999997780, 1.000000000000000444, 0.9999999999999997780, 1.000000000000000444, 0.9999999999999994449, 1.000000000000000444, 0.9999999999999997780, 1.000000000000000444, 0.9999999999999997780, 1.000000000000000000, 0.9999999999999997780, 1.000000000000000222, 1.000000000000000222, 1.000000000000000000, 1.000000000000000000) ) ) 
 REPRESENTATION_ITEM ( '' )  SURFACE ( )  );
#39774 = CARTESIAN_POINT ( 'NONE',  ( 3.661125528703466525, 1.714762188600306825, -1.331539952715065978 ) ) ;
#39775 = CARTESIAN_POINT ( 'NONE',  ( 2.209345402013741300, -0.4006574107652469130, 1.781019818369505847 ) ) ;
#39776 = CARTESIAN_POINT ( 'NONE',  ( 0.000000000000000000, 0.03624871340549007392, -6.329999999999995630 ) ) ;
#39777 = CARTESIAN_POINT ( 'NONE',  ( 4.575475080723796495, 1.571334676144776621, 1.419386683734702226 ) ) ;
#39778 = ORIENTED_EDGE ( 'NONE', *, *, #153901, .F. ) ;
#39780 = CARTESIAN_POINT ( 'NONE',  ( -1.364683531250014514, 1.051041667008090208, -0.7879004041258289570 ) ) ;
#39779 = CARTESIAN_POINT ( 'NONE',  ( 4.722401423535961484, 2.193339426362813871, 0.6665824366990577010 ) ) ;
#39781 = CARTESIAN_POINT ( 'NONE',  ( 0.07755575628181145265, 0.2276780653837663093, -2.222404768597835201 ) ) ;
#39782 = CARTESIAN_POINT ( 'NONE',  ( 2.703961570921634028, 5.242040035128820108, -1.199719254218446718 ) ) ;
#39783 = EDGE_CURVE ( 'NONE', #41218, #176198, #85972, .T. ) ;
#39784 = CARTESIAN_POINT ( 'NONE',  ( 0.1180496341894651385, -0.5612577129426484790, 2.044807062438446454 ) ) ;
#39785 = CARTESIAN_POINT ( 'NONE',  ( -5.748293942514186128, 6.769059690097084747, -1.082531754730544860 ) ) ;
#39786 = CARTESIAN_POINT ( 'NONE',  ( 3.199361063144961825, 6.676412307070352270, -0.7216878364870267237 ) ) ;
#39787 = CARTESIAN_POINT ( 'NONE',  ( -6.033015167956805591, 8.061603667414825480, -1.443375672974058777 ) ) ;
#39788 = CARTESIAN_POINT ( 'NONE',  ( 3.106226591306694651, 6.638031766584184368, 0.000000000000000000 ) ) ;
#39789 = VERTEX_POINT ( 'NONE', #96138 ) ;
#39790 = CARTESIAN_POINT ( 'NONE',  ( 5.203750078570229753, 1.864167652161516031, 0.7691231355932278690 ) ) ;
#39792 = CARTESIAN_POINT ( 'NONE',  ( 3.801677422522796945, -1.558724286948458548, -1.350822056805228266 ) ) ;
#39791 = CARTESIAN_POINT ( 'NONE',  ( 6.498435699651741615, 6.475929825882159818, -0.7998128361456281477 ) ) ;
#39794 = CARTESIAN_POINT ( 'NONE',  ( -0.2408018239684278916, 2.008845716682732263, -2.515352618630611659 ) ) ;
#39793 = DIRECTION ( 'NONE',  ( 0.000000000000000000, 1.000000000000000000, 0.000000000000000000 ) ) ;
#39795 = CARTESIAN_POINT ( 'NONE',  ( 4.136646265500957043, 5.919449624541475607, -1.443375672974068769 ) ) ;
#39796 = CARTESIAN_POINT ( 'NONE',  ( 0.000000000000000000, -1.246874999522042948, -3.793834371823813001 ) ) ;
#39797 = DIRECTION ( 'NONE',  ( -0.000000000000000000, -0.000000000000000000, 1.000000000000000000 ) ) ;
#39798 = CARTESIAN_POINT ( 'NONE',  ( 5.999973295341066937, -0.7855225714627244171, -2.046000194487001433 ) ) ;
#39799 = CARTESIAN_POINT ( 'NONE',  ( 3.217422812353257555, 1.967887761762876941, 0.4390297752325384995 ) ) ;
#39800 = CARTESIAN_POINT ( 'NONE',  ( 3.825598141381767903, 0.9817388958630569595, -1.557492293685861284 ) ) ;
#39801 = CARTESIAN_POINT ( 'NONE',  ( 6.667912619822566000, 6.673652899414787676, 1.040834085586084257E-14 ) ) ;
#39803 = EDGE_CURVE ( 'NONE', #49550, #130236, #200051, .T. ) ;
#39802 = FILL_AREA_STYLE_COLOUR ( '', #165964 ) ;
#39804 = CARTESIAN_POINT ( 'NONE',  ( 1.043494860557155679, 0.7046062621528689229, -1.574481895975497592 ) ) ;
#39805 = CARTESIAN_POINT ( 'NONE',  ( 4.028709946750490545, 3.988235255965033588, -0.8025987720412866011 ) ) ;
#39806 = CARTESIAN_POINT ( 'NONE',  ( 0.4054594355042361875, -1.236789717346518769, -1.937488090237641014 ) ) ;
#39807 = CARTESIAN_POINT ( 'NONE',  ( -6.201965203247477909, 9.323044272842313518, 1.199719254218452047 ) ) ;
#39808 = CARTESIAN_POINT ( 'NONE',  ( 6.649321564832020748, -1.812311508879884459, -1.354277771019767762 ) ) ;
#39809 = CARTESIAN_POINT ( 'NONE',  ( 2.262461133243711675, 0.9012960022399997273, 1.903611236745775814 ) ) ;
#39810 = CARTESIAN_POINT ( 'NONE',  ( -6.231907884136888676, 7.299589282028351001, -1.199719254218453823 ) ) ;
#39811 = CARTESIAN_POINT ( 'NONE',  ( 7.263417608619159083, 9.497073181520933716, -1.599625672291262513 ) ) ;
#39812 = CARTESIAN_POINT ( 'NONE',  ( 6.685579144870162693, 6.972466221869550118, -0.7216878364870458196 ) ) ;
#39813 = DIRECTION ( 'NONE',  ( 1.000000000000000000, 0.000000000000000000, -2.220446049250313081E-16 ) ) ;
#39814 = CARTESIAN_POINT ( 'NONE',  ( -7.226659571283968297, 8.389856573708110332, 1.199719254218450271 ) ) ;
#39815 = CARTESIAN_POINT ( 'NONE',  ( 7.754900676892376055, 8.149731665903665601, 1.040834085586084257E-14 ) ) ;
#39816 = CARTESIAN_POINT ( 'NONE',  ( 4.350666953118342839, 7.402852620340107492, 1.136566098749042242 ) ) ;
#39817 = CARTESIAN_POINT ( 'NONE',  ( -3.737243898861318137, 7.511868315313511069, 0.7998128361456341429 ) ) ;
#39818 = CARTESIAN_POINT ( 'NONE',  ( 4.201594209339031494, 1.983332154306137518, -1.000733898520693499 ) ) ;
#39819 = CARTESIAN_POINT ( 'NONE',  ( 2.168174125648382411, -1.346884454587377711, 1.728604079486287137 ) ) ;
#39820 = CARTESIAN_POINT ( 'NONE',  ( -6.762819695118240659, 6.784377820593065600, 0.7998128361456341429 ) ) ;
#39821 = CARTESIAN_POINT ( 'NONE',  ( 0.5048604690408053930, -0.7474223562033958101, -2.076596198196341003 ) ) ;
#39822 = CARTESIAN_POINT ( 'NONE',  ( -4.285259070371116863, 7.157163461145040095, 1.199719254218452935 ) ) ;
#39823 = CARTESIAN_POINT ( 'NONE',  ( 5.142999638377217408, -0.2383176028181442918, -1.947251298587366231 ) ) ;
#39824 = DIRECTION ( 'NONE',  ( -0.8003905296791066215, 0.000000000000000000, -0.5994789404140892231 ) ) ;
#39825 = CARTESIAN_POINT ( 'NONE',  ( -1.364683531250012516, 2.030208333674750953, 0.7879004041258379498 ) ) ;
#39826 = CARTESIAN_POINT ( 'NONE',  ( -4.828112100242294424, 5.765790550771681566, -1.082531754730549967 ) ) ;
#39828 = ORIENTED_EDGE ( 'NONE', *, *, #19530, .T. ) ;
#39827 = CARTESIAN_POINT ( 'NONE',  ( -5.748293942514172805, 8.689798118699771479, -1.082531754730538864 ) ) ;
#39829 = CARTESIAN_POINT ( 'NONE',  ( 4.728832233812888752, 1.460412846248357210, -1.537820402542383169 ) ) ;
#39830 = CARTESIAN_POINT ( 'NONE',  ( -5.147255595043616516, 6.034161611419515125, 1.199719254218452935 ) ) ;
#39831 = ORIENTED_EDGE ( 'NONE', *, *, #161571, .T. ) ;
#39832 = CARTESIAN_POINT ( 'NONE',  ( 5.489210439962995736, 1.908424935776025455, -1.015307555102950010 ) ) ;
#39833 = CARTESIAN_POINT ( 'NONE',  ( 5.198661835836162481, 8.152523677529138979, 1.199719254218462483 ) ) ;
#39834 = CARTESIAN_POINT ( 'NONE',  ( 4.599059095968327071, -0.4863373063577690059, 1.775805238918099382 ) ) ;
#39835 = UNCERTAINTY_MEASURE_WITH_UNIT (LENGTH_MEASURE( 1.000000000000000082E-05 ), #53915, 'distance_accuracy_value', 'NONE');
#39836 = CARTESIAN_POINT ( 'NONE',  ( -5.881612045648562770, 6.018300081020916181, 0.2952277700727298781 ) ) ;
#39837 = CARTESIAN_POINT ( 'NONE',  ( 0.6823417656249882723, 1.238541667008083547, -1.181850606188749264 ) ) ;
#39838 = CARTESIAN_POINT ( 'NONE',  ( -0.05959145049940026140, -1.342969899416647905, -1.106900597494438143 ) ) ;
#39839 = CARTESIAN_POINT ( 'NONE',  ( 6.827182134110246103, 3.705739211453745074, 2.325493694733235195 ) ) ;
#39840 = CARTESIAN_POINT ( 'NONE',  ( -0.3866901564497978727, 3.102326550341739875, 2.027579305719746205 ) ) ;
#39841 = CARTESIAN_POINT ( 'NONE',  ( 11.81905481421901705, 13.75735655617266495, -1.592167362352180149 ) ) ;
#39842 = CARTESIAN_POINT ( 'NONE',  ( 4.540002997438313592, 0.9271085556134452954, -1.952944755896801610 ) ) ;
#39843 = AXIS2_PLACEMENT_3D ( 'NONE', #191579, #40026, #72501 ) ;
#39844 = CARTESIAN_POINT ( 'NONE',  ( -3.601662362724658895, 7.353689856487406473, -0.7998128361456281477 ) ) ;
#39845 = CARTESIAN_POINT ( 'NONE',  ( 6.415388720371407949, 0.6297814698452592896, 1.915305867393565897 ) ) ;
#39846 = CARTESIAN_POINT ( 'NONE',  ( -8.392133896734675247, 10.81390885098904420, 1.443375672974064550 ) ) ;
#39847 = CARTESIAN_POINT ( 'NONE',  ( 3.467792127863758456, 2.109446376165153847, -0.4717452660116944196 ) ) ;
#39848 = CARTESIAN_POINT ( 'NONE',  ( 4.481683897012714191, 1.285251931988955709, 1.494896804799286993 ) ) ;
#39849 = CARTESIAN_POINT ( 'NONE',  ( 3.936634314383654853, 0.9622043370151998065, 1.442083020896669954 ) ) ;
#39850 = AXIS2_PLACEMENT_3D ( 'NONE', #62622, #194762, #112515 ) ;
#39851 = CARTESIAN_POINT ( 'NONE',  ( 0.8201894534925309177, 1.301127354658284663, -1.763390660798454634 ) ) ;
#39852 = CARTESIAN_POINT ( 'NONE',  ( 1.571738265064129836, 0.1679657064320304316, -2.301541284809864862 ) ) ;
#39853 = CARTESIAN_POINT ( 'NONE',  ( 3.550122082181893290, 2.060967561582152108, 0.003633429623469893420 ) ) ;
#39854 = CARTESIAN_POINT ( 'NONE',  ( 6.198774611348529362, 1.617120784385807974, 1.075137550886333004 ) ) ;
#39855 = CARTESIAN_POINT ( 'NONE',  ( -7.876924059415400414, 9.252461493148505411, 1.082531754730558626 ) ) ;
#39856 = CARTESIAN_POINT ( 'NONE',  ( -5.306037014901836990, 7.283738832175834510, 1.599625672291263179 ) ) ;
#39857 = CARTESIAN_POINT ( 'NONE',  ( 1.284279953904121641, 3.034610286488902187, 0.7750000000000117906 ) ) ;
#39859 = VERTEX_POINT ( 'NONE', #66761 ) ;
#39858 = CARTESIAN_POINT ( 'NONE',  ( -2.830620210203090181, 6.524417021870718258, 0.000000000000000000 ) ) ;
#39860 = CARTESIAN_POINT ( 'NONE',  ( -7.253248993186740989, 9.485209796849769504, 1.443375672974090751 ) ) ;
#39861 = CARTESIAN_POINT ( 'NONE',  ( 3.663272223086514234, -1.945104670120747059, -1.042327912031751458 ) ) ;
#39862 = CARTESIAN_POINT ( 'NONE',  ( 1.001543065824772753E-15, -3.259374999522042682, 3.793834371823811669 ) ) ;
#39863 = ORIENTED_EDGE ( 'NONE', *, *, #107334, .T. ) ;
#39864 = CARTESIAN_POINT ( 'NONE',  ( 0.7075644152179439983, 0.5912319408809820764, -1.764584214936999684 ) ) ;
#39865 = CARTESIAN_POINT ( 'NONE',  ( -0.02880301295726198432, 2.855735178999906587, -2.761736421759506399 ) ) ;
#39866 = CARTESIAN_POINT ( 'NONE',  ( 1.499999999999989120, 5.077083334016151639, -0.8660254037844323793 ) ) ;
#39867 = CARTESIAN_POINT ( 'NONE',  ( 4.521492410791133842, 7.227233577430748568, -1.288726771885986055 ) ) ;
#39869 = FACE_OUTER_BOUND ( 'NONE', #6126, .T. ) ;
#39868 = CARTESIAN_POINT ( 'NONE',  ( -6.423891471114925977, 6.884501071190606503, -0.7550301924055674574 ) ) ;
#39870 = CARTESIAN_POINT ( 'NONE',  ( 6.175717916360309090, -0.9808100270635997653, 1.557957644481674730 ) ) ;
#39871 = ORIENTED_EDGE ( 'NONE', *, *, #112217, .T. ) ;
#39872 = CARTESIAN_POINT ( 'NONE',  ( 1.832957655136749908, 0.2007874442899897915, 2.051070037287055392 ) ) ;
#39873 = CARTESIAN_POINT ( 'NONE',  ( 1.360316468749969809, 1.036458333674743049, -0.7853790794158820310 ) ) ;
#39874 = CARTESIAN_POINT ( 'NONE',  ( -6.368579470117215813, 8.453095353268645695, 1.599625672291283607 ) ) ;
#39875 = CARTESIAN_POINT ( 'NONE',  ( 10.91850271852025500, -9.971093637360025852, -0.1617895344457838669 ) ) ;
#39876 = CARTESIAN_POINT ( 'NONE',  ( 11.84668730067608600, 19.00000000000000000, -1.320000000000001616 ) ) ;
#39877 = CARTESIAN_POINT ( 'NONE',  ( 5.522248639467795428, 5.337044922334209573, -0.7998128361456231517 ) ) ;
#39878 = CARTESIAN_POINT ( 'NONE',  ( 1.094684877246233201, -0.5000429121475665761, -1.999180680717755898 ) ) ;
#39880 = CARTESIAN_POINT ( 'NONE',  ( 4.651808992177354440, 0.7092673950449077669, 1.699362209096597187 ) ) ;
#39879 = CARTESIAN_POINT ( 'NONE',  ( 7.837739514543059934E-16, -2.859583229930517945E-15, -6.399999999999999467 ) ) ;
#39881 = CARTESIAN_POINT ( 'NONE',  ( 6.226218857173709154, 8.287007971501239467, 1.599625672291281386 ) ) ;
#39882 = CARTESIAN_POINT ( 'NONE',  ( -6.656127069666307072, 6.730179434224282886, 0.7998128361456341429 ) ) ;
#39883 = CARTESIAN_POINT ( 'NONE',  ( -0.2409995289980246258, 7.629137130509076492, -2.600476469121239198 ) ) ;
#39884 = AXIS2_PLACEMENT_3D ( 'NONE', #81254, #148399, #193931 ) ;
#39885 = CARTESIAN_POINT ( 'NONE',  ( 4.020313978404310262, -1.133593497508533110, -1.893353337301090233 ) ) ;
#39886 = CARTESIAN_POINT ( 'NONE',  ( 6.819576192995205233, -2.197070018990463502, 0.5395731105267542738 ) ) ;
#39887 = CARTESIAN_POINT ( 'NONE',  ( -5.748293942514180799, 7.729428904398431222, -1.443375672974052559 ) ) ;
#39888 = CARTESIAN_POINT ( 'NONE',  ( 0.7031954830387620037, 1.685401770928725007, -0.9037484838233383888 ) ) ;
#39889 = CARTESIAN_POINT ( 'NONE',  ( 1.042204282965590201, 0.8216761606248854655, 1.841732292558920570 ) ) ;
#39890 = CARTESIAN_POINT ( 'NONE',  ( -6.818239719371408825, -6.631671897293992757, 6.594971851908693061 ) ) ;
#39891 = CARTESIAN_POINT ( 'NONE',  ( 1.335823321505170025, -1.456863090139989714, 1.777644367010343451 ) ) ;
#39892 = CARTESIAN_POINT ( 'NONE',  ( 6.772336237553374438, -1.148929780121176414, 1.476827877338216854 ) ) ;
#39893 = CARTESIAN_POINT ( 'NONE',  ( 11.33772463945036790, 19.00000000000000000, -3.680000000000002824 ) ) ;
#39894 = CARTESIAN_POINT ( 'NONE',  ( 4.022871489700263758, 7.776595455899835585, -0.3464378842543735515 ) ) ;
#39895 = CARTESIAN_POINT ( 'NONE',  ( 1.340467186903429253, 0.3614942610149494695, 1.835218787103513050 ) ) ;
#39896 = VECTOR ( 'NONE', #82026, 1000.000000000000000 ) ;
#39897 = CARTESIAN_POINT ( 'NONE',  ( 2.290250256651988892, -0.7762311197250795214, -1.861343989391924358 ) ) ;
#39899 = DIRECTION ( 'NONE',  ( 0.9885327375000381167, 0.000000000000000000, 0.1510067114093955609 ) ) ;
#39898 = CARTESIAN_POINT ( 'NONE',  ( 0.6823417656249882723, 0.3427083336747516196, 1.181850606188755259 ) ) ;
#39901 = CARTESIAN_POINT ( 'NONE',  ( 5.074884281356676574, -1.982714853632736807, -0.7105774565657559938 ) ) ;
#39900 = CARTESIAN_POINT ( 'NONE',  ( -9.179033691651859783, 10.66762638080401260, 1.199719254218462483 ) ) ;
#39902 = CARTESIAN_POINT ( 'NONE',  ( 6.598014311344812199, 10.84943379654430906, 1.040834085586084257E-14 ) ) ;
#39904 = CARTESIAN_POINT ( 'NONE',  ( -7.690499447449645309, 9.995335326823163058, 1.599625672291295375 ) ) ;
#39903 = CARTESIAN_POINT ( 'NONE',  ( 4.037295881819344956, 7.932205305423046582, -0.7998128361456362523 ) ) ;
#39905 = CARTESIAN_POINT ( 'NONE',  ( -0.1588444833727709893, -6.630981389236889179, -9.484513307599968357 ) ) ;
#39906 = CARTESIAN_POINT ( 'NONE',  ( 3.990493710177836828, -1.159536886187025440, 1.653596977174769833 ) ) ;
#39907 = CARTESIAN_POINT ( 'NONE',  ( -1.201851678989727383E-14, 4.696875000341419693, -1.575800808251660134 ) ) ;
#39908 = CIRCLE ( 'NONE', #160964, 0.08000000000000040412 ) ;
#39909 = CARTESIAN_POINT ( 'NONE',  ( 6.877413164483755281, -0.1458786163922053403, 2.030295828278828374 ) ) ;
#39910 = CARTESIAN_POINT ( 'NONE',  ( 9.137832345930652522, 10.72352116074969075, -1.082531754730543083 ) ) ;
#39911 = CARTESIAN_POINT ( 'NONE',  ( 4.727887898869392203, -1.325758432718616042, -1.707240035374466114 ) ) ;
#39912 = CARTESIAN_POINT ( 'NONE',  ( 7.212011367826596242, 7.378711115411311638, 0.000000000000000000 ) ) ;
#39913 = CARTESIAN_POINT ( 'NONE',  ( -1.402160292154681736E-14, -0.8656249996585829720, 1.575800808251672791 ) ) ;
#39914 = CARTESIAN_POINT ( 'NONE',  ( 5.936491157937257235, 8.019268665717216749, 1.599625672291268286 ) ) ;
#39915 = CARTESIAN_POINT ( 'NONE',  ( 7.632877294369377452, 8.967740267261513409, -1.082531754730537976 ) ) ;
#39917 = CARTESIAN_POINT ( 'NONE',  ( 1.419999999999990603, 6.200000000000045475, 2.873333333333337070 ) ) ;
#39916 = CARTESIAN_POINT ( 'NONE',  ( 2.207711330564741559, -1.742939566808225482, -1.294460726261867034 ) ) ;
#39919 = CARTESIAN_POINT ( 'NONE',  ( 2.261056740009634414, 1.805359621025553363, -0.3608742708730780513 ) ) ;
#39918 = CARTESIAN_POINT ( 'NONE',  ( -6.087247782855839340, 6.204136622861004646, 0.000000000000000000 ) ) ;
#39920 = EDGE_CURVE ( 'NONE', #196061, #149524, #130973, .T. ) ;
#39921 = CARTESIAN_POINT ( 'NONE',  ( -0.6823417656250003738, 2.717708333674753618, -1.181850606188749264 ) ) ;
#39922 = CARTESIAN_POINT ( 'NONE',  ( 3.210657068901449307, 1.982179491636561819, 0.9350799695589939731 ) ) ;
#39923 = CARTESIAN_POINT ( 'NONE',  ( 6.983263157960330147, 2.416677186285462575, 2.534499922921686021 ) ) ;
#39924 = CARTESIAN_POINT ( 'NONE',  ( 3.503020383517113423, 1.785049946035693891, -1.390086647613536952 ) ) ;
#39925 = CARTESIAN_POINT ( 'NONE',  ( -6.043183783389232566, 8.073467052085995022, 1.599625672291269396 ) ) ;
#39926 = CARTESIAN_POINT ( 'NONE',  ( 6.348694402744908594, 6.841026321354189754, -0.6301123915167846645 ) ) ;
#39927 = CARTESIAN_POINT ( 'NONE',  ( -1.500000000000015099, 14.22916666666666785, -0.8660254037844309360 ) ) ;
#39928 = CARTESIAN_POINT ( 'NONE',  ( 5.560252395380215873, 6.619954228432645138, 1.082531754730549078 ) ) ;
#39929 = CARTESIAN_POINT ( 'NONE',  ( 5.202326708214688900, -0.5966268589385533838, -1.666288158821194187 ) ) ;
#39930 = CARTESIAN_POINT ( 'NONE',  ( 3.352200558804620645, 0.9032658637736007412, -1.799124413793075528 ) ) ;
#39931 = CARTESIAN_POINT ( 'NONE',  ( 8.772289083241844310, 10.19309100432570148, -1.199719254218446718 ) ) ;
#39932 = CARTESIAN_POINT ( 'NONE',  ( 1.430846025165666280, 2.029450977514839938, 0.5621798225463514598 ) ) ;
#39934 = CARTESIAN_POINT ( 'NONE',  ( -1.500000000000013101, 0.9208333333333594828, 0.8660254037844403729 ) ) ;
#39933 = CARTESIAN_POINT ( 'NONE',  ( -1.364683531250010295, 11.13020833367473372, 0.7879004041258445001 ) ) ;
#39935 = CARTESIAN_POINT ( 'NONE',  ( 0.8714670931111346830, -0.2923345663568870378, 1.947617037577647592 ) ) ;
#39936 = CARTESIAN_POINT ( 'NONE',  ( -4.309512724297390740, 6.121127159803966933, 1.599625672291270506 ) ) ;
#39937 = CARTESIAN_POINT ( 'NONE',  ( 0.4144086874100678664, 0.7473079093508437909, 1.814158889769983185 ) ) ;
#39939 = ORIENTED_EDGE ( 'NONE', *, *, #161766, .F. ) ;
#39938 = CARTESIAN_POINT ( 'NONE',  ( 6.222923320161976690, 1.335851037236086558, -1.223852264422401692 ) ) ;
#39940 = CARTESIAN_POINT ( 'NONE',  ( 7.307481608085759639, 7.627742752295940676, 1.040834085586084257E-14 ) ) ;
#39941 = CARTESIAN_POINT ( 'NONE',  ( 5.137510444216992767, -1.323429205136433140, -1.322332877454430955 ) ) ;
#39942 = CARTESIAN_POINT ( 'NONE',  ( 2.866659414285625651, 5.431854185720147221, -1.199719254218446718 ) ) ;
#39944 = ORIENTED_EDGE ( 'NONE', *, *, #111631, .T. ) ;
#39943 = TOROIDAL_SURFACE ( 'NONE', #36363, 0.4800000000000000933, 0.08000000000000000167 ) ;
#39945 = CARTESIAN_POINT ( 'NONE',  ( 4.662978783614929235, 1.603679166536524869, -1.309313232293010776 ) ) ;
#39946 = CARTESIAN_POINT ( 'NONE',  ( 1.224999999999989209, 1.604166666666679619, 0.7072540797572898219 ) ) ;
#39947 = EDGE_CURVE ( 'NONE', #159976, #205805, #13777, .T. ) ;
#39948 = CARTESIAN_POINT ( 'NONE',  ( -5.194182247366913252, 7.153241603385088965, 1.443375672974058777 ) ) ;
#39949 = CARTESIAN_POINT ( 'NONE',  ( 0.006158830626129541130, 7.078243236992583398, -2.121324627965408993 ) ) ;
#39950 = CARTESIAN_POINT ( 'NONE',  ( 8.762647353133951711, 9.117510088278095282, 1.040834085586084257E-14 ) ) ;
#39951 = CARTESIAN_POINT ( 'NONE',  ( -8.422639742587602285, 10.84949900448412841, -1.599625672291263179 ) ) ;
#39952 = CARTESIAN_POINT ( 'NONE',  ( 5.833751235630055376, 10.02806988486892514, 0.7998128361456331437 ) ) ;
#39953 = CYLINDRICAL_SURFACE ( 'NONE', #94039, 1.250000000000000000 ) ;
#39954 = CARTESIAN_POINT ( 'NONE',  ( 1.364683531249986537, 0.1552083336747499542, -0.7879004041258309554 ) ) ;
#39955 = CARTESIAN_POINT ( 'NONE',  ( -1.402160292154681736E-14, 1.837500000000019895, -1.732050807568863648 ) ) ;
#39957 = CARTESIAN_POINT ( 'NONE',  ( 5.660692828905515839, 6.562895374266609849, -1.199719254218445830 ) ) ;
#39956 = CARTESIAN_POINT ( 'NONE',  ( 4.527759979645433752, 1.903474890065796732, -0.4746247275292309609 ) ) ;
#39958 = CARTESIAN_POINT ( 'NONE',  ( 1.968124833515383809, 1.674630251985644414, 1.122327857054454814 ) ) ;
#39959 = CARTESIAN_POINT ( 'NONE',  ( 0.000000000000000000, 13.49999999999999822, 0.000000000000000000 ) ) ;
#39960 = CARTESIAN_POINT ( 'NONE',  ( 0.9432342461353732110, -1.730868645791438620, -1.344178957308760802 ) ) ;
#39961 = CARTESIAN_POINT ( 'NONE',  ( 2.178771278573924608, -0.08713135167291724548, -1.868625915979430951 ) ) ;
#39962 = CARTESIAN_POINT ( 'NONE',  ( -1.001543065824772872E-14, 4.571875000341418804, 1.575800808251672791 ) ) ;
#39963 = CARTESIAN_POINT ( 'NONE',  ( 4.095951438411546519, 1.318107682886668242, 1.521754241968393373 ) ) ;
#39964 = CARTESIAN_POINT ( 'NONE',  ( -7.296259222448620463, 11.66405285949874759, 0.7998128361456481317 ) ) ;
#39965 = B_SPLINE_CURVE_WITH_KNOTS ( 'NONE', 3,
 ( #163786, #145439, #115086, #31652, #110819, #16429, #111898, #79322 ),
 .UNSPECIFIED., .F., .F.,
 ( 4, 2, 2, 4 ),
 ( 0.000000000000000000, 0.0002567066673176287726, 0.0005134133346352575452, 0.001026826669270511404 ),
 .UNSPECIFIED. ) ;
#39967 = CARTESIAN_POINT ( 'NONE',  ( 3.005573934588702034, -2.039760842771252136, 0.5671949335201897924 ) ) ;
#39966 = CARTESIAN_POINT ( 'NONE',  ( -4.121315508874255684, 7.752025827087861920, -0.7216878364870267237 ) ) ;
#39968 = CARTESIAN_POINT ( 'NONE',  ( 3.588273936444265289, 7.344317902764286643, -0.3372145678562175064 ) ) ;
#39969 = CARTESIAN_POINT ( 'NONE',  ( 4.510256325466165173, 2.069976601481211542, -0.04757507122059301263 ) ) ;
#39970 = CARTESIAN_POINT ( 'NONE',  ( 5.182959862174088883, 9.268813282503625572, 0.7998128361456331437 ) ) ;
#39972 = CARTESIAN_POINT ( 'NONE',  ( 6.720655732516667591, 2.416141799769660370, 2.554522868665403568 ) ) ;
#39971 = CARTESIAN_POINT ( 'NONE',  ( 1.189138979623612480, 1.585436599910443611, 1.363068659274695893 ) ) ;
#39974 = ORIENTED_EDGE ( 'NONE', *, *, #135584, .T. ) ;
#39973 = CARTESIAN_POINT ( 'NONE',  ( 6.053692819838605743, 0.5272490726609192491, -1.747765065496959869 ) ) ;
#39975 = CARTESIAN_POINT ( 'NONE',  ( 8.125414133291656071, 8.374071331795406081, -0.7998128361456291469 ) ) ;
#39976 = DIRECTION ( 'NONE',  ( -0.000000000000000000, -1.000000000000000000, -0.000000000000000000 ) ) ;
#39977 = CARTESIAN_POINT ( 'NONE',  ( -11.76695491367977198, 4.673720869072629291, 4.995412848167409159 ) ) ;
#39978 = CARTESIAN_POINT ( 'NONE',  ( 6.263503779389103521, 10.25124547602188763, 1.040834085586084257E-14 ) ) ;
#39979 = CARTESIAN_POINT ( 'NONE',  ( -1.364683531250000748, 12.92187500034139980, 0.000000000000000000 ) ) ;
#39980 = CARTESIAN_POINT ( 'NONE',  ( 5.830699381415811899, 1.280921311228696347, -1.420062396151056117 ) ) ;
#39981 = CARTESIAN_POINT ( 'NONE',  ( -8.616370316684697883, 10.01118577667568132, -1.199719254218446718 ) ) ;
#39982 = CARTESIAN_POINT ( 'NONE',  ( 6.006425746053997372, 6.966250444273174303, -1.199719254218445830 ) ) ;
#39983 = CARTESIAN_POINT ( 'NONE',  ( 0.1531059978909261043, -6.764708007038248816, 10.99917004716958857 ) ) ;
#39984 = CARTESIAN_POINT ( 'NONE',  ( -2.788906526875773208E-15, 12.21875000068279782, -1.499999999999998446 ) ) ;
#39985 = CARTESIAN_POINT ( 'NONE',  ( 3.846762897975340767, 5.510976019103107859, -1.599625672291256295 ) ) ;
#39986 = ORIENTED_EDGE ( 'NONE', *, *, #49632, .F. ) ;
#39987 = CARTESIAN_POINT ( 'NONE',  ( 6.169546029190325243, 1.392557221580101423, 1.458547251757099650 ) ) ;
#39988 = CARTESIAN_POINT ( 'NONE',  ( -4.016479854857874621, 7.690552166905142428, -0.3130353517275369368 ) ) ;
#39989 =( GEOMETRIC_REPRESENTATION_CONTEXT ( 3 ) GLOBAL_UNCERTAINTY_ASSIGNED_CONTEXT ( ( #191927 ) ) GLOBAL_UNIT_ASSIGNED_CONTEXT ( ( #38477, #118715, #101332 ) ) REPRESENTATION_CONTEXT ( 'NONE', 'WORKASPACE' ) );
#39990 = CARTESIAN_POINT ( 'NONE',  ( 1.874158809982179319, 3.299964346911585356, -0.3999999999999993006 ) ) ;
#39991 = CARTESIAN_POINT ( 'NONE',  ( 0.1399997263886038068, 0.2431072571701595186, -2.034387401959360187 ) ) ;
#39992 = CARTESIAN_POINT ( 'NONE',  ( -4.555176424511596878, 7.297827681030051750, 1.082531754730560403 ) ) ;
#39993 = AXIS2_PLACEMENT_3D ( 'NONE', #7468, #139650, #91965 ) ;
#39994 = CARTESIAN_POINT ( 'NONE',  ( 2.846322183865124700, 5.408127416896231665, -1.199719254218446718 ) ) ;
#39995 = CARTESIAN_POINT ( 'NONE',  ( 3.766418665963155998, -0.7939890815925625400, -1.802475468321093732 ) ) ;
#39996 = CARTESIAN_POINT ( 'NONE',  ( 4.200796113533305842, 1.844717850457804120, 0.8146114232021259838 ) ) ;
#39997 = CARTESIAN_POINT ( 'NONE',  ( -7.379715684540041565, 7.504089808251839244, 1.040834085586084257E-14 ) ) ;
#39998 = CARTESIAN_POINT ( 'NONE',  ( -3.083288183660637838, 6.450096981798545848, -0.7078863735355921394 ) ) ;
#39999 = CARTESIAN_POINT ( 'NONE',  ( 4.400438482046089561, 1.694813852089768869, -1.389250428430639950 ) ) ;
#40000 = LINE ( 'NONE', #124528, #116119 ) ;
#40001 = CARTESIAN_POINT ( 'NONE',  ( 3.276308702328960099, -1.148522560162130501, 1.546420931960400758 ) ) ;
#40002 = CARTESIAN_POINT ( 'NONE',  ( -9.006694118179950692, 9.402231314165087284, 1.040834085586084257E-14 ) ) ;
#40003 = CARTESIAN_POINT ( 'NONE',  ( -0.1294898018151836583, 2.884012836773319766, -2.415168928093185396 ) ) ;
#40004 = CARTESIAN_POINT ( 'NONE',  ( 0.1331565106231329398, 0.7299000548664087429, -2.029785554894456556 ) ) ;
#40005 = CARTESIAN_POINT ( 'NONE',  ( 1.364683531249997417, 12.98437500034139980, 2.602085213965210642E-15 ) ) ;
#40006 = CARTESIAN_POINT ( 'NONE',  ( 3.649115900372475796, 7.409052317076538330, 1.040834085586084257E-14 ) ) ;
#40007 = CARTESIAN_POINT ( 'NONE',  ( -4.957044826794452241, 6.512741263612475962, -2.499999999999995115 ) ) ;
#40008 = CARTESIAN_POINT ( 'NONE',  ( 3.933273961740286317, 7.602920365423422311, 0.7216878364870257245 ) ) ;
#40010 = CARTESIAN_POINT ( 'NONE',  ( 2.754543805099545217, 1.998131736582898332, 0.2443565819899694291 ) ) ;
#40009 = CARTESIAN_POINT ( 'NONE',  ( 5.706567001488551227, 1.626822141722890303, 0.8623401093873286349 ) ) ;
#40011 = CARTESIAN_POINT ( 'NONE',  ( 5.062018989497997445, 1.914771916633486448, -1.271085502950035417 ) ) ;
#40013 = CARTESIAN_POINT ( 'NONE',  ( 3.045584334709343644, 1.312524258565110680, 1.319513337161677846 ) ) ;
#40012 = CARTESIAN_POINT ( 'NONE',  ( 10.51595811585101004, 9.986596539918549453, -3.553980774159643197 ) ) ;
#40014 = CARTESIAN_POINT ( 'NONE',  ( 1.642778471875000035, -0.9260416661887073131, -2.845375778867859751 ) ) ;
#40015 = CARTESIAN_POINT ( 'NONE',  ( -0.1290005225502922348, 7.629137130509076492, -2.773995091683972625 ) ) ;
#40016 = CARTESIAN_POINT ( 'NONE',  ( -1.123270288250342919, 2.846052654332832610, 0.7749999999993751887 ) ) ;
#40017 = CARTESIAN_POINT ( 'NONE',  ( -7.555971681517696936, 7.709721804725773175, 0.7998128361456462443 ) ) ;
#40018 = CARTESIAN_POINT ( 'NONE',  ( -3.201133666602369310, 6.748756687762456963, -0.7216878364870458196 ) ) ;
#40019 = CARTESIAN_POINT ( 'NONE',  ( 5.689037021386003090, 1.583751769416761324, 1.365026519206056665 ) ) ;
#40020 = CARTESIAN_POINT ( 'NONE',  ( 6.046573322014824114, 7.117052299514516456, -1.082531754730543083 ) ) ;
#40021 = ORIENTED_EDGE ( 'NONE', *, *, #77981, .T. ) ;
#40022 = CARTESIAN_POINT ( 'NONE',  ( 4.663288057535367237, 8.288536188413402783, 0.5084364831346009916 ) ) ;
#40023 = CARTESIAN_POINT ( 'NONE',  ( 6.410786927598755902, 1.272630858062718584, -1.164536656126140324 ) ) ;
#40024 = CARTESIAN_POINT ( 'NONE',  ( -6.098470168048611306, 6.009303372345148553, 1.040834085586084257E-14 ) ) ;
#40025 = CARTESIAN_POINT ( 'NONE',  ( 2.408496482339622879, -0.9999731500247920346, -1.416544738438466400 ) ) ;
#40026 = DIRECTION ( 'NONE',  ( -1.000000000000000000, 0.000000000000000000, 0.000000000000000000 ) ) ;
#40028 = CARTESIAN_POINT ( 'NONE',  ( -7.067878151425722955, 7.140279352951794500, 0.7998128361456341429 ) ) ;
#40027 = AXIS2_PLACEMENT_3D ( 'NONE', #166428, #16952, #18018 ) ;
#40029 = CARTESIAN_POINT ( 'NONE',  ( -5.868066076333878556, 6.026401760103492045, 0.3561039394813777514 ) ) ;
#40030 = CARTESIAN_POINT ( 'NONE',  ( 6.842638762948665132, -2.127444276778973631, -0.4322993451541176091 ) ) ;
#40031 = CARTESIAN_POINT ( 'NONE',  ( 5.391160240453525709, 1.608232483172780558, -0.8641324296934371763 ) ) ;
#40032 = CARTESIAN_POINT ( 'NONE',  ( 3.010546455304231372, 0.6564385890225448161, 1.848828695667027677 ) ) ;
#40033 = CARTESIAN_POINT ( 'NONE',  ( -3.928309112595642638, 7.388819966165147690, 0.6129890987886537079 ) ) ;
#40034 = CARTESIAN_POINT ( 'NONE',  ( -7.818248136574758256, 12.27303992597924420, 0.000000000000000000 ) ) ;
#40035 = CARTESIAN_POINT ( 'NONE',  ( 6.238723240582662477, 10.43026088065513513, -0.7998128361456291469 ) ) ;
#40036 = EDGE_CURVE ( 'NONE', #83383, #81693, #74135, .T. ) ;
#40037 = CARTESIAN_POINT ( 'NONE',  ( 3.615986862044855421, -0.6139777315949943581, 2.029667854546577388 ) ) ;
#40038 = CARTESIAN_POINT ( 'NONE',  ( -3.958617665510283601, 4.681104033592509595, -1.082531754730549967 ) ) ;
#40039 = DIRECTION ( 'NONE',  ( 0.000000000000000000, 0.000000000000000000, -1.000000000000000000 ) ) ;
#40040 = B_SPLINE_CURVE_WITH_KNOTS ( 'NONE', 3,
 ( #157137, #77997, #94280, #192797 ),
 .UNSPECIFIED., .F., .F.,
 ( 4, 4 ),
 ( 0.000000000000000000, 0.0001577902508744045485 ),
 .UNSPECIFIED. ) ;
#40041 = CIRCLE ( 'NONE', #36467, 9.999999999999998224 ) ;
#40042 = CARTESIAN_POINT ( 'NONE',  ( 1.780221101387355009, -1.146701191353172611, -1.723467693327894068 ) ) ;
#40044 = CARTESIAN_POINT ( 'NONE',  ( 1.499999999999993117, 15.13541666734946745, 0.8660254037844409281 ) ) ;
#40043 = CARTESIAN_POINT ( 'NONE',  ( 6.827182134110207024, 2.985003573113382380, 2.264833014350222662 ) ) ;
#40046 = ORIENTED_EDGE ( 'NONE', *, *, #107183, .T. ) ;
#40045 = CARTESIAN_POINT ( 'NONE',  ( 4.617978872065289231, -0.5927926152728602016, 2.140694073679518805 ) ) ;
#40047 = CARTESIAN_POINT ( 'NONE',  ( 1.670936656956054644, 1.588967112724626096, 1.661273962566457874 ) ) ;
#40049 = CARTESIAN_POINT ( 'NONE',  ( 6.385603471572667722, -1.944119864917488893, 0.6893456996763939193 ) ) ;
#40048 = CARTESIAN_POINT ( 'NONE',  ( 10.05978679165993839, 10.83876546646586014, 0.7216878364870438212 ) ) ;
#40051 = CARTESIAN_POINT ( 'NONE',  ( -3.285556943750000070, -3.609374999522043659, 0.000000000000000000 ) ) ;
#40050 = CARTESIAN_POINT ( 'NONE',  ( 5.225741863424510747, 5.061396693608882558, 0.7998128361456352531 ) ) ;
#40052 = CARTESIAN_POINT ( 'NONE',  ( 6.181194517112824194, 1.274813594131599226, 1.328792456347933637 ) ) ;
#40053 = EDGE_LOOP ( 'NONE', ( #153906, #187955, #200470 ) ) ;
#40054 = CARTESIAN_POINT ( 'NONE',  ( 1.387358672525637715, 7.251968950354889643, -4.302625267139783993 ) ) ;
#40055 = CARTESIAN_POINT ( 'NONE',  ( 2.935702856749936362, -1.841876368404654629, 0.5141854427313449216 ) ) ;
#40056 = CARTESIAN_POINT ( 'NONE',  ( -0.1106727585416201337, 1.364743060583981649, -2.259751816641343058 ) ) ;
#40057 = CARTESIAN_POINT ( 'NONE',  ( 3.979312383816283383, 1.623897443016858011, -0.5815980338331677713 ) ) ;
#40058 = CARTESIAN_POINT ( 'NONE',  ( 1.903530124611974017, -1.954778955200174861, 0.4946342604733033887 ) ) ;
#40059 = CARTESIAN_POINT ( 'NONE',  ( 4.289826696582184518, 1.777288211397337170, -1.457785959652138530 ) ) ;
#40060 = CARTESIAN_POINT ( 'NONE',  ( 4.007294123747324299, 1.937827550919896336, 1.167430888521280963 ) ) ;
#40061 = CARTESIAN_POINT ( 'NONE',  ( 6.217421135136044441, -0.2594034420708571931, 2.089956235961006659 ) ) ;
#40062 = CARTESIAN_POINT ( 'NONE',  ( -6.943184063974186415, 7.273005294157565359, -0.7216878364870338292 ) ) ;
#40063 = EDGE_LOOP ( 'NONE', ( #145473, #127716, #81646, #187436, #138281 ) ) ;
#40064 = CARTESIAN_POINT ( 'NONE',  ( 4.499107683057060214, 1.420662411309661088, 1.055048638519467286 ) ) ;
#40066 = CARTESIAN_POINT ( 'NONE',  ( 0.8500709472824579116, 2.289359419033740295, -0.1177234237379476411 ) ) ;
#40065 = CARTESIAN_POINT ( 'NONE',  ( 7.147083253059300922, 8.367293879104554577, 1.199719254218452935 ) ) ;
#40067 = CARTESIAN_POINT ( 'NONE',  ( 5.701068745948241201, -0.4431999317857804876, 1.786873912291174538 ) ) ;
#40068 = CARTESIAN_POINT ( 'NONE',  ( -3.273404022695637572, 5.906389562198459231, 1.199719254218462483 ) ) ;
#40069 = CARTESIAN_POINT ( 'NONE',  ( 6.263654578238285531, 1.123272483274835087, 1.881548979392036802 ) ) ;
#40070 = CARTESIAN_POINT ( 'NONE',  ( -2.435661151949389147, 5.993355110582911038, 0.7998128361456341429 ) ) ;
#40071 = CARTESIAN_POINT ( 'NONE',  ( -4.353456923439328108, 15.51896013954493192, 11.19146259264864085 ) ) ;
#40072 = CARTESIAN_POINT ( 'NONE',  ( 6.162566008723842081, -0.7415158119226210598, -1.933206815039355320 ) ) ;
#40073 = CARTESIAN_POINT ( 'NONE',  ( -0.2351498743046881446, -0.1506043639611966134, -1.983733596389973597 ) ) ;
#40074 = CARTESIAN_POINT ( 'NONE',  ( -1.364683531249997417, 5.509375000341417916, 1.214306433183764966E-14 ) ) ;
#40075 = CARTESIAN_POINT ( 'NONE',  ( 4.424389683245252947, 1.183944675904605504, -1.519688292035234367 ) ) ;
#40076 = CARTESIAN_POINT ( 'NONE',  ( -0.6823417656250039265, 10.31770833367473550, -1.181850606188755259 ) ) ;
#40077 = DIRECTION ( 'NONE',  ( 0.000000000000000000, 1.000000000000000000, 0.000000000000000000 ) ) ;
#40078 = CARTESIAN_POINT ( 'NONE',  ( 0.8970957097632881183, -2.168902827774013442, -0.4795612232612302961 ) ) ;
#40080 = EDGE_LOOP ( 'NONE', ( #156000, #30119, #34739, #10982, #146094, #81451, #38759, #5324 ) ) ;
#40079 = FACE_OUTER_BOUND ( 'NONE', #123994, .T. ) ;
#40081 = CARTESIAN_POINT ( 'NONE',  ( -4.858757509019083543, 5.629766575900002401, -2.420000000000000373 ) ) ;
#40082 = CARTESIAN_POINT ( 'NONE',  ( 10.70146331988817323, 11.37946204949139251, 0.7998128361456341429 ) ) ;
#40083 = DIRECTION ( 'NONE',  ( 0.000000000000000000, 1.000000000000000000, 0.000000000000000000 ) ) ;
#40084 = CARTESIAN_POINT ( 'NONE',  ( 11.88168329227126563, 11.38000000000000078, -1.685799833707129380 ) ) ;
#40085 = CARTESIAN_POINT ( 'NONE',  ( 10.35108092051076412, 10.47472330378973204, 5.983479465268499276 ) ) ;
#40086 = CARTESIAN_POINT ( 'NONE',  ( 9.368320956918608999, 11.95279375453699622, 1.443375672974076540 ) ) ;
#40087 = CARTESIAN_POINT ( 'NONE',  ( 1.170277241841523264, -0.8789641444944886750, -1.754005360843587047 ) ) ;
#40088 = CARTESIAN_POINT ( 'NONE',  ( 0.6823417656249882723, 1.988541667008083991, -1.181850606188749264 ) ) ;
#40089 = CARTESIAN_POINT ( 'NONE',  ( 1.499999999999989120, 3.754166666666685082, 0.8660254037844522523 ) ) ;
#40090 = CARTESIAN_POINT ( 'NONE',  ( 6.584431417889404337, 1.130572321132311098, -1.603143135845342515 ) ) ;
#40091 = CARTESIAN_POINT ( 'NONE',  ( -8.646349277213090545, 11.11049346154719508, 1.599625672291269396 ) ) ;
#40092 = CARTESIAN_POINT ( 'NONE',  ( -4.351804119862249465, 7.060559992272473551, 1.082531754730560403 ) ) ;
#40093 = CARTESIAN_POINT ( 'NONE',  ( 0.3568017664055183613, 0.8693207686717405736, 2.089032543936353736 ) ) ;
#40095 = ORIENTED_EDGE ( 'NONE', *, *, #77256, .F. ) ;
#40094 = CARTESIAN_POINT ( 'NONE',  ( -4.530395885260773525, 8.437212299446219532, 0.7998128361456481317 ) ) ;
#40097 = EDGE_CURVE ( 'NONE', #163559, #16492, #43093, .T. ) ;
#40096 = CARTESIAN_POINT ( 'NONE',  ( -1.364683531249997417, 5.509375000341417916, 1.214306433183764966E-14 ) ) ;
#40098 = CARTESIAN_POINT ( 'NONE',  ( 1.194370141144196706, -0.4488658031855938813, -1.815784161679114384 ) ) ;
#40099 = CARTESIAN_POINT ( 'NONE',  ( 6.766931417284230754, -1.733354565069046505, 0.04740994324908299334 ) ) ;
#40101 = CARTESIAN_POINT ( 'NONE',  ( 4.230150181147958044, 2.149441460308566754, 0.4267382380854707336 ) ) ;
#40100 = CARTESIAN_POINT ( 'NONE',  ( 1.360316468749947605, 2.536458333674726173, -0.7853790794159141164 ) ) ;
#40102 = CARTESIAN_POINT ( 'NONE',  ( 4.085262347903253044, -0.2225469472450763153, -2.296823545465367822 ) ) ;
#40103 = CARTESIAN_POINT ( 'NONE',  ( 0.5673477787482993362, 0.2024836561579176908, -2.050924697174760780 ) ) ;
#40104 = CARTESIAN_POINT ( 'NONE',  ( 2.730336461235380430, 0.2382978201147344655, 1.927214864610910183 ) ) ;
#40105 = CARTESIAN_POINT ( 'NONE',  ( -5.924549939047510705, 6.974691686052601369, 1.082531754730549967 ) ) ;
#40106 = B_SPLINE_CURVE_WITH_KNOTS ( 'NONE', 3,
 ( #75248, #204133, #170598, #138124, #205217, #108883 ),
 .UNSPECIFIED., .F., .F.,
 ( 4, 2, 4 ),
 ( 0.000000000000000000, 0.0003779448103413553901, 0.0007558896206827107802 ),
 .UNSPECIFIED. ) ;
#40107 = CYLINDRICAL_SURFACE ( 'NONE', #26408, 1.250000000000000000 ) ;
#40108 = CARTESIAN_POINT ( 'NONE',  ( 4.904590598983499916, -2.104870323260544129, -0.2570220051709286579 ) ) ;
#40109 = CARTESIAN_POINT ( 'NONE',  ( 1.253848497529134409, -2.775557561562891351E-14, 0.5275650105875644424 ) ) ;
#40110 = CARTESIAN_POINT ( 'NONE',  ( 3.832657856672664565, 0.6767144645295587457, -1.899618369658891748 ) ) ;
#40111 = CARTESIAN_POINT ( 'NONE',  ( -4.406036734316890247, 7.123831375802920363, -1.082531754730548412 ) ) ;
#40112 = CARTESIAN_POINT ( 'NONE',  ( -5.596483547390937119, 9.751257581923240991, 0.000000000000000000 ) ) ;
#40113 = CARTESIAN_POINT ( 'NONE',  ( 9.103410076571945453, 12.70806329172093818, 1.199719254218450271 ) ) ;
#40114 = CARTESIAN_POINT ( 'NONE',  ( 1.049113529465800054, -1.437755431736492673, -1.125068434497819680 ) ) ;
#40115 = CARTESIAN_POINT ( 'NONE',  ( -7.259464905474441565, 7.434073576000447048, -0.7998128361456362523 ) ) ;
#40116 = CARTESIAN_POINT ( 'NONE',  ( -4.145761110728687804, 8.058748072483927771, -0.7998128361456481317 ) ) ;
#40117 = CARTESIAN_POINT ( 'NONE',  ( -10.82858503610327894, 5.585649091226504659, 6.509997993261127824 ) ) ;
#40118 = ORIENTED_EDGE ( 'NONE', *, *, #199528, .F. ) ;
#40119 = CARTESIAN_POINT ( 'NONE',  ( 5.787979943833009067, -0.9286772032993969583, 1.839872548930401974 ) ) ;
#40120 = CARTESIAN_POINT ( 'NONE',  ( -5.600926855776877211, 9.548515408466085930, -0.7216878364870338292 ) ) ;
#40121 = UNCERTAINTY_MEASURE_WITH_UNIT (LENGTH_MEASURE( 1.000000000000000082E-05 ), #16299, 'distance_accuracy_value', 'NONE');
#40122 = CARTESIAN_POINT ( 'NONE',  ( 6.156811153937166381, 10.19704708965311468, 0.000000000000000000 ) ) ;
#40123 = CARTESIAN_POINT ( 'NONE',  ( -2.916975605234527702, 6.554888639415577423, 1.040834085586084257E-14 ) ) ;
#40124 = CARTESIAN_POINT ( 'NONE',  ( -8.597841969360544567, 13.18256606422934674, 0.7998128361456341429 ) ) ;
#40125 = CARTESIAN_POINT ( 'NONE',  ( 5.127605754342813960, -0.2940821729933600914, 1.998008755081616572 ) ) ;
#40127 = ORIENTED_EDGE ( 'NONE', *, *, #160637, .T. ) ;
#40126 = CARTESIAN_POINT ( 'NONE',  ( 5.778047442595251937, 2.188849720005956900, -0.3775064732549227586 ) ) ;
#40128 = CARTESIAN_POINT ( 'NONE',  ( -6.831329296439251131, 9.063246493969506545, -1.599625672291271394 ) ) ;
#40129 = CARTESIAN_POINT ( 'NONE',  ( 4.469384193999260901, 8.366031992974468423, -0.7998128361456231517 ) ) ;
#40130 = CARTESIAN_POINT ( 'NONE',  ( 4.645419472943275174, -1.591690889772362283, -1.309095959863779246 ) ) ;
#40131 = CARTESIAN_POINT ( 'NONE',  ( 3.920546200773936896, -1.392545040883992336, -1.458557299768625581 ) ) ;
#40132 = VERTEX_POINT ( 'NONE', #73184 ) ;
#40133 = DIRECTION ( 'NONE',  ( 1.000000000000000000, 0.000000000000000000, 0.000000000000000000 ) ) ;
#40135 = EDGE_LOOP ( 'NONE', ( #58314, #177613, #89278, #200665 ) ) ;
#40134 = CARTESIAN_POINT ( 'NONE',  ( -5.257529707049291900, 9.355811434857983500, 0.7998128361456291469 ) ) ;
#40136 = CARTESIAN_POINT ( 'NONE',  ( 5.228576739797318851, 7.698598165248225378, -1.206158463488806953 ) ) ;
#40137 = CARTESIAN_POINT ( 'NONE',  ( 4.411482401463855396, 0.5350073857553553358, 1.943773423102819864 ) ) ;
#40138 = CARTESIAN_POINT ( 'NONE',  ( 3.925598083870453614, 0.9833751987384667936, -1.556331266066004027 ) ) ;
#40139 = CARTESIAN_POINT ( 'NONE',  ( 0.000000000000000000, 3.000000000000000888, -6.329999999999995630 ) ) ;
#40140 = CARTESIAN_POINT ( 'NONE',  ( 0.9796492596481393145, -0.06170110713811990943, -2.307032891211552084 ) ) ;
#40141 = CARTESIAN_POINT ( 'NONE',  ( 4.435452530326143616, 5.203724702582467998, -1.199719254218452047 ) ) ;
#40142 = CARTESIAN_POINT ( 'NONE',  ( 3.849029623751087481, -1.769594347601778361, 1.241129261558816754 ) ) ;
#40143 = CARTESIAN_POINT ( 'NONE',  ( 8.259941899223605333, 10.65968485389279508, -1.599625672291268286 ) ) ;
#40144 = CARTESIAN_POINT ( 'NONE',  ( -5.168682875307782254, 7.053215992657626110, -1.599625672291256295 ) ) ;
#40145 = CARTESIAN_POINT ( 'NONE',  ( 3.550466583917981200, 2.079229874635016184, -0.9797032261932754338 ) ) ;
#40146 = CIRCLE ( 'NONE', #136936, 0.08000000000000020983 ) ;
#40147 = CARTESIAN_POINT ( 'NONE',  ( -3.673896439623305810, 4.156855427197417185, -7.499999999999991118 ) ) ;
#40148 = CARTESIAN_POINT ( 'NONE',  ( 2.887410755087606695, 1.321643875934110479, 1.324118206929347563 ) ) ;
#40149 = CARTESIAN_POINT ( 'NONE',  ( 6.596557512146871360, -0.5253642993188823995, -1.900122941938019450 ) ) ;
#40150 = PRESENTATION_LAYER_ASSIGNMENT (  '', '', ( #29641 ) ) ;
#40152 = CARTESIAN_POINT ( 'NONE',  ( -5.427006627220116286, 9.553534508390610469, -0.7998128361456362523 ) ) ;
#40151 = CARTESIAN_POINT ( 'NONE',  ( 0.6823417656249917140, 5.092708333674749177, 1.181850606188765695 ) ) ;
#40154 = CARTESIAN_POINT ( 'NONE',  ( 1.770444396619451632, 1.136427050704125419, 1.891651738277564831 ) ) ;
#40153 = CARTESIAN_POINT ( 'NONE',  ( -6.586563698140583512, 6.578745824119123675, 1.040834085586084257E-14 ) ) ;
#40155 = FACE_OUTER_BOUND ( 'NONE', #16113, .T. ) ;
#40156 = CARTESIAN_POINT ( 'NONE',  ( 5.138703914779377158, 5.953908307786102583, 1.199719254218462483 ) ) ;
#40157 = CARTESIAN_POINT ( 'NONE',  ( -6.274726165026268454, 6.214935368819085149, 0.7998128361456341429 ) ) ;
#40158 = CARTESIAN_POINT ( 'NONE',  ( 11.89197816957260478, 13.79999999999999893, 0.8055420615339539125 ) ) ;
#40159 = CARTESIAN_POINT ( 'NONE',  ( 5.770382930017874834, -1.251004719971451795, 1.523686133408495236 ) ) ;
#40160 = CARTESIAN_POINT ( 'NONE',  ( 6.147156021580305385, -1.953063626952681542, 1.228987080356194195 ) ) ;
#40161 = CARTESIAN_POINT ( 'NONE',  ( 6.760206150924522817, -1.860609546209352372, 0.04724569877399482920 ) ) ;
#40162 = CARTESIAN_POINT ( 'NONE',  ( 3.186439481354142789, 1.149679979862153756, -1.712247615763124120 ) ) ;
#40163 = CARTESIAN_POINT ( 'NONE',  ( 5.816084710582486217, 9.729256562414162701, 1.040834085586084257E-14 ) ) ;
#40164 = CARTESIAN_POINT ( 'NONE',  ( 6.318982112420993502, 9.529840343536603697, -1.199719254218452047 ) ) ;
#40165 = CARTESIAN_POINT ( 'NONE',  ( 5.951666246274784910, 9.887435020721849099, 0.7216878364870438212 ) ) ;
#40166 = CARTESIAN_POINT ( 'NONE',  ( 1.364683531249988535, 3.426041667008085323, 0.7879004041258500513 ) ) ;
#40167 = CARTESIAN_POINT ( 'NONE',  ( -8.795359111960578957, 14.48154074047005757, 8.214599990152152031 ) ) ;
#40168 = CARTESIAN_POINT ( 'NONE',  ( 3.985733972293228344, 7.593847367743336463, 1.040834085586084257E-14 ) ) ;
#40169 = CARTESIAN_POINT ( 'NONE',  ( 5.582552312218076018, 1.297699880476494094, -1.740541793301546347 ) ) ;
#40171 = CARTESIAN_POINT ( 'NONE',  ( 5.460457653299121361, -1.667157065227730106, -0.7818181906407914994 ) ) ;
#40170 = CARTESIAN_POINT ( 'NONE',  ( -0.02900071798687918478, 7.629137130509076492, -2.773797386654376584 ) ) ;
#40172 = EDGE_CURVE ( 'NONE', #38245, #10803, #155098, .T. ) ;
#40173 = FACE_OUTER_BOUND ( 'NONE', #37, .T. ) ;
#40174 = CARTESIAN_POINT ( 'NONE',  ( 11.89942855770814312, 11.37999999999999901, -0.7000000000000009548 ) ) ;
#40175 = DIRECTION ( 'NONE',  ( -0.007014632059889177630, 0.000000000000000000, -0.9999753971658824625 ) ) ;
#40176 = CARTESIAN_POINT ( 'NONE',  ( 0.6501784551898766029, 0.7083214130543177278, -2.148700229429708841 ) ) ;
#40177 = CARTESIAN_POINT ( 'NONE',  ( -4.061425534073997312, 7.733864674645915649, 0.6335290845049870168 ) ) ;
#40178 = CARTESIAN_POINT ( 'NONE',  ( -1.718115394875207258, -1.600000000000000755, 2.017567716309124126 ) ) ;
#40179 = CARTESIAN_POINT ( 'NONE',  ( 6.013528089337225602, 7.174620582783560963, 1.187335689305318853 ) ) ;
#40180 = CARTESIAN_POINT ( 'NONE',  ( -3.811250578772977349, 7.460559751961507224, -0.7216878364870458196 ) ) ;
#40181 = CARTESIAN_POINT ( 'NONE',  ( 0.01216826571975513152, -1.911853497171299265, -0.04704278909201110859 ) ) ;
#40182 = CARTESIAN_POINT ( 'NONE',  ( 1.639140867700689785, -1.278921918198316465, -1.223650632631252622 ) ) ;
#40183 = PRESENTATION_LAYER_ASSIGNMENT (  '', '', ( #202798 ) ) ;
#40184 = CARTESIAN_POINT ( 'NONE',  ( 6.410797320372758179, -0.5389820150160546941, -1.939520479220447902 ) ) ;
#40186 = CARTESIAN_POINT ( 'NONE',  ( 3.550306043379815257, -1.284141074626928392, 1.421643848488469031 ) ) ;
#40185 = CARTESIAN_POINT ( 'NONE',  ( -9.642873567817536795, 12.27310513391906532, 1.599625672291281386 ) ) ;
#40187 = CARTESIAN_POINT ( 'NONE',  ( 2.198393463710220264, 5.716542807637226886, 0.7998128361456462443 ) ) ;
#40188 = CARTESIAN_POINT ( 'NONE',  ( 3.877371502699510142, -0.1471681016796568819, 1.964127982587125398 ) ) ;
#40189 = CARTESIAN_POINT ( 'NONE',  ( -0.2104748580754166598, -0.006608320950483163522, -2.103482951484026753 ) ) ;
#40190 = CARTESIAN_POINT ( 'NONE',  ( -0.7500000000000006661, 10.95833333333333393, -1.299038105676657340 ) ) ;
#40191 = CARTESIAN_POINT ( 'NONE',  ( 2.834663617355744680, 0.2272019944037397543, 1.856728029318695627 ) ) ;
#40193 = ORIENTED_EDGE ( 'NONE', *, *, #29138, .T. ) ;
#40192 = CARTESIAN_POINT ( 'NONE',  ( 6.199779612253428773, -0.5740575353240050527, 1.626695425327763678 ) ) ;
#40195 = CARTESIAN_POINT ( 'NONE',  ( 2.412988153552339643, 5.758977245878946327, 0.7216878364870438212 ) ) ;
#40194 = CARTESIAN_POINT ( 'NONE',  ( 2.121956728516772639, -2.140194184088719531, 0.5379336890513550795 ) ) ;
#40196 = MECHANICAL_DESIGN_GEOMETRIC_PRESENTATION_REPRESENTATION (  '', ( #19443 ), #140576 ) ;
#40197 = CARTESIAN_POINT ( 'NONE',  ( 0.6823417656249917140, 3.905208333674754950, 1.181850606188765695 ) ) ;
#40198 = CARTESIAN_POINT ( 'NONE',  ( 0.1685210592646404493, -0.8794871949406095624, -1.863628177300826305 ) ) ;
#40199 = CARTESIAN_POINT ( 'NONE',  ( 6.916630921265960019, 11.22115317478565188, 0.7998128361456462443 ) ) ;
#40200 = CARTESIAN_POINT ( 'NONE',  ( -6.549078289569701283, -6.948428148671524696, 6.549078289569724376 ) ) ;
#40201 = CARTESIAN_POINT ( 'NONE',  ( 9.579665964948882007, -7.473374494045003757, 1.734723475976807094E-15 ) ) ;
#40202 = CARTESIAN_POINT ( 'NONE',  ( 0.1747926744264452492, 5.725295659261265158, -2.449351454080525681 ) ) ;
#40203 = AXIS2_PLACEMENT_3D ( 'NONE', #101807, #54131, #137525 ) ;
#40204 = DIRECTION ( 'NONE',  ( 1.000000000000000000, -5.578564026256504688E-16, 0.000000000000000000 ) ) ;
#40205 = ORIENTED_EDGE ( 'NONE', *, *, #146727, .T. ) ;
#40206 = CARTESIAN_POINT ( 'NONE',  ( 2.066927875543830950, 1.535623996113824496, -1.388825173883188713 ) ) ;
#40207 = CARTESIAN_POINT ( 'NONE',  ( -1.500000000000011324, 3.670833333333356485, 0.8660254037844403729 ) ) ;
#40208 = CARTESIAN_POINT ( 'NONE',  ( 5.311043488251262268, 7.219303374425030562, -1.599625672291256295 ) ) ;
#40209 = CARTESIAN_POINT ( 'NONE',  ( -6.198085906554800850, 7.039857339855744023, 1.052733950999720003 ) ) ;
#40210 = CARTESIAN_POINT ( 'NONE',  ( 1.172527652694483669, 0.8205418800426617087, 1.845675728695548745 ) ) ;
#40211 = CARTESIAN_POINT ( 'NONE',  ( -2.353344407399531160E-15, 2.999999999999989342, 1.857347330825967369 ) ) ;
#40212 = CARTESIAN_POINT ( 'NONE',  ( -0.6823417656250212460, 3.801041667008085767, 1.181850606188767472 ) ) ;
#40213 = VECTOR ( 'NONE', #48091, 1000.000000000000000 ) ;
#40215 = CARTESIAN_POINT ( 'NONE',  ( 8.093854517678360949, 12.38665467069271386, 1.040834085586084257E-14 ) ) ;
#40214 = CARTESIAN_POINT ( 'NONE',  ( 0.1749903794560592474, 0.7218944060462629819, -2.038148089257747930 ) ) ;
#40216 = CARTESIAN_POINT ( 'NONE',  ( 5.712267477471262289, -1.587595409608580255, -1.242535230690837489 ) ) ;
#40217 = CARTESIAN_POINT ( 'NONE',  ( 6.016788071399586713, 0.1949370894720331426, 1.905806522959735627 ) ) ;
#40218 = DIRECTION ( 'NONE',  ( 0.000000000000000000, 0.000000000000000000, -1.000000000000000000 ) ) ;
#40219 = CARTESIAN_POINT ( 'NONE',  ( 4.071962858106247474, -1.261020321617589479, 1.792237525612811355 ) ) ;
#40220 = CARTESIAN_POINT ( 'NONE',  ( -1.500000000000013101, 2.160416667349489561, -0.8660254037844313801 ) ) ;
#40221 = CARTESIAN_POINT ( 'NONE',  ( 2.443496805918866865, -1.782974011999260977, 0.6919810379762068031 ) ) ;
#40222 = CARTESIAN_POINT ( 'NONE',  ( -4.205000198532790279, 8.057583998263570635, 0.7998128361456341429 ) ) ;
#40223 = CARTESIAN_POINT ( 'NONE',  ( 3.673896439178911066, 7.230036912443299713, 0.7216878364870317197 ) ) ;
#40225 = CARTESIAN_POINT ( 'NONE',  ( 6.275037739279882842, 1.841983620878117733, -1.043829292874172143 ) ) ;
#40224 = CARTESIAN_POINT ( 'NONE',  ( -4.912887863224139728, 4.752532773970169266, -0.2786491325915474437 ) ) ;
#40226 = CARTESIAN_POINT ( 'NONE',  ( -1.402160292154681736E-14, 10.48437500034139447, 1.575800808251682339 ) ) ;
#40228 = CARTESIAN_POINT ( 'NONE',  ( -6.200875153403786477, 8.327716660428123419, -1.599625672291271394 ) ) ;
#40227 = CARTESIAN_POINT ( 'NONE',  ( 6.286699343557897279, 1.907799665397521105, -1.078441415684105120 ) ) ;
#40230 = ORIENTED_EDGE ( 'NONE', *, *, #159606, .F. ) ;
#40229 = CARTESIAN_POINT ( 'NONE',  ( 2.801416971846592219, -0.5432927088015163664, 1.637025921142007956 ) ) ;
#40231 = CARTESIAN_POINT ( 'NONE',  ( 5.994406619193555663, -1.133004004027007516, 1.792352430775605798 ) ) ;
#40232 = CARTESIAN_POINT ( 'NONE',  ( 6.109920781252839994, 10.27999134477033216, 1.040834085586084257E-14 ) ) ;
#40233 = CARTESIAN_POINT ( 'NONE',  ( 4.150767584078112193, 7.994312614733129152, 0.7998128361456321445 ) ) ;
#40234 = CARTESIAN_POINT ( 'NONE',  ( -3.023105066167323329, 5.702484939155337607, -2.420000000000000373 ) ) ;
#40235 = CARTESIAN_POINT ( 'NONE',  ( 0.2210476084268316321, -1.750679471464357650, -0.8856473702157914296 ) ) ;
#40236 = CARTESIAN_POINT ( 'NONE',  ( 6.825099317097807372, -8.105676417795693922, -6.608557002163611749 ) ) ;
#40237 = CARTESIAN_POINT ( 'NONE',  ( 4.306686350635271054, 8.176217842383143974, -0.7998128361456221525 ) ) ;
#40238 = CARTESIAN_POINT ( 'NONE',  ( 2.020417662918754687, 3.956598013261175772, -11.36521191596581737 ) ) ;
#40239 = ORIENTED_EDGE ( 'NONE', *, *, #51077, .F. ) ;
#40240 =( NAMED_UNIT ( * ) PLANE_ANGLE_UNIT ( ) SI_UNIT ( $, .RADIAN. ) );
#40241 = VERTEX_POINT ( 'NONE', #51632 ) ;
#40242 = CARTESIAN_POINT ( 'NONE',  ( 2.736723853829028830, 1.706320744115387811, 0.6085963735071827641 ) ) ;
#40243 = EDGE_LOOP ( 'NONE', ( #103237, #49351, #15970, #64840 ) ) ;
#40244 = CARTESIAN_POINT ( 'NONE',  ( 8.218213668177886788, 12.73966637951625813, 0.7998128361456462443 ) ) ;
#40245 = CARTESIAN_POINT ( 'NONE',  ( 4.492547798081839794, 6.334668079219206049, 1.599625672291262513 ) ) ;
#40246 = CARTESIAN_POINT ( 'NONE',  ( 3.316878987808123735, 1.426168316962544091, -1.116757653536442740 ) ) ;
#40247 = CARTESIAN_POINT ( 'NONE',  ( 7.471952054462754234, 8.850270497362297206, 1.082531754730549078 ) ) ;
#40248 = DIRECTION ( 'NONE',  ( -3.330669073875477510E-16, 2.265265487380573707E-16, 1.000000000000000000 ) ) ;
#40249 = CARTESIAN_POINT ( 'NONE',  ( 5.856753424380153561, 5.998585917076054486, 0.3190708477142957245 ) ) ;
#40251 = CARTESIAN_POINT ( 'NONE',  ( 0.6823417656249969321, 14.77604166700806410, -1.181850606188757036 ) ) ;
#40250 = CARTESIAN_POINT ( 'NONE',  ( 5.002340964340571183, 1.856068601349126324, 0.1372510170762584192 ) ) ;
#40252 = CARTESIAN_POINT ( 'NONE',  ( 2.671383988363975170, 1.356552116283934240, 1.352788525452413237 ) ) ;
#40253 = CARTESIAN_POINT ( 'NONE',  ( 0.7096328715897933792, -1.817275359149352676, 0.1739118742359047065 ) ) ;
#40254 = LINE ( 'NONE', #139903, #166572 ) ;
#40255 = CARTESIAN_POINT ( 'NONE',  ( -11.13243988973272636, 5.430794512910079419, -4.010128837087161280 ) ) ;
#40256 = CARTESIAN_POINT ( 'NONE',  ( 4.920187338115698417, 7.999083482620499730, 0.9937779052983791717 ) ) ;
#40257 = CARTESIAN_POINT ( 'NONE',  ( 9.165183341830644537, 14.44137815449902895, 8.758053443030863860 ) ) ;
#40258 = DIRECTION ( 'NONE',  ( 0.000000000000000000, 0.7071067811865432429, 0.7071067811865517916 ) ) ;
#40259 = DIRECTION ( 'NONE',  ( 0.000000000000000000, -1.000000000000000000, 0.000000000000000000 ) ) ;
#40260 = CARTESIAN_POINT ( 'NONE',  ( 7.022760382198770301, 8.255937203062467589, -1.082531754730543083 ) ) ;
#40261 = CARTESIAN_POINT ( 'NONE',  ( -4.711622075948912247, 5.455646162483875017, -1.199719254218446718 ) ) ;
#40262 = CARTESIAN_POINT ( 'NONE',  ( 6.661184041420940005, -7.215597533173327527, -6.773376349083132908 ) ) ;
#40263 = CARTESIAN_POINT ( 'NONE',  ( 1.869195317527425404, 2.000202809997845499, -0.6082070056973082339 ) ) ;
#40264 = CARTESIAN_POINT ( 'NONE',  ( 6.821331454403446237, -0.1310627394537598467, 1.896496729248610125 ) ) ;
#40265 = CARTESIAN_POINT ( 'NONE',  ( -5.032047568966410367, 9.022472597102808578, 1.214306433183764966E-14 ) ) ;
#40266 = CARTESIAN_POINT ( 'NONE',  ( 2.098414945899258033, -0.4839449910110822373, -1.760204267430766301 ) ) ;
#40267 = CARTESIAN_POINT ( 'NONE',  ( 3.106307083854151774, -2.204334110825040494, 0.1085914373066959593 ) ) ;
#40268 = CARTESIAN_POINT ( 'NONE',  ( 0.000000000000000000, 12.31951671548121219, 0.000000000000000000 ) ) ;
#40269 = CARTESIAN_POINT ( 'NONE',  ( 1.054777118923880597, 0.3758132965740559883, 1.874924941132802836 ) ) ;
#40270 = CARTESIAN_POINT ( 'NONE',  ( 1.135132829348266092, -0.04487231981731241992, -1.969206670302141804 ) ) ;
#40271 = CARTESIAN_POINT ( 'NONE',  ( 3.561997098397641448, -1.302002156301942604, 1.441148521680717387 ) ) ;
#40272 = AXIS2_PLACEMENT_3D ( 'NONE', #12485, #69749, #151045 ) ;
#40273 = VERTEX_POINT ( 'NONE', #3899 ) ;
#40274 = CARTESIAN_POINT ( 'NONE',  ( 1.499999999999822586, 7.240846818246208905, 4.154462424328221104 ) ) ;
#40276 = CARTESIAN_POINT ( 'NONE',  ( 0.1388275050690327694, -0.1366109201720016320, -1.830645452005694951 ) ) ;
#40275 = CARTESIAN_POINT ( 'NONE',  ( -3.817502770699643388, 6.611447778194983194, 1.199719254218452935 ) ) ;
#40277 = CARTESIAN_POINT ( 'NONE',  ( 5.520104819419390907, 6.469152373191302985, 1.199719254218452935 ) ) ;
#40278 = CARTESIAN_POINT ( 'NONE',  ( 0.008219159353561588180, -7.627132808484223148, 9.567202289542827032 ) ) ;
#40279 = LINE ( 'NONE', #106389, #4812 ) ;
#40280 = CARTESIAN_POINT ( 'NONE',  ( -5.448397627845328550, 7.449826213943242514, 1.599625672291263179 ) ) ;
#40281 = CARTESIAN_POINT ( 'NONE',  ( 3.122796855005858241, 0.05607861761174406934, 2.191015320347329709 ) ) ;
#40282 = CARTESIAN_POINT ( 'NONE',  ( 0.1399997263886003374, 7.629137130509076492, -2.599723212958489516 ) ) ;
#40283 = VERTEX_POINT ( 'NONE', #153390 ) ;
#40284 = CARTESIAN_POINT ( 'NONE',  ( 5.528692779322568640, 9.672168352510192690, 0.7998128361456341429 ) ) ;
#40285 = CARTESIAN_POINT ( 'NONE',  ( 5.311496422476285062, 4.760750348442155833, -2.499999999999999556 ) ) ;
#40286 = CARTESIAN_POINT ( 'NONE',  ( 4.090329635444483358, -1.806102819543849769, -0.2658631594732660530 ) ) ;
#40287 = CARTESIAN_POINT ( 'NONE',  ( -8.663296969452339624, 13.05100419776235299, 1.040834085586084257E-14 ) ) ;
#40288 = CARTESIAN_POINT ( 'NONE',  ( -5.227029541856937023, 7.814379162078399332, 1.287352361829100733 ) ) ;
#40289 = DIRECTION ( 'NONE',  ( 0.000000000000000000, 0.000000000000000000, 1.000000000000000000 ) ) ;
#40290 = CARTESIAN_POINT ( 'NONE',  ( 4.961713530105988923, 1.850188064717460223, -0.2750520410098392654 ) ) ;
#40291 = CARTESIAN_POINT ( 'NONE',  ( 9.077347539549325717, 10.54899253668443393, -1.199719254218446718 ) ) ;
#40292 = CARTESIAN_POINT ( 'NONE',  ( 2.121591023604427306, -1.868723361717766096, 0.4677975013653943859 ) ) ;
#40293 = CARTESIAN_POINT ( 'NONE',  ( 6.350445966956749899, -1.952004966925089624, -0.1956573963535559180 ) ) ;
#40294 = ADVANCED_FACE ( 'NONE', ( #152322, #184797 ), #139290, .T. ) ;
#40295 = CARTESIAN_POINT ( 'NONE',  ( 0.7500000000000006661, 14.58333333333333748, 1.299038105676657340 ) ) ;
#40296 = CARTESIAN_POINT ( 'NONE',  ( -4.726989112658928072, 8.666571064744069020, 1.040834085586084257E-14 ) ) ;
#40297 = CARTESIAN_POINT ( 'NONE',  ( 5.671388329218120639, 5.511041227042920099, 1.040834085586084257E-14 ) ) ;
#40298 = EDGE_CURVE ( 'NONE', #45216, #56229, #200701, .T. ) ;
#40299 = CARTESIAN_POINT ( 'NONE',  ( -4.624739795592936353, 7.449261290616792763, -1.082531754730549967 ) ) ;
#40300 = AXIS2_PLACEMENT_3D ( 'NONE', #27389, #86259, #202105 ) ;
#40301 = SHAPE_REPRESENTATION ( 'rubber for air flow regulation', ( #200407 ), #135205 ) ;
#40302 = CARTESIAN_POINT ( 'NONE',  ( 0.5447201963149818082, -1.530340168762192254, 1.463345158046714056 ) ) ;
#40303 = AXIS2_PLACEMENT_3D ( 'NONE', #29949, #146916, #13676 ) ;
#40304 = CARTESIAN_POINT ( 'NONE',  ( -1.225000000000005640, 0.5625000006828015930, -1.734723475976807094E-15 ) ) ;
#40305 = CARTESIAN_POINT ( 'NONE',  ( -4.148431816101615155, 3.942184661647709198, 0.7216878364870317197 ) ) ;
#40306 = CARTESIAN_POINT ( 'NONE',  ( 5.506714918851105089, 0.5956099481174789156, 1.982760374633622424 ) ) ;
#40308 = CARTESIAN_POINT ( 'NONE',  ( -1.402160292154681736E-14, 2.509375000341417028, -1.575800808251660134 ) ) ;
#40307 = CARTESIAN_POINT ( 'NONE',  ( 0.9602180038516641147, -1.664555262390180257, -0.7873027242753791732 ) ) ;
#40309 = ORIENTED_EDGE ( 'NONE', *, *, #184415, .T. ) ;
#40310 = CARTESIAN_POINT ( 'NONE',  ( 4.782019082252658926, 1.911913310736196081, -1.275919496871528169 ) ) ;
#40311 = CARTESIAN_POINT ( 'NONE',  ( 6.643132081016124069, 7.813037518349371879, 1.082531754730558626 ) ) ;
#40313 = DIRECTION ( 'NONE',  ( 1.000000000000000000, -0.000000000000000000, -0.000000000000000000 ) ) ;
#40312 = CARTESIAN_POINT ( 'NONE',  ( 4.746763178560250651, 7.591621904078704297, 1.082531754730549078 ) ) ;
#40314 = B_SPLINE_CURVE_WITH_KNOTS ( 'NONE', 3,
 ( #1260, #117233, #100911, #167000, #112983, #150758, #178994, #30609 ),
 .UNSPECIFIED., .F., .F.,
 ( 4, 2, 2, 4 ),
 ( 0.0003130156513459784388, 0.0009018580307267097616, 0.001196279220417075613, 0.001490700410107441247 ),
 .UNSPECIFIED. ) ;
#40315 = CARTESIAN_POINT ( 'NONE',  ( 0.8324521645294904459, 2.259258938120102922, 0.3867697638584958186 ) ) ;
#40316 = CARTESIAN_POINT ( 'NONE',  ( -0.07804408512528809849, -9.997559919034475939, -9.579522898042005963 ) ) ;
#40317 = CARTESIAN_POINT ( 'NONE',  ( -5.264308783856126439, 9.363720357799287797, -0.7998128361456362523 ) ) ;
#40318 = CARTESIAN_POINT ( 'NONE',  ( 4.734287085814634644, 0.3336016870040105498, 1.912933106389144822 ) ) ;
#40319 = ORIENTED_EDGE ( 'NONE', *, *, #6983, .T. ) ;
#40321 = EDGE_CURVE ( 'NONE', #10807, #201966, #154464, .T. ) ;
#40320 = CARTESIAN_POINT ( 'NONE',  ( 7.890482213029013536, 12.14938698193514277, 1.040834085586084257E-14 ) ) ;
#40322 = ORIENTED_EDGE ( 'NONE', *, *, #49463, .F. ) ;
#40323 = CARTESIAN_POINT ( 'NONE',  ( 6.521744167503259249, -0.4122283346772101509, 1.874327247564554266 ) ) ;
#40324 = CARTESIAN_POINT ( 'NONE',  ( 1.066563130004109405, -1.557762288434235476, -0.7409518577887274082 ) ) ;
#40325 = CARTESIAN_POINT ( 'NONE',  ( 6.139861302770143858, 2.010801613648224961, -0.1531635369260639090 ) ) ;
#40327 = SURFACE_STYLE_USAGE ( .BOTH. , #87997 ) ;
#40326 = CARTESIAN_POINT ( 'NONE',  ( -8.422639742587602285, 10.84949900448412841, -1.599625672291263179 ) ) ;
#40328 = CARTESIAN_POINT ( 'NONE',  ( -3.285556943750000514, -0.9260416661887070910, -1.896917185911906500 ) ) ;
#40330 = CARTESIAN_POINT ( 'NONE',  ( 1.252431388357349684, -1.398210551426328330, 1.084949785890441110 ) ) ;
#40329 = CARTESIAN_POINT ( 'NONE',  ( 2.326223132658828963, 2.028069097222063188, 0.5071170776438630456 ) ) ;
#40331 = DIRECTION ( 'NONE',  ( 3.330669073875478989E-16, -3.540251991789410786E-16, -1.000000000000000000 ) ) ;
#40332 = CARTESIAN_POINT ( 'NONE',  ( 3.890815911290066875, 1.937189890886330756, -1.225201777657213498 ) ) ;
#40333 = CARTESIAN_POINT ( 'NONE',  ( 2.712550014960776856, -0.1704709713557898410, 1.731945008791212270 ) ) ;
#40334 = CARTESIAN_POINT ( 'NONE',  ( 3.680148631105580215, 6.380924938676771241, -1.199719254218446718 ) ) ;
#40335 = CARTESIAN_POINT ( 'NONE',  ( 3.006218798242997980, -0.8556837461295877523, 1.940463308995137526 ) ) ;
#40336 = CARTESIAN_POINT ( 'NONE',  ( 0.3282377607281209420, 0.6361645503674333568, 1.224999999999965894 ) ) ;
#40337 = CARTESIAN_POINT ( 'NONE',  ( 2.284178307277694664, -1.682821195468919395, 0.4169209145809901762 ) ) ;
#40338 = CARTESIAN_POINT ( 'NONE',  ( -1.360316468750007779, 2.171875000341411344, -4.336808689942017736E-14 ) ) ;
#40339 = CARTESIAN_POINT ( 'NONE',  ( 2.119380567849386665, 0.3219547178687692801, -1.832826937841147252 ) ) ;
#40340 = CARTESIAN_POINT ( 'NONE',  ( 1.926474581872784420, 1.115185415580312700, 1.862746952601635808 ) ) ;
#40341 = CARTESIAN_POINT ( 'NONE',  ( 6.145923705696426431, 6.064665832934283962, 0.7998128361456341429 ) ) ;
#40342 = CARTESIAN_POINT ( 'NONE',  ( 3.889861467948489082, -2.010801299972611478, 0.1531677096566556595 ) ) ;
#40343 = CARTESIAN_POINT ( 'NONE',  ( 2.281250000000002220, 0.7852924748301068902, 1.895863743164037718 ) ) ;
#40344 = CARTESIAN_POINT ( 'NONE',  ( -0.7500000000000215383, 2.472916667349486897, 1.299038105676671107 ) ) ;
#40345 = CARTESIAN_POINT ( 'NONE',  ( 0.4988883441144418840, 1.603466095971857852, -1.067369714357151222 ) ) ;
#40346 = CARTESIAN_POINT ( 'NONE',  ( 0.6823417656249969321, 14.02604166700806232, -1.181850606188757036 ) ) ;
#40347 = CARTESIAN_POINT ( 'NONE',  ( 4.465202103771027886, -1.783222260262930181, 1.324459880397445666 ) ) ;
#40348 = VERTEX_POINT ( 'NONE', #151265 ) ;
#40349 = CARTESIAN_POINT ( 'NONE',  ( -2.449742653233043743, 3.299999999999976730, -0.4000000000000339950 ) ) ;
#40350 = CARTESIAN_POINT ( 'NONE',  ( 1.499999999999987566, -0.2249999999999821587, 0.000000000000000000 ) ) ;
#40352 = ADVANCED_FACE ( 'NONE', ( #53757 ), #72113, .F. ) ;
#40351 = CARTESIAN_POINT ( 'NONE',  ( 6.414979237560321401, 10.63589287712906462, 1.040834085586084257E-14 ) ) ;
#40353 = CARTESIAN_POINT ( 'NONE',  ( -1.364683531250014514, -0.5114583329919092369, -0.7879004041258359514 ) ) ;
#40354 = CARTESIAN_POINT ( 'NONE',  ( 0.2588218971089132348, 2.215798623493638875, 0.1571155685827912152 ) ) ;
#40356 = CARTESIAN_POINT ( 'NONE',  ( 4.685966490639408732, -1.205361723144786845, -1.547842780461285983 ) ) ;
#40355 = AXIS2_PLACEMENT_3D ( 'NONE', #122292, #67283, #68356 ) ;
#40357 = CARTESIAN_POINT ( 'NONE',  ( 7.782016984564043227, 12.02284421539267356, 0.7216878364870438212 ) ) ;
#40358 = FILL_AREA_STYLE ('',( #26212 ) ) ;
#40359 = CARTESIAN_POINT ( 'NONE',  ( 5.343176995970949861, -1.944282970029135083, 1.156607043288411019 ) ) ;
#40360 = CARTESIAN_POINT ( 'NONE',  ( -6.468648687495877958, 6.719380688266201496, 0.000000000000000000 ) ) ;
#40361 = CARTESIAN_POINT ( 'NONE',  ( 3.596185909054748553, 0.9300860933913506212, -1.841171126807969349 ) ) ;
#40362 = CARTESIAN_POINT ( 'NONE',  ( -5.032047568966410367, 9.022472597102808578, 1.214306433183764966E-14 ) ) ;
#40364 = EDGE_CURVE ( 'NONE', #133393, #29771, #75620, .T. ) ;
#40363 = CARTESIAN_POINT ( 'NONE',  ( -1.499999999999997780, 2.181250000682817713, 1.214306433183764966E-14 ) ) ;
#40365 = CARTESIAN_POINT ( 'NONE',  ( -1.364683531250010295, 5.551041667008087543, -0.7879004041258300672 ) ) ;
#40366 = CARTESIAN_POINT ( 'NONE',  ( 4.358574879328508622, -1.387578095181252413, 1.254630796652965730 ) ) ;
#40367 = CARTESIAN_POINT ( 'NONE',  ( 3.234723362560991244, 1.734343004352358664, -0.003563068559135627086 ) ) ;
#40368 = CARTESIAN_POINT ( 'NONE',  ( 2.999246388560794951, -1.738348057599903074, 0.08809733484680536131 ) ) ;
#40369 = CARTESIAN_POINT ( 'NONE',  ( 0.3984806668858055789, -0.7796899918033869392, -2.155833124811225687 ) ) ;
#40370 = CARTESIAN_POINT ( 'NONE',  ( 0.7982362974770088604, -0.7925503509537080715, 2.059710425106767939 ) ) ;
#40371 = CARTESIAN_POINT ( 'NONE',  ( 4.476172314981810452, -2.028359691925533781, -0.5064535023821553628 ) ) ;
#40372 = CARTESIAN_POINT ( 'NONE',  ( 6.017518264666532168, -1.080727962582687773, -1.613252759315900731 ) ) ;
#40373 = ADVANCED_FACE ( 'NONE', ( #4961 ), #131532, .T. ) ;
#40374 = DIRECTION ( 'NONE',  ( 8.638326563840814399E-31, -0.000000000000000000, 1.000000000000000000 ) ) ;
#40375 = FILL_AREA_STYLE ('',( #141104 ) ) ;
#40376 = CARTESIAN_POINT ( 'NONE',  ( 0.7564826839323666174, 1.942540863013635821, -0.5404934282097761944 ) ) ;
#40377 = CARTESIAN_POINT ( 'NONE',  ( 1.248456593208754795, 1.040400552670465162, -1.847740296886036582 ) ) ;
#40378 = CARTESIAN_POINT ( 'NONE',  ( 0.000000000000000000, 0.000000000000000000, 0.000000000000000000 ) ) ;
#40379 = CARTESIAN_POINT ( 'NONE',  ( -9.073431116043565225, 11.60875560684942265, -1.599625672291263179 ) ) ;
#40380 = CARTESIAN_POINT ( 'NONE',  ( 5.459129407796876166, 9.520734742405036144, 1.040834085586084257E-14 ) ) ;
#40381 = CARTESIAN_POINT ( 'NONE',  ( 0.9174905902279941738, -4.140925090156048149, -0.4108596822587322062 ) ) ;
#40382 = CARTESIAN_POINT ( 'NONE',  ( 4.758326833623739205, 0.7015320795021735556, 1.685726030614169924 ) ) ;
#40383 = VERTEX_POINT ( 'NONE', #114053 ) ;
#40384 = CARTESIAN_POINT ( 'NONE',  ( -8.106849506328558164, 8.422688943663599659, 0.000000000000000000 ) ) ;
#40385 = CYLINDRICAL_SURFACE ( 'NONE', #8902, 12.00000000000000178 ) ;
#40386 = CARTESIAN_POINT ( 'NONE',  ( -3.285556943750000514, -2.676041666188707424, -1.896917185911906500 ) ) ;
#40387 = CARTESIAN_POINT ( 'NONE',  ( -7.100719765255177229, 9.307259030929609267, -1.599625672291263179 ) ) ;
#40388 = CARTESIAN_POINT ( 'NONE',  ( 1.951431513787309724, -1.802353211750299167, 0.9118321038049399530 ) ) ;
#40389 = CARTESIAN_POINT ( 'NONE',  ( 5.368293279414073638, 1.083412401764087374, 1.922438065789177308 ) ) ;
#40390 = CARTESIAN_POINT ( 'NONE',  ( -5.483346782084204563, 5.361935765378481378, 0.000000000000000000 ) ) ;
#40391 = CARTESIAN_POINT ( 'NONE',  ( 2.641259143913599949, 1.703662207083409763, -0.7491738860408488909 ) ) ;
#40392 = CARTESIAN_POINT ( 'NONE',  ( 8.543609354905870035, 13.11929468069890525, 0.7998128361456462443 ) ) ;
#40393 = CARTESIAN_POINT ( 'NONE',  ( 4.421367491832275398, 8.172362817197386775, 0.7216878364870369378 ) ) ;
#40394 = VERTEX_POINT ( 'NONE', #111917 ) ;
#40395 = ORIENTED_EDGE ( 'NONE', *, *, #151879, .T. ) ;
#40396 = CARTESIAN_POINT ( 'NONE',  ( -3.716906668440817185, 7.488141546489591072, 0.7998128361456341429 ) ) ;
#40397 =( BOUNDED_CURVE ( )  B_SPLINE_CURVE ( 2, ( #2589, #446, #180313, #163004, #182419, #117503, #118568 ),
 .UNSPECIFIED., .F., .T. ) 
 B_SPLINE_CURVE_WITH_KNOTS ( ( 3, 2, 2, 3 ),
 ( 0.2500000000000002776, 0.2541666666666668184, 0.2583333333333333592, 0.2624999999999999001 ),
 .UNSPECIFIED. ) 
 CURVE ( )  GEOMETRIC_REPRESENTATION_ITEM ( )  RATIONAL_B_SPLINE_CURVE ( ( 0.9999999999999911182, 0.8660254037844475894, 1.000000000000000000, 0.8660254037844387076, 1.000000000000000000, 0.8660254037844422603, 0.9999999999999964473 ) ) 
 REPRESENTATION_ITEM ( '' )  );
#40398 = CARTESIAN_POINT ( 'NONE',  ( -9.321394304595349567, 10.83371376257142416, 1.199719254218462483 ) ) ;
#40399 = CARTESIAN_POINT ( 'NONE',  ( 5.057177669875371429, -1.544152220135000420, -0.9737345633797565014 ) ) ;
#40401 = CARTESIAN_POINT ( 'NONE',  ( -4.418902842294746947, 7.322973332268160718, -1.241058569461401362 ) ) ;
#40400 = CARTESIAN_POINT ( 'NONE',  ( -7.533490631048818109, 8.818102486758951031, -1.199719254218452047 ) ) ;
#40402 = CARTESIAN_POINT ( 'NONE',  ( 6.463557619869761517, 6.860074278669063830, -0.6545079704341187909 ) ) ;
#40403 = CARTESIAN_POINT ( 'NONE',  ( 0.1452960159114678740, -0.1365383601019970750, -1.704228001402931625 ) ) ;
#40404 = CARTESIAN_POINT ( 'NONE',  ( 0.4975142532120572225, -0.5819891871022980778, -1.640261313346396133 ) ) ;
#40405 = CARTESIAN_POINT ( 'NONE',  ( 5.338606043529401823, 2.272755431710461238, 0.3992410602531944464 ) ) ;
#40406 = CARTESIAN_POINT ( 'NONE',  ( 4.420840606507738357, 7.315341919971147355, 1.199719254218451159 ) ) ;
#40407 = CARTESIAN_POINT ( 'NONE',  ( 6.854756222516505737, -1.675677847961650313, 1.365199464886861946 ) ) ;
#40408 = CARTESIAN_POINT ( 'NONE',  ( 5.361359679200154105, 8.342337828120466980, 1.199719254218462483 ) ) ;
#40409 = CARTESIAN_POINT ( 'NONE',  ( 5.958471553546731414, 1.734833135700924345, 1.507719323494296937 ) ) ;
#40410 = CARTESIAN_POINT ( 'NONE',  ( 1.220146605508150803E-14, 11.46875000068279604, -1.499999999999998446 ) ) ;
#40411 = CARTESIAN_POINT ( 'NONE',  ( -4.911796789900812144, 8.952456364851418158, 0.7998128361456291469 ) ) ;
#40412 = CARTESIAN_POINT ( 'NONE',  ( 5.506679003988666388, 1.415762158562785533, -1.222804595763474333 ) ) ;
#40414 = CARTESIAN_POINT ( 'NONE',  ( -5.496904935697871863, 5.377753611261092637, 0.7998128361456281477 ) ) ;
#40413 = CARTESIAN_POINT ( 'NONE',  ( 3.199369407753744454, 1.726971514772487559, -0.8218122705464236954 ) ) ;
#40415 = CARTESIAN_POINT ( 'NONE',  ( 5.321004863918796346, 2.037934703285459115, 0.8473243778325880715 ) ) ;
#40416 = CARTESIAN_POINT ( 'NONE',  ( 4.962167979565689002, -1.173633690672538865, 1.762117774576977602 ) ) ;
#40417 = CARTESIAN_POINT ( 'NONE',  ( 0.6124999999999828360, 0.9791666673494778816, -1.060881119635955327 ) ) ;
#40418 = CARTESIAN_POINT ( 'NONE',  ( 6.883263157960366918, 2.433703524355503411, 2.428201320676713237 ) ) ;
#40419 = CARTESIAN_POINT ( 'NONE',  ( 5.112833325684902341, 7.058334528089426740, -1.443375672974078761 ) ) ;
#40420 = CARTESIAN_POINT ( 'NONE',  ( -3.811250578772977349, 7.460559751961507224, -0.7216878364870458196 ) ) ;
#40421 = CARTESIAN_POINT ( 'NONE',  ( 6.147156607449644206, 0.2074554230099104890, 2.110329589018632657 ) ) ;
#40422 = CARTESIAN_POINT ( 'NONE',  ( 1.940857006665818174, 2.282658722630509729, 0.3375727702036589450 ) ) ;
#40423 = CARTESIAN_POINT ( 'NONE',  ( 3.314850587115983238, -1.487306837207631238, 1.279512770686676681 ) ) ;
#40424 = PRESENTATION_STYLE_ASSIGNMENT (( #188789 ) ) ;
#40425 = CARTESIAN_POINT ( 'NONE',  ( 6.332891742935283119, -1.956728314951971637, -0.6523575503349694493 ) ) ;
#40426 = CARTESIAN_POINT ( 'NONE',  ( 3.063779527008304360, 6.518233848244248563, 0.7216878364870317197 ) ) ;
#40427 = CARTESIAN_POINT ( 'NONE',  ( 3.705121118284530279, 7.544668081299086282, -1.734723475976807094E-15 ) ) ;
#40429 = ORIENTED_EDGE ( 'NONE', *, *, #31198, .T. ) ;
#40428 = B_SPLINE_CURVE_WITH_KNOTS ( 'NONE', 3,
 ( #141016, #58655, #26143, #92256, #158302, #147381, #13084, #210217, #81304, #63986 ),
 .UNSPECIFIED., .F., .F.,
 ( 4, 3, 3, 4 ),
 ( 1.060539725738902859E-15, 3.125190826550851492E-05, 5.893811830794473683E-05, 8.663425284181113851E-05 ),
 .UNSPECIFIED. ) ;
#40430 = CARTESIAN_POINT ( 'NONE',  ( 5.928922775424462444, -1.700964743930567513, 1.082835439959836776 ) ) ;
#40431 = CARTESIAN_POINT ( 'NONE',  ( -9.134442807305063639, 11.67993591332117376, 1.599625672291281386 ) ) ;
#40432 = CARTESIAN_POINT ( 'NONE',  ( -0.07900062026858570285, 7.629137130509076492, -2.773896239169175271 ) ) ;
#40433 = CARTESIAN_POINT ( 'NONE',  ( -11.69243366784185945, 8.407932920124673970, 1.097391832464843286 ) ) ;
#40435 = AXIS2_PLACEMENT_3D ( 'NONE', #177959, #208291, #79381 ) ;
#40434 = CARTESIAN_POINT ( 'NONE',  ( 2.079201016916156330, 2.024566655493876155, 0.7844037353602287821 ) ) ;
#40436 = CARTESIAN_POINT ( 'NONE',  ( 0.000000000000000000, 8.920000000000001705, 0.000000000000000000 ) ) ;
#40437 = CARTESIAN_POINT ( 'NONE',  ( 0.2113915902133572944, 1.759560880827226947, -1.183302968686468226 ) ) ;
#40438 = CARTESIAN_POINT ( 'NONE',  ( 1.499999999999987121, 2.327083334016154303, -0.8660254037844262731 ) ) ;
#40439 = CARTESIAN_POINT ( 'NONE',  ( -3.530628709500676976, 14.55202870934159520, -11.43095269779774448 ) ) ;
#40440 = CARTESIAN_POINT ( 'NONE',  ( 5.622977593387656015, 6.244972703327866803, 1.018919728668438385 ) ) ;
#40441 = CARTESIAN_POINT ( 'NONE',  ( 5.502223863662048409, 7.574938096329499437, 1.338028725624084148 ) ) ;
#40442 = CARTESIAN_POINT ( 'NONE',  ( 0.6321923500852930644, 1.061553894661429576, -1.766199267744901658 ) ) ;
#40444 = CARTESIAN_POINT ( 'NONE',  ( 0.000000000000000000, 2.499999999999998668, 0.000000000000000000 ) ) ;
#40443 = CARTESIAN_POINT ( 'NONE',  ( -10.66756793585402363, 11.33991743478486391, 0.7998128361456462443 ) ) ;
#40445 = CARTESIAN_POINT ( 'NONE',  ( -0.6823417656250212460, 1.051041667008083325, 1.181850606188755259 ) ) ;
#40446 = EDGE_LOOP ( 'NONE', ( #45438, #21366, #70838, #62490, #74152, #186619 ) ) ;
#40447 = CARTESIAN_POINT ( 'NONE',  ( 3.809155001108741612, 1.613891119516493777, -1.025466636117925212 ) ) ;
#40448 = CARTESIAN_POINT ( 'NONE',  ( 4.979261681649114202, 1.650653357529890730, -0.6390028274257038010 ) ) ;
#40449 = CARTESIAN_POINT ( 'NONE',  ( 4.715203562502613188, 8.723097599553565118, 0.7998128361456341429 ) ) ;
#40450 = CARTESIAN_POINT ( 'NONE',  ( -5.088387723830502196, 4.830873854090670605, -0.7998128361456221525 ) ) ;
#40451 = CARTESIAN_POINT ( 'NONE',  ( 0.4217375466794699435, -1.802849824360297060, 0.1778772001973498718 ) ) ;
#40453 = CARTESIAN_POINT ( 'NONE',  ( 6.134394303309665730, 0.6061128391178214336, 1.817247008912269646 ) ) ;
#40452 = CARTESIAN_POINT ( 'NONE',  ( -0.4734754237523640663, 6.885074608495208359, -3.701908037242890526 ) ) ;
#40454 = CARTESIAN_POINT ( 'NONE',  ( 1.064989848632340363, 1.568927673159369762, -1.351003706900590018 ) ) ;
#40455 = CARTESIAN_POINT ( 'NONE',  ( -1.364683531250012516, 0.5927083336747520637, 0.7879004041258379498 ) ) ;
#40456 = CARTESIAN_POINT ( 'NONE',  ( 5.981297838379462384, 1.727768277425823396, -0.7175292643646775659 ) ) ;
#40457 = CARTESIAN_POINT ( 'NONE',  ( 2.719161800852238464, -0.1789327596440904167, 1.816892639718168390 ) ) ;
#40459 = CARTESIAN_POINT ( 'NONE',  ( 5.279289985772466665, 7.652873027719338417, 1.222721368963412214 ) ) ;
#40458 = CARTESIAN_POINT ( 'NONE',  ( 5.883472226557855400, 2.040502603023553796, -0.8411249186189362348 ) ) ;
#40460 = CARTESIAN_POINT ( 'NONE',  ( 1.364683531249988757, 0.1343750003414204142, 0.000000000000000000 ) ) ;
#40461 = AXIS2_PLACEMENT_3D ( 'NONE', #76577, #109161, #39824 ) ;
#40462 = CARTESIAN_POINT ( 'NONE',  ( 3.174340740746087075, -1.014436240984006865, -1.795896229016210821 ) ) ;
#40463 = CARTESIAN_POINT ( 'NONE',  ( -8.525379664894808585, 8.840697785332414682, -0.7998128361456291469 ) ) ;
#40464 = CARTESIAN_POINT ( 'NONE',  ( 8.727698198895078363, 11.20540053684285553, -1.599625672291257406 ) ) ;
#40465 = CARTESIAN_POINT ( 'NONE',  ( 5.030238685870051185, 5.827365540725222282, -1.199719254218452047 ) ) ;
#40466 = CARTESIAN_POINT ( 'NONE',  ( -0.005636871015592820333, -9.933099847254503345, -10.91969863820289177 ) ) ;
#40467 = COLOUR_RGB ( '', 0.72549020, 0.75294118, 0.79215686) ;
#40468 = CARTESIAN_POINT ( 'NONE',  ( 6.391088794356012848, 0.1989163192229244648, 2.060770550043041993 ) ) ;
#40469 = CARTESIAN_POINT ( 'NONE',  ( -1.402160292154681736E-14, -0.3656249996585805295, 1.575800808251672791 ) ) ;
#40470 = CARTESIAN_POINT ( 'NONE',  ( 3.427187520701843404, 0.04928524951339217919, 2.161187641841005647 ) ) ;
#40472 = CARTESIAN_POINT ( 'NONE',  ( 2.400770673373255448, 0.4268909467371252431, 1.914702609522442867 ) ) ;
#40471 = CARTESIAN_POINT ( 'NONE',  ( 4.793620647492384812, 1.883690600511141566, -0.7290150168693364519 ) ) ;
#40473 = CARTESIAN_POINT ( 'NONE',  ( 6.620655732516652847, 2.941130357193070033, 2.725706755162327966 ) ) ;
#40476 = CARTESIAN_POINT ( 'NONE',  ( 5.653386867218496370, 9.539442411822841805, 1.040834085586084257E-14 ) ) ;
#40475 = CARTESIAN_POINT ( 'NONE',  ( 3.475000000000000533, -0.2041666666666657748, 2.006292185433948827 ) ) ;
#40474 = FACE_OUTER_BOUND ( 'NONE', #163144, .T. ) ;
#40477 = CARTESIAN_POINT ( 'NONE',  ( -6.149505192250180663, 9.332117270003974951, -1.199719254218452047 ) ) ;
#40478 = CARTESIAN_POINT ( 'NONE',  ( 2.167204200501818612, 1.841733140229084853, -0.8216742516050157263 ) ) ;
#40480 = CARTESIAN_POINT ( 'NONE',  ( 1.965118028437739639, 0.3835514080770347500, 0.6713998180129714388 ) ) ;
#40479 = CARTESIAN_POINT ( 'NONE',  ( -3.228813138348844536, 6.918699094715619502, 0.7998128361456341429 ) ) ;
#40481 = CARTESIAN_POINT ( 'NONE',  ( -0.7500000000000215383, 5.472916667349482900, 1.299038105676671107 ) ) ;
#40482 = CARTESIAN_POINT ( 'NONE',  ( 6.064708884584704585, 0.6063723501847050334, 1.813766235492550560 ) ) ;
#40483 = FACE_OUTER_BOUND ( 'NONE', #189299, .T. ) ;
#40484 = CARTESIAN_POINT ( 'NONE',  ( 4.460269348771534581, 8.147471973634706544, -0.7216878364870207285 ) ) ;
#40486 = CARTESIAN_POINT ( 'NONE',  ( 4.482046101484723266, -2.016035353076811809, -0.04666016718203602753 ) ) ;
#40485 = CARTESIAN_POINT ( 'NONE',  ( -8.853111119599343937, 10.39134639669645566, 1.082531754730558626 ) ) ;
#40487 = CARTESIAN_POINT ( 'NONE',  ( 1.499999999999990896, 4.525000000000021672, 1.214306433183764966E-14 ) ) ;
#40488 = CARTESIAN_POINT ( 'NONE',  ( -1.364683531250014514, 15.40104166700806765, -0.7879004041258335089 ) ) ;
#40489 = CARTESIAN_POINT ( 'NONE',  ( 6.457991230880992362, 1.719707694194565484, -0.1327171722449934921 ) ) ;
#40490 = CARTESIAN_POINT ( 'NONE',  ( 7.700104897918568447, 7.948153567185284096, 0.000000000000000000 ) ) ;
#40491 = CARTESIAN_POINT ( 'NONE',  ( 8.270110514656026979, 10.67154823856396817, 1.443375672974076540 ) ) ;
#40492 = CARTESIAN_POINT ( 'NONE',  ( -0.4000000000000393241, 3.248764396332298965, 0.4641653677812256906 ) ) ;
#40493 = CARTESIAN_POINT ( 'NONE',  ( 4.270664716992385479, -1.744513905240049567, -0.6754176267826096369 ) ) ;
#40494 = CARTESIAN_POINT ( 'NONE',  ( -0.02900071798685524560, -0.004641455105012376459, -2.173770343569726649 ) ) ;
#40495 = AXIS2_PLACEMENT_3D ( 'NONE', #39709, #7184, #185934 ) ;
#40496 = CARTESIAN_POINT ( 'NONE',  ( 1.745070579777140418, -0.2997347613497360896, -2.048299739058518920 ) ) ;
#40497 = CARTESIAN_POINT ( 'NONE',  ( -2.331034670843834533E-15, -9.181223591647247773, -10.14523337821909976 ) ) ;
#40498 = VERTEX_POINT ( 'NONE', #176843 ) ;
#40499 = CARTESIAN_POINT ( 'NONE',  ( 3.715816618597135523, 6.492813934075403637, -1.199719254218453823 ) ) ;
#40500 = DIRECTION ( 'NONE',  ( -8.881784197001252323E-16, 0.000000000000000000, 1.000000000000000000 ) ) ;
#40501 = CARTESIAN_POINT ( 'NONE',  ( 6.639320575229251453, 0.008029245381881154262, 1.796863947021019481 ) ) ;
#40502 = CARTESIAN_POINT ( 'NONE',  ( 4.326460416092276162, 7.101268681199365496, -1.082531754730548412 ) ) ;
#40503 = CARTESIAN_POINT ( 'NONE',  ( 0.000000000000000000, 0.000000000000000000, 0.000000000000000000 ) ) ;
#40504 = VECTOR ( 'NONE', #78463, 1000.000000000000000 ) ;
#40505 = CARTESIAN_POINT ( 'NONE',  ( 6.914295152845067349, 11.01050207838719075, 1.040834085586084257E-14 ) ) ;
#40506 = EDGE_CURVE ( 'NONE', #134461, #179867, #160588, .T. ) ;
#40507 = CARTESIAN_POINT ( 'NONE',  ( 6.916630921265960019, 11.22115317478565188, 0.7998128361456462443 ) ) ;
#40509 = CARTESIAN_POINT ( 'NONE',  ( 6.503544296663656077, -1.856690447402360888, 0.4709783565581044940 ) ) ;
#40508 = CARTESIAN_POINT ( 'NONE',  ( -5.636439174979254396, 7.598931675607687453, -1.599625672291256295 ) ) ;
#40510 = CARTESIAN_POINT ( 'NONE',  ( -15.75000000000000000, 12.69999999999998153, 1.799999999999999600 ) ) ;
#40511 = CARTESIAN_POINT ( 'NONE',  ( -4.948362878863562742, 5.835806782504650236, 1.082531754730558626 ) ) ;
#40512 = FACE_OUTER_BOUND ( 'NONE', #154942, .T. ) ;
#40514 = ORIENTED_EDGE ( 'NONE', *, *, #200594, .F. ) ;
#40513 = CARTESIAN_POINT ( 'NONE',  ( 4.582292731738905722, 5.408724944192588424, -1.082531754730548412 ) ) ;
#40515 = CARTESIAN_POINT ( 'NONE',  ( -8.690413276679693766, 9.241163032322203819, 1.040834085586084257E-14 ) ) ;
#40516 =( GEOMETRIC_REPRESENTATION_CONTEXT ( 3 ) GLOBAL_UNCERTAINTY_ASSIGNED_CONTEXT ( ( #40121 ) ) GLOBAL_UNIT_ASSIGNED_CONTEXT ( ( #16299, #34697, #108313 ) ) REPRESENTATION_CONTEXT ( 'NONE', 'WORKASPACE' ) );
#40517 = CARTESIAN_POINT ( 'NONE',  ( 3.520547545725543515, 1.372905562624787024, -1.669742455111824508 ) ) ;
#40518 = CARTESIAN_POINT ( 'NONE',  ( -4.995253251992230581, 4.792493313604505367, 0.000000000000000000 ) ) ;
#40519 = CARTESIAN_POINT ( 'NONE',  ( 2.891631901464575272, 6.595597328342462262, 0.000000000000000000 ) ) ;
#40520 = CARTESIAN_POINT ( 'NONE',  ( 0.5277791401020451856, -0.3051165123582540994, 2.098401203810342786 ) ) ;
#40521 = CARTESIAN_POINT ( 'NONE',  ( 5.913091143547533513, 1.611232972626057247, 0.8583240166551918682 ) ) ;
#40522 = CARTESIAN_POINT ( 'NONE',  ( 1.282427153303007605, -1.922404290768309432, -0.4359020612285709473 ) ) ;
#40523 = CARTESIAN_POINT ( 'NONE',  ( 3.023589307540079041, -0.3687504995396119201, 1.876329818327879817 ) ) ;
#40524 = ORIENTED_EDGE ( 'NONE', *, *, #157408, .T. ) ;
#40525 = DIRECTION ( 'NONE',  ( -1.000000000000000000, 1.014813233446432150E-15, 1.972152263052529514E-31 ) ) ;
#40526 = CARTESIAN_POINT ( 'NONE',  ( 5.459413677600381654, 1.609035625656387802, 1.135536449648701041 ) ) ;
#40527 = CARTESIAN_POINT ( 'NONE',  ( 0.8670093773819181893, 1.871751486835357747, -0.5171616756182734198 ) ) ;
#40528 = VERTEX_POINT ( 'NONE', #60956 ) ;
#40529 = CARTESIAN_POINT ( 'NONE',  ( -5.152980901645737077, 8.169505597632108262, -1.199719254218453823 ) ) ;
#40531 = CARTESIAN_POINT ( 'NONE',  ( -1.225000000000038058, 1.333333334016162386, 0.7072540797572777205 ) ) ;
#40530 = CARTESIAN_POINT ( 'NONE',  ( -5.957882158562513908, 5.915560371269843465, -0.7998128361456362523 ) ) ;
#40532 = CARTESIAN_POINT ( 'NONE',  ( 6.251718229232841928, 8.387033582228703210, -1.443375672974078761 ) ) ;
#40534 = ORIENTED_EDGE ( 'NONE', *, *, #115776, .F. ) ;
#40533 = CARTESIAN_POINT ( 'NONE',  ( 4.986922676292999235, -1.801926769106906745, -0.6406197933803285949 ) ) ;
#40535 = EDGE_CURVE ( 'NONE', #212849, #116379, #211064, .T. ) ;
#40536 = CARTESIAN_POINT ( 'NONE',  ( 1.325528760500709780, -0.05309137938146882979, 2.206304558879538025 ) ) ;
#40537 = CARTESIAN_POINT ( 'NONE',  ( 9.453622214572620308, 4.518459228531092720, -7.392429638475873865 ) ) ;
#40538 = CARTESIAN_POINT ( 'NONE',  ( 6.586586637485376983, -1.237022783311360730, 1.588989491490456762 ) ) ;
#40539 = CARTESIAN_POINT ( 'NONE',  ( 0.3190191529055473874, 8.208688096292709346, 1.977123213039587268 ) ) ;
#40540 = CARTESIAN_POINT ( 'NONE',  ( 10.99663476780025206, -7.859187537802522883, -0.2753234695294711765 ) ) ;
#40541 = CARTESIAN_POINT ( 'NONE',  ( -3.929058411375426108, 5.499999999999998224, 0.7499999999999988898 ) ) ;
#40542 = CARTESIAN_POINT ( 'NONE',  ( 2.260293373024503616, -2.069953001785612479, 0.04851313490940312168 ) ) ;
#40543 = CARTESIAN_POINT ( 'NONE',  ( -5.768104287610143821, 8.816873204598778102, -1.199719254218440723 ) ) ;
#40544 = CARTESIAN_POINT ( 'NONE',  ( -4.651028767811522080, 8.324525799487361155, 0.4279074293446327171 ) ) ;
#40545 = CARTESIAN_POINT ( 'NONE',  ( 0.7608789386071808103, -1.564954856162886765, 1.491513986042219297 ) ) ;
#40546 = CARTESIAN_POINT ( 'NONE',  ( 5.503720292143644777, 8.508425209887878538, 1.199719254218462483 ) ) ;
#40547 = CARTESIAN_POINT ( 'NONE',  ( -10.65047922011206261, 5.918049078515057460, 5.531760622192766874 ) ) ;
#40548 = CARTESIAN_POINT ( 'NONE',  ( 3.879041347285658414, 6.579279767591636130, -1.082531754730548412 ) ) ;
#40549 = CARTESIAN_POINT ( 'NONE',  ( -4.874313559192080092, 4.961021341527962036, 0.5169845646830675268 ) ) ;
#40550 = CARTESIAN_POINT ( 'NONE',  ( 11.84668730067608244, 12.69999999999998153, 1.319999999999998286 ) ) ;
#40551 = CARTESIAN_POINT ( 'NONE',  ( -0.6823417656250039265, 12.63020833367473017, -1.181850606188755259 ) ) ;
#40553 = CARTESIAN_POINT ( 'NONE',  ( -5.610041701004606196, 9.767075427805856691, -0.7998128361456362523 ) ) ;
#40552 = CARTESIAN_POINT ( 'NONE',  ( 6.825078400183574701, 6.039200712630649726, 2.350557101739355392 ) ) ;
#40554 = CARTESIAN_POINT ( 'NONE',  ( 4.816919938037654170, 0.8852131329995099884, -1.491020713638806949 ) ) ;
#40555 = CARTESIAN_POINT ( 'NONE',  ( -4.440459003675619520, 5.139289244831666714, 1.199719254218462483 ) ) ;
#40556 = CARTESIAN_POINT ( 'NONE',  ( 1.920843890195075510, -1.466934385316904565, 1.461102248941518855 ) ) ;
#40557 = CARTESIAN_POINT ( 'NONE',  ( 3.497769638136785986, -2.085511745926827309, 0.3643098080348127765 ) ) ;
#40558 = CARTESIAN_POINT ( 'NONE',  ( 5.926885707468349196, 10.06645042535509660, 1.040834085586084257E-14 ) ) ;
#40559 = CARTESIAN_POINT ( 'NONE',  ( 1.364683531249990311, 3.634375000341416584, 1.214306433183764966E-14 ) ) ;
#40560 = CARTESIAN_POINT ( 'NONE',  ( 1.446085390411493199, -0.8901679511373729037, 1.756898273940428634 ) ) ;
#40561 = CARTESIAN_POINT ( 'NONE',  ( 6.108345433475511399, 6.019830046288782377, 0.1574382575924727079 ) ) ;
#40562 = CARTESIAN_POINT ( 'NONE',  ( -0.4638907948587486785, -7.079050064870612502, -10.61081979358357330 ) ) ;
#40563 = CARTESIAN_POINT ( 'NONE',  ( 3.820531118927258607, 2.176299813863972865, 0.7200661129266039406 ) ) ;
#40564 = CARTESIAN_POINT ( 'NONE',  ( 2.262075381241589245, 0.7800679334904643270, 1.650788133108482825 ) ) ;
#40565 = CARTESIAN_POINT ( 'NONE',  ( 5.285699784481295183, 7.260012063351913625, 1.599625672291268286 ) ) ;
#40567 = ADVANCED_FACE ( 'NONE', ( #180046 ), #24430, .F. ) ;
#40566 = CARTESIAN_POINT ( 'NONE',  ( 5.450014562569148957, 9.302174723065263606, 1.040834085586084257E-14 ) ) ;
#40568 = CARTESIAN_POINT ( 'NONE',  ( -6.808165692356648258, 11.09461040772476714, 0.7998128361456481317 ) ) ;
#40569 =( BOUNDED_CURVE ( )  B_SPLINE_CURVE ( 2, ( #89813, #154790, #36753 ),
 .UNSPECIFIED., .F., .T. ) 
 B_SPLINE_CURVE_WITH_KNOTS ( ( 3, 3 ),
 ( 0.2499999999999997502, 0.2554818834627949897 ),
 .UNSPECIFIED. ) 
 CURVE ( )  GEOMETRIC_REPRESENTATION_ITEM ( )  RATIONAL_B_SPLINE_CURVE ( ( 1.000000000000003997, 0.9118680251885524779, 0.9396870620400654683 ) ) 
 REPRESENTATION_ITEM ( '' )  );
#40570 = CARTESIAN_POINT ( 'NONE',  ( 2.584242159373177028, 1.080601423880021894, 1.698455611904861495 ) ) ;
#40571 = CARTESIAN_POINT ( 'NONE',  ( 3.063279882407277999, 1.654721480355027863, 1.053479689057647217 ) ) ;
#40572 = CARTESIAN_POINT ( 'NONE',  ( -8.941766003412679353, 10.39081407785832845, -1.199719254218446718 ) ) ;
#40573 = CARTESIAN_POINT ( 'NONE',  ( -5.388475986427523345, 8.373973519885682393, 1.199719254218452047 ) ) ;
#40574 = CARTESIAN_POINT ( 'NONE',  ( 0.07516593201273641389, 2.869485459350088696, -2.532657826882792840 ) ) ;
#40576 = CARTESIAN_POINT ( 'NONE',  ( 4.170580646280578563, -1.651567487535645640, -0.6365977468129493388 ) ) ;
#40575 = CARTESIAN_POINT ( 'NONE',  ( 5.894497796308646009, 1.709714471583067885, -1.202884697265863778 ) ) ;
#40577 = DIRECTION ( 'NONE',  ( -0.000000000000000000, -1.000000000000000000, -0.000000000000000000 ) ) ;
#40578 = CARTESIAN_POINT ( 'NONE',  ( 1.183813618819636870, -0.9825931803647185436, 1.958887836816553429 ) ) ;
#40579 = CARTESIAN_POINT ( 'NONE',  ( 5.788919933143140462, 1.322006966288125085, 1.131936178618123456 ) ) ;
#40580 = CARTESIAN_POINT ( 'NONE',  ( 6.564118927310645724, 10.80988918183778225, -0.7998128361456291469 ) ) ;
#40581 = CARTESIAN_POINT ( 'NONE',  ( -5.049006180819098688, 6.469209200322729281, -1.249999994511374668 ) ) ;
#40582 = CARTESIAN_POINT ( 'NONE',  ( 6.117888908451988073, 0.2214900195740623634, 2.288030219478351057 ) ) ;
#40584 = ADVANCED_FACE ( 'NONE', ( #144390 ), #146504, .F. ) ;
#40583 = CARTESIAN_POINT ( 'NONE',  ( 0.000000000000000000, 0.000000000000000000, 0.000000000000000000 ) ) ;
#40585 = CARTESIAN_POINT ( 'NONE',  ( 5.184772435558752335, -0.9287019638352255191, -1.463892056132688024 ) ) ;
#40586 = CARTESIAN_POINT ( 'NONE',  ( 1.770444396619451632, 1.136427050704125419, 1.891651738277564831 ) ) ;
#40587 = CARTESIAN_POINT ( 'NONE',  ( 5.635278836315742446, -0.04772081403418790974, -2.170810874590335171 ) ) ;
#40588 = DIRECTION ( 'NONE',  ( -0.9632918427306580433, 0.000000000000000000, 0.2684563758389303945 ) ) ;
#40589 = CARTESIAN_POINT ( 'NONE',  ( 1.534521455381025801, 0.6695800964386169341, 2.008721144947374526 ) ) ;
#40590 = CARTESIAN_POINT ( 'NONE',  ( 4.281250000000002665, 0.7852924748302082536, 1.895863743163987980 ) ) ;
#40591 = CARTESIAN_POINT ( 'NONE',  ( -0.5654481856765094516, 7.808910395760659817, -1.918425245283294611 ) ) ;
#40592 = CARTESIAN_POINT ( 'NONE',  ( 4.172816426537079515, -1.797186248846779133, -0.6940461778226751921 ) ) ;
#40593 = CARTESIAN_POINT ( 'NONE',  ( 0.7334294796089964041, 2.054545164755026576, 0.8448789909778311458 ) ) ;
#40594 = ORIENTED_EDGE ( 'NONE', *, *, #73487, .T. ) ;
#40595 = CARTESIAN_POINT ( 'NONE',  ( 0.7499999999999902300, 4.066666666666690411, -1.299038105676658228 ) ) ;
#40596 = CARTESIAN_POINT ( 'NONE',  ( 5.684946482831785275, 5.526859072925533134, -0.7998128361456231517 ) ) ;
#40597 = CARTESIAN_POINT ( 'NONE',  ( 7.481401836642521452, 7.622723652371411696, 1.040834085586084257E-14 ) ) ;
#40598 = CARTESIAN_POINT ( 'NONE',  ( 3.334858576441266376, 1.407893888572855801, -1.718160706149525430 ) ) ;
#40599 = CARTESIAN_POINT ( 'NONE',  ( -8.853111120043687166, 9.430977182913531820, 1.040834085586084257E-14 ) ) ;
#40600 = CARTESIAN_POINT ( 'NONE',  ( -11.55950211276791428, 9.719999999999998863, -3.221476510067114329 ) ) ;
#40601 = CARTESIAN_POINT ( 'NONE',  ( 5.829642864196157070, 8.784705193995428374, 1.082531754730558626 ) ) ;
#40602 = CARTESIAN_POINT ( 'NONE',  ( -8.256552360598034213, 11.61609960646427986, 1.082531754730549967 ) ) ;
#40603 = CARTESIAN_POINT ( 'NONE',  ( 5.207740401424913124, 9.089797878388800711, -0.7216878364870458196 ) ) ;
#40604 = CIRCLE ( 'NONE', #54372, 2.600000000000000533 ) ;
#40605 = CARTESIAN_POINT ( 'NONE',  ( 1.670546294658280084, 1.392546765991018454, 1.458555661489918442 ) ) ;
#40607 = CARTESIAN_POINT ( 'NONE',  ( 0.3212321915853528220, -1.840712657873358138, -0.9308276203483353273 ) ) ;
#40606 = CARTESIAN_POINT ( 'NONE',  ( 7.995557903757111617, 10.35123685918189729, 1.599625672291281386 ) ) ;
#40608 = CARTESIAN_POINT ( 'NONE',  ( -11.33772463945037146, 11.00911576511424528, 3.599999999999998757 ) ) ;
#40609 = CARTESIAN_POINT ( 'NONE',  ( 7.810905894804431426, 8.285347430126213553, 0.000000000000000000 ) ) ;
#40610 = CARTESIAN_POINT ( 'NONE',  ( -0.1121326479804653220, -0.4008509640632436088, -1.803546454093779561 ) ) ;
#40612 = ADVANCED_FACE ( 'NONE', ( #35908 ), #184282, .T. ) ;
#40611 = CARTESIAN_POINT ( 'NONE',  ( -2.474997580123502683, 0.9706168436483498807, 11.64394813633530390 ) ) ;
#40613 = CARTESIAN_POINT ( 'NONE',  ( -0.6823417656250003738, 2.717708333674753618, -1.181850606188749264 ) ) ;
#40614 = CARTESIAN_POINT ( 'NONE',  ( 1.018396826474694761, 1.632260513341069252, 0.6844030214382245125 ) ) ;
#40615 = CARTESIAN_POINT ( 'NONE',  ( -0.1224325501351306023, -0.4448023855274513272, -1.973852191825019364 ) ) ;
#40616 = CARTESIAN_POINT ( 'NONE',  ( 0.1867156058280826092, 1.363667594142993877, 1.237386390646778578 ) ) ;
#40617 = CARTESIAN_POINT ( 'NONE',  ( 4.458679977242249848, -2.047270833213535202, -1.031427349252316272 ) ) ;
#40618 = CARTESIAN_POINT ( 'NONE',  ( 2.255570300226293234, 0.7868700230135963203, 1.664660379391752043 ) ) ;
#40619 = EDGE_CURVE ( 'NONE', #145502, #56116, #155246, .T. ) ;
#40620 = CARTESIAN_POINT ( 'NONE',  ( 9.585778300061798873, 11.14216175728232550, -1.199719254218440723 ) ) ;
#40621 = SHAPE_REPRESENTATION_RELATIONSHIP ( 'NONE' , 'NONE' ,  #99753, #122417 ) ;
#40622 = CARTESIAN_POINT ( 'NONE',  ( 3.504746488097260748, 1.439749907568649068, -1.122338611188322455 ) ) ;
#40623 = CARTESIAN_POINT ( 'NONE',  ( 4.113907844847329187, 0.1017495355152969322, 2.013985960686740295 ) ) ;
#40624 = CARTESIAN_POINT ( 'NONE',  ( -8.479735010343349089, 11.98044238112085758, 1.199719254218453823 ) ) ;
#40626 = FACE_OUTER_BOUND ( 'NONE', #204531, .T. ) ;
#40625 = CARTESIAN_POINT ( 'NONE',  ( 3.678848304420906601, -2.179822953419420006, -0.6058417560294343529 ) ) ;
#40627 = CARTESIAN_POINT ( 'NONE',  ( 5.895568648972373538, 1.592330039046478740, 1.378332891347531231 ) ) ;
#40628 = CARTESIAN_POINT ( 'NONE',  ( -1.859593142679977218, 3.245846270153701418, -0.4000000000000284439 ) ) ;
#40629 = CARTESIAN_POINT ( 'NONE',  ( 3.051297593704501043, 1.777051743073382761, -1.062048545217339823 ) ) ;
#40630 = CARTESIAN_POINT ( 'NONE',  ( 4.542145155778077203, 5.257923088951247159, -1.199719254218452047 ) ) ;
#40631 = CARTESIAN_POINT ( 'NONE',  ( 1.360316468749939833, 0.02604166700813021276, 0.7853790794158660438 ) ) ;
#40632 = CARTESIAN_POINT ( 'NONE',  ( 6.059260758684835046, -1.791542317298041365, 1.134111293253435182 ) ) ;
#40634 = CARTESIAN_POINT ( 'NONE',  ( 0.8559318490590170914, 1.924348548886562815, -0.09362981192203097269 ) ) ;
#40633 = CARTESIAN_POINT ( 'NONE',  ( -7.980945979938748103, 12.46285407657057220, 0.000000000000000000 ) ) ;
#40635 = UNCERTAINTY_MEASURE_WITH_UNIT (LENGTH_MEASURE( 1.000000000000000082E-05 ), #90258, 'distance_accuracy_value', 'NONE');
#40636 = CARTESIAN_POINT ( 'NONE',  ( -3.467853430045390706, 7.267855778353407459, 0.7998128361456352531 ) ) ;
#40637 = CARTESIAN_POINT ( 'NONE',  ( 8.880754312151170282, 10.31963377138658089, 1.199719254218453823 ) ) ;
#40638 = CARTESIAN_POINT ( 'NONE',  ( 4.055297343818923039, 7.745280977848496562, 0.7216878364870257245 ) ) ;
#40639 = CARTESIAN_POINT ( 'NONE',  ( 4.707534831891463156, 6.823246043637223757, 1.233988984638714426 ) ) ;
#40640 = DIRECTION ( 'NONE',  ( 0.3085202182251676195, 0.000000000000000000, -0.9512177852344304574 ) ) ;
#40641 = CARTESIAN_POINT ( 'NONE',  ( -3.795392936821753604, 6.515376628678959392, -1.199719254218452047 ) ) ;
#40642 = CARTESIAN_POINT ( 'NONE',  ( 0.3521972369381949908, -1.576644756679127513, -1.565149006781616725 ) ) ;
#40643 = CARTESIAN_POINT ( 'NONE',  ( 2.415183150638998466, 1.880743233677120818, 0.9477269459148714992 ) ) ;
#40644 = CARTESIAN_POINT ( 'NONE',  ( -3.980200614063634568, 6.801261928786307642, 1.199719254218452935 ) ) ;
#40645 = CARTESIAN_POINT ( 'NONE',  ( 8.697719238366680372, 10.10609285197134533, 1.199719254218462483 ) ) ;
#40646 = CARTESIAN_POINT ( 'NONE',  ( 6.157066405694873623, 1.522017207847397469, -1.070502804743376668 ) ) ;
#40647 = CARTESIAN_POINT ( 'NONE',  ( 8.613507663383630941, 8.943513783569379427, -0.7998128361456221525 ) ) ;
#40648 = CYLINDRICAL_SURFACE ( 'NONE', #22791, 0.7500000000000011102 ) ;
#40649 = CARTESIAN_POINT ( 'NONE',  ( -7.105881907338178038, 7.462819444748888920, -0.7216878364870338292 ) ) ;
#40652 = ORIENTED_EDGE ( 'NONE', *, *, #133456, .T. ) ;
#40651 = CARTESIAN_POINT ( 'NONE',  ( -7.700668062882065179, 10.96756792579566664, -1.082531754730543971 ) ) ;
#40650 = AXIS2_PLACEMENT_3D ( 'NONE', #174703, #76106, #142210 ) ;
#40653 = CARTESIAN_POINT ( 'NONE',  ( -0.05226516427493665962, -1.936187138999283297, 0.8653993394739032397 ) ) ;
#40654 = CARTESIAN_POINT ( 'NONE',  ( -7.587723245503481095, 8.881373870289390737, 1.199719254218452047 ) ) ;
#40656 = CARTESIAN_POINT ( 'NONE',  ( 2.857805160684105950, -0.6180756922911297968, 1.862011555624979886 ) ) ;
#40655 = CARTESIAN_POINT ( 'NONE',  ( -1.225000000000008971, -0.7499999999999867883, -8.673617379884035472E-15 ) ) ;
#40657 = CARTESIAN_POINT ( 'NONE',  ( 2.342841879718413622, 0.4729757327756216601, 2.109170662781891359 ) ) ;
#40659 = CARTESIAN_POINT ( 'NONE',  ( -4.916882227542496153, 6.680427897100001289, -1.249109758411016236 ) ) ;
#40658 = CARTESIAN_POINT ( 'NONE',  ( -3.298376509874564988, 7.070132704820777825, 0.000000000000000000 ) ) ;
#40660 = CARTESIAN_POINT ( 'NONE',  ( 1.364683531249986537, 1.405208333674755838, -0.7879004041258239610 ) ) ;
#40661 = CARTESIAN_POINT ( 'NONE',  ( 4.066134141799277124, -1.624876214689898957, -0.6237973674530649104 ) ) ;
#40662 = CARTESIAN_POINT ( 'NONE',  ( 6.371969008742804697, 7.496680600697164465, -1.082531754730543083 ) ) ;
#40663 = CARTESIAN_POINT ( 'NONE',  ( -11.91002632418505058, 5.203875245307159503, 4.700031268430899800 ) ) ;
#40664 = CARTESIAN_POINT ( 'NONE',  ( 0.4269344243218140544, 2.069031678568326704, 0.6260965431626740463 ) ) ;
#40665 = CARTESIAN_POINT ( 'NONE',  ( 1.792342068719571468, -1.899328565777322231, 0.6766080823841430503 ) ) ;
#40666 = CARTESIAN_POINT ( 'NONE',  ( -0.09411116651288103929, -9.919020924439822195, -10.99959762541856811 ) ) ;
#40667 = FACE_OUTER_BOUND ( 'NONE', #158391, .T. ) ;
#40668 = CARTESIAN_POINT ( 'NONE',  ( 2.483225996990960027, 1.803144932609510143, -0.7974705804912070040 ) ) ;
#40670 = EDGE_LOOP ( 'NONE', ( #207171, #33600, #48500 ) ) ;
#40669 = CARTESIAN_POINT ( 'NONE',  ( -4.001064729808656573, 7.682009594836471500, 1.214306433183764966E-14 ) ) ;
#40671 = COLOUR_RGB ( '', 0.09019608, 0.27058824, 0.51372549) ;
#40672 = CARTESIAN_POINT ( 'NONE',  ( -6.902509602688830626, 7.225551755991315162, -0.7216878364870338292 ) ) ;
#40673 = CARTESIAN_POINT ( 'NONE',  ( 4.877901405866606588, 8.912911750144889567, 0.7998128361456341429 ) ) ;
#40674 = CARTESIAN_POINT ( 'NONE',  ( -6.469175572376043348, 7.576401584974034265, 1.199719254218452047 ) ) ;
#40675 = CARTESIAN_POINT ( 'NONE',  ( 2.490883850439883140, -1.933321517186505245, -0.5842891067564592866 ) ) ;
#40676 = CARTESIAN_POINT ( 'NONE',  ( -9.124274191872631334, 12.62844174295135069, -1.082531754730543083 ) ) ;
#40677 = CARTESIAN_POINT ( 'NONE',  ( 6.141700272255690152, -1.665644196019906875, -1.597301777034014991 ) ) ;
#40678 = CARTESIAN_POINT ( 'NONE',  ( -0.4288785890452732064, 3.049942316455313218, 0.4196807566830707548 ) ) ;
#40679 = CARTESIAN_POINT ( 'NONE',  ( 2.764445781119912127, -0.7462812867886670087, -1.814464804917370166 ) ) ;
#40680 = CARTESIAN_POINT ( 'NONE',  ( 9.257519960032755790, 9.694861462993381807, 0.7998128361456462443 ) ) ;
#40681 = CARTESIAN_POINT ( 'NONE',  ( 1.125625214514534900, 0.3961039030971892916, 1.976955501819408711 ) ) ;
#40682 = EDGE_LOOP ( 'NONE', ( #94591, #94491, #190620, #23593 ) ) ;
#40683 = CARTESIAN_POINT ( 'NONE',  ( 2.360703550434081421, -2.027734997378250359, -0.6095688489828243739 ) ) ;
#40685 = CARTESIAN_POINT ( 'NONE',  ( -5.747767057189642870, 8.793146435774861658, -1.199719254218440723 ) ) ;
#40684 = CARTESIAN_POINT ( 'NONE',  ( -10.33323920393391582, 4.021557182957058885, 5.965898435992110116 ) ) ;
#40686 = CARTESIAN_POINT ( 'NONE',  ( 2.361056629804247020, 1.805642548105116596, -0.3588866333120652174 ) ) ;
#40687 = EDGE_LOOP ( 'NONE', ( #50652, #83734, #109849, #9808, #18876 ) ) ;
#40688 = CARTESIAN_POINT ( 'NONE',  ( -9.541187415715041809, 12.15447128979948310, -1.599625672291263179 ) ) ;
#40689 = CARTESIAN_POINT ( 'NONE',  ( 9.604651411913359027, 12.70286830212710072, 7.196651313930959581 ) ) ;
#40690 = CARTESIAN_POINT ( 'NONE',  ( 4.447591161967184625, -1.937652164471121763, 0.8620916771790232414 ) ) ;
#40691 = CARTESIAN_POINT ( 'NONE',  ( 0.6558947131179297951, -1.335331635844772880, 1.267786537210900510 ) ) ;
#40692 = CARTESIAN_POINT ( 'NONE',  ( -1.500000000000011324, 5.202083334016151639, 0.8660254037844403729 ) ) ;
#40693 = CARTESIAN_POINT ( 'NONE',  ( 7.076466111328892694, 10.34329533227067799, -1.199719254218441611 ) ) ;
#40694 = CARTESIAN_POINT ( 'NONE',  ( 7.526711554241970248, 8.810193563817646734, -1.199719254218452047 ) ) ;
#40695 = CARTESIAN_POINT ( 'NONE',  ( 4.762995170230669650, -1.839058295199582638, -0.9300793793675359300 ) ) ;
#40697 = CARTESIAN_POINT ( 'NONE',  ( 1.768857366986800184, 1.761637791510446860, -0.5354853023365884201 ) ) ;
#40696 = CARTESIAN_POINT ( 'NONE',  ( -8.227100285394159940, 8.492705175914988303, 0.7998128361456602331 ) ) ;
#40698 = CARTESIAN_POINT ( 'NONE',  ( 0.6823417656249917140, 4.842708333674755394, 1.181850606188765695 ) ) ;
#40699 = LINE ( 'NONE', #73157, #177547 ) ;
#40700 = DIRECTION ( 'NONE',  ( 0.000000000000000000, 0.000000000000000000, 1.000000000000000000 ) ) ;
#40701 = CARTESIAN_POINT ( 'NONE',  ( 1.278255639411193245, 1.316999024263129092, 1.770685722221450709 ) ) ;
#40702 = CARTESIAN_POINT ( 'NONE',  ( 4.095213043127944097, 1.914038588809761299, -1.205934879490217382 ) ) ;
#40703 = CARTESIAN_POINT ( 'NONE',  ( -7.321039761699444703, 10.52466824108257804, 1.082531754730549967 ) ) ;
#40704 = CARTESIAN_POINT ( 'NONE',  ( 3.234412676589659252, 1.145595053071927438, -1.403395578055862902 ) ) ;
#40705 = CARTESIAN_POINT ( 'NONE',  ( 2.922943415214097396, -1.687269874283424453, 0.9073053738915691779 ) ) ;
#40706 = CARTESIAN_POINT ( 'NONE',  ( 4.598136200040512378, 0.8882050449813773119, -1.870312673664726644 ) ) ;
#40707 = CARTESIAN_POINT ( 'NONE',  ( 1.364683531249988535, 3.926041667008087543, 0.7879004041258500513 ) ) ;
#40708 = CARTESIAN_POINT ( 'NONE',  ( 2.676590784821473168, -1.886132711224804748, -0.5737105244360584111 ) ) ;
#40709 = CARTESIAN_POINT ( 'NONE',  ( 1.272347295514785870, -1.224129819625971782, 1.487435282370595857 ) ) ;
#40710 = CARTESIAN_POINT ( 'NONE',  ( 4.469519713540137218, 1.814478506493342191, -0.4545110902946307152 ) ) ;
#40711 = CARTESIAN_POINT ( 'NONE',  ( 1.858496626375233163, 2.301273984257983241, -0.1728945724901974068 ) ) ;
#40712 = CARTESIAN_POINT ( 'NONE',  ( 3.947575701020007877, 1.346737928234511106, 1.284688856454605732 ) ) ;
#40713 = CARTESIAN_POINT ( 'NONE',  ( -1.364683531250010295, 4.780208333674755394, 0.7879004041258379498 ) ) ;
#40714 = CARTESIAN_POINT ( 'NONE',  ( -5.382750679825375251, 6.238629533673094585, -1.199719254218446718 ) ) ;
#40715 = CARTESIAN_POINT ( 'NONE',  ( 5.438792177376376991, 9.497007973581119700, 1.040834085586084257E-14 ) ) ;
#40716 = DIRECTION ( 'NONE',  ( -1.000000000000000000, 0.000000000000000000, 0.000000000000000000 ) ) ;
#40717 = CARTESIAN_POINT ( 'NONE',  ( 0.8210893850928849824, 1.946682464879319729, 0.8042085006434143146 ) ) ;
#40718 = CARTESIAN_POINT ( 'NONE',  ( 2.995988758495615745, 6.439144618312774959, -0.7216878364870267237 ) ) ;
#40720 = CARTESIAN_POINT ( 'NONE',  ( 6.346625304528514810, 6.577020074804287297, 0.000000000000000000 ) ) ;
#40719 = CARTESIAN_POINT ( 'NONE',  ( 1.364683531249990311, 4.946875000341417916, 1.214306433183764966E-14 ) ) ;
#40721 = CARTESIAN_POINT ( 'NONE',  ( 6.919229410208834530, -0.1638780278429008419, 2.126154539342207883 ) ) ;
#40722 = CARTESIAN_POINT ( 'NONE',  ( 1.635180430577408028, 1.980530345366804834, 0.7584260845197098311 ) ) ;
#40723 =( NAMED_UNIT ( * ) PLANE_ANGLE_UNIT ( ) SI_UNIT ( $, .RADIAN. ) );
#40724 = CARTESIAN_POINT ( 'NONE',  ( 0.4045644467639066821, -2.005039209919571075, -0.2428365769681257724 ) ) ;
#40725 = CARTESIAN_POINT ( 'NONE',  ( -0.6823417656250246877, 0.3010416670080895418, 1.181850606188755259 ) ) ;
#40726 = CARTESIAN_POINT ( 'NONE',  ( -5.124618876285560454, 5.081069565195661220, 0.7216878364870317197 ) ) ;
#40727 = CARTESIAN_POINT ( 'NONE',  ( 4.364835388595708743, 7.179726155748598515, 1.199719254218462483 ) ) ;
#40728 = CARTESIAN_POINT ( 'NONE',  ( 0.8433209000573947955, -1.854398715148808385, 1.110445933987347367 ) ) ;
#40731 = CARTESIAN_POINT ( 'NONE',  ( 3.877268743828270470, 5.546566172598190292, 1.443375672974062551 ) ) ;
#40730 = CARTESIAN_POINT ( 'NONE',  ( 6.825078400183588023, 6.037369320589220045, 2.550557596425677254 ) ) ;
#40729 = CARTESIAN_POINT ( 'NONE',  ( 3.901714345682657292, 7.774026846596938434, 0.7998128361456271485 ) ) ;
#40732 = CARTESIAN_POINT ( 'NONE',  ( -3.006876207180748217, 6.730049018344652190, -0.7998128361456481317 ) ) ;
#40733 = CARTESIAN_POINT ( 'NONE',  ( 5.893767612163585135, -2.000732204962274441, 0.2516274335107801519 ) ) ;
#40734 = CARTESIAN_POINT ( 'NONE',  ( -7.646435448427427062, 10.90429654226522693, 1.082531754730549967 ) ) ;
#40735 = CARTESIAN_POINT ( 'NONE',  ( 0.3104468679729632807, 1.506874830639578056, -1.591553791636945991 ) ) ;
#40736 = CARTESIAN_POINT ( 'NONE',  ( -1.001543065824772872E-14, 4.962500000000019007, 1.732050807568877637 ) ) ;
#40738 = CARTESIAN_POINT ( 'NONE',  ( 1.364683531249996529, 10.96354166700806942, 0.7879004041258403923 ) ) ;
#40737 = CARTESIAN_POINT ( 'NONE',  ( 0.7435140528431654072, -1.938958340150579662, 1.165708873083745045 ) ) ;
#40739 = CARTESIAN_POINT ( 'NONE',  ( -9.297140650669053485, 11.86975006391249643, 1.599625672291281386 ) ) ;
#40741 = CARTESIAN_POINT ( 'NONE',  ( 0.6498251619827577485, 0.9450094616851455465, 1.666218678892321226 ) ) ;
#40740 = CARTESIAN_POINT ( 'NONE',  ( -5.924549939047510705, 6.974691686052601369, 1.082531754730549967 ) ) ;
#40742 = CARTESIAN_POINT ( 'NONE',  ( 1.364683531249986537, 1.176041667008082658, 0.7879004041258500513 ) ) ;
#40743 = DIRECTION ( 'NONE',  ( -0.000000000000000000, -1.000000000000000000, -0.000000000000000000 ) ) ;
#40744 = ADVANCED_FACE ( 'NONE', ( #168052 ), #100906, .F. ) ;
#40745 = CARTESIAN_POINT ( 'NONE',  ( -0.08896015503664694846, 7.049507384514476449, -3.948637857580539201 ) ) ;
#40746 = CARTESIAN_POINT ( 'NONE',  ( 3.246439759211931175, 0.4201230555563889579, 1.672790298054289693 ) ) ;
#40747 = CARTESIAN_POINT ( 'NONE',  ( 5.204350862799327793, 7.165104988056252289, -1.599625672291281386 ) ) ;
#40748 = CARTESIAN_POINT ( 'NONE',  ( 0.4558546072216109191, 0.6692488815305540628, 1.638537551351123112 ) ) ;
#40749 = CARTESIAN_POINT ( 'NONE',  ( 1.594390828295478402, -1.075120693119306692, 1.701777395020438899 ) ) ;
#40750 = FILL_AREA_STYLE ('',( #171799 ) ) ;
#40751 = CARTESIAN_POINT ( 'NONE',  ( 8.886479618753304166, 12.45497775759917758, -1.199719254218446718 ) ) ;
#40752 = CARTESIAN_POINT ( 'NONE',  ( 4.682781310676605635, -2.139571651222616833, -0.5399477217277389718 ) ) ;
#40753 = VECTOR ( 'NONE', #16531, 1000.000000000000000 ) ;
#40754 = VERTEX_POINT ( 'NONE', #201586 ) ;
#40755 = CARTESIAN_POINT ( 'NONE',  ( 8.310784975052673218, 10.71900177569337487, -1.443375672974063439 ) ) ;
#40756 = CARTESIAN_POINT ( 'NONE',  ( -5.915100157312088491, 10.12297696016459092, -0.7998128361456362523 ) ) ;
#40758 = CARTESIAN_POINT ( 'NONE',  ( 3.567982607561688280, -0.9913820634350966055, 1.755780237201590488 ) ) ;
#40757 = CARTESIAN_POINT ( 'NONE',  ( 4.002672028760116518, -2.097606743168555443, -0.3097674545872729501 ) ) ;
#40760 = VERTEX_POINT ( 'NONE', #181101 ) ;
#40759 = CARTESIAN_POINT ( 'NONE',  ( 3.093827002871222920, 1.152939038403834493, 1.397299590375496336 ) ) ;
#40761 = CARTESIAN_POINT ( 'NONE',  ( 6.073126464278658432, 6.050012061272033392, 0.000000000000000000 ) ) ;
#40762 = ADVANCED_FACE ( 'NONE', ( #50039 ), #65376, .T. ) ;
#40763 = ORIENTED_EDGE ( 'NONE', *, *, #195142, .F. ) ;
#40764 = CARTESIAN_POINT ( 'NONE',  ( 1.850267049257280139, 0.5840378008528935849, 1.777222254475477659 ) ) ;
#40765 = EDGE_CURVE ( 'NONE', #62251, #140937, #89492, .T. ) ;
#40766 = VECTOR ( 'NONE', #63424, 1000.000000000000000 ) ;
#40767 = CARTESIAN_POINT ( 'NONE',  ( 5.742758765878789085, 0.3605303665093100851, 1.789564367143759327 ) ) ;
#40768 = DIRECTION ( 'NONE',  ( 0.000000000000000000, -1.000000000000000000, 0.000000000000000000 ) ) ;
#40769 = AXIS2_PLACEMENT_3D ( 'NONE', #143917, #209913, #193676 ) ;
#40770 = DIRECTION ( 'NONE',  ( 5.578564026256490882E-16, 1.000000000000000000, 9.066213480720158442E-32 ) ) ;
#40771 = FACE_OUTER_BOUND ( 'NONE', #206018, .T. ) ;
#40772 = CARTESIAN_POINT ( 'NONE',  ( -0.6823417656250212460, 2.363541667008084435, 1.181850606188767472 ) ) ;
#40773 = CARTESIAN_POINT ( 'NONE',  ( 2.493461049780987260, 3.507114751586604129, -11.73081193161139169 ) ) ;
#40774 = CARTESIAN_POINT ( 'NONE',  ( 7.187230829020130329, 7.557726520044554697, 0.7216878364870267237 ) ) ;
#40775 = CARTESIAN_POINT ( 'NONE',  ( -3.187575512988701565, 6.732938841879847480, 0.000000000000000000 ) ) ;
#40776 = CARTESIAN_POINT ( 'NONE',  ( -5.798046968499580345, 6.793418213784815585, 1.199719254218452935 ) ) ;
#40777 = CARTESIAN_POINT ( 'NONE',  ( 4.553055379497691568, 0.3652949536288411791, 2.088752307168060707 ) ) ;
#40779 = CARTESIAN_POINT ( 'NONE',  ( -10.37105062950515943, 6.927298630606520291, 5.133691221222295376 ) ) ;
#40778 = CARTESIAN_POINT ( 'NONE',  ( -0.1294898018151837138, 2.036186877494918335, -2.343407025977122693 ) ) ;
#40780 = CARTESIAN_POINT ( 'NONE',  ( 5.184826486558015368, -0.2386506126292788632, -1.956774853079599197 ) ) ;
#40781 = CARTESIAN_POINT ( 'NONE',  ( 1.364683531249988757, 0.8843750003414210248, 0.000000000000000000 ) ) ;
#40782 = CARTESIAN_POINT ( 'NONE',  ( 0.0002439367322616680669, -0.9454701154091667004, 1.777349279628215095 ) ) ;
#40783 = ORIENTED_EDGE ( 'NONE', *, *, #202457, .T. ) ;
#40784 = CARTESIAN_POINT ( 'NONE',  ( 0.4568545718052554050, -1.995212666551810399, -0.7087754862673681933 ) ) ;
#40785 = CARTESIAN_POINT ( 'NONE',  ( 0.000000000000000000, 9.799999999999998934, 0.000000000000000000 ) ) ;
#40786 = CARTESIAN_POINT ( 'NONE',  ( 1.205626512970816355, -1.630946839658468983, -1.275175305487465049 ) ) ;
#40787 = CARTESIAN_POINT ( 'NONE',  ( 6.692885107001518286, 7.837396042037102717, -1.199719254218452047 ) ) ;
#40788 = VERTEX_POINT ( 'NONE', #67313 ) ;
#40789 = CARTESIAN_POINT ( 'NONE',  ( 6.554440917563797875, 6.611545590104705994, -0.7998128361456481317 ) ) ;
#40790 = CARTESIAN_POINT ( 'NONE',  ( 4.213551878797002992, 8.137837301896977849, 0.000000000000000000 ) ) ;
#40792 = CARTESIAN_POINT ( 'NONE',  ( 3.683011284406639607, 7.448596931783069586, 0.7998128361456321445 ) ) ;
#40791 = CARTESIAN_POINT ( 'NONE',  ( 3.521503319566265944, -1.245636697800769355, -1.678868242315070258 ) ) ;
#40793 = CARTESIAN_POINT ( 'NONE',  ( 7.849244587668864348, 8.122149871893999062, 0.7998128361456291469 ) ) ;
#40796 = ORIENTED_EDGE ( 'NONE', *, *, #92773, .T. ) ;
#40795 = CARTESIAN_POINT ( 'NONE',  ( 1.224954274949443978, 1.597400116765529843, 0.8541874478597778486 ) ) ;
#40794 = CARTESIAN_POINT ( 'NONE',  ( 2.414841169274529520, 1.629557050654990791, 0.8231356554938076275 ) ) ;
#40797 = CARTESIAN_POINT ( 'NONE',  ( 5.514374426699260923, -0.9893691592960799364, -1.972764877262770833 ) ) ;
#40798 = CARTESIAN_POINT ( 'NONE',  ( -15.75000000000000000, 12.30000000000000071, -1.800000000000001155 ) ) ;
#40799 = CARTESIAN_POINT ( 'NONE',  ( 4.542132036680512464, 0.9468659437555368985, -1.993456357439137960 ) ) ;
#40800 = CARTESIAN_POINT ( 'NONE',  ( 6.123478934866503742, 10.29580919065294431, 0.7998128361456462443 ) ) ;
#40801 = CARTESIAN_POINT ( 'NONE',  ( 2.859904825981678833, 0.6862549603197342085, -1.785085608301796523 ) ) ;
#40802 =( GEOMETRIC_REPRESENTATION_CONTEXT ( 3 ) GLOBAL_UNCERTAINTY_ASSIGNED_CONTEXT ( ( #81398 ) ) GLOBAL_UNIT_ASSIGNED_CONTEXT ( ( #207681, #57177, #88623 ) ) REPRESENTATION_CONTEXT ( 'NONE', 'WORKASPACE' ) );
#40803 = CARTESIAN_POINT ( 'NONE',  ( 7.736899214892750010, 12.17813285068358020, 1.040834085586084257E-14 ) ) ;
#40804 = CARTESIAN_POINT ( 'NONE',  ( 5.195788487752976081, -1.461605715988937515, -1.466586839339318660 ) ) ;
#40805 = DIRECTION ( 'NONE',  ( 0.01240427322301438165, -0.9999230640433337536, 0.000000000000000000 ) ) ;
#40806 = CARTESIAN_POINT ( 'NONE',  ( 5.882419586753742102, -0.3201050945752722532, -2.167950725039065052 ) ) ;
#40807 = VERTEX_POINT ( 'NONE', #65195 ) ;
#40808 = ORIENTED_EDGE ( 'NONE', *, *, #6746, .F. ) ;
#40809 = TOROIDAL_SURFACE ( 'NONE', #193078, 4.899999999999999467, 0.4000000000000000222 ) ;
#40810 = CARTESIAN_POINT ( 'NONE',  ( 9.578206935422374002, -9.900000000000074962, -0.1671882239537531845 ) ) ;
#40811 = CARTESIAN_POINT ( 'NONE',  ( 5.571474780572990504, 5.464751763615448787, 0.7998128361456352531 ) ) ;
#40812 = CARTESIAN_POINT ( 'NONE',  ( 3.285556943750000070, -1.071874999522042016, 0.000000000000000000 ) ) ;
#40813 = SURFACE_STYLE_FILL_AREA ( #190229 ) ;
#40814 = CARTESIAN_POINT ( 'NONE',  ( -8.676855123066030018, 9.225345186439589895, -0.7216878364870267237 ) ) ;
#40815 = CARTESIAN_POINT ( 'NONE',  ( 5.273195401072370281, 5.116759154198018855, -0.7998128361456481317 ) ) ;
#40816 = CARTESIAN_POINT ( 'NONE',  ( 5.770397209236588942, -0.9257025293247715947, -1.851810055641222252 ) ) ;
#40817 = CARTESIAN_POINT ( 'NONE',  ( 4.389231790275191614, 1.720148140252445668, -0.8676111672119514173 ) ) ;
#40818 = CARTESIAN_POINT ( 'NONE',  ( 0.2808753465170962249, 1.674874268995883320, -1.122520385770640061 ) ) ;
#40819 = CARTESIAN_POINT ( 'NONE',  ( -10.13488352141530768, 11.78278451552804817, 1.199719254218462483 ) ) ;
#40820 = CARTESIAN_POINT ( 'NONE',  ( 7.679767667498067496, 7.924426798361372093, 0.000000000000000000 ) ) ;
#40821 = CARTESIAN_POINT ( 'NONE',  ( -4.191371940688026321, 3.976852638198642875, -0.5757558571073126963 ) ) ;
#40822 = CARTESIAN_POINT ( 'NONE',  ( 0.09403522832084068583, -2.191061582759439297, -0.04926842934906834615 ) ) ;
#40823 = CARTESIAN_POINT ( 'NONE',  ( 5.092344371507952161, -1.812320225013038133, -0.2200062734805732223 ) ) ;
#40824 = CARTESIAN_POINT ( 'NONE',  ( 5.478903473698239601, 7.485416367438324059, -1.443375672974078761 ) ) ;
#40826 = EDGE_CURVE ( 'NONE', #107467, #1301, #96523, .T. ) ;
#40825 = CARTESIAN_POINT ( 'NONE',  ( 8.062294901620731480, 12.55776115186623620, 1.040834085586084257E-14 ) ) ;
#40827 = CARTESIAN_POINT ( 'NONE',  ( -5.173318132066234476, 8.193232366456022930, -1.199719254218453823 ) ) ;
#40828 = CARTESIAN_POINT ( 'NONE',  ( 5.854423403002611437, 5.724582146458163656, 1.040834085586084257E-14 ) ) ;
#40829 = CARTESIAN_POINT ( 'NONE',  ( 5.578253857379852576, 5.472660686556754861, -0.7998128361456481317 ) ) ;
#40830 = VERTEX_POINT ( 'NONE', #33778 ) ;
#40832 = CARTESIAN_POINT ( 'NONE',  ( 6.047140908842845164, 0.2017661761196144488, 2.003097277516131758 ) ) ;
#40831 = CARTESIAN_POINT ( 'NONE',  ( 2.313779677144182312, 1.201330555204615180, -1.395457044143719072 ) ) ;
#40833 = CARTESIAN_POINT ( 'NONE',  ( 1.933413756328787869, 1.181669745456917830, 1.971221161662185528 ) ) ;
#40834 = CARTESIAN_POINT ( 'NONE',  ( 0.3560157238547481118, -1.860367465765656814, -0.05377290132800408712 ) ) ;
#40835 = CARTESIAN_POINT ( 'NONE',  ( -6.552668314106420588, 6.539201209412602189, -0.7998128361456291469 ) ) ;
#40836 = CARTESIAN_POINT ( 'NONE',  ( -8.081892667527538876, -5.166862915010145052, 7.462104991928527831 ) ) ;
#40837 = CARTESIAN_POINT ( 'NONE',  ( -4.634189577772691138, 4.300976017023221409, 1.214306433183764966E-14 ) ) ;
#40838 = LINE ( 'NONE', #75454, #2067 ) ;
#40839 = CARTESIAN_POINT ( 'NONE',  ( -5.307090785106547415, 5.156303768904543894, -0.7998128361456362523 ) ) ;
#40841 = CARTESIAN_POINT ( 'NONE',  ( 0.6373110600932235803, -1.319858442276698129, -1.325903642019378381 ) ) ;
#40840 = CARTESIAN_POINT ( 'NONE',  ( 2.771125873548622831, 1.984386128312282116, -0.6585125772022564217 ) ) ;
#40842 = CARTESIAN_POINT ( 'NONE',  ( 1.669295836627190610, -0.7230268306642473330, -1.882186858670406693 ) ) ;
#40843 = CARTESIAN_POINT ( 'NONE',  ( 8.487040972474689582, 9.964264558384387627, -1.082531754730543083 ) ) ;
#40844 = ORIENTED_EDGE ( 'NONE', *, *, #72931, .F. ) ;
#40845 = CARTESIAN_POINT ( 'NONE',  ( -0.6823417656250212460, 4.113541667008085767, 1.181850606188767472 ) ) ;
#40846 = CARTESIAN_POINT ( 'NONE',  ( 2.208218529973245303, 1.555207145793806811, 0.7814158636046761863 ) ) ;
#40847 = CIRCLE ( 'NONE', #20081, 1.500000000000000222 ) ;
#40848 = CARTESIAN_POINT ( 'NONE',  ( 5.931855901178834323, 6.879252291918818152, 1.199719254218462483 ) ) ;
#40850 = CARTESIAN_POINT ( 'NONE',  ( -0.1054627972275563597, 3.385846599571565640, -2.076146368081344118 ) ) ;
#40849 = DIRECTION ( 'NONE',  ( 1.000000000000000000, -0.000000000000000000, -0.000000000000000000 ) ) ;
#40851 = CARTESIAN_POINT ( 'NONE',  ( 3.369487540355073030, 1.682505700701863338, -0.3791672619692722512 ) ) ;
#40853 = EDGE_CURVE ( 'NONE', #112831, #48301, #66247, .T. ) ;
#40852 = CARTESIAN_POINT ( 'NONE',  ( 2.402122600552298870, -0.8417629408748151798, -2.023652355447076001 ) ) ;
#40854 = CARTESIAN_POINT ( 'NONE',  ( 5.391335350415090488, 1.947751002805158560, -1.037606470750504828 ) ) ;
#40855 = CARTESIAN_POINT ( 'NONE',  ( -11.27976636440881641, 5.060096319113082330, -5.788224378391188196 ) ) ;
#40856 = CARTESIAN_POINT ( 'NONE',  ( 2.061612764771907802, 1.803244147071264125, 1.208790786097496905 ) ) ;
#40857 = CARTESIAN_POINT ( 'NONE',  ( 0.9964003531478006215, -0.4411313887022934033, -1.771462291394958255 ) ) ;
#40858 = SURFACE_STYLE_USAGE ( .BOTH. , #90675 ) ;
#40859 = CARTESIAN_POINT ( 'NONE',  ( 4.680926624126137803, 1.758507693093620539, -1.179036559061322542 ) ) ;
#40860 = CARTESIAN_POINT ( 'NONE',  ( 6.539320575229274901, 7.629137130509072051, 2.496737603865983424 ) ) ;
#40861 = EDGE_LOOP ( 'NONE', ( #136928, #49291 ) ) ;
#40862 = VECTOR ( 'NONE', #132939, 1000.000000000000000 ) ;
#40864 = CARTESIAN_POINT ( 'NONE',  ( 0.6823417656249899377, 1.155208333674752286, 1.181850606188755259 ) ) ;
#40863 = CARTESIAN_POINT ( 'NONE',  ( 4.300488954165425426, 1.772315894223834176, -1.453880271152303116 ) ) ;
#40865 = CARTESIAN_POINT ( 'NONE',  ( -2.609770642201835855, 0.3830433331901538785, 0.000000000000000000 ) ) ;
#40866 = CARTESIAN_POINT ( 'NONE',  ( 3.734381245560244089, 6.444196322207211836, 1.199719254218462483 ) ) ;
#40867 = CARTESIAN_POINT ( 'NONE',  ( -0.09290056220616692284, -0.4702265987995763452, -2.075310686570643437 ) ) ;
#40868 = CARTESIAN_POINT ( 'NONE',  ( -5.666945020832185875, 7.634521829102760115, 1.443375672974064550 ) ) ;
#40869 = CARTESIAN_POINT ( 'NONE',  ( 4.853455804012228647, 4.764712647543454693, 0.7216878364870317197 ) ) ;
#40870 = CARTESIAN_POINT ( 'NONE',  ( -5.490689023410187275, 8.389259046411751797, 1.082531754730548412 ) ) ;
#40871 = CARTESIAN_POINT ( 'NONE',  ( 4.936577329151614180, 4.931964103531220722, -0.7216878364870458196 ) ) ;
#40872 = ORIENTED_EDGE ( 'NONE', *, *, #164153, .T. ) ;
#40873 = CARTESIAN_POINT ( 'NONE',  ( 4.764296165657141202, 1.880435471729305030, -0.7283773170061805802 ) ) ;
#40875 = CARTESIAN_POINT ( 'NONE',  ( 3.573143115351416377, 1.862571710426489169, 0.8863520062180642034 ) ) ;
#40874 = CARTESIAN_POINT ( 'NONE',  ( 5.497994985541524215, 6.373081223675282736, -1.199719254218445830 ) ) ;
#40877 = CARTESIAN_POINT ( 'NONE',  ( -0.1411974294642202310, 0.2398548052158452348, -1.934266582396115819 ) ) ;
#40876 = LINE ( 'NONE', #41947, #161264 ) ;
#40878 = CARTESIAN_POINT ( 'NONE',  ( 8.025500584646550806, 8.327781868367935658, 0.000000000000000000 ) ) ;
#40880 = EDGE_CURVE ( 'NONE', #195414, #126635, #165919, .T. ) ;
#40879 = CARTESIAN_POINT ( 'NONE',  ( -3.285556943749998737, -2.880208332855377584, 1.896917185911908499 ) ) ;
#40881 = CARTESIAN_POINT ( 'NONE',  ( 5.666036703420031628, -1.392593631063457682, 1.692088878451535106 ) ) ;
#40882 = CARTESIAN_POINT ( 'NONE',  ( 3.481092415823695774, -2.014232707597499505, -0.09613569647320965861 ) ) ;
#40883 = CARTESIAN_POINT ( 'NONE',  ( 3.263068207883256466, 1.795673413606920565, -0.4063787724192802209 ) ) ;
#40884 = ADVANCED_FACE ( 'NONE', ( #103056 ), #133457, .T. ) ;
#40885 = CARTESIAN_POINT ( 'NONE',  ( 7.332262146892202459, 7.448727347662698506, -0.7998128361456281477 ) ) ;
#40886 = CARTESIAN_POINT ( 'NONE',  ( 0.1469036390603413456, -1.327996847208750442, -1.100432056080926202 ) ) ;
#40887 = CARTESIAN_POINT ( 'NONE',  ( -7.739006755302186846, 7.923262724141010516, 0.7998128361456462443 ) ) ;
#40888 = CARTESIAN_POINT ( 'NONE',  ( 6.807534431281101028, -0.5077146954460194372, 2.213219090469565664 ) ) ;
#40889 = CARTESIAN_POINT ( 'NONE',  ( 1.752698641044206251, 0.6620485714215967876, 1.999371444633216033 ) ) ;
#40890 = CARTESIAN_POINT ( 'NONE',  ( -7.123883369337781879, 7.275895117174344229, 0.7998128361456341429 ) ) ;
#40891 = APPLICATION_CONTEXT ( 'automotive_design' ) ;
#40892 = CARTESIAN_POINT ( 'NONE',  ( 5.913327553854682783, 10.05063257947248800, -0.7998128361456291469 ) ) ;
#40893 = CARTESIAN_POINT ( 'NONE',  ( 6.170369307550816806, 9.252495721234380355, 1.082531754730549967 ) ) ;
#40894 = CARTESIAN_POINT ( 'NONE',  ( -5.065942953000576843, 9.062017211809330064, -0.7998128361456231517 ) ) ;
#40895 = CARTESIAN_POINT ( 'NONE',  ( 6.765155463094746580, 9.876136559377135526, 1.082531754730558626 ) ) ;
#40896 = CARTESIAN_POINT ( 'NONE',  ( 4.104435073692848768, 7.689436668370499106, -0.6928796192886893524 ) ) ;
#40897 = CARTESIAN_POINT ( 'NONE',  ( -5.762378981008047241, 6.681529218386182301, 1.199719254218450271 ) ) ;
#40898 = CARTESIAN_POINT ( 'NONE',  ( 4.342156631555553759, -1.367984123109561301, -1.750111109629876260 ) ) ;
#40899 = CARTESIAN_POINT ( 'NONE',  ( 2.273600812266802773, 1.349468827467028120, 1.726581335083368307 ) ) ;
#40900 = CARTESIAN_POINT ( 'NONE',  ( 0.7334016978863610037, 0.1661181961954381059, 2.200687262777756725 ) ) ;
#40901 = CARTESIAN_POINT ( 'NONE',  ( -3.962726036944197894, 7.845207153068690431, -0.7998128361456481317 ) ) ;
#40902 = CARTESIAN_POINT ( 'NONE',  ( 4.281663391851794565, -1.878042059144067633, 0.5673916069991248312 ) ) ;
#40903 = CARTESIAN_POINT ( 'NONE',  ( 9.378489572351044856, 11.96465713920816043, -1.599625672291262513 ) ) ;
#40904 = CARTESIAN_POINT ( 'NONE',  ( 7.065207446497155708, 9.336104335703744539, 0.000000000000000000 ) ) ;
#40905 = CARTESIAN_POINT ( 'NONE',  ( -1.364683531250014514, 0.2802083336747505649, 0.7879004041258379498 ) ) ;
#40906 = CARTESIAN_POINT ( 'NONE',  ( 6.610000000000021636, 3.695490760540712127, 2.514297579034238783 ) ) ;
#40908 = VERTEX_POINT ( 'NONE', #199461 ) ;
#40907 = CARTESIAN_POINT ( 'NONE',  ( -7.239690840017442675, 7.548653522882887934, 0.7216878364870317197 ) ) ;
#40909 = CARTESIAN_POINT ( 'NONE',  ( 3.515986968957810266, -0.6120941298391362473, 2.030368431519948391 ) ) ;
#40910 = CARTESIAN_POINT ( 'NONE',  ( -4.634908411025374875, 6.500755460986618495, 1.599625672291263179 ) ) ;
#40911 = CARTESIAN_POINT ( 'NONE',  ( 5.717692609583751029, -2.109997883074541392, 0.4692839721026839661 ) ) ;
#40912 = CARTESIAN_POINT ( 'NONE',  ( 4.458453498679889826, -1.646799808365447371, -0.8236825204945983359 ) ) ;
#40913 = CARTESIAN_POINT ( 'NONE',  ( -5.889415777131212337, 6.013640170854067435, 0.2549476635474844932 ) ) ;
#40914 = CARTESIAN_POINT ( 'NONE',  ( -1.402160292154681736E-14, 1.509375000341420359, -1.575800808251659024 ) ) ;
#40915 = CARTESIAN_POINT ( 'NONE',  ( 0.02830193721903468546, -1.592744100209501967, 0.7021035195741828216 ) ) ;
#40916 = CARTESIAN_POINT ( 'NONE',  ( 6.727182134110201162, 1.271184308336456015, 2.025152302351560518 ) ) ;
#40917 = CARTESIAN_POINT ( 'NONE',  ( 3.063779527008311021, 5.557864633942907417, 1.082531754730546636 ) ) ;
#40918 = CARTESIAN_POINT ( 'NONE',  ( 11.75119899582183614, 6.933193708961042034, -2.442676079799758426 ) ) ;
#40919 = CARTESIAN_POINT ( 'NONE',  ( 4.047864428982482110, 0.7307185629543844207, -2.034579650689218866 ) ) ;
#40920 = CARTESIAN_POINT ( 'NONE',  ( -4.761938266897808525, 6.578680616179308771, 1.599625672291267398 ) ) ;
#40921 = EDGE_CURVE ( 'NONE', #98224, #54631, #50717, .T. ) ;
#40922 = CARTESIAN_POINT ( 'NONE',  ( 6.028672669474048007, 1.986741788447304646, -0.3418859329693338944 ) ) ;
#40923 = CARTESIAN_POINT ( 'NONE',  ( -7.741342523278709642, 10.05465224862374285, 1.443375672974090751 ) ) ;
#40925 = COLOUR_RGB ( '', 0.40784314, 0.44705882, 0.49803922) ;
#40924 = CIRCLE ( 'NONE', #193034, 11.92000000000000171 ) ;
#40926 = CARTESIAN_POINT ( 'NONE',  ( 3.696290335837215668, -2.159122111672501454, -0.1082323872379290647 ) ) ;
#40927 = CARTESIAN_POINT ( 'NONE',  ( 3.708241208800214572, -0.7959428688352770953, -1.803694655455597262 ) ) ;
#40928 = PLANE ( 'NONE',  #37362 ) ;
#40929 = CARTESIAN_POINT ( 'NONE',  ( 0.6050338814152752542, -0.7811975584859867094, -2.171474816401474328 ) ) ;
#40930 = CARTESIAN_POINT ( 'NONE',  ( 3.180987545930415106, -0.1479678519747235910, -2.055505606019301990 ) ) ;
#40931 = CARTESIAN_POINT ( 'NONE',  ( 5.495633776345048460, -1.942234966517431660, 0.004081557570839721392 ) ) ;
#40932 = CARTESIAN_POINT ( 'NONE',  ( -8.148087131688692253, 9.568818410800712826, -1.082531754730543083 ) ) ;
#40933 = CARTESIAN_POINT ( 'NONE',  ( -7.130662446144611977, 7.283804040115648526, 0.000000000000000000 ) ) ;
#40935 = VERTEX_POINT ( 'NONE', #151814 ) ;
#40934 = CARTESIAN_POINT ( 'NONE',  ( -4.248501033035892327, 6.049946853332221153, -1.599625672291271394 ) ) ;
#40936 = CARTESIAN_POINT ( 'NONE',  ( -6.683806541412762314, 9.781229484081471526, -1.082531754730537976 ) ) ;
#40937 = CARTESIAN_POINT ( 'NONE',  ( 2.678998284833411070, -2.111460168698295004, -0.6414983429729387288 ) ) ;
#40938 = CARTESIAN_POINT ( 'NONE',  ( -1.642778471875000035, -4.105208332855374564, -2.845375778867859751 ) ) ;
#40939 = ORIENTED_EDGE ( 'NONE', *, *, #77201, .F. ) ;
#40940 = CARTESIAN_POINT ( 'NONE',  ( 0.6900174830311635032, 0.9632304765912635958, -1.592144255797292463 ) ) ;
#40941 = CARTESIAN_POINT ( 'NONE',  ( -0.1290005225502918740, 6.946858002156244716, -2.769053915224591211 ) ) ;
#40942 = CARTESIAN_POINT ( 'NONE',  ( -1.001543065824772872E-14, 4.993750000682814161, 1.732050807568877637 ) ) ;
#40943 = CARTESIAN_POINT ( 'NONE',  ( 4.800107077129743161, 6.969409711611327829, -1.408023891483715317 ) ) ;
#40945 = CARTESIAN_POINT ( 'NONE',  ( -11.01135777277262129, 12.69999999999999929, -1.400000000000001910 ) ) ;
#40944 = CARTESIAN_POINT ( 'NONE',  ( -3.563261906135796409, 6.332667919118538435, 2.420000000000010587 ) ) ;
#40946 = CARTESIAN_POINT ( 'NONE',  ( 5.279192629422701621, 1.239228542960477242, 1.361826556748657602 ) ) ;
#40947 = ORIENTED_EDGE ( 'NONE', *, *, #22937, .F. ) ;
#40948 = CARTESIAN_POINT ( 'NONE',  ( 2.272404554480491168, -1.268947053487592846, 1.623793324639089874 ) ) ;
#40949 = CARTESIAN_POINT ( 'NONE',  ( -3.355169270512988773E-14, 0.9531250003414385441, 1.570758158831740303 ) ) ;
#40950 = CARTESIAN_POINT ( 'NONE',  ( -7.881367368245678406, 8.089350105908421185, 0.7998128361456602331 ) ) ;
#40951 = LINE ( 'NONE', #4132, #12778 ) ;
#40952 = EDGE_CURVE ( 'NONE', #93781, #164855, #200207, .T. ) ;
#40953 = CARTESIAN_POINT ( 'NONE',  ( 5.657830175604453338, 5.495223381160312393, 0.7998128361456341429 ) ) ;
#40954 = CARTESIAN_POINT ( 'NONE',  ( 1.235309500465184396, -1.863545150897191416, 0.8803144705526543268 ) ) ;
#40956 = CARTESIAN_POINT ( 'NONE',  ( 4.581507094455529838, -0.8636776874328588871, 1.626104626046148249 ) ) ;
#40955 = DIRECTION ( 'NONE',  ( 0.000000000000000000, 0.000000000000000000, 1.000000000000000000 ) ) ;
#40957 = CARTESIAN_POINT ( 'NONE',  ( 6.551614543901692400, 8.666636272683888365, 1.599625672291281386 ) ) ;
#40958 = CARTESIAN_POINT ( 'NONE',  ( -4.444040490229335560, 8.406740681901359480, 0.7998128361456352531 ) ) ;
#40960 = ORIENTED_EDGE ( 'NONE', *, *, #68201, .F. ) ;
#40959 = CARTESIAN_POINT ( 'NONE',  ( -0.2409995289980003397, 0.7158067089181943121, -2.082568332340509087 ) ) ;
#40961 = EDGE_CURVE ( 'NONE', #92178, #156117, #22300, .T. ) ;
#40962 = CARTESIAN_POINT ( 'NONE',  ( 3.967548030458594166, 0.2710504330169676845, -2.190103208553782821 ) ) ;
#40963 = CARTESIAN_POINT ( 'NONE',  ( 0.2105424042340813540, -0.9235240298187572527, -1.952328634516012684 ) ) ;
#40964 = CARTESIAN_POINT ( 'NONE',  ( 3.714077560468319827, 1.074663192196689376, -1.706111893292367343 ) ) ;
#40965 = CARTESIAN_POINT ( 'NONE',  ( -4.446711195602239819, 8.131654128270509929, -0.7216878364870267237 ) ) ;
#40966 = CARTESIAN_POINT ( 'NONE',  ( -0.07025823700084612988, -1.875094440630159065, 0.3749275819610526916 ) ) ;
#40967 = CARTESIAN_POINT ( 'NONE',  ( 0.4445464637146989695, -1.457232572767804379, 1.394089106691732693 ) ) ;
#40968 = CARTESIAN_POINT ( 'NONE',  ( 5.831415467209187575, 9.817418788470464008, 0.000000000000000000 ) ) ;
#40969 = CARTESIAN_POINT ( 'NONE',  ( 0.07536363704233049743, 2.002983476668462881, -2.558365315478607904 ) ) ;
#40970 = CARTESIAN_POINT ( 'NONE',  ( 3.834746474454188013E-15, 12.09375000068279604, 1.500000000000001554 ) ) ;
#40971 = CARTESIAN_POINT ( 'NONE',  ( 1.734723475976807094E-15, 15.00041888085534758, 11.91973154060107376 ) ) ;
#40972 = CARTESIAN_POINT ( 'NONE',  ( 0.3033014811697418711, -0.5033704626738467747, 1.801585485020948951 ) ) ;
#40973 = CARTESIAN_POINT ( 'NONE',  ( 2.624232735793774030, 2.001858099149746550, 0.2420302859193757539 ) ) ;
#40975 = CARTESIAN_POINT ( 'NONE',  ( -4.828904602364790577, 7.233969404134618308, 1.215374634475984594 ) ) ;
#40974 = CARTESIAN_POINT ( 'NONE',  ( 0.6823417656249899377, 0.8427083336747520637, 1.181850606188755259 ) ) ;
#40977 = CARTESIAN_POINT ( 'NONE',  ( 3.545630178961965751, -1.594748897588176950, -1.375714639268589279 ) ) ;
#40976 = CARTESIAN_POINT ( 'NONE',  ( -7.181014916732457287, 11.52960116949655678, -0.7998128361456291469 ) ) ;
#40978 = CARTESIAN_POINT ( 'NONE',  ( 8.294891053462476904, 8.571794405328034827, 1.040834085586084257E-14 ) ) ;
#40980 = CARTESIAN_POINT ( 'NONE',  ( -7.153898609505128015, 11.49796547773133604, 0.7998128361456481317 ) ) ;
#40979 = CARTESIAN_POINT ( 'NONE',  ( 5.408776937209000657, 5.274937613024121674, 0.7998128361456352531 ) ) ;
#40981 = DIRECTION ( 'NONE',  ( 0.4999999999999998890, 0.000000000000000000, 0.8660254037844385966 ) ) ;
#40982 = CARTESIAN_POINT ( 'NONE',  ( 4.658466178349073061, 2.014666459302273616, 0.1442823096002471550 ) ) ;
#40983 = CARTESIAN_POINT ( 'NONE',  ( 1.364683531249988535, 5.155208333674749177, -0.7879004041258300672 ) ) ;
#40984 = CARTESIAN_POINT ( 'NONE',  ( 9.924205255523292024, 10.68058700763975466, -0.7216878364870257245 ) ) ;
#40985 = CARTESIAN_POINT ( 'NONE',  ( 4.270900206319126369, -2.015198044118733822, -0.7823990653590962019 ) ) ;
#40986 = CARTESIAN_POINT ( 'NONE',  ( 5.688527969385528849, 8.794310509995222347, -1.199719254218452047 ) ) ;
#40987 = CARTESIAN_POINT ( 'NONE',  ( -0.6823417656250246877, -0.6364583329919113464, 1.181850606188755259 ) ) ;
#40989 = SURFACE_SIDE_STYLE ('',( #189349 ) ) ;
#40988 = CARTESIAN_POINT ( 'NONE',  ( 6.313256805818848960, 7.394496357324014113, 1.199719254218452047 ) ) ;
#40990 = CARTESIAN_POINT ( 'NONE',  ( 7.687109908824030668, 10.95175007939464606, -1.082531754730543083 ) ) ;
#40992 = CARTESIAN_POINT ( 'NONE',  ( 4.951116456854005143, 6.538279688806404089, 2.442614223628301495 ) ) ;
#40991 = CARTESIAN_POINT ( 'NONE',  ( 2.506498380571024143, 2.170641363890627229, 0.05523593993728668355 ) ) ;
#40994 = CARTESIAN_POINT ( 'NONE',  ( 1.153568636672014369, 0.7464410156945017194, 1.683350060182234209 ) ) ;
#40993 = CARTESIAN_POINT ( 'NONE',  ( -6.073689629242165822, 7.148687991279732756, -1.082531754730544860 ) ) ;
#40995 = CARTESIAN_POINT ( 'NONE',  ( 1.364683531249988757, 2.384375000341422357, 1.214306433183764966E-14 ) ) ;
#40996 = CARTESIAN_POINT ( 'NONE',  ( 3.614928802375876771, -0.1595779646587774658, 2.185787688459623901 ) ) ;
#40997 = CARTESIAN_POINT ( 'NONE',  ( -0.1747071867222168284, -7.850481869465710361, 10.96497182194659104 ) ) ;
#40998 = CARTESIAN_POINT ( 'NONE',  ( 3.555803421180541157, 0.5519491744547943002, -2.194038648399123215 ) ) ;
#40999 = CARTESIAN_POINT ( 'NONE',  ( -7.705111371268023923, 7.883718109434487253, 1.040834085586084257E-14 ) ) ;
#41001 = AXIS2_PLACEMENT_3D ( 'NONE', #16960, #149115, #696 ) ;
#41000 = CARTESIAN_POINT ( 'NONE',  ( 1.364683531249988535, 4.717708333674756283, -0.7879004041258300672 ) ) ;
#41002 = CARTESIAN_POINT ( 'NONE',  ( 6.307155384238837037, 6.868572428096745064, 0.7081091520576547893 ) ) ;
#41003 = CARTESIAN_POINT ( 'NONE',  ( 0.7500000000000006661, 14.33333333333333748, 1.299038105676657340 ) ) ;
#41004 = CARTESIAN_POINT ( 'NONE',  ( 6.400857919427532572, 6.640291458853147866, -0.7216878364870458196 ) ) ;
#41005 =( BOUNDED_CURVE ( )  B_SPLINE_CURVE ( 2, ( #60940, #181083, #112963, #178975, #14295, #180031, #80390, #77179, #64147 ),
 .UNSPECIFIED., .F., .T. ) 
 B_SPLINE_CURVE_WITH_KNOTS ( ( 3, 2, 2, 2, 3 ),
 ( 0.3958333333333333703, 0.4027777777777777901, 0.4166666666666666852, 0.4305555555555555802, 0.4375000000000000000 ),
 .UNSPECIFIED. ) 
 CURVE ( )  GEOMETRIC_REPRESENTATION_ITEM ( )  RATIONAL_B_SPLINE_CURVE ( ( 0.9330127018922194093, 0.9330127018922196314, 1.000000000000000000, 0.8660254037844387076, 1.000000000000000000, 0.8660254037844387076, 1.000000000000000000, 0.9330127018922194093, 0.9330127018922194093 ) ) 
 REPRESENTATION_ITEM ( '' )  );
#41006 = CARTESIAN_POINT ( 'NONE',  ( 5.905463120178883862, -0.4284811148945049109, 1.716917210449308673 ) ) ;
#41007 = CARTESIAN_POINT ( 'NONE',  ( 7.086107841436786181, 11.41887624831828418, 1.040834085586084257E-14 ) ) ;
#41008 = CARTESIAN_POINT ( 'NONE',  ( 0.9562493570349944738, 2.103547740682055966, -0.1031677049159150372 ) ) ;
#41010 = CARTESIAN_POINT ( 'NONE',  ( -1.402160292154681736E-14, 1.087500000000024336, -1.732050807568863648 ) ) ;
#41009 = CARTESIAN_POINT ( 'NONE',  ( -0.6823417656250003738, 10.15104166700806587, 1.181850606188754593 ) ) ;
#41011 = CARTESIAN_POINT ( 'NONE',  ( 1.346085547170269070, -0.8884179423524626307, 1.757888261374307870 ) ) ;
#41012 = CIRCLE ( 'NONE', #186311, 11.09999999999999964 ) ;
#41013 = CARTESIAN_POINT ( 'NONE',  ( -4.821859908315634158, 5.654533310236863564, 1.199719254218452935 ) ) ;
#41014 = CARTESIAN_POINT ( 'NONE',  ( 0.7499999999999902300, 5.347916667349482012, -1.299038105676658228 ) ) ;
#41016 = ORIENTED_EDGE ( 'NONE', *, *, #73284, .T. ) ;
#41015 = CARTESIAN_POINT ( 'NONE',  ( 5.836161222118039227, -1.013825144121174526, -1.501122385605196952 ) ) ;
#41017 = CARTESIAN_POINT ( 'NONE',  ( 7.782016984564065432, 8.181367358187307204, 0.7216878364870458196 ) ) ;
#41018 = EDGE_CURVE ( 'NONE', #94296, #102958, #61083, .T. ) ;
#41019 = CARTESIAN_POINT ( 'NONE',  ( 9.561524646135536543, 12.17819805862340310, -1.599625672291262513 ) ) ;
#41020 = CARTESIAN_POINT ( 'NONE',  ( 4.821099876132087125, -0.09137817997613774390, 1.868553921495450965 ) ) ;
#41021 = CARTESIAN_POINT ( 'NONE',  ( 2.544126380858701797, 6.119897877643793116, 0.7998128361456462443 ) ) ;
#41022 = CARTESIAN_POINT ( 'NONE',  ( 4.118080132427735407, 2.055207691244304691, -0.2483996215696740451 ) ) ;
#41023 = CARTESIAN_POINT ( 'NONE',  ( -4.957638175832625493E-14, 1.687500000000000000, -1.414508159514599628 ) ) ;
#41024 = CARTESIAN_POINT ( 'NONE',  ( -5.953438849732214599, 6.118302544208584770, 0.7216878364870257245 ) ) ;
#41025 = DIRECTION ( 'NONE',  ( -0.000000000000000000, 1.000000000000000000, -0.000000000000000000 ) ) ;
#41026 = CARTESIAN_POINT ( 'NONE',  ( 8.727698198895078363, 11.20540053684285553, -1.599625672291257406 ) ) ;
#41027 = CARTESIAN_POINT ( 'NONE',  ( 7.666209513884374438, 7.908608952478760834, 0.7998128361456281477 ) ) ;
#41028 = CARTESIAN_POINT ( 'NONE',  ( 5.069834057255440563, 4.910074306249716969, -0.2341815111036758823 ) ) ;
#41029 = CARTESIAN_POINT ( 'NONE',  ( -1.364683531250014514, 0.4885416670080875434, -0.7879004041258289570 ) ) ;
#41030 = CARTESIAN_POINT ( 'NONE',  ( 1.499999999999989120, 1.025000000000019007, 0.000000000000000000 ) ) ;
#41031 = CARTESIAN_POINT ( 'NONE',  ( 4.123457186961496213, 0.2424046295769199388, -1.946780420294342617 ) ) ;
#41032 = CARTESIAN_POINT ( 'NONE',  ( 1.739611019359630584, -1.913509794028777522, -0.6351045200190530426 ) ) ;
#41033 = EDGE_CURVE ( 'NONE', #142064, #83117, #49874, .T. ) ;
#41034 = CARTESIAN_POINT ( 'NONE',  ( -0.1108833634136781182, 7.629137130509072939, -2.496956624467902675 ) ) ;
#41035 = CARTESIAN_POINT ( 'NONE',  ( -1.743066579297358008E-15, 2.187499999999992006, -1.225000000000032951 ) ) ;
#41036 = CARTESIAN_POINT ( 'NONE',  ( 1.669004442688322154, 0.1428430569143137041, -1.865171992484420338 ) ) ;
#41037 = CARTESIAN_POINT ( 'NONE',  ( -1.364683531250012516, 4.988541667008084879, -0.7879004041258300672 ) ) ;
#41038 = CARTESIAN_POINT ( 'NONE',  ( 3.709243207436668577, 1.698441389738635676, -1.080623863572414356 ) ) ;
#41039 = CARTESIAN_POINT ( 'NONE',  ( -9.155833807930273238, 9.576227618873799585, -0.7998128361456291469 ) ) ;
#41041 = CARTESIAN_POINT ( 'NONE',  ( 2.847379581703746609, 0.3079039886237054935, -2.094596350150164987 ) ) ;
#41040 = CARTESIAN_POINT ( 'NONE',  ( -5.083944415444539899, 8.875092884753202682, 0.000000000000000000 ) ) ;
#41042 = FACE_OUTER_BOUND ( 'NONE', #78205, .T. ) ;
#41043 = CARTESIAN_POINT ( 'NONE',  ( 4.615722581382986967, 0.4567890626981512270, -2.019179087418949692 ) ) ;
#41044 = CARTESIAN_POINT ( 'NONE',  ( 6.703580607314123085, 6.785541894813420072, 0.000000000000000000 ) ) ;
#41046 = CARTESIAN_POINT ( 'NONE',  ( 6.620655732516684822, 2.041257794637734602, 2.379778264366624096 ) ) ;
#41045 = CARTESIAN_POINT ( 'NONE',  ( -0.1234093946873336678, -0.1598125250084568849, -2.056614676860648583 ) ) ;
#41048 = EDGE_LOOP ( 'NONE', ( #21686, #169818, #71922, #166517 ) ) ;
#41047 = CARTESIAN_POINT ( 'NONE',  ( 4.911078036072877850, 1.588895129109271220, 0.8988584441092376531 ) ) ;
#41049 = CARTESIAN_POINT ( 'NONE',  ( 8.106885785967500979, 11.54545161934907682, 1.199719254218460707 ) ) ;
#41050 = CARTESIAN_POINT ( 'NONE',  ( 7.845789747616911392, -6.699703214240884996, -7.710100441483645817 ) ) ;
#41051 = CARTESIAN_POINT ( 'NONE',  ( -11.94980361058169116, 13.39999999999999858, 1.099999999999994982 ) ) ;
#41052 = CARTESIAN_POINT ( 'NONE',  ( -10.14895191633106819, 4.000000000000000888, 7.601392964450660372 ) ) ;
#41053 = CARTESIAN_POINT ( 'NONE',  ( 6.087247782411444597, 10.04561347954795281, -0.7216878364870267237 ) ) ;
#41054 = CARTESIAN_POINT ( 'NONE',  ( -0.6823417656250039265, 12.13020833367473017, -1.181850606188755259 ) ) ;
#41055 = CARTESIAN_POINT ( 'NONE',  ( -0.005635951793048382327, -1.756493610686832740, -0.4425278525194314971 ) ) ;
#41056 = CARTESIAN_POINT ( 'NONE',  ( -9.267161690140662600, 10.77044237904097734, -1.199719254218441611 ) ) ;
#41057 =( BOUNDED_SURFACE ( )  B_SPLINE_SURFACE ( 1, 2, ( 
 ( #210357, #79306, #177884, #97711, #128152, #195194, #132360, #160554, #148577, #15347, #198362, #61996, #48951, #146, #115069, #181065, #194112, #45762, #14277, #111880, #114017, #32683, #130271, #129220, #164819, #50002, #161638, #196260, #98763, #16410, #145422, #82490, #211423, #46831, #116126, #112944, #80372, #146467, #212486, #64128, #180013, #36939, #119330, #51070, #120409, #183193, #134488, #185317, #19620, #203688, #153908, #85692, #86765, #103021, #169076, #20675, #71558, #100874, #4411, #70482, #2279, #151780, #166961, #136598, #3353, #200491, #69423, #202622, #152836, #54272, #186384, #168017, #137666, #55334, #135529, #201553, #121486, #5478, #53199, #38021, #104092, #170141, #21727, #33743, #18551, #87837, #99821, #68355, #165887, #84628, #17472, #83556, #52136, #149638, #1220, #67282, #133421, #199427, #117195, #34799, #150719, #118264, #184248, #35875, #101950, #23879, #40156, #207964, #41238, #125747, #107345, #26016, #143022, #173367, #60653, #42303, #22803, #10824, #209017, #56402, #206899, #24951, #156036, #190643, #91053, #76898, #88917, #159223, #154971, #6556, #89985, #92127, #157114, #187458, #174440, #7625, #58530, #140887, #8703, #72636, #73710, #123628, #158179, #139808, #124685, #93192, #74787, #108418, #138733, #172291, #188525, #9772, #109489, #75845, #122563, #105172, #106269, #205836, #141952, #204751, #57469, #39086, #171209, #27084, #59590, #189592, #191709, #43367, #175496, #179753, #97446, #214318, #44431, #62781, #176550, #80101, #113749, #162439, #161375, #197050, #82228, #192772, #14015, #213287, #196003, #126816, #64913, #61729, #193848, #164558, #111614, #148319, #177626, #79036, #30302, #31370, #130012, #212221, #144095, #131062, #127897, #12958, #63856, #112679, #145151, #29234, #147255, #45498, #163502, #128944, #48688, #211157, #95326, #15086, #194922, #178689, #47637, #110548, #77972, #46559, #81176, #96388, #146205, #114803, #180802, #32428, #98494, #16143, #28160, #94256, #160295, #11898, #210090, #70226, #116932, #136337, #133158, #149373, #99559, #182931, #83288, #956, #183994, #103830, #50804, #135278, #120146, #34547, #84370, #67022, #65950, #49738, #134222, #199159, #100618, #115865, #87577, #150458, #166693, #85434, #18284, #54007, #4155, #200232, #198108, #51882, #2019, #68088, #186123, #118005, #35608, #168817, #101686, #17212, #202357, #167755, #19354, #181850, #33487, #151519, #37757, #169878, #132099, #52933, #3087, #69158, #201292, #119068, #165624, #36674, #185049, #102762, #20421, #21468, #86503, #152568, #153648, #5217, #123372, #104909, #40978, #23626, #24692, #189339, #187197, #138471, #26832, #74532, #90795, #55078, #156859, #191457, #188262, #42050, #91873, #203423, #107089, #71292, #72371, #124434, #57212, #43122, #206645, #204493, #109236, #6296, #173111, #174189, #157929, #73444, #39902, #175246, #121227, #106011, #125494, #75594, #137404, #58278, #172033, #89734, #154715, #22549, #170950, #190392, #56143, #155783, #88655, #9522, #140632, #8445, #92935, #38825, #108162, #122304, #25761, #7367, #141706, #207717, #139548, #205575, #59340, #13774, #178439, #208770, #96135, #130812, #127637, #195746, #31124, #142765, #128696, #10576, #11647, #63607, #210907, #196802, #145958, #77719, #48445, #160043, #62534, #113496, #97198, #12701, #193602, #114559, #111361, #143841, #179503, #209835, #47383, #95066, #163251, #177366, #94004, #211968, #161114, #194664, #162187, #158979, #110296, #78778, #14833, #144899, #61472, #28980, #46309, #112425, #30045, #79849, #129763, #147014, #45244, #80924, #213037, #64666, #180552, #32173, #76650, #27907, #192522, #60400, #176304, #126562, #44176, #136077, #83038, #167501, #152318, #149113, #116671, #99314, #98250, #81979, #166433, #165364, #16957, #148067, #119885, #182669, #115608, #117753, #693, #86248, #36422, #18024, #15895, #84111, #66758, #181603, #3895, #132899, #100363, #201035, #198904, #49487, #102498, #50549, #34291, #214073, #150199, #1770, #69967, #67826, #133973, #118809, #199981, #135021, #51628, #184794, #183743, #33231, #151261, #35353, #101429, #19099, #164307, #85177, #2833, #52678, #68902 ),
 ( #168562, #20161, #131847, #202094, #53752, #185862, #65699, #197856, #38572, #73180, #74278, #104647, #6037, #120969, #37497, #21214, #55882, #170693, #22280, #87318, #41797, #138217, #203175, #155526, #186939, #140372, #90537, #122040, #153385, #188004, #88392, #54820, #206389, #154459, #204230, #106824, #72108, #137148, #156602, #39630, #105739, #4957, #71036, #171766, #58016, #8193, #103573, #56954, #23362, #89472, #7106, #139286, #205316, #40718, #123126, #189085, #172854, #124180, #24425, #190143, #169631, #16590, #134666, #116309, #52319, #34983, #36052, #200669, #198542, #149830, #38204, #85884, #102132, #66396, #168201, #202807, #199612, #53379, #103204, #326, #118448, #82672, #83738, #135712, #68538, #54456, #3530, #1400, #120599, #17655, #184435, #185500, #169266, #51255, #182299, #20852, #151960, #19800, #104278, #148756, #69605, #33927, #201738, #101054, #119514, #37125, #50188, #67461, #132544, #86950, #153019, #100001, #4594, #186576, #117380, #70668, #136778, #166068, #133607, #183377, #167143, #18728, #84812, #150901, #2462, #92036, #145065, #174349, #10740, #127808, #45408, #26990, #59499, #211068, #125656, #158093, #193762, #25928, #209998, #109401, #111524, #191618, #108329, #11809, #175407, #76810, #110461, #170322, #121674, #93097, #61640, #159138, #9681, #43280, #208930, #60565, #142930, #126724, #192685, #161280, #44339, #75758, #77884, #177530, #141867, #29143, #176461, #42212, #203874, #28074, #190557, #94167, #160208, #62691, #144006, #95232, #12867, #128850, #194833, #46467, #21910, #154091, #5659, #71739, #137853, #55518, #200150, #32341, #195912, #49653, #98407, #68002, #112590, #16058, #162351, #65864, #181765, #47549, #178602, #33398, #867, #80013, #118988, #3007, #204409, #36592, #4074, #35527, #101603, #86426, #171947, #122219, #51804, #38745, #20340, #136256, #201214, #69077, #151436, #22463, #184966, #155698, #7280, #37675, #153566, #135197, #5135, #102679, #168737, #72283, #120064, #56062, #186040, #104826, #73357, #103752, #139461, #121148, #167671, #89645, #117922, #52854, #71211, #169802, #152491, #54996, #21391, #183916, #19272, #23536, #85354, #70144, #202276, #170872, #87501, #53927, #88575, #137327, #203344, #187112, #154632, #6212, #138391, #188180, #39815, #105922, #158897, #111279, #191371, #175163, #173025, #190307, #206564, #26750, #127556, #60316, #140551, #123292, #124350, #74447, #208687, #24606, #91786, #177284, #57126, #45167, #126475, #28899, #78696, #192439, #94984, #44094, #176221, #205492, #189256, #141620, #40895, #10493, #110214, #92851, #25678, #61394, #161030, #107000, #76566, #77636, #27823, #90715, #143758, #58191, #41965, #12625, #108077, #156777, #174106, #157842, #109150, #93921, #159961, #142677, #8364, #209753, #9438, #75508, #11566, #43038, #207629, #59247, #193525, #125405, #142541, #126340, #76433, #177143, #206427, #110075, #176087, #107944, #125274, #58051, #27685, #191236, #91652, #42899, #93784, #208547, #159820, #11423, #59117, #172888, #25544, #111143, #205353, #193385, #192300, #28760, #12491, #43959, #45029, #77499, #143618, #139322, #56987, #75375, #189120, #92715, #209612, #175027, #173970, #61255, #94844, #123160, #26614, #127413, #160895, #40755, #106861, #74312, #124216, #24463, #190178, #90576, #41833, #157705, #109008, #156636, #8229, #10356, #140409, #9302, #141489, #207495, #158761, #64457, #34077, #198692, #130601, #131637, #81769, #213867, #15682, #116456, #145754, #49284, #115403, #47167, #196590, #211754, #181396, #114345, #96986, #180342, #33020, #147849, #99097, #165150, #212821, #182449, #100146, #31963, #98046, #29835, #164099, #129546, #63392, #16741, #65490, #82826, #197640, #148902, #78564, #132685, #144684, #50336, #128484, #210695, #62324, #161973, #46095, #112211, #113281, #178220, #95919, #13563, #79635, #195528, #179287, #163037, #14617, #136929, #152105, #17802, #54599, #68688, #103349, #185648, #86031, #117528, #184580, #168352, #120747, #134810, #37279, #204014, #69754, #201879, #183522, #36199, #84960, #53528, #154239, #153165, #151049, #1548, #102274, #101203, #186721, #38348, #135858, #104425, #119662 ) ),
 .UNSPECIFIED., .F., .F., .T. ) 
 B_SPLINE_SURFACE_WITH_KNOTS ( ( 2, 2 ),
 ( 3, 2, 2, 2, 2, 2, 2, 2, 2, 2, 2, 2, 2, 2, 2, 2, 2, 2, 2, 2, 2, 2, 2, 2, 2, 2, 2, 2, 2, 2, 2, 2, 2, 2, 2, 2, 2, 2, 2, 2, 2, 2, 2, 2, 2, 2, 2, 2, 2, 2, 2, 2, 2, 2, 2, 2, 2, 2, 2, 2, 2, 2, 2, 2, 2, 2, 2, 2, 2, 2, 2, 2, 2, 2, 2, 2, 2, 2, 2, 2, 2, 2, 2, 2, 2, 2, 2, 2, 2, 2, 2, 2, 2, 2, 2, 2, 2, 2, 2, 2, 2, 2, 2, 2, 2, 2, 2, 2, 2, 2, 2, 2, 2, 2, 2, 2, 2, 2, 2, 2, 2, 2, 2, 2, 2, 2, 2, 2, 2, 2, 2, 2, 2, 2, 2, 2, 2, 2, 2, 2, 2, 2, 2, 2, 2, 2, 2, 2, 2, 2, 2, 2, 2, 2, 2, 2, 2, 2, 2, 2, 2, 2, 2, 2, 2, 2, 2, 2, 2, 2, 2, 2, 2, 2, 2, 2, 2, 2, 2, 2, 2, 2, 2, 2, 2, 2, 2, 2, 2, 2, 2, 2, 2, 2, 2, 2, 2, 2, 2, 2, 2, 2, 2, 2, 2, 2, 2, 2, 2, 2, 2, 2, 2, 2, 2, 2, 2, 2, 2, 2, 2, 2, 2, 2, 2, 2, 2, 2, 2, 2, 2, 2, 2, 2, 2, 2, 2, 2, 2, 2, 3 ),
 ( 0.000000000000000000, 1.000000000000000000 ),
 ( 0.000000000000000000, 0.004166666666666666609, 0.008333333333333333218, 0.01250000000000000069, 0.01666666666666666644, 0.02083333333333333218, 0.02500000000000000139, 0.02916666666666666713, 0.03333333333333333287, 0.03749999999999999861, 0.04166666666666666435, 0.04583333333333333010, 0.05000000000000000278, 0.05416666666666666852, 0.05833333333333333426, 0.06250000000000000000, 0.06666666666666666574, 0.07083333333333333148, 0.07499999999999999722, 0.07916666666666666297, 0.08333333333333332871, 0.08749999999999999445, 0.09166666666666666019, 0.09583333333333333981, 0.1000000000000000056, 0.1041666666666666713, 0.1083333333333333370, 0.1125000000000000028, 0.1166666666666666685, 0.1208333333333333343, 0.1250000000000000000, 0.1291666666666666796, 0.1333333333333333315, 0.1375000000000000111, 0.1416666666666666630, 0.1458333333333333426, 0.1499999999999999944, 0.1541666666666666741, 0.1583333333333333259, 0.1625000000000000056, 0.1666666666666666574, 0.1708333333333333370, 0.1749999999999999889, 0.1791666666666666685, 0.1833333333333333204, 0.1875000000000000000, 0.1916666666666666796, 0.1958333333333333315, 0.2000000000000000111, 0.2041666666666666630, 0.2083333333333333426, 0.2124999999999999944, 0.2166666666666666741, 0.2208333333333333259, 0.2250000000000000056, 0.2291666666666666574, 0.2333333333333333370, 0.2374999999999999889, 0.2416666666666666685, 0.2458333333333333204, 0.2500000000000000000, 0.2541666666666666519, 0.2583333333333333592, 0.2625000000000000111, 0.2666666666666666630, 0.2708333333333333148, 0.2750000000000000222, 0.2791666666666666741, 0.2833333333333333259, 0.2874999999999999778, 0.2916666666666666852, 0.2958333333333333370, 0.2999999999999999889, 0.3041666666666666408, 0.3083333333333333481, 0.3125000000000000000, 0.3166666666666666519, 0.3208333333333333592, 0.3250000000000000111, 0.3291666666666666630, 0.3333333333333333148, 0.3375000000000000222, 0.3416666666666666741, 0.3458333333333333259, 0.3499999999999999778, 0.3541666666666666852, 0.3583333333333333370, 0.3624999999999999889, 0.3666666666666666408, 0.3708333333333333481, 0.3750000000000000000, 0.3791666666666666519, 0.3833333333333333592, 0.3875000000000000111, 0.3916666666666666630, 0.3958333333333333148, 0.4000000000000000222, 0.4041666666666666741, 0.4083333333333333259, 0.4124999999999999778, 0.4166666666666666852, 0.4208333333333333370, 0.4249999999999999889, 0.4291666666666666408, 0.4333333333333333481, 0.4375000000000000000, 0.4416666666666666519, 0.4458333333333333592, 0.4500000000000000111, 0.4541666666666666630, 0.4583333333333333148, 0.4625000000000000222, 0.4666666666666666741, 0.4708333333333333259, 0.4749999999999999778, 0.4791666666666666852, 0.4833333333333333370, 0.4874999999999999889, 0.4916666666666666408, 0.4958333333333333481, 0.5000000000000000000, 0.5041666666666666519, 0.5083333333333333037, 0.5124999999999999556, 0.5166666666666667185, 0.5208333333333333703, 0.5250000000000000222, 0.5291666666666666741, 0.5333333333333333259, 0.5374999999999999778, 0.5416666666666666297, 0.5458333333333332815, 0.5500000000000000444, 0.5541666666666666963, 0.5583333333333333481, 0.5625000000000000000, 0.5666666666666666519, 0.5708333333333333037, 0.5749999999999999556, 0.5791666666666667185, 0.5833333333333333703, 0.5875000000000000222, 0.5916666666666666741, 0.5958333333333333259, 0.5999999999999999778, 0.6041666666666666297, 0.6083333333333332815, 0.6125000000000000444, 0.6166666666666666963, 0.6208333333333333481, 0.6250000000000000000, 0.6291666666666666519, 0.6333333333333333037, 0.6374999999999999556, 0.6416666666666667185, 0.6458333333333333703, 0.6500000000000000222, 0.6541666666666666741, 0.6583333333333333259, 0.6624999999999999778, 0.6666666666666666297, 0.6708333333333332815, 0.6750000000000000444, 0.6791666666666666963, 0.6833333333333333481, 0.6875000000000000000, 0.6916666666666666519, 0.6958333333333333037, 0.6999999999999999556, 0.7041666666666667185, 0.7083333333333333703, 0.7125000000000000222, 0.7166666666666666741, 0.7208333333333333259, 0.7249999999999999778, 0.7291666666666666297, 0.7333333333333332815, 0.7375000000000000444, 0.7416666666666666963, 0.7458333333333333481, 0.7500000000000000000, 0.7541666666666666519, 0.7583333333333333037, 0.7624999999999999556, 0.7666666666666667185, 0.7708333333333333703, 0.7750000000000000222, 0.7791666666666666741, 0.7833333333333333259, 0.7874999999999999778, 0.7916666666666666297, 0.7958333333333332815, 0.8000000000000000444, 0.8041666666666666963, 0.8083333333333333481, 0.8125000000000000000, 0.8166666666666666519, 0.8208333333333333037, 0.8249999999999999556, 0.8291666666666667185, 0.8333333333333333703, 0.8375000000000000222, 0.8416666666666666741, 0.8458333333333333259, 0.8499999999999999778, 0.8541666666666666297, 0.8583333333333332815, 0.8625000000000000444, 0.8666666666666666963, 0.8708333333333333481, 0.8750000000000000000, 0.8791666666666666519, 0.8833333333333333037, 0.8874999999999999556, 0.8916666666666667185, 0.8958333333333333703, 0.9000000000000000222, 0.9041666666666666741, 0.9083333333333333259, 0.9124999999999999778, 0.9166666666666666297, 0.9208333333333332815, 0.9250000000000000444, 0.9291666666666666963, 0.9333333333333333481, 0.9375000000000000000, 0.9416666666666666519, 0.9458333333333333037, 0.9499999999999999556, 0.9541666666666667185, 0.9583333333333333703, 0.9625000000000000222, 0.9666666666666666741, 0.9708333333333333259, 0.9749999999999999778, 0.9791666666666666297, 0.9833333333333332815, 0.9875000000000000444, 0.9916666666666666963, 0.9958333333333333481, 1.000000000000000000 ),
 .UNSPECIFIED. ) 
 GEOMETRIC_REPRESENTATION_ITEM ( )  RATIONAL_B_SPLINE_SURFACE ( (
 ( 1.000000000000000000, 0.8660254037844387076, 1.000000000000000000, 0.8660254037844387076, 1.000000000000000000, 0.8660254037844387076, 1.000000000000000000, 0.8660254037844387076, 1.000000000000000000, 0.8660254037844387076, 1.000000000000000000, 0.8660254037844387076, 1.000000000000000000, 0.8660254037844387076, 1.000000000000000000, 0.8660254037844387076, 1.000000000000000000, 0.8660254037844387076, 1.000000000000000000, 0.8660254037844387076, 1.000000000000000000, 0.8660254037844387076, 1.000000000000000000, 0.8660254037844387076, 1.000000000000000000, 0.8660254037844387076, 1.000000000000000000, 0.8660254037844387076, 1.000000000000000000, 0.8660254037844387076, 1.000000000000000000, 0.8660254037844387076, 1.000000000000000000, 0.8660254037844387076, 1.000000000000000000, 0.8660254037844387076, 1.000000000000000000, 0.8660254037844387076, 1.000000000000000000, 0.8660254037844387076, 1.000000000000000000, 0.8660254037844387076, 1.000000000000000000, 0.8660254037844387076, 1.000000000000000000, 0.8660254037844387076, 1.000000000000000000, 0.8660254037844387076, 1.000000000000000000, 0.8660254037844387076, 1.000000000000000000, 0.8660254037844387076, 1.000000000000000000, 0.8660254037844387076, 1.000000000000000000, 0.8660254037844387076, 1.000000000000000000, 0.8660254037844387076, 1.000000000000000000, 0.8660254037844387076, 1.000000000000000000, 0.8660254037844387076, 1.000000000000000000, 0.8660254037844387076, 1.000000000000000000, 0.8660254037844387076, 1.000000000000000000, 0.8660254037844387076, 1.000000000000000000, 0.8660254037844387076, 1.000000000000000000, 0.8660254037844387076, 1.000000000000000000, 0.8660254037844387076, 1.000000000000000000, 0.8660254037844387076, 1.000000000000000000, 0.8660254037844387076, 1.000000000000000000, 0.8660254037844387076, 1.000000000000000000, 0.8660254037844387076, 1.000000000000000000, 0.8660254037844387076, 1.000000000000000000, 0.8660254037844387076, 1.000000000000000000, 0.8660254037844387076, 1.000000000000000000, 0.8660254037844387076, 1.000000000000000000, 0.8660254037844387076, 1.000000000000000000, 0.8660254037844387076, 1.000000000000000000, 0.8660254037844387076, 1.000000000000000000, 0.8660254037844387076, 1.000000000000000000, 0.8660254037844387076, 1.000000000000000000, 0.8660254037844387076, 1.000000000000000000, 0.8660254037844387076, 1.000000000000000000, 0.8660254037844387076, 1.000000000000000000, 0.8660254037844387076, 1.000000000000000000, 0.8660254037844387076, 1.000000000000000000, 0.8660254037844387076, 1.000000000000000000, 0.8660254037844387076, 1.000000000000000000, 0.8660254037844387076, 1.000000000000000000, 0.8660254037844387076, 1.000000000000000000, 0.8660254037844387076, 1.000000000000000000, 0.8660254037844387076, 1.000000000000000000, 0.8660254037844387076, 1.000000000000000000, 0.8660254037844387076, 1.000000000000000000, 0.8660254037844387076, 1.000000000000000000, 0.8660254037844387076, 1.000000000000000000, 0.8660254037844387076, 1.000000000000000000, 0.8660254037844387076, 1.000000000000000000, 0.8660254037844387076, 1.000000000000000000, 0.8660254037844387076, 1.000000000000000000, 0.8660254037844387076, 1.000000000000000000, 0.8660254037844387076, 1.000000000000000000, 0.8660254037844387076, 1.000000000000000000, 0.8660254037844387076, 1.000000000000000000, 0.8660254037844387076, 1.000000000000000000, 0.8660254037844387076, 1.000000000000000000, 0.8660254037844387076, 1.000000000000000000, 0.8660254037844387076, 1.000000000000000000, 0.8660254037844387076, 1.000000000000000000, 0.8660254037844387076, 1.000000000000000000, 0.8660254037844387076, 1.000000000000000000, 0.8660254037844387076, 1.000000000000000000, 0.8660254037844387076, 1.000000000000000000, 0.8660254037844387076, 1.000000000000000000, 0.8660254037844387076, 1.000000000000000000, 0.8660254037844387076, 1.000000000000000000, 0.8660254037844387076, 1.000000000000000000, 0.8660254037844387076, 1.000000000000000000, 0.8660254037844387076, 1.000000000000000000, 0.8660254037844387076, 1.000000000000000000, 0.8660254037844387076, 1.000000000000000000, 0.8660254037844387076, 1.000000000000000000, 0.8660254037844387076, 1.000000000000000000, 0.8660254037844387076, 1.000000000000000000, 0.8660254037844387076, 1.000000000000000000, 0.8660254037844387076, 1.000000000000000000, 0.8660254037844387076, 1.000000000000000000, 0.8660254037844387076, 1.000000000000000000, 0.8660254037844387076, 1.000000000000000000, 0.8660254037844387076, 1.000000000000000000, 0.8660254037844387076, 1.000000000000000000, 0.8660254037844387076, 1.000000000000000000, 0.8660254037844387076, 1.000000000000000000, 0.8660254037844387076, 1.000000000000000000, 0.8660254037844387076, 1.000000000000000000, 0.8660254037844387076, 1.000000000000000000, 0.8660254037844387076, 1.000000000000000000, 0.8660254037844387076, 1.000000000000000000, 0.8660254037844387076, 1.000000000000000000, 0.8660254037844387076, 1.000000000000000000, 0.8660254037844387076, 1.000000000000000000, 0.8660254037844387076, 1.000000000000000000, 0.8660254037844387076, 1.000000000000000000, 0.8660254037844387076, 1.000000000000000000, 0.8660254037844387076, 1.000000000000000000, 0.8660254037844387076, 1.000000000000000000, 0.8660254037844387076, 1.000000000000000000, 0.8660254037844387076, 1.000000000000000000, 0.8660254037844387076, 1.000000000000000000, 0.8660254037844387076, 1.000000000000000000, 0.8660254037844387076, 1.000000000000000000, 0.8660254037844387076, 1.000000000000000000, 0.8660254037844387076, 1.000000000000000000, 0.8660254037844387076, 1.000000000000000000, 0.8660254037844387076, 1.000000000000000000, 0.8660254037844387076, 1.000000000000000000, 0.8660254037844387076, 1.000000000000000000, 0.8660254037844387076, 1.000000000000000000, 0.8660254037844387076, 1.000000000000000000, 0.8660254037844387076, 1.000000000000000000, 0.8660254037844387076, 1.000000000000000000, 0.8660254037844387076, 1.000000000000000000, 0.8660254037844387076, 1.000000000000000000, 0.8660254037844387076, 1.000000000000000000, 0.8660254037844387076, 1.000000000000000000, 0.8660254037844387076, 1.000000000000000000, 0.8660254037844387076, 1.000000000000000000, 0.8660254037844387076, 1.000000000000000000, 0.8660254037844387076, 1.000000000000000000, 0.8660254037844387076, 1.000000000000000000, 0.8660254037844387076, 1.000000000000000000, 0.8660254037844387076, 1.000000000000000000, 0.8660254037844387076, 1.000000000000000000, 0.8660254037844387076, 1.000000000000000000, 0.8660254037844387076, 1.000000000000000000, 0.8660254037844387076, 1.000000000000000000, 0.8660254037844387076, 1.000000000000000000, 0.8660254037844387076, 1.000000000000000000, 0.8660254037844387076, 1.000000000000000000, 0.8660254037844387076, 1.000000000000000000, 0.8660254037844387076, 1.000000000000000000, 0.8660254037844387076, 1.000000000000000000, 0.8660254037844387076, 1.000000000000000000, 0.8660254037844387076, 1.000000000000000000, 0.8660254037844387076, 1.000000000000000000, 0.8660254037844387076, 1.000000000000000000, 0.8660254037844387076, 1.000000000000000000, 0.8660254037844387076, 1.000000000000000000, 0.8660254037844387076, 1.000000000000000000, 0.8660254037844387076, 1.000000000000000000, 0.8660254037844387076, 1.000000000000000000, 0.8660254037844387076, 1.000000000000000000, 0.8660254037844387076, 1.000000000000000000, 0.8660254037844387076, 1.000000000000000000, 0.8660254037844387076, 1.000000000000000000, 0.8660254037844387076, 1.000000000000000000, 0.8660254037844387076, 1.000000000000000000, 0.8660254037844387076, 1.000000000000000000, 0.8660254037844387076, 1.000000000000000000, 0.8660254037844387076, 1.000000000000000000, 0.8660254037844387076, 1.000000000000000000, 0.8660254037844387076, 1.000000000000000000, 0.8660254037844387076, 1.000000000000000000, 0.8660254037844387076, 1.000000000000000000, 0.8660254037844387076, 1.000000000000000000, 0.8660254037844387076, 1.000000000000000000, 0.8660254037844387076, 1.000000000000000000, 0.8660254037844387076, 1.000000000000000000, 0.8660254037844387076, 1.000000000000000000, 0.8660254037844387076, 1.000000000000000000, 0.8660254037844387076, 1.000000000000000000, 0.8660254037844387076, 1.000000000000000000, 0.8660254037844387076, 1.000000000000000000, 0.8660254037844387076, 1.000000000000000000, 0.8660254037844387076, 1.000000000000000000, 0.8660254037844387076, 1.000000000000000000, 0.8660254037844387076, 1.000000000000000000, 0.8660254037844387076, 1.000000000000000000, 0.8660254037844387076, 1.000000000000000000, 0.8660254037844387076, 1.000000000000000000, 0.8660254037844387076, 1.000000000000000000, 0.8660254037844387076, 1.000000000000000000, 0.8660254037844387076, 1.000000000000000000, 0.8660254037844387076, 1.000000000000000000, 0.8660254037844387076, 1.000000000000000000, 0.8660254037844387076, 1.000000000000000000, 0.8660254037844387076, 1.000000000000000000, 0.8660254037844387076, 1.000000000000000000, 0.8660254037844387076, 1.000000000000000000, 0.8660254037844387076, 1.000000000000000000, 0.8660254037844387076, 1.000000000000000000, 0.8660254037844387076, 1.000000000000000000, 0.8660254037844387076, 1.000000000000000000, 0.8660254037844387076, 1.000000000000000000, 0.8660254037844387076, 1.000000000000000000, 0.8660254037844387076, 1.000000000000000000, 0.8660254037844387076, 1.000000000000000000, 0.8660254037844387076, 1.000000000000000000, 0.8660254037844387076, 1.000000000000000000, 0.8660254037844387076, 1.000000000000000000, 0.8660254037844387076, 1.000000000000000000, 0.8660254037844387076, 1.000000000000000000, 0.8660254037844387076, 1.000000000000000000, 0.8660254037844387076, 1.000000000000000000, 0.8660254037844387076, 1.000000000000000000, 0.8660254037844387076, 1.000000000000000000, 0.8660254037844387076, 1.000000000000000000, 0.8660254037844387076, 1.000000000000000000, 0.8660254037844387076, 1.000000000000000000, 0.8660254037844387076, 1.000000000000000000, 0.8660254037844387076, 1.000000000000000000, 0.8660254037844387076, 1.000000000000000000, 0.8660254037844387076, 1.000000000000000000, 0.8660254037844387076, 1.000000000000000000, 0.8660254037844387076, 1.000000000000000000, 0.8660254037844387076, 1.000000000000000000, 0.8660254037844387076, 1.000000000000000000, 0.8660254037844387076, 1.000000000000000000, 0.8660254037844387076, 1.000000000000000000, 0.8660254037844387076, 1.000000000000000000, 0.8660254037844387076, 1.000000000000000000, 0.8660254037844387076, 1.000000000000000000, 0.8660254037844387076, 1.000000000000000000, 0.8660254037844387076, 1.000000000000000000, 0.8660254037844387076, 1.000000000000000000, 0.8660254037844387076, 1.000000000000000000, 0.8660254037844387076, 1.000000000000000000, 0.8660254037844387076, 1.000000000000000000, 0.8660254037844387076, 1.000000000000000000, 0.8660254037844387076, 1.000000000000000000, 0.8660254037844387076, 1.000000000000000000),
 ( 1.000000000000000000, 0.8660254037844387076, 1.000000000000000000, 0.8660254037844387076, 1.000000000000000000, 0.8660254037844387076, 1.000000000000000000, 0.8660254037844387076, 1.000000000000000000, 0.8660254037844387076, 1.000000000000000000, 0.8660254037844387076, 1.000000000000000000, 0.8660254037844387076, 1.000000000000000000, 0.8660254037844387076, 1.000000000000000000, 0.8660254037844387076, 1.000000000000000000, 0.8660254037844387076, 1.000000000000000000, 0.8660254037844387076, 1.000000000000000000, 0.8660254037844387076, 1.000000000000000000, 0.8660254037844387076, 1.000000000000000000, 0.8660254037844387076, 1.000000000000000000, 0.8660254037844387076, 1.000000000000000000, 0.8660254037844387076, 1.000000000000000000, 0.8660254037844387076, 1.000000000000000000, 0.8660254037844387076, 1.000000000000000000, 0.8660254037844387076, 1.000000000000000000, 0.8660254037844387076, 1.000000000000000000, 0.8660254037844387076, 1.000000000000000000, 0.8660254037844387076, 1.000000000000000000, 0.8660254037844387076, 1.000000000000000000, 0.8660254037844387076, 1.000000000000000000, 0.8660254037844387076, 1.000000000000000000, 0.8660254037844387076, 1.000000000000000000, 0.8660254037844387076, 1.000000000000000000, 0.8660254037844387076, 1.000000000000000000, 0.8660254037844387076, 1.000000000000000000, 0.8660254037844387076, 1.000000000000000000, 0.8660254037844387076, 1.000000000000000000, 0.8660254037844387076, 1.000000000000000000, 0.8660254037844387076, 1.000000000000000000, 0.8660254037844387076, 1.000000000000000000, 0.8660254037844387076, 1.000000000000000000, 0.8660254037844387076, 1.000000000000000000, 0.8660254037844387076, 1.000000000000000000, 0.8660254037844387076, 1.000000000000000000, 0.8660254037844387076, 1.000000000000000000, 0.8660254037844387076, 1.000000000000000000, 0.8660254037844387076, 1.000000000000000000, 0.8660254037844387076, 1.000000000000000000, 0.8660254037844387076, 1.000000000000000000, 0.8660254037844387076, 1.000000000000000000, 0.8660254037844387076, 1.000000000000000000, 0.8660254037844387076, 1.000000000000000000, 0.8660254037844387076, 1.000000000000000000, 0.8660254037844387076, 1.000000000000000000, 0.8660254037844387076, 1.000000000000000000, 0.8660254037844387076, 1.000000000000000000, 0.8660254037844387076, 1.000000000000000000, 0.8660254037844387076, 1.000000000000000000, 0.8660254037844387076, 1.000000000000000000, 0.8660254037844387076, 1.000000000000000000, 0.8660254037844387076, 1.000000000000000000, 0.8660254037844387076, 1.000000000000000000, 0.8660254037844387076, 1.000000000000000000, 0.8660254037844387076, 1.000000000000000000, 0.8660254037844387076, 1.000000000000000000, 0.8660254037844387076, 1.000000000000000000, 0.8660254037844387076, 1.000000000000000000, 0.8660254037844387076, 1.000000000000000000, 0.8660254037844387076, 1.000000000000000000, 0.8660254037844387076, 1.000000000000000000, 0.8660254037844387076, 1.000000000000000000, 0.8660254037844387076, 1.000000000000000000, 0.8660254037844387076, 1.000000000000000000, 0.8660254037844387076, 1.000000000000000000, 0.8660254037844387076, 1.000000000000000000, 0.8660254037844387076, 1.000000000000000000, 0.8660254037844387076, 1.000000000000000000, 0.8660254037844387076, 1.000000000000000000, 0.8660254037844387076, 1.000000000000000000, 0.8660254037844387076, 1.000000000000000000, 0.8660254037844387076, 1.000000000000000000, 0.8660254037844387076, 1.000000000000000000, 0.8660254037844387076, 1.000000000000000000, 0.8660254037844387076, 1.000000000000000000, 0.8660254037844387076, 1.000000000000000000, 0.8660254037844387076, 1.000000000000000000, 0.8660254037844387076, 1.000000000000000000, 0.8660254037844387076, 1.000000000000000000, 0.8660254037844387076, 1.000000000000000000, 0.8660254037844387076, 1.000000000000000000, 0.8660254037844387076, 1.000000000000000000, 0.8660254037844387076, 1.000000000000000000, 0.8660254037844387076, 1.000000000000000000, 0.8660254037844387076, 1.000000000000000000, 0.8660254037844387076, 1.000000000000000000, 0.8660254037844387076, 1.000000000000000000, 0.8660254037844387076, 1.000000000000000000, 0.8660254037844387076, 1.000000000000000000, 0.8660254037844387076, 1.000000000000000000, 0.8660254037844387076, 1.000000000000000000, 0.8660254037844387076, 1.000000000000000000, 0.8660254037844387076, 1.000000000000000000, 0.8660254037844387076, 1.000000000000000000, 0.8660254037844387076, 1.000000000000000000, 0.8660254037844387076, 1.000000000000000000, 0.8660254037844387076, 1.000000000000000000, 0.8660254037844387076, 1.000000000000000000, 0.8660254037844387076, 1.000000000000000000, 0.8660254037844387076, 1.000000000000000000, 0.8660254037844387076, 1.000000000000000000, 0.8660254037844387076, 1.000000000000000000, 0.8660254037844387076, 1.000000000000000000, 0.8660254037844387076, 1.000000000000000000, 0.8660254037844387076, 1.000000000000000000, 0.8660254037844387076, 1.000000000000000000, 0.8660254037844387076, 1.000000000000000000, 0.8660254037844387076, 1.000000000000000000, 0.8660254037844387076, 1.000000000000000000, 0.8660254037844387076, 1.000000000000000000, 0.8660254037844387076, 1.000000000000000000, 0.8660254037844387076, 1.000000000000000000, 0.8660254037844387076, 1.000000000000000000, 0.8660254037844387076, 1.000000000000000000, 0.8660254037844387076, 1.000000000000000000, 0.8660254037844387076, 1.000000000000000000, 0.8660254037844387076, 1.000000000000000000, 0.8660254037844387076, 1.000000000000000000, 0.8660254037844387076, 1.000000000000000000, 0.8660254037844387076, 1.000000000000000000, 0.8660254037844387076, 1.000000000000000000, 0.8660254037844387076, 1.000000000000000000, 0.8660254037844387076, 1.000000000000000000, 0.8660254037844387076, 1.000000000000000000, 0.8660254037844387076, 1.000000000000000000, 0.8660254037844387076, 1.000000000000000000, 0.8660254037844387076, 1.000000000000000000, 0.8660254037844387076, 1.000000000000000000, 0.8660254037844387076, 1.000000000000000000, 0.8660254037844387076, 1.000000000000000000, 0.8660254037844387076, 1.000000000000000000, 0.8660254037844387076, 1.000000000000000000, 0.8660254037844387076, 1.000000000000000000, 0.8660254037844387076, 1.000000000000000000, 0.8660254037844387076, 1.000000000000000000, 0.8660254037844387076, 1.000000000000000000, 0.8660254037844387076, 1.000000000000000000, 0.8660254037844387076, 1.000000000000000000, 0.8660254037844387076, 1.000000000000000000, 0.8660254037844387076, 1.000000000000000000, 0.8660254037844387076, 1.000000000000000000, 0.8660254037844387076, 1.000000000000000000, 0.8660254037844387076, 1.000000000000000000, 0.8660254037844387076, 1.000000000000000000, 0.8660254037844387076, 1.000000000000000000, 0.8660254037844387076, 1.000000000000000000, 0.8660254037844387076, 1.000000000000000000, 0.8660254037844387076, 1.000000000000000000, 0.8660254037844387076, 1.000000000000000000, 0.8660254037844387076, 1.000000000000000000, 0.8660254037844387076, 1.000000000000000000, 0.8660254037844387076, 1.000000000000000000, 0.8660254037844387076, 1.000000000000000000, 0.8660254037844387076, 1.000000000000000000, 0.8660254037844387076, 1.000000000000000000, 0.8660254037844387076, 1.000000000000000000, 0.8660254037844387076, 1.000000000000000000, 0.8660254037844387076, 1.000000000000000000, 0.8660254037844387076, 1.000000000000000000, 0.8660254037844387076, 1.000000000000000000, 0.8660254037844387076, 1.000000000000000000, 0.8660254037844387076, 1.000000000000000000, 0.8660254037844387076, 1.000000000000000000, 0.8660254037844387076, 1.000000000000000000, 0.8660254037844387076, 1.000000000000000000, 0.8660254037844387076, 1.000000000000000000, 0.8660254037844387076, 1.000000000000000000, 0.8660254037844387076, 1.000000000000000000, 0.8660254037844387076, 1.000000000000000000, 0.8660254037844387076, 1.000000000000000000, 0.8660254037844387076, 1.000000000000000000, 0.8660254037844387076, 1.000000000000000000, 0.8660254037844387076, 1.000000000000000000, 0.8660254037844387076, 1.000000000000000000, 0.8660254037844387076, 1.000000000000000000, 0.8660254037844387076, 1.000000000000000000, 0.8660254037844387076, 1.000000000000000000, 0.8660254037844387076, 1.000000000000000000, 0.8660254037844387076, 1.000000000000000000, 0.8660254037844387076, 1.000000000000000000, 0.8660254037844387076, 1.000000000000000000, 0.8660254037844387076, 1.000000000000000000, 0.8660254037844387076, 1.000000000000000000, 0.8660254037844387076, 1.000000000000000000, 0.8660254037844387076, 1.000000000000000000, 0.8660254037844387076, 1.000000000000000000, 0.8660254037844387076, 1.000000000000000000, 0.8660254037844387076, 1.000000000000000000, 0.8660254037844387076, 1.000000000000000000, 0.8660254037844387076, 1.000000000000000000, 0.8660254037844387076, 1.000000000000000000, 0.8660254037844387076, 1.000000000000000000, 0.8660254037844387076, 1.000000000000000000, 0.8660254037844387076, 1.000000000000000000, 0.8660254037844387076, 1.000000000000000000, 0.8660254037844387076, 1.000000000000000000, 0.8660254037844387076, 1.000000000000000000, 0.8660254037844387076, 1.000000000000000000, 0.8660254037844387076, 1.000000000000000000, 0.8660254037844387076, 1.000000000000000000, 0.8660254037844387076, 1.000000000000000000, 0.8660254037844387076, 1.000000000000000000, 0.8660254037844387076, 1.000000000000000000, 0.8660254037844387076, 1.000000000000000000, 0.8660254037844387076, 1.000000000000000000, 0.8660254037844387076, 1.000000000000000000, 0.8660254037844387076, 1.000000000000000000, 0.8660254037844387076, 1.000000000000000000, 0.8660254037844387076, 1.000000000000000000, 0.8660254037844387076, 1.000000000000000000, 0.8660254037844387076, 1.000000000000000000, 0.8660254037844387076, 1.000000000000000000, 0.8660254037844387076, 1.000000000000000000, 0.8660254037844387076, 1.000000000000000000, 0.8660254037844387076, 1.000000000000000000, 0.8660254037844387076, 1.000000000000000000, 0.8660254037844387076, 1.000000000000000000, 0.8660254037844387076, 1.000000000000000000, 0.8660254037844387076, 1.000000000000000000, 0.8660254037844387076, 1.000000000000000000, 0.8660254037844387076, 1.000000000000000000, 0.8660254037844387076, 1.000000000000000000, 0.8660254037844387076, 1.000000000000000000, 0.8660254037844387076, 1.000000000000000000, 0.8660254037844387076, 1.000000000000000000, 0.8660254037844387076, 1.000000000000000000, 0.8660254037844387076, 1.000000000000000000, 0.8660254037844387076, 1.000000000000000000, 0.8660254037844387076, 1.000000000000000000, 0.8660254037844387076, 1.000000000000000000, 0.8660254037844387076, 1.000000000000000000, 0.8660254037844387076, 1.000000000000000000, 0.8660254037844387076, 1.000000000000000000, 0.8660254037844387076, 1.000000000000000000, 0.8660254037844387076, 1.000000000000000000, 0.8660254037844387076, 1.000000000000000000, 0.8660254037844387076, 1.000000000000000000) ) ) 
 REPRESENTATION_ITEM ( '' )  SURFACE ( )  );
#41058 = AXIS2_PLACEMENT_3D ( 'NONE', #199024, #183865, #100485 ) ;
#41059 = CARTESIAN_POINT ( 'NONE',  ( 4.981731378017507872, 7.899438143407371271, -1.199719254218452047 ) ) ;
#41060 = CARTESIAN_POINT ( 'NONE',  ( -1.360316468750011332, 2.421875000341397577, -1.387778780781445676E-14 ) ) ;
#41061 = CARTESIAN_POINT ( 'NONE',  ( 0.9999999999999833467, 8.600000000000013856, -0.3999999999999832023 ) ) ;
#41062 = CARTESIAN_POINT ( 'NONE',  ( 10.54788032175191326, 11.40820791823982994, 0.7216878364870317197 ) ) ;
#41063 = EDGE_LOOP ( 'NONE', ( #51662, #140408, #190802, #202507, #208213 ) ) ;
#41064 = CARTESIAN_POINT ( 'NONE',  ( -5.250750630242457362, 9.347902511916677426, 0.000000000000000000 ) ) ;
#41065 = CARTESIAN_POINT ( 'NONE',  ( 5.519157712072518152, -1.821736412749059397, 0.8647389720048551665 ) ) ;
#41066 = CARTESIAN_POINT ( 'NONE',  ( -1.858365260435290220E-15, -9.595263517168275413, -9.591985693222424558 ) ) ;
#41067 = CARTESIAN_POINT ( 'NONE',  ( -7.487360338304386964, -6.465328379374276402, 7.487360338304412721 ) ) ;
#41068 = AXIS2_PLACEMENT_3D ( 'NONE', #202249, #6187, #167644 ) ;
#41069 = CARTESIAN_POINT ( 'NONE',  ( -6.496151039430258400, 6.761311432142845135, -0.1280508955800782056 ) ) ;
#41070 = CARTESIAN_POINT ( 'NONE',  ( -5.314433026876900001, 6.262888621853549331, 1.082531754730548412 ) ) ;
#41071 = CARTESIAN_POINT ( 'NONE',  ( 4.546061579283848353, 4.198160018786257552, -0.7998128361456211532 ) ) ;
#41072 = CARTESIAN_POINT ( 'NONE',  ( 2.430458318764291192, -1.215629356985904685, 1.549377053225237111 ) ) ;
#41073 = CARTESIAN_POINT ( 'NONE',  ( 4.868767636308747093, -0.2496254991312534810, -2.000855965115163837 ) ) ;
#41074 = CARTESIAN_POINT ( 'NONE',  ( -6.181627972826976958, 9.299317504018391745, 1.199719254218452047 ) ) ;
#41075 = CARTESIAN_POINT ( 'NONE',  ( 6.827182134110196365, 7.629137130509086262, 2.689055895399253160 ) ) ;
#41076 = CARTESIAN_POINT ( 'NONE',  ( 4.734432829848630675, 0.3728853646711489112, 2.159338447334692823 ) ) ;
#41077 = CARTESIAN_POINT ( 'NONE',  ( 4.572363442555127833, 8.499999999999996447, 0.3169179603640607246 ) ) ;
#41078 = CARTESIAN_POINT ( 'NONE',  ( 3.100521554045695627, -0.5575540177290801980, -1.843951249938739378 ) ) ;
#41079 = CARTESIAN_POINT ( 'NONE',  ( -7.486073373039941359, 11.88550270185529278, -0.7998128361456291469 ) ) ;
#41080 =( NAMED_UNIT ( * ) PLANE_ANGLE_UNIT ( ) SI_UNIT ( $, .RADIAN. ) );
#41081 = CARTESIAN_POINT ( 'NONE',  ( 0.2060869173217265982, -0.5842117877600698783, 2.128085570573131413 ) ) ;
#41082 = CARTESIAN_POINT ( 'NONE',  ( 0.1753634416057497925, 0.0001173177735149660839, -2.144164757042037017 ) ) ;
#41084 = ADVANCED_FACE ( 'NONE', ( #21760 ), #108145, .T. ) ;
#41083 = CARTESIAN_POINT ( 'NONE',  ( -1.796836089791512103, 14.48004991555888310, 11.89866442307391736 ) ) ;
#41085 = CARTESIAN_POINT ( 'NONE',  ( 5.986088515633498197, 6.942523675449257858, -1.199719254218446718 ) ) ;
#41086 = DIRECTION ( 'NONE',  ( 0.000000000000000000, -1.000000000000000000, 0.000000000000000000 ) ) ;
#41087 = CARTESIAN_POINT ( 'NONE',  ( 5.397554552016228691, 5.469770863539975991, 0.7216878364870328300 ) ) ;
#41089 = CARTESIAN_POINT ( 'NONE',  ( 2.438141639825658125, -1.160823251276057011, -1.644512180470799834 ) ) ;
#41088 = CARTESIAN_POINT ( 'NONE',  ( 6.128435733830499998, 0.1874100934057248424, 1.831705376836203936 ) ) ;
#41090 = CARTESIAN_POINT ( 'NONE',  ( 4.833568131691490244, -1.505864581002622105, 1.736428821378619647 ) ) ;
#41092 = CARTESIAN_POINT ( 'NONE',  ( 3.502650316321722634, 0.4479755722775873861, 1.806107967122023927 ) ) ;
#41091 = CARTESIAN_POINT ( 'NONE',  ( -6.474900878978163021, 9.711745571186627402, -1.199719254218452047 ) ) ;
#41093 = CARTESIAN_POINT ( 'NONE',  ( 6.393551957296131683, 9.616838495890963401, 1.199719254218452047 ) ) ;
#41094 = CARTESIAN_POINT ( 'NONE',  ( 11.96217875511318063, 11.32854366578976446, -0.9561995067075083066 ) ) ;
#41095 = CARTESIAN_POINT ( 'NONE',  ( -6.398558430645608475, 9.552403038140164782, -1.199719254218440723 ) ) ;
#41096 = CARTESIAN_POINT ( 'NONE',  ( -5.804299160426249493, 5.944306240018289778, -0.7216878364870338292 ) ) ;
#41098 = CARTESIAN_POINT ( 'NONE',  ( 6.110894567773135222, -0.2550301881006194482, 2.075043241552937179 ) ) ;
#41097 = B_SPLINE_CURVE_WITH_KNOTS ( 'NONE', 3,
 ( #197291, #148562, #35855, #32664, #69405, #17455, #83540, #181048 ),
 .UNSPECIFIED., .F., .F.,
 ( 4, 2, 2, 4 ),
 ( 2.544396950729599234E-07, 0.0002984430161323445535, 0.0005966315925696161248, 0.001193008745444159267 ),
 .UNSPECIFIED. ) ;
#41099 = CARTESIAN_POINT ( 'NONE',  ( 6.507550544879468823, 6.694489845221929691, -0.7216878364870257245 ) ) ;
#41100 = VERTEX_POINT ( 'NONE', #87262 ) ;
#41101 = AXIS2_PLACEMENT_3D ( 'NONE', #83534, #149616, #67261 ) ;
#41102 = DIRECTION ( 'NONE',  ( 0.7592566023652993490, 0.6507913734559652719, -8.881784197001246407E-16 ) ) ;
#41104 = CARTESIAN_POINT ( 'NONE',  ( 4.273844736805816780, 6.009238164405336313, 1.599625672291267398 ) ) ;
#41103 = FACE_OUTER_BOUND ( 'NONE', #97157, .T. ) ;
#41105 = CARTESIAN_POINT ( 'NONE',  ( 6.076716319674939193, -1.640139352550730401, -0.5342243915677049593 ) ) ;
#41106 = CARTESIAN_POINT ( 'NONE',  ( -4.954615070790188369, 7.867802451642154082, -1.199719254218452047 ) ) ;
#41107 = CARTESIAN_POINT ( 'NONE',  ( 0.8965906023701503136, -0.7780376274850349105, -1.549907966113317270 ) ) ;
#41108 = CARTESIAN_POINT ( 'NONE',  ( -5.926322542504877333, 7.047036066744706950, -1.082531754730549967 ) ) ;
#41109 = CARTESIAN_POINT ( 'NONE',  ( -1.499999999999997780, 5.431250000682820378, 1.214306433183764966E-14 ) ) ;
#41110 = DIRECTION ( 'NONE',  ( -1.000000000000000000, -0.000000000000000000, -0.000000000000000000 ) ) ;
#41111 = CARTESIAN_POINT ( 'NONE',  ( 5.823135961761455981, -1.959396665126054815, -0.9353919727212963720 ) ) ;
#41112 = CARTESIAN_POINT ( 'NONE',  ( 4.688025921862073453, -0.8580590012943272171, 1.611482198803436905 ) ) ;
#41113 = CARTESIAN_POINT ( 'NONE',  ( 2.465611527742004760, -0.4346729355233552861, 1.912824223707191296 ) ) ;
#41114 = CARTESIAN_POINT ( 'NONE',  ( 9.561191386655707447, -9.006862915010142245, -0.6000160562356342542 ) ) ;
#41115 = CARTESIAN_POINT ( 'NONE',  ( 6.511106444361020706, 5.279176164185798825, 2.500000000000011546 ) ) ;
#41116 = CARTESIAN_POINT ( 'NONE',  ( 6.588372581236919601, 9.773852880496709972, -1.199719254218440723 ) ) ;
#41117 = CARTESIAN_POINT ( 'NONE',  ( 3.246849895443252532, 2.069243461727567013, 0.4626693848822636124 ) ) ;
#41118 = CARTESIAN_POINT ( 'NONE',  ( 0.000000000000000000, 13.49999999999999822, -1.500000000000000222 ) ) ;
#41119 = DIRECTION ( 'NONE',  ( 0.000000000000000000, 0.000000000000000000, -1.000000000000000000 ) ) ;
#41120 = CARTESIAN_POINT ( 'NONE',  ( -5.343048727742272241, 6.363526295613923800, -1.106837213068444292 ) ) ;
#41121 = CARTESIAN_POINT ( 'NONE',  ( 1.692325190600419305, 1.023896122633965566, -1.799289093316607469 ) ) ;
#41123 = CARTESIAN_POINT ( 'NONE',  ( 1.500000000000001332, 14.90625000068279604, 0.000000000000000000 ) ) ;
#41122 = CARTESIAN_POINT ( 'NONE',  ( -9.604686356149274573, 3.481540744127370690, 7.193747284969077782 ) ) ;
#41125 = EDGE_LOOP ( 'NONE', ( #107040, #189646, #8415, #127939, #195716, #131393 ) ) ;
#41124 = CARTESIAN_POINT ( 'NONE',  ( 3.598459204466686323, -1.093923138158871433, 1.933176262723006467 ) ) ;
#41126 = CARTESIAN_POINT ( 'NONE',  ( 1.354533853113936814, 0.1633331948888619711, -2.292934881128176450 ) ) ;
#41128 = CARTESIAN_POINT ( 'NONE',  ( 6.860222192644392258, -2.062229998417430377, 0.04471529749722201463 ) ) ;
#41127 = CARTESIAN_POINT ( 'NONE',  ( 10.22248463502393001, 11.02857961705718282, 0.7216878364870438212 ) ) ;
#41130 = CARTESIAN_POINT ( 'NONE',  ( 1.737499999999999378, -0.4666666666666673402, -3.009438278150925683 ) ) ;
#41129 = CARTESIAN_POINT ( 'NONE',  ( 5.174371902270911150, 6.065797303184739420, 1.199719254218452047 ) ) ;
#41131 = B_SPLINE_CURVE_WITH_KNOTS ( 'NONE', 3,
 ( #99685, #114932, #213412, #2145 ),
 .UNSPECIFIED., .F., .F.,
 ( 4, 4 ),
 ( 0.007151640131792815283, 0.007705906178639654498 ),
 .UNSPECIFIED. ) ;
#41132 = EDGE_CURVE ( 'NONE', #144059, #156928, #153629, .T. ) ;
#41133 = DIRECTION ( 'NONE',  ( 1.000000000000000000, 0.000000000000000000, 0.000000000000000000 ) ) ;
#41134 = LINE ( 'NONE', #90945, #168764 ) ;
#41135 = FILL_AREA_STYLE ('',( #75743 ) ) ;
#41136 = CARTESIAN_POINT ( 'NONE',  ( -0.1102773484824119410, 4.081664357266182819, -2.758211214536327116 ) ) ;
#41137 = CARTESIAN_POINT ( 'NONE',  ( 3.451896303776471608, 1.724958192144626867, 0.0007732285732166971348 ) ) ;
#41138 = CARTESIAN_POINT ( 'NONE',  ( 2.606657977298726614, 1.900416011228076130, 0.6748465934659984011 ) ) ;
#41139 = CARTESIAN_POINT ( 'NONE',  ( 2.532212319380182208, -1.909192193906615209, 1.279991936841210043 ) ) ;
#41140 = CARTESIAN_POINT ( 'NONE',  ( 3.673342012549928981, 0.05998355446043589223, -2.261782774625902714 ) ) ;
#41141 = CARTESIAN_POINT ( 'NONE',  ( 5.461587592249073531, 0.4120570304669196604, -2.065184316587692415 ) ) ;
#41142 = CARTESIAN_POINT ( 'NONE',  ( -7.458393901293492334, 7.874083437696761223, 0.7216878364870317197 ) ) ;
#41143 = CARTESIAN_POINT ( 'NONE',  ( 4.006921011573481906, 1.516870794648169873, 0.9113941657561406284 ) ) ;
#41144 = EDGE_CURVE ( 'NONE', #127784, #140828, #29007, .T. ) ;
#41146 = CARTESIAN_POINT ( 'NONE',  ( 0.2348727637096776621, 0.3982709639365061838, 2.257261336973298338 ) ) ;
#41145 = CARTESIAN_POINT ( 'NONE',  ( 6.770317605177710085, 8.992066187497757213, 1.599625672291268286 ) ) ;
#41147 = CARTESIAN_POINT ( 'NONE',  ( 6.017501326166345699, -1.026660802952833240, -1.528114487065170390 ) ) ;
#41148 = CARTESIAN_POINT ( 'NONE',  ( -3.113568832632681360, 6.784247404713427798, -0.7998128361456281477 ) ) ;
#41149 = AXIS2_PLACEMENT_3D ( 'NONE', #200524, #52170, #3387 ) ;
#41150 = CARTESIAN_POINT ( 'NONE',  ( 5.560537033210596114, -1.979929515673630513, -0.9395970221138388867 ) ) ;
#41151 = CARTESIAN_POINT ( 'NONE',  ( -2.774614992291035698, 6.388801257648172971, 1.040834085586084257E-14 ) ) ;
#41152 = CARTESIAN_POINT ( 'NONE',  ( -1.741635578173613697, 15.44819650159847235, 11.86206419467665185 ) ) ;
#41153 = CARTESIAN_POINT ( 'NONE',  ( 5.687960312649480876, -1.310561514506687564, -1.602779375087557412 ) ) ;
#41154 = CARTESIAN_POINT ( 'NONE',  ( 0.5675926644314840397, 1.357872185771633156, 1.490966652548594285 ) ) ;
#41155 = CARTESIAN_POINT ( 'NONE',  ( 1.499999999999985123, -0.9229166659838452524, -0.8660254037844323793 ) ) ;
#41156 = CARTESIAN_POINT ( 'NONE',  ( 3.809137074456845795, 1.652770800469059775, 0.9896037298236616264 ) ) ;
#41157 = CARTESIAN_POINT ( 'NONE',  ( -1.364683531250000748, 10.60937500034139802, 0.000000000000000000 ) ) ;
#41158 = CARTESIAN_POINT ( 'NONE',  ( -2.155383234892699562, 5.458438174109348395, 1.040834085586084257E-14 ) ) ;
#41159 = CARTESIAN_POINT ( 'NONE',  ( 6.328397690248316110, -1.000878058022572903, -1.869571840794107986 ) ) ;
#41161 = EDGE_LOOP ( 'NONE', ( #72180, #135788, #186607, #128139 ) ) ;
#41160 = CARTESIAN_POINT ( 'NONE',  ( 5.063044020060520900, 4.871582543017558109, 0.7998128361456352531 ) ) ;
#41162 = CARTESIAN_POINT ( 'NONE',  ( -4.340018570150318666, 6.156717313299049366, -1.443375672974066548 ) ) ;
#41163 = CARTESIAN_POINT ( 'NONE',  ( 8.543609354905870035, 13.11929468069890525, 0.7998128361456462443 ) ) ;
#41164 = DIRECTION ( 'NONE',  ( 1.000000000000000000, 0.000000000000000000, 0.000000000000000000 ) ) ;
#41165 = CARTESIAN_POINT ( 'NONE',  ( -11.01135777277262306, 10.09367418006288197, 1.399999999999998579 ) ) ;
#41166 = AXIS2_PLACEMENT_3D ( 'NONE', #59649, #28221, #124743 ) ;
#41167 = CARTESIAN_POINT ( 'NONE',  ( 11.09299181971603510, 9.057582982347017975, -4.454713115659062694 ) ) ;
#41168 = CARTESIAN_POINT ( 'NONE',  ( -1.499999999999964029, 7.750000000000000000, 10.64483442802189117 ) ) ;
#41169 = CARTESIAN_POINT ( 'NONE',  ( 1.047228354049560828, 1.731870006261830408, -0.9216698261682305660 ) ) ;
#41170 = CARTESIAN_POINT ( 'NONE',  ( 1.364683531249988757, 0.6968750003414209138, 0.000000000000000000 ) ) ;
#41171 = EDGE_CURVE ( 'NONE', #187973, #153164, #52625, .T. ) ;
#41172 = LINE ( 'NONE', #58467, #12737 ) ;
#41173 = CARTESIAN_POINT ( 'NONE',  ( 5.529730448059603454, 1.891198321494348633, -0.5216162335564683561 ) ) ;
#41174 = CARTESIAN_POINT ( 'NONE',  ( -6.997979842947967377, 11.31606025008131233, -0.7998128361456291469 ) ) ;
#41175 = EDGE_CURVE ( 'NONE', #205126, #206199, #86194, .T. ) ;
#41176 = CARTESIAN_POINT ( 'NONE',  ( -6.371969008298464132, 6.536311385877402458, 1.040834085586084257E-14 ) ) ;
#41177 = CARTESIAN_POINT ( 'NONE',  ( 6.561405286136595905, 0.3748316153167965403, -2.128808860954830795 ) ) ;
#41179 = EDGE_LOOP ( 'NONE', ( #96764, #54625, #15237, #158376, #197281 ) ) ;
#41178 = CARTESIAN_POINT ( 'NONE',  ( -5.585069213825653023, 8.603332285183535433, -1.199719254218440723 ) ) ;
#41180 = CARTESIAN_POINT ( 'NONE',  ( 1.364683531249988535, 5.405208333674750953, -0.7879004041258300672 ) ) ;
#41181 = CARTESIAN_POINT ( 'NONE',  ( 1.879943753831798015, -1.004885234286160722, 1.577526331995420472 ) ) ;
#41182 = CARTESIAN_POINT ( 'NONE',  ( 0.1583034150156861219, 0.9959709328331721734, 1.419360398433693549 ) ) ;
#41184 = CARTESIAN_POINT ( 'NONE',  ( 3.878626735558046157, -0.2160506499642600997, -2.180900317982924275 ) ) ;
#41183 = CARTESIAN_POINT ( 'NONE',  ( 0.6801582343749883464, 2.473958333674766585, 1.178068619123824323 ) ) ;
#41185 = CARTESIAN_POINT ( 'NONE',  ( 4.647712500454345808, -1.780663920513593013, -1.467712336591691313 ) ) ;
#41186 = CARTESIAN_POINT ( 'NONE',  ( 6.872340646960426902, -1.271554428311357565, 1.622191329735128029 ) ) ;
#41187 = CARTESIAN_POINT ( 'NONE',  ( 2.695178803863579997, -0.6086341500050916897, 1.844178105057793893 ) ) ;
#41188 = CARTESIAN_POINT ( 'NONE',  ( -5.599154252319524794, 6.595063384869953360, 1.082531754730546636 ) ) ;
#41189 = SURFACE_SIDE_STYLE ('',( #6507 ) ) ;
#41190 = CARTESIAN_POINT ( 'NONE',  ( 5.291314375706784645, -0.05428322906628547939, -2.120082430678168706 ) ) ;
#41191 = CARTESIAN_POINT ( 'NONE',  ( 0.3282377607281215526, 2.926335450315382225, -1.225000000000001421 ) ) ;
#41192 = CARTESIAN_POINT ( 'NONE',  ( 3.604138833494671346, -0.1455340571130462057, 2.011204217620660817 ) ) ;
#41193 = CARTESIAN_POINT ( 'NONE',  ( -5.734735788456164940, 5.792872629394710593, 0.7216878364870317197 ) ) ;
#41194 = CARTESIAN_POINT ( 'NONE',  ( -6.095272577795516789, 9.268845886473535245, 1.199719254218452047 ) ) ;
#41195 = CARTESIAN_POINT ( 'NONE',  ( 10.39640486358069360, 11.02356051713265650, 0.7998128361456462443 ) ) ;
#41196 = CARTESIAN_POINT ( 'NONE',  ( 1.347985785199314668, 1.823511463271022093, 0.09156768404049858701 ) ) ;
#41197 = CARTESIAN_POINT ( 'NONE',  ( -4.749098946536820520, 8.762642214260091933, 0.7998128361456281477 ) ) ;
#41198 = CARTESIAN_POINT ( 'NONE',  ( -0.02465203476893947088, 15.46327782766690007, 11.97749487451462613 ) ) ;
#41199 = CARTESIAN_POINT ( 'NONE',  ( -10.81012925547440773, 5.523932969818027949, 6.547168141744070802 ) ) ;
#41200 = ORIENTED_EDGE ( 'NONE', *, *, #166038, .T. ) ;
#41201 = CARTESIAN_POINT ( 'NONE',  ( 5.471578299931997513, 1.986755592664890324, -0.5475478416450995089 ) ) ;
#41202 = CARTESIAN_POINT ( 'NONE',  ( -6.034787771414192648, 9.094317262408276648, 1.082531754730549967 ) ) ;
#41203 = CARTESIAN_POINT ( 'NONE',  ( 5.029711800989886683, 4.970344644017389513, 1.040834085586084257E-14 ) ) ;
#41204 = CARTESIAN_POINT ( 'NONE',  ( -3.093231602212184850, 6.760520635889515795, -0.7998128361456281477 ) ) ;
#41205 = CARTESIAN_POINT ( 'NONE',  ( -4.329849954717889915, 6.144853928627882489, 1.599625672291270506 ) ) ;
#41206 = CARTESIAN_POINT ( 'NONE',  ( 4.442060220718175856, -1.244341337028841421, -1.590709041654225553 ) ) ;
#41207 = CARTESIAN_POINT ( 'NONE',  ( 5.250715360749964589, 2.188191852258320136, 0.3812115871067219275 ) ) ;
#41209 = CARTESIAN_POINT ( 'NONE',  ( 8.934460041725669655, 9.525884258209195821, 1.040834085586084257E-14 ) ) ;
#41208 = CARTESIAN_POINT ( 'NONE',  ( -7.075376061485238566, 9.347967719856493218, 1.599625672291269396 ) ) ;
#41210 = CARTESIAN_POINT ( 'NONE',  ( 7.169564303528210836, 7.258913197071374945, -0.7998128361456281477 ) ) ;
#41211 = CARTESIAN_POINT ( 'NONE',  ( 4.522374016017603360, 1.269557654445327532, -1.623317902228790910 ) ) ;
#41212 = CARTESIAN_POINT ( 'NONE',  ( 3.656875104409584853, 1.122498086849915921, 1.674887873639265390 ) ) ;
#41213 = EDGE_LOOP ( 'NONE', ( #161177, #163758, #28767, #79411, #78012 ) ) ;
#41214 = DIRECTION ( 'NONE',  ( 1.000000000000000000, -0.000000000000000000, -0.000000000000000000 ) ) ;
#41215 = CARTESIAN_POINT ( 'NONE',  ( 5.542585869888291938, 5.360771691158120689, -0.7998128361456211532 ) ) ;
#41216 = CIRCLE ( 'NONE', #34222, 0.2000000000000000944 ) ;
#41218 = VERTEX_POINT ( 'NONE', #53696 ) ;
#41217 = CARTESIAN_POINT ( 'NONE',  ( -5.745623237141265882, 9.925253886631958622, 0.7998128361456291469 ) ) ;
#41219 = CARTESIAN_POINT ( 'NONE',  ( 5.528015674651411970, 7.440572265265038787, -1.248273786418591103 ) ) ;
#41220 = EDGE_CURVE ( 'NONE', #100853, #203895, #185806, .T. ) ;
#41221 = CARTESIAN_POINT ( 'NONE',  ( 3.567732365556259833, 1.591074578583808075, -1.238131541301431549 ) ) ;
#41222 = CARTESIAN_POINT ( 'NONE',  ( 2.659893383946440260, -1.269561761542839617, 1.333649727802692198 ) ) ;
#41223 = CARTESIAN_POINT ( 'NONE',  ( 4.496171506534474283, 8.048216686630640382, 2.444650791391935307 ) ) ;
#41224 = CARTESIAN_POINT ( 'NONE',  ( 0.9269276575891262082, 1.370462819911044239, -1.856556161720348763 ) ) ;
#41225 = CARTESIAN_POINT ( 'NONE',  ( 2.898410978271408922, 6.603506251283770112, -0.7998128361456362523 ) ) ;
#41226 = CARTESIAN_POINT ( 'NONE',  ( 3.602937629199114866, 1.706465849011790104, -1.326752773236601346 ) ) ;
#41227 = CARTESIAN_POINT ( 'NONE',  ( 9.260382613333817403, 10.76253345609967660, -1.199719254218446718 ) ) ;
#41228 = CARTESIAN_POINT ( 'NONE',  ( -7.237355071596549116, 7.338002426484427687, 1.040834085586084257E-14 ) ) ;
#41229 = CARTESIAN_POINT ( 'NONE',  ( -0.002323312721275774470, -7.217450603046129842, -9.500350659417616583 ) ) ;
#41230 = CARTESIAN_POINT ( 'NONE',  ( 2.676452114398766291, -1.789519730395791486, -0.5449050523786898026 ) ) ;
#41231 = ORIENTED_EDGE ( 'NONE', *, *, #183348, .F. ) ;
#41232 = CARTESIAN_POINT ( 'NONE',  ( 5.647334207030327846, -1.553848685622709835, -1.213239188487026166 ) ) ;
#41234 = CARTESIAN_POINT ( 'NONE',  ( -6.237633190739009237, 9.434933268240943249, 1.199719254218452047 ) ) ;
#41233 = CARTESIAN_POINT ( 'NONE',  ( 1.364683531249988535, 4.113541667008088432, 0.7879004041258500513 ) ) ;
#41236 = CARTESIAN_POINT ( 'NONE',  ( 0.8212658843103730621, 2.040464674744349338, 0.8412164853940640175 ) ) ;
#41235 = CARTESIAN_POINT ( 'NONE',  ( -6.925517538482230506, 6.974191971184389160, 0.7998128361456341429 ) ) ;
#41237 = CARTESIAN_POINT ( 'NONE',  ( -1.492392680118208803, 7.408236896935049387, -4.235501437639352496 ) ) ;
#41238 = CARTESIAN_POINT ( 'NONE',  ( 5.691725559638619814, 5.534767995866836543, 1.040834085586084257E-14 ) ) ;
#41239 = CARTESIAN_POINT ( 'NONE',  ( -6.735703387890906946, 6.752742128827836865, -0.7998128361456291469 ) ) ;
#41240 = CARTESIAN_POINT ( 'NONE',  ( -7.967649405165836640, -5.251137252134745914, 7.547231044119360632 ) ) ;
#41241 = CARTESIAN_POINT ( 'NONE',  ( 6.578986288830292573, -0.09655258645749519031, -1.969210242046049331 ) ) ;
#41242 = CARTESIAN_POINT ( 'NONE',  ( 6.094374174207308315, -2.295927367373576722, -0.2327322904458818675 ) ) ;
#41243 = CARTESIAN_POINT ( 'NONE',  ( 6.602007162813277041, 0.7109360278478898953, -1.720114357745919476 ) ) ;
#41244 = CARTESIAN_POINT ( 'NONE',  ( 3.151292761600641867, 1.771340389172958441, -1.056411398746412544 ) ) ;
#41245 = CARTESIAN_POINT ( 'NONE',  ( 6.805829924380114804, 8.002851668940699881, 1.082531754730558626 ) ) ;
#41246 = CARTESIAN_POINT ( 'NONE',  ( 6.831329296439236032, 9.063246493969506545, -1.599625672291267398 ) ) ;
#41247 = CARTESIAN_POINT ( 'NONE',  ( 6.602457619730760285, 8.725953194484466380, 1.443375672974076540 ) ) ;
#41248 = CARTESIAN_POINT ( 'NONE',  ( -1.364683531250012516, 2.801041667008090652, -0.7879004041258289570 ) ) ;
#41249 = CARTESIAN_POINT ( 'NONE',  ( -6.714560252712822752, 14.48050415317768724, 9.956001885444296207 ) ) ;
#41250 = CARTESIAN_POINT ( 'NONE',  ( 5.639828713160493834, 5.682147708216442439, 1.040834085586084257E-14 ) ) ;
#41251 = CARTESIAN_POINT ( 'NONE',  ( 5.793482113768906316, -1.965262051535413335, 0.9231745368859373135 ) ) ;
#41253 = CARTESIAN_POINT ( 'NONE',  ( 5.671403949121008203, 1.101820082107987098, 1.475039313902235305 ) ) ;
#41252 = DIRECTION ( 'NONE',  ( -0.6249999999999992228, 1.210928637341016588E-14, -0.7806247497998003437 ) ) ;
#41255 = CARTESIAN_POINT ( 'NONE',  ( 6.620655732516679493, 2.454579131793722002, 2.310038015908893350 ) ) ;
#41254 = CARTESIAN_POINT ( 'NONE',  ( 10.99126615174920651, -5.166862915010145052, -0.4382560683119322009 ) ) ;
#41256 = CARTESIAN_POINT ( 'NONE',  ( 6.392125918040960642, -0.5824770489515176397, -2.112646119873210271 ) ) ;
#41257 = CARTESIAN_POINT ( 'NONE',  ( 9.579764304849151202, -9.919999999999998153, -0.06720017513373727214 ) ) ;
#41258 = CARTESIAN_POINT ( 'NONE',  ( 6.631690487938540102, -1.471565961622269381, -1.718669407966398666 ) ) ;
#41259 = CARTESIAN_POINT ( 'NONE',  ( -4.461457896923207933, 7.279594253155052819, -1.276495073192641883 ) ) ;
#41260 = FILL_AREA_STYLE_COLOUR ( '', #30656 ) ;
#41261 = CARTESIAN_POINT ( 'NONE',  ( 6.599791786788117953, 6.770233575417231364, 0.1470628079319712123 ) ) ;
#41262 = VECTOR ( 'NONE', #26290, 1000.000000000000000 ) ;
#41263 = CARTESIAN_POINT ( 'NONE',  ( -4.082413651046300274, 6.816547455312373494, 1.082531754730549967 ) ) ;
#41264 = CARTESIAN_POINT ( 'NONE',  ( 0.1703706300211875746, 0.7318840393725855042, 1.766877091004593225 ) ) ;
#41265 = CARTESIAN_POINT ( 'NONE',  ( 1.850134630017237880, 0.5516246727584225296, 1.681758779177483287 ) ) ;
#41266 = EDGE_CURVE ( 'NONE', #56668, #118760, #61858, .T. ) ;
#41267 = CARTESIAN_POINT ( 'NONE',  ( 6.006499477249034769, -2.003593090125683762, -0.1951834861853833925 ) ) ;
#41268 = CARTESIAN_POINT ( 'NONE',  ( 5.122148429244435697, -1.124054950784241891, -1.780691527792167994 ) ) ;
#41270 = CARTESIAN_POINT ( 'NONE',  ( 3.216317514422084578, 1.869562491224942224, 0.4167181705077570575 ) ) ;
#41269 = CARTESIAN_POINT ( 'NONE',  ( -3.267151830768952880, 5.795132321663641228, -1.082531754730549078 ) ) ;
#41271 = CARTESIAN_POINT ( 'NONE',  ( -0.02244404828157658613, -0.004869073801674199918, -2.189079685368473527 ) ) ;
#41272 = CARTESIAN_POINT ( 'NONE',  ( 4.703538277703087189, -1.521029056438701232, -1.251204274914043957 ) ) ;
#41273 = CARTESIAN_POINT ( 'NONE',  ( -0.1929003719821283658, -0.4722129235960635940, -2.074948700427194481 ) ) ;
#41274 = CARTESIAN_POINT ( 'NONE',  ( -2.435661151949389147, 5.993355110582911038, 0.7998128361456341429 ) ) ;
#41275 = CARTESIAN_POINT ( 'NONE',  ( 2.922558825391399662, 1.760836971185793187, 0.6318509464167121337 ) ) ;
#41277 = VERTEX_POINT ( 'NONE', #24368 ) ;
#41276 = CARTESIAN_POINT ( 'NONE',  ( 5.690025311828595278, -0.7696446287084879323, 1.543740960907719950 ) ) ;
#41279 = CARTESIAN_POINT ( 'NONE',  ( 4.121315508874254796, 5.831287398485176077, -1.443375672974051449 ) ) ;
#41278 = CARTESIAN_POINT ( 'NONE',  ( 2.209865124170300898, -0.4819264253047173541, 2.153463223375853719 ) ) ;
#41280 = EDGE_CURVE ( 'NONE', #205506, #154674, #48064, .T. ) ;
#41281 = CARTESIAN_POINT ( 'NONE',  ( 1.364683531249990311, 3.946875000341417028, 1.214306433183764966E-14 ) ) ;
#41282 = CARTESIAN_POINT ( 'NONE',  ( 6.074655751228532630, 1.318658252384183438, -1.452748870126779890 ) ) ;
#41284 = AXIS2_PLACEMENT_3D ( 'NONE', #100931, #128471, #18612 ) ;
#41283 = CARTESIAN_POINT ( 'NONE',  ( 6.252281394196331554, 10.44607872653774372, 1.040834085586084257E-14 ) ) ;
#41285 = CARTESIAN_POINT ( 'NONE',  ( 0.000000000000000000, -6.527411821100059797, 0.000000000000000000 ) ) ;
#41286 = CARTESIAN_POINT ( 'NONE',  ( 0.000000000000000000, 0.4330127018922214077, 0.000000000000000000 ) ) ;
#41287 = CARTESIAN_POINT ( 'NONE',  ( -3.554208825076827782, 7.298327395898266623, 0.7998128361456341429 ) ) ;
#41288 = DIRECTION ( 'NONE',  ( 1.000000000000000000, -0.000000000000000000, 1.224646799147353207E-16 ) ) ;
#41289 = VERTEX_POINT ( 'NONE', #105678 ) ;
#41290 = CARTESIAN_POINT ( 'NONE',  ( 1.627480586986803868, 0.1543294891723171747, -2.064685722993148342 ) ) ;
#41291 = CARTESIAN_POINT ( 'NONE',  ( 0.7499999999999902300, 2.983333333333351600, 1.299038105676669330 ) ) ;
#41292 = CARTESIAN_POINT ( 'NONE',  ( 5.657830175604453338, 5.495223381160312393, 0.7998128361456341429 ) ) ;
#41293 = CARTESIAN_POINT ( 'NONE',  ( 8.014278199453778839, 8.522615118883788199, 0.000000000000000000 ) ) ;
#41294 = CARTESIAN_POINT ( 'NONE',  ( 0.01237536129615121258, -2.019283296508204817, -0.04721428876065454638 ) ) ;
#41295 = CARTESIAN_POINT ( 'NONE',  ( -0.4330238300980990274, -6.527411821100045586, -9.549638505170015890 ) ) ;
#41296 = CARTESIAN_POINT ( 'NONE',  ( -1.364683531249997417, 4.009375000341424133, 1.214306433183764966E-14 ) ) ;
#41297 = ORIENTED_EDGE ( 'NONE', *, *, #193885, .F. ) ;
#41299 = CARTESIAN_POINT ( 'NONE',  ( 9.246297574839980271, 10.85006392781057905, 1.082531754730549967 ) ) ;
#41298 = CARTESIAN_POINT ( 'NONE',  ( -11.41381675112453387, 10.90000000000000036, -3.704697986577184299 ) ) ;
#41300 = CARTESIAN_POINT ( 'NONE',  ( 5.624374986212743011, 0.3960386850128463920, -1.976653645673176474 ) ) ;
#41301 = CARTESIAN_POINT ( 'NONE',  ( 5.260912935490944520, -0.05370519216219872549, -1.915158585242337397 ) ) ;
#41302 = CARTESIAN_POINT ( 'NONE',  ( 6.539320575229230492, 2.428701779328062749, 2.485127258459709054 ) ) ;
#41303 = CARTESIAN_POINT ( 'NONE',  ( 2.982162443640325122, -2.159563097825706990, -0.3721831821169723220 ) ) ;
#41304 = CARTESIAN_POINT ( 'NONE',  ( 0.7499999999999885647, 2.597916667349486897, -1.299038105676658228 ) ) ;
#41305 = CARTESIAN_POINT ( 'NONE',  ( 1.898553772666348394, -1.876154101037771582, -0.3696338911259658411 ) ) ;
#41306 = CARTESIAN_POINT ( 'NONE',  ( -4.394814349124112951, 8.279033840620114049, -0.7998128361456281477 ) ) ;
#41308 = CARTESIAN_POINT ( 'NONE',  ( -0.03552856956758054796, -1.956598898622825766, -0.4871759670460884539 ) ) ;
#41307 = CARTESIAN_POINT ( 'NONE',  ( 6.825078400183526739, -0.0002198122173603066763, 1.955566246027613753 ) ) ;
#41309 = CARTESIAN_POINT ( 'NONE',  ( -0.6823417656250003738, 9.963541667008065872, 1.181850606188754593 ) ) ;
#41310 = CIRCLE ( 'NONE', #51655, 0.07999999999999982125 ) ;
#41312 = CARTESIAN_POINT ( 'NONE',  ( -4.471156797456668386, 8.438376373666578445, -0.7998128361456362523 ) ) ;
#41311 = CARTESIAN_POINT ( 'NONE',  ( 6.269083535738129598, 2.097726667780253074, -0.6343229546324488100 ) ) ;
#41314 = EDGE_LOOP ( 'NONE', ( #191409, #50507, #123813, #154683, #116305 ) ) ;
#41313 = CARTESIAN_POINT ( 'NONE',  ( 2.836578922267366742, 0.2088710044844780678, 1.711989638784001677 ) ) ;
#41315 = CARTESIAN_POINT ( 'NONE',  ( 5.871359616481898414, -1.819694913365289768, -1.088597390283413402 ) ) ;
#41316 = CARTESIAN_POINT ( 'NONE',  ( 3.662674053986138656, 7.424870162959149589, 0.7998128361456321445 ) ) ;
#41317 = CYLINDRICAL_SURFACE ( 'NONE', #95241, 2.000000000000000000 ) ;
#41318 = CARTESIAN_POINT ( 'NONE',  ( 4.496500501226593727, 8.397667684739696270, 0.7998128361456462443 ) ) ;
#41319 = CARTESIAN_POINT ( 'NONE',  ( 2.033424464989775249, 3.426985321572571852, -11.42673966862522583 ) ) ;
#41320 = ORIENTED_EDGE ( 'NONE', *, *, #164628, .T. ) ;
#41321 = DIRECTION ( 'NONE',  ( 0.000000000000000000, 1.000000000000000000, 0.000000000000000000 ) ) ;
#41322 = ORIENTED_EDGE ( 'NONE', *, *, #201896, .T. ) ;
#41323 = CARTESIAN_POINT ( 'NONE',  ( 3.017991377792153429, -1.809312282836759378, 0.09115427604276456208 ) ) ;
#41324 = ORIENTED_EDGE ( 'NONE', *, *, #166876, .T. ) ;
#41325 = CARTESIAN_POINT ( 'NONE',  ( 8.378048858240820351, 11.86180853700128601, -1.199719254218446718 ) ) ;
#41326 = CARTESIAN_POINT ( 'NONE',  ( 3.898851692381625877, 6.706354853490643642, -1.199719254218452047 ) ) ;
#41327 = CARTESIAN_POINT ( 'NONE',  ( 3.352039220170324185, 0.8117645143102337757, -1.619458714540458866 ) ) ;
#41328 = CARTESIAN_POINT ( 'NONE',  ( 7.960045584554727327, 8.459343734834927631, 0.7216878364870267237 ) ) ;
#41329 =( GEOMETRIC_REPRESENTATION_CONTEXT ( 3 ) GLOBAL_UNCERTAINTY_ASSIGNED_CONTEXT ( ( #19012 ) ) GLOBAL_UNIT_ASSIGNED_CONTEXT ( ( #20529, #120253, #138574 ) ) REPRESENTATION_CONTEXT ( 'NONE', 'WORKASPACE' ) );
#41330 = CARTESIAN_POINT ( 'NONE',  ( -10.99440753328290121, -7.824706741106413510, 0.3572413387872626633 ) ) ;
#41331 = CARTESIAN_POINT ( 'NONE',  ( 5.838973523318124137, 6.009393772954500612, 0.3882124113597507087 ) ) ;
#41332 = ORIENTED_EDGE ( 'NONE', *, *, #204060, .T. ) ;
#41333 = CIRCLE ( 'NONE', #131353, 11.49999999999998934 ) ;
#41335 = CARTESIAN_POINT ( 'NONE',  ( 0.6823417656249969321, 14.02604166700806232, -1.181850606188757036 ) ) ;
#41334 = CARTESIAN_POINT ( 'NONE',  ( 4.721077684499490168, -1.662108436276054091, -0.8373904101051653504 ) ) ;
#41336 = CARTESIAN_POINT ( 'NONE',  ( 2.847180372343278254, 0.2781937080071684720, -1.895151957576347579 ) ) ;
#41337 = CARTESIAN_POINT ( 'NONE',  ( 1.237009950130557812, -1.652246606862219025, 0.7767072072360350354 ) ) ;
#41338 = CARTESIAN_POINT ( 'NONE',  ( -10.78227258717170578, 6.269840026405313793, 4.500979083849748541 ) ) ;
#41339 = CARTESIAN_POINT ( 'NONE',  ( 5.176795123377851304, 7.746134302493202561, 1.185296789734613387 ) ) ;
#41340 = CARTESIAN_POINT ( 'NONE',  ( 6.277139874739040337, -0.02379966007286238305, 9.660711923649619224E-16 ) ) ;
#41341 = CARTESIAN_POINT ( 'NONE',  ( -10.99946651476068560, -9.910601012391426323, 0.1083346235443097966 ) ) ;
#41342 = DIRECTION ( 'NONE',  ( 0.000000000000000000, 0.000000000000000000, 1.000000000000000000 ) ) ;
#41343 = CARTESIAN_POINT ( 'NONE',  ( 7.646435448427411963, 8.023188899361205273, -0.7216878364870257245 ) ) ;
#41344 = CARTESIAN_POINT ( 'NONE',  ( 5.594576842560746499, 1.939643975919752572, 0.3403973628498639936 ) ) ;
#41345 = CARTESIAN_POINT ( 'NONE',  ( 2.536342520008515233, 0.6839386381054488595, 1.897109991223707937 ) ) ;
#41346 = CARTESIAN_POINT ( 'NONE',  ( -5.115504031057831469, 4.862509545855891346, 0.7998128361456341429 ) ) ;
#41347 = CARTESIAN_POINT ( 'NONE',  ( 0.1808504484964272296, -2.097240537080494516, -0.5235256853268268618 ) ) ;
#41348 = CARTESIAN_POINT ( 'NONE',  ( 1.904351452098542063, 1.548259960728815665, -1.405051437006714643 ) ) ;
#41349 = CARTESIAN_POINT ( 'NONE',  ( 6.668979838189343035, -1.761623494860217631, -0.7799453142821392015 ) ) ;
#41350 = CARTESIAN_POINT ( 'NONE',  ( -4.381256195510448315, 8.263215994737505454, 1.040834085586084257E-14 ) ) ;
#41351 = CARTESIAN_POINT ( 'NONE',  ( 1.887459117809231701, 1.256508940344562397, 1.324596713471258402 ) ) ;
#41352 = CARTESIAN_POINT ( 'NONE',  ( 3.369938178094655346, 2.153121441420174698, -0.4834393813165636100 ) ) ;
#41353 = CARTESIAN_POINT ( 'NONE',  ( 11.94980361058169116, 12.70000000000000107, 1.099999999999994982 ) ) ;
#41354 = CARTESIAN_POINT ( 'NONE',  ( 1.283307755816986528, 0.1377011610334301639, -1.907463248872851569 ) ) ;
#41355 = CARTESIAN_POINT ( 'NONE',  ( 1.064831551406957511, 1.493571888342230203, -1.284017422347245807 ) ) ;
#41356 = CARTESIAN_POINT ( 'NONE',  ( 2.858853853349733409, 0.2825237051190258031, -1.921275437378862305 ) ) ;
#41357 = ORIENTED_EDGE ( 'NONE', *, *, #23547, .T. ) ;
#41358 = DIRECTION ( 'NONE',  ( -1.000000000000000000, 0.000000000000000000, 1.465138070926357285E-17 ) ) ;
#41360 = CARTESIAN_POINT ( 'NONE',  ( 6.262542430310119812, -0.6688554880303022587, -1.736790604091620560 ) ) ;
#41359 = CARTESIAN_POINT ( 'NONE',  ( -3.983063267364693960, 7.868933921892603323, -0.7998128361456481317 ) ) ;
#41361 = CARTESIAN_POINT ( 'NONE',  ( 5.923986774528332333, 5.876015756563318426, -0.7998128361456481317 ) ) ;
#41362 = CARTESIAN_POINT ( 'NONE',  ( 1.734723475976807094E-15, 2.499999999999998668, 3.150000000000001243 ) ) ;
#41363 = CARTESIAN_POINT ( 'NONE',  ( 10.73535870392234237, 11.41900666419791399, 0.000000000000000000 ) ) ;
#41364 = CARTESIAN_POINT ( 'NONE',  ( -6.286140498591554326, 7.362860665558790707, 1.199719254218452047 ) ) ;
#41365 = CARTESIAN_POINT ( 'NONE',  ( 2.349409277133751139, 0.5813161652389825518, -2.113004480973964760 ) ) ;
#41366 = CARTESIAN_POINT ( 'NONE',  ( 0.4019237886466778820, 11.60491455036742536, 1.500000000000001554 ) ) ;
#41367 = CARTESIAN_POINT ( 'NONE',  ( 6.713222337422018349, 7.861122810861019161, -1.199719254218452047 ) ) ;
#41368 = DIRECTION ( 'NONE',  ( 1.000000000000000000, -0.000000000000000000, -0.000000000000000000 ) ) ;
#41370 = CARTESIAN_POINT ( 'NONE',  ( 5.964077395145578109, -1.074666730956087335, 1.706109649615504154 ) ) ;
#41369 = CARTESIAN_POINT ( 'NONE',  ( 2.455445036260803349, 0.4872311372507812655, -1.759406031448563557 ) ) ;
#41371 =( NAMED_UNIT ( * ) SI_UNIT ( $, .STERADIAN. ) SOLID_ANGLE_UNIT ( ) );
#41372 = CARTESIAN_POINT ( 'NONE',  ( -4.288456660624211381, 3.897620947016656956, 1.214306433183764966E-14 ) ) ;
#41373 = CARTESIAN_POINT ( 'NONE',  ( -5.072456052330698739, 7.961014115122230450, -1.198640345919316674 ) ) ;
#41374 = CARTESIAN_POINT ( 'NONE',  ( 0.000000000000000000, -6.893137084989842123, 0.000000000000000000 ) ) ;
#41375 = B_SPLINE_CURVE_WITH_KNOTS ( 'NONE', 3,
 ( #211584, #12318, #44865, #61089, #29667, #146635, #11256, #210528, #77334, #48070 ),
 .UNSPECIFIED., .F., .F.,
 ( 4, 1, 1, 1, 1, 1, 1, 4 ),
 ( 0.000000000000000000, 0.09272347919791326665, 0.1850049962306132278, 0.2567072177207115891, 0.3610482009861257779, 0.5209239196176974618, 0.7336689415868371533, 1.000000000000000000 ),
 .UNSPECIFIED. ) ;
#41376 = CARTESIAN_POINT ( 'NONE',  ( 7.228468454380276853, 11.58496363008569574, 1.040834085586084257E-14 ) ) ;
#41377 = CARTESIAN_POINT ( 'NONE',  ( 2.051278105266049590, -1.547248087829168339, -1.147608674410576901 ) ) ;
#41378 = CARTESIAN_POINT ( 'NONE',  ( 5.981297772519293510, -0.05168599705708888659, 1.961257141919122926 ) ) ;
#41379 = CARTESIAN_POINT ( 'NONE',  ( 0.7500000000000006661, 15.41666666666666963, -1.299038105676657340 ) ) ;
#41380 = CARTESIAN_POINT ( 'NONE',  ( -6.714312387265696458, 8.856450423275211037, 1.599625672291283607 ) ) ;
#41381 = CARTESIAN_POINT ( 'NONE',  ( 3.147464216666835402, 6.823792019419957278, -0.7998128361456291469 ) ) ;
#41382 = CARTESIAN_POINT ( 'NONE',  ( -3.973948422136968084, 7.650373902552835226, -0.7216878364870458196 ) ) ;
#41383 = CARTESIAN_POINT ( 'NONE',  ( 8.353795204314554468, 12.89784483834236184, -0.7998128361456352531 ) ) ;
#41384 = CARTESIAN_POINT ( 'NONE',  ( 11.89829993707161471, 13.82919228251124721, 1.561606677374347329 ) ) ;
#41385 = CARTESIAN_POINT ( 'NONE',  ( 5.664915734613279241, 1.571387620024040421, -1.347999112033698266 ) ) ;
#41386 = CARTESIAN_POINT ( 'NONE',  ( 1.364683531249988535, 3.176041667008084435, 0.7879004041258500513 ) ) ;
#41387 = CARTESIAN_POINT ( 'NONE',  ( 5.239047776066017903, 2.296150469294107488, -0.1107920306624484569 ) ) ;
#41388 = CARTESIAN_POINT ( 'NONE',  ( 6.724481002698112775, 8.868313807946373473, -1.443375672974057666 ) ) ;
#41390 = CARTESIAN_POINT ( 'NONE',  ( -8.912450614902597934, 3.507114751586604129, -8.024806578263023127 ) ) ;
#41389 = CARTESIAN_POINT ( 'NONE',  ( 5.397554552016216256, 7.390509292142662723, 1.443375672974065660 ) ) ;
#41391 = CARTESIAN_POINT ( 'NONE',  ( 0.05906008026819106055, -2.050595067678960604, -1.024705011274627431 ) ) ;
#41392 = CARTESIAN_POINT ( 'NONE',  ( 8.002408263930250953, -6.836568542494980250, -7.346809171966436125 ) ) ;
#41393 = CARTESIAN_POINT ( 'NONE',  ( -7.259464905474441565, 7.434073576000447048, -0.7998128361456362523 ) ) ;
#41394 = CARTESIAN_POINT ( 'NONE',  ( 5.121012332258009891, -1.843477085030984286, 0.6107378676363499626 ) ) ;
#41395 = ORIENTED_EDGE ( 'NONE', *, *, #175333, .T. ) ;
#41396 = CARTESIAN_POINT ( 'NONE',  ( 9.707274797260268429, 10.42750147299956964, 0.000000000000000000 ) ) ;
#41397 = EDGE_LOOP ( 'NONE', ( #174661, #107209, #39167, #102565 ) ) ;
#41398 = CARTESIAN_POINT ( 'NONE',  ( 6.152599605923961157, 1.892562589925715466, 0.2737767527046449101 ) ) ;
#41399 = CARTESIAN_POINT ( 'NONE',  ( 0.7501351305400367764, 0.4964161116564491660, 1.651887862327553691 ) ) ;
#41400 = CARTESIAN_POINT ( 'NONE',  ( 6.104703911763087909, 1.883310800321544409, 0.7212973825745233603 ) ) ;
#41402 = CARTESIAN_POINT ( 'NONE',  ( -3.634994582239682526, 6.294558541704648569, 1.082531754730549967 ) ) ;
#41401 = CARTESIAN_POINT ( 'NONE',  ( -9.989660255170729641, 10.54902514065433827, -0.7998128361456291469 ) ) ;
#41403 = CARTESIAN_POINT ( 'NONE',  ( -3.285556943749998737, -1.917708332855377673, 1.896917185911908499 ) ) ;
#41405 = CARTESIAN_POINT ( 'NONE',  ( 1.305125929463516909, -0.4348595813401417987, 1.715451362885108466 ) ) ;
#41404 = CARTESIAN_POINT ( 'NONE',  ( 2.080132315211229876, -2.050506710900898977, -0.4067329413659624970 ) ) ;
#41406 = CARTESIAN_POINT ( 'NONE',  ( 6.574846728087075931, -0.8593996854794653251, 1.822268861383633531 ) ) ;
#41407 = EDGE_CURVE ( 'NONE', #158170, #36876, #182906, .T. ) ;
#41409 = CARTESIAN_POINT ( 'NONE',  ( 3.838036126445078633, 2.281091060459582209, 0.2259633074802695485 ) ) ;
#41408 = SURFACE_STYLE_FILL_AREA ( #123797 ) ;
#41410 = CARTESIAN_POINT ( 'NONE',  ( 2.114833760799132989, -1.688328753782810221, 0.4216566245275765179 ) ) ;
#41411 = AXIS2_PLACEMENT_3D ( 'NONE', #180562, #197866, #210917 ) ;
#41412 = CARTESIAN_POINT ( 'NONE',  ( 3.181995841446764839, 2.068044944583770306, -0.4684364081647199307 ) ) ;
#41413 = CARTESIAN_POINT ( 'NONE',  ( 4.929271367020211514, 7.908511140569038922, 1.199719254218452047 ) ) ;
#41414 = CARTESIAN_POINT ( 'NONE',  ( 2.670900524536640841, -0.6599870735717223713, -1.603529595030905641 ) ) ;
#41415 = CARTESIAN_POINT ( 'NONE',  ( 1.360316468750004448, 2.546875000341383810, -3.295974604355933479E-14 ) ) ;
#41416 = CARTESIAN_POINT ( 'NONE',  ( 1.345918344774723163, -0.8409936141995101311, 1.660288665089631799 ) ) ;
#41417 = CARTESIAN_POINT ( 'NONE',  ( 2.928372970691155430, 1.159507463759208878, 1.835456099276617570 ) ) ;
#41418 = CARTESIAN_POINT ( 'NONE',  ( 6.148786358997489820, 7.132337826040578754, -1.199719254218446718 ) ) ;
#41419 = CARTESIAN_POINT ( 'NONE',  ( 3.977750132953357998, -0.7672935630990398437, 1.865046046545227654 ) ) ;
#41420 = CARTESIAN_POINT ( 'NONE',  ( 3.187500000000002665, -1.451031289060985330, 1.451031289061251117 ) ) ;
#41421 = CARTESIAN_POINT ( 'NONE',  ( -1.500000000000013101, 2.660416667349483788, -0.8660254037844313801 ) ) ;
#41422 = CARTESIAN_POINT ( 'NONE',  ( 1.061403713111798153, 0.3786953092320010650, -1.888642112844605592 ) ) ;
#41423 = CARTESIAN_POINT ( 'NONE',  ( 0.6823417656249934904, 14.94270833367473195, 1.181850606188764807 ) ) ;
#41424 = CARTESIAN_POINT ( 'NONE',  ( 4.254274768897357006, 0.9481281144863746846, -2.009013624686401212 ) ) ;
#41425 = ORIENTED_EDGE ( 'NONE', *, *, #130663, .F. ) ;
#41426 = FACE_OUTER_BOUND ( 'NONE', #188070, .T. ) ;
#41427 = CARTESIAN_POINT ( 'NONE',  ( -1.500000000000001332, 0.9000000000000187850, 0.000000000000000000 ) ) ;
#41428 = CARTESIAN_POINT ( 'NONE',  ( 6.564118927310645724, 10.80988918183778225, -0.7998128361456291469 ) ) ;
#41429 = CARTESIAN_POINT ( 'NONE',  ( 1.364683531249986537, -0.6364583329919177856, 0.7879004041258500513 ) ) ;
#41430 = CARTESIAN_POINT ( 'NONE',  ( 6.328415579541645464, -1.046111920768664660, -1.959710881125435789 ) ) ;
#41431 = CARTESIAN_POINT ( 'NONE',  ( 5.002378505967389088, 1.956489882415031190, 0.1462272935644214900 ) ) ;
#41432 = CARTESIAN_POINT ( 'NONE',  ( 10.08690309888728187, 10.87040115823107911, -0.7216878364870257245 ) ) ;
#41433 =( GEOMETRIC_REPRESENTATION_CONTEXT ( 3 ) GLOBAL_UNCERTAINTY_ASSIGNED_CONTEXT ( ( #196722 ) ) GLOBAL_UNIT_ASSIGNED_CONTEXT ( ( #25166, #7839, #175704 ) ) REPRESENTATION_CONTEXT ( 'NONE', 'WORKASPACE' ) );
#41434 = CARTESIAN_POINT ( 'NONE',  ( 5.659536867407776839, 0.4493550105662181271, -2.217189852095033942 ) ) ;
#41435 = CARTESIAN_POINT ( 'NONE',  ( -4.814553946628611136, 8.631080347793099961, 0.000000000000000000 ) ) ;
#41436 = CARTESIAN_POINT ( 'NONE',  ( 2.752447824977616087, -2.056971473714273468, -0.1544007921008266060 ) ) ;
#41437 = CARTESIAN_POINT ( 'NONE',  ( -6.392833124043511894, 7.417059051927569868, 1.199719254218450271 ) ) ;
#41438 = ADVANCED_FACE ( 'NONE', ( #208460 ), #189025, .T. ) ;
#41439 = EDGE_LOOP ( 'NONE', ( #141924, #102034 ) ) ;
#41440 = CARTESIAN_POINT ( 'NONE',  ( 0.7499999999999885647, 2.597916667349486897, -1.299038105676658228 ) ) ;
#41441 = CARTESIAN_POINT ( 'NONE',  ( -1.364683531249997417, 4.571875000341417028, 1.214306433183764966E-14 ) ) ;
#41442 = CARTESIAN_POINT ( 'NONE',  ( 4.499188554602613799, 1.501106652244098116, 1.115835331622745841 ) ) ;
#41443 = CARTESIAN_POINT ( 'NONE',  ( 3.814867129904021770, 0.9234608866974923780, -1.467580195302587986 ) ) ;
#41444 = CARTESIAN_POINT ( 'NONE',  ( 1.698380523978352485, 1.446983168995601199, 0.9667953101664509274 ) ) ;
#41445 = CARTESIAN_POINT ( 'NONE',  ( 1.048812564444784989, -1.803156034432966681, 1.415383320267731726 ) ) ;
#41446 = CARTESIAN_POINT ( 'NONE',  ( 1.009129827085092135, 1.670030910484705755, -1.442630471070925458 ) ) ;
#41447 = CARTESIAN_POINT ( 'NONE',  ( 4.739831270385728601, 2.085251124590303373, 0.1521322122139453781 ) ) ;
#41448 = CARTESIAN_POINT ( 'NONE',  ( 6.070255116781061666, -1.844781929399732290, -0.6067975954986597475 ) ) ;
#41450 = ORIENTED_EDGE ( 'NONE', *, *, #101458, .T. ) ;
#41449 = CARTESIAN_POINT ( 'NONE',  ( 3.147653791585717453, 8.999999999999998224, -2.420000000000002149 ) ) ;
#41451 = CARTESIAN_POINT ( 'NONE',  ( 0.1939827082095749167, 1.755770691208278889, 0.9913967135185000057 ) ) ;
#41452 = CARTESIAN_POINT ( 'NONE',  ( -7.815970093360414158E-14, 8.210952333604092601, -2.038660652713623733 ) ) ;
#41453 = CARTESIAN_POINT ( 'NONE',  ( -2.944427096284358836, 6.586915378973714930, -0.4196793407983508972 ) ) ;
#41454 = CARTESIAN_POINT ( 'NONE',  ( -8.962103233833181193, 10.41454084668224489, -1.199719254218446718 ) ) ;
#41455 = CARTESIAN_POINT ( 'NONE',  ( 7.039708073993665494, 9.236078724457858158, 1.599625672291281386 ) ) ;
#41456 = CARTESIAN_POINT ( 'NONE',  ( 0.9679107548759222635, -4.157144623729205790, -0.3235293953625327235 ) ) ;
#41457 = CARTESIAN_POINT ( 'NONE',  ( 4.529811765687052016, -1.125283923072720071, -1.437579299059896343 ) ) ;
#41458 = CARTESIAN_POINT ( 'NONE',  ( 1.782535857997105566, -1.180187651135233384, 1.864495428577646274 ) ) ;
#41459 = ORIENTED_EDGE ( 'NONE', *, *, #78717, .F. ) ;
#41460 = CARTESIAN_POINT ( 'NONE',  ( -6.770317605177755382, 8.992066187497757213, 1.599625672291269396 ) ) ;
#41461 = CARTESIAN_POINT ( 'NONE',  ( -5.029148636026397945, 4.832037928311032182, 0.7998128361456281477 ) ) ;
#41462 = CARTESIAN_POINT ( 'NONE',  ( 0.000000000000000000, -2.034374999522043481, -3.793834371823813001 ) ) ;
#41463 = CARTESIAN_POINT ( 'NONE',  ( -7.867809214632013770, 8.073532260025807261, 1.040834085586084257E-14 ) ) ;
#41464 = CARTESIAN_POINT ( 'NONE',  ( 1.406516720256438369, -2.010457973371252205, -0.1935789593500591155 ) ) ;
#41465 = CARTESIAN_POINT ( 'NONE',  ( 0.9999999999999833467, 5.868705557303652398, 4.125226524755083446 ) ) ;
#41466 = CARTESIAN_POINT ( 'NONE',  ( -3.688700311369816909, 6.461178242310183784, -1.199719254218450271 ) ) ;
#41467 = CARTESIAN_POINT ( 'NONE',  ( 2.764321045800025800, -0.7073474514263197177, -1.721481455096545377 ) ) ;
#41468 = CARTESIAN_POINT ( 'NONE',  ( 4.403700966340357681, 4.032072637018845107, -0.7998128361456211532 ) ) ;
#41469 = CARTESIAN_POINT ( 'NONE',  ( 4.000000000000012434, 0.000000000000000000, -0.7500000000000006661 ) ) ;
#41470 = VERTEX_POINT ( 'NONE', #155464 ) ;
#41471 = CARTESIAN_POINT ( 'NONE',  ( -3.255929445576174697, 6.950334786480840243, -0.7998128361456281477 ) ) ;
#41472 = CARTESIAN_POINT ( 'NONE',  ( -8.670602931139386627, 10.07445716020612103, 1.199719254218462483 ) ) ;
#41473 = CARTESIAN_POINT ( 'NONE',  ( 4.916531288042031989, 1.256637652550334883, -1.324621001416517840 ) ) ;
#41475 = CARTESIAN_POINT ( 'NONE',  ( -4.009952404978103679, 7.802135278885950598, 0.4104602055842437314 ) ) ;
#41474 = CARTESIAN_POINT ( 'NONE',  ( -4.516801452008150086, 5.298631777878131111, 1.199719254218452935 ) ) ;
#41476 = CARTESIAN_POINT ( 'NONE',  ( 5.595231165798738360, 7.497995327707586810, -1.335214257040851615 ) ) ;
#41477 = CARTESIAN_POINT ( 'NONE',  ( 0.5261554912905551662, 1.716204961384654171, -0.2456527019241669663 ) ) ;
#41478 = CARTESIAN_POINT ( 'NONE',  ( 6.527308116070499544, -1.206667617865687214, -1.390688675169844624 ) ) ;
#41479 = CARTESIAN_POINT ( 'NONE',  ( 4.741030679083562127, 0.3911436318500530751, 2.274166950501448348 ) ) ;
#41480 = CARTESIAN_POINT ( 'NONE',  ( 4.203910148689107729, 7.062256385849379647, -1.199719254218448494 ) ) ;
#41481 = CARTESIAN_POINT ( 'NONE',  ( 0.7376602057446514094, -1.455437688833590926, -1.459210590049898171 ) ) ;
#41482 = CARTESIAN_POINT ( 'NONE',  ( 7.806797523370503811, 8.002351953554066810, 1.040834085586084257E-14 ) ) ;
#41483 =( GEOMETRIC_REPRESENTATION_CONTEXT ( 3 ) GLOBAL_UNCERTAINTY_ASSIGNED_CONTEXT ( ( #18257 ) ) GLOBAL_UNIT_ASSIGNED_CONTEXT ( ( #42147, #125592, #28003 ) ) REPRESENTATION_CONTEXT ( 'NONE', 'WORKASPACE' ) );
#41484 = CARTESIAN_POINT ( 'NONE',  ( 5.624470717464387093, 0.4563550445067353079, -2.252502686463413006 ) ) ;
#41485 = CARTESIAN_POINT ( 'NONE',  ( -0.4500000000000215494, 3.999999999999989786, -0.5000000000000160982 ) ) ;
#41486 = CARTESIAN_POINT ( 'NONE',  ( -7.598418745816086783, 7.829519723065708092, 0.000000000000000000 ) ) ;
#41487 = CARTESIAN_POINT ( 'NONE',  ( 6.174654088403855212, -1.776896415251895789, -0.5849557326117056366 ) ) ;
#41489 = CARTESIAN_POINT ( 'NONE',  ( -4.014095998097799267, 6.840806543492835345, -1.199719254218450271 ) ) ;
#41488 = CARTESIAN_POINT ( 'NONE',  ( 1.933716311909071006, -1.854087253938462521, 0.4680378644332866545 ) ) ;
#41490 = CARTESIAN_POINT ( 'NONE',  ( 5.022202109028018668, -1.178465353167540197, -1.865713892744431446 ) ) ;
#41491 = CARTESIAN_POINT ( 'NONE',  ( 4.979753661315234226, -0.7591050579739184734, 1.976773538454196677 ) ) ;
#41492 = CARTESIAN_POINT ( 'NONE',  ( 0.6124999999999793943, 0.4791666673494773820, -1.060881119635969094 ) ) ;
#41493 = CARTESIAN_POINT ( 'NONE',  ( 6.197485614778188712, 6.403023770095574108, -0.7216878364870458196 ) ) ;
#41494 = CARTESIAN_POINT ( 'NONE',  ( -6.265276382846530545, 6.482112999508623297, 0.000000000000000000 ) ) ;
#41495 = CARTESIAN_POINT ( 'NONE',  ( 2.397911878029312494, 1.783863880296262305, 1.463803424465635272 ) ) ;
#41496 = CARTESIAN_POINT ( 'NONE',  ( 3.279693232472491893, -1.891448704997201302, 0.5207070127687256633 ) ) ;
#41497 =( LENGTH_UNIT ( ) NAMED_UNIT ( * ) SI_UNIT ( .MILLI., .METRE. ) );
#41498 = CARTESIAN_POINT ( 'NONE',  ( 6.420768979138045118, -1.462686491410120970, 1.454469991251945649 ) ) ;
#41499 = CARTESIAN_POINT ( 'NONE',  ( 2.738383840280320669, 6.138605547061593448, 0.7216878364870338292 ) ) ;
#41500 = CARTESIAN_POINT ( 'NONE',  ( 3.054329744828568227, 6.785411478933790264, 0.000000000000000000 ) ) ;
#41501 = EDGE_LOOP ( 'NONE', ( #4048, #192765, #190260, #96327 ) ) ;
#41502 = CARTESIAN_POINT ( 'NONE',  ( 5.594935472981866553, 1.780666063871166882, 0.9463038388278843804 ) ) ;
#41503 = CARTESIAN_POINT ( 'NONE',  ( -9.646789991323334590, 11.21334206375407305, 1.199719254218462483 ) ) ;
#41504 = CARTESIAN_POINT ( 'NONE',  ( -11.01135777277262129, 10.89999999999998259, 1.399999999999998579 ) ) ;
#41505 = CARTESIAN_POINT ( 'NONE',  ( 7.262363838414439776, 11.62450824479221900, 0.7998128361456462443 ) ) ;
#41506 = CARTESIAN_POINT ( 'NONE',  ( 1.657326198882978385, 1.776537685197575822, -1.247748726553777221 ) ) ;
#41507 = DIRECTION ( 'NONE',  ( 1.014813233446432150E-15, 1.000000000000000000, -4.583713267641621330E-32 ) ) ;
#41508 = CARTESIAN_POINT ( 'NONE',  ( -9.367496997901326949, 14.48154074413197456, -7.499999999620649227 ) ) ;
#41510 = CARTESIAN_POINT ( 'NONE',  ( 4.037628742901151924, 7.560846779974220055, 0.4916741515407979102 ) ) ;
#41509 = B_SPLINE_CURVE_WITH_KNOTS ( 'NONE', 3,
 ( #199385, #211381, #130228, #197266, #67245, #80328, #32643, #133380, #63008, #51031 ),
 .UNSPECIFIED., .F., .F.,
 ( 4, 1, 1, 1, 1, 1, 1, 4 ),
 ( 0.000000000000000000, 0.09853459476447307130, 0.1926867929487333375, 0.2613852218134048999, 0.3629775382994345767, 0.5216635214973427415, 0.7338723600040717443, 1.000000000000000000 ),
 .UNSPECIFIED. ) ;
#41511 = CARTESIAN_POINT ( 'NONE',  ( 4.978670620768666844, 8.057607364700732688, 1.103355461389814662 ) ) ;
#41512 = CARTESIAN_POINT ( 'NONE',  ( 1.124374118904346798, 1.229854006068244132, -1.653384075620732307 ) ) ;
#41514 = CARTESIAN_POINT ( 'NONE',  ( 6.727182134110180733, 7.053024033604696541, 2.509100769544295950 ) ) ;
#41513 = CYLINDRICAL_SURFACE ( 'NONE', #11517, 1.500000000000000222 ) ;
#41515 = CARTESIAN_POINT ( 'NONE',  ( -1.364683531250012516, 1.280208333674755172, 0.7879004041258379498 ) ) ;
#41516 = SURFACE_STYLE_USAGE ( .BOTH. , #189874 ) ;
#41517 = VERTEX_POINT ( 'NONE', #90480 ) ;
#41518 = CARTESIAN_POINT ( 'NONE',  ( 3.123589223026546957, -0.3706944625661895976, 1.875830702792554483 ) ) ;
#41519 = STYLED_ITEM ( 'NONE', ( #204397 ), #127801 ) ;
#41520 = CARTESIAN_POINT ( 'NONE',  ( 5.084699950150380232, -0.2187599903600515594, -1.756180685135479091 ) ) ;
#41521 = CARTESIAN_POINT ( 'NONE',  ( 7.198453214212898743, 7.362893269528701268, 0.7998128361456291469 ) ) ;
#41522 = CARTESIAN_POINT ( 'NONE',  ( -3.066115294984855133, 6.728884944124295053, 0.7998128361456341429 ) ) ;
#41524 = CARTESIAN_POINT ( 'NONE',  ( 6.503544296663656077, -1.856690447402360888, 0.4709783565581044940 ) ) ;
#41523 = FACE_OUTER_BOUND ( 'NONE', #74723, .T. ) ;
#41525 = CARTESIAN_POINT ( 'NONE',  ( -1.500000000000015099, -0.1208333333333093396, -0.8660254037844383745 ) ) ;
#41526 = CARTESIAN_POINT ( 'NONE',  ( 0.3091450132529197647, -1.663722454078466306, 1.232067777400827069 ) ) ;
#41527 = CARTESIAN_POINT ( 'NONE',  ( -1.499999999999997780, 5.900000000000023448, 1.214306433183764966E-14 ) ) ;
#41528 = CARTESIAN_POINT ( 'NONE',  ( 6.455916552660014851, 1.865467424361374249, -0.1398750677365916961 ) ) ;
#41529 = CARTESIAN_POINT ( 'NONE',  ( 2.385134503015675200, 1.669401249834654433, -0.7394980648879890817 ) ) ;
#41531 = CARTESIAN_POINT ( 'NONE',  ( 6.003728048595398548, 7.077753126805482076, 1.059392881431284961 ) ) ;
#41530 = CARTESIAN_POINT ( 'NONE',  ( 5.654950187766193181, -1.741821662664808867, 1.355018943897445149 ) ) ;
#41532 = EDGE_CURVE ( 'NONE', #41837, #129023, #35372, .T. ) ;
#41533 = CARTESIAN_POINT ( 'NONE',  ( 1.364683531249986537, 0.4052083336747511200, -0.7879004041258309554 ) ) ;
#41534 = CARTESIAN_POINT ( 'NONE',  ( 3.350102204537624306, -0.8385132117052511713, 1.884735577694598430 ) ) ;
#41535 = CARTESIAN_POINT ( 'NONE',  ( -7.877450944739929461, 9.149113176073413456, 1.199719254218462483 ) ) ;
#41536 = CARTESIAN_POINT ( 'NONE',  ( 7.889955328148847258, 11.29236608522730911, -1.199719254218446718 ) ) ;
#41537 = CARTESIAN_POINT ( 'NONE',  ( 3.832150974156964818, 7.622593236491780999, 1.040834085586084257E-14 ) ) ;
#41538 = CARTESIAN_POINT ( 'NONE',  ( 0.2984011986874868794, -2.161112683670802337, -0.05330630956579958390 ) ) ;
#41539 = CARTESIAN_POINT ( 'NONE',  ( 6.047819040147648373, 9.213483425884394507, 1.199719254218452047 ) ) ;
#41540 = CARTESIAN_POINT ( 'NONE',  ( 5.125469573878929097, 0.2063957376101481500, -2.060066405364005426 ) ) ;
#41541 = CARTESIAN_POINT ( 'NONE',  ( 0.6823417656249882723, -0.2614583329919109578, -1.181850606188749264 ) ) ;
#41542 = CARTESIAN_POINT ( 'NONE',  ( 3.409602121571019051, -0.4253414365745535886, 2.119164713334599881 ) ) ;
#41543 = CARTESIAN_POINT ( 'NONE',  ( -4.640257700270903563, 8.337993449908045918, -0.3781808898682629261 ) ) ;
#41545 = CARTESIAN_POINT ( 'NONE',  ( 1.926150285298435572, 1.005797860886543660, 1.684270608208485065 ) ) ;
#41544 = CARTESIAN_POINT ( 'NONE',  ( 3.580727245018202165, -1.354872245433702105, 1.497987768207516668 ) ) ;
#41546 = CARTESIAN_POINT ( 'NONE',  ( 6.620655732516684822, 2.041257794637734602, 2.379778264366624096 ) ) ;
#41547 = B_SPLINE_CURVE_WITH_KNOTS ( 'NONE', 3,
 ( #66334, #1339, #81552, #132480 ),
 .UNSPECIFIED., .F., .F.,
 ( 4, 4 ),
 ( 0.000000000000000000, 0.0007854274309115643520 ),
 .UNSPECIFIED. ) ;
#41548 = EDGE_CURVE ( 'NONE', #136086, #103541, #151640, .T. ) ;
#41551 = CARTESIAN_POINT ( 'NONE',  ( 5.992340707560147806, 8.974519344586754599, 1.082531754730558626 ) ) ;
#41550 = CARTESIAN_POINT ( 'NONE',  ( -3.285556943749998737, -2.880208332855377584, 1.896917185911908499 ) ) ;
#41549 = CARTESIAN_POINT ( 'NONE',  ( 10.43625799253549857, 3.019799309333581316, 6.025376361322622998 ) ) ;
#41552 = CARTESIAN_POINT ( 'NONE',  ( -7.795011973214244883, 8.058878488363559356, 0.7998128361456341429 ) ) ;
#41553 = CARTESIAN_POINT ( 'NONE',  ( 1.798064920797682653, -0.9548589541341389042, -1.776165177175797583 ) ) ;
#41555 = CARTESIAN_POINT ( 'NONE',  ( -10.93220419382131325, -5.754340240174524723, 1.121760655089042704E-14 ) ) ;
#41554 = CARTESIAN_POINT ( 'NONE',  ( -5.901876940650454095, 5.779944607047298177, -0.7998128361456291469 ) ) ;
#41556 = CARTESIAN_POINT ( 'NONE',  ( -3.712022485150084705, 7.355926397811426654, 0.5818110939905510870 ) ) ;
#41557 = CARTESIAN_POINT ( 'NONE',  ( 5.625241921295836889, 1.689600096388569561, 0.8957793909229804230 ) ) ;
#41558 = CARTESIAN_POINT ( 'NONE',  ( -11.94650005372637835, 12.44897299662361867, 1.135399707157293658 ) ) ;
#41559 = CARTESIAN_POINT ( 'NONE',  ( 4.487385655998867406, 8.179107665399927285, 0.7216878364870438212 ) ) ;
#41561 = CARTESIAN_POINT ( 'NONE',  ( 2.776970437579088014, 1.727991955821889025, -1.039012595151635354 ) ) ;
#41560 = CARTESIAN_POINT ( 'NONE',  ( -7.483737604619046913, 11.67485160545682987, 0.000000000000000000 ) ) ;
#41562 = CARTESIAN_POINT ( 'NONE',  ( -1.201851678989727383E-14, 3.837500000000021227, -1.732050807568863648 ) ) ;
#41563 = CARTESIAN_POINT ( 'NONE',  ( -1.402160292154681736E-14, 13.48437500034139269, 1.575800808251682339 ) ) ;
#41564 = CARTESIAN_POINT ( 'NONE',  ( 6.651377187556704484, -1.389000575594327103, -1.022263415358831473 ) ) ;
#41565 = CARTESIAN_POINT ( 'NONE',  ( 7.849244587668864348, 8.122149871893999062, 0.7998128361456291469 ) ) ;
#41566 = CARTESIAN_POINT ( 'NONE',  ( 8.920901888111997025, 10.47043562662792304, 1.082531754730549967 ) ) ;
#41567 = CARTESIAN_POINT ( 'NONE',  ( -11.41381678389388377, 11.02879418241073139, -3.704697885617973530 ) ) ;
#41568 = CARTESIAN_POINT ( 'NONE',  ( 4.358574879328508622, -1.387578095181252413, 1.254630796652965730 ) ) ;
#41569 = FILL_AREA_STYLE ('',( #136925 ) ) ;
#41570 = CARTESIAN_POINT ( 'NONE',  ( 1.639598513223254006, 1.914365469054382540, -0.7886191548351070280 ) ) ;
#41571 = CARTESIAN_POINT ( 'NONE',  ( -7.553300976144787349, 8.945177572657957654, -1.082531754730549967 ) ) ;
#41572 = ORIENTED_EDGE ( 'NONE', *, *, #45759, .F. ) ;
#41573 = CARTESIAN_POINT ( 'NONE',  ( 4.146814880933355596, 5.931313009212638931, 1.599625672291261402 ) ) ;
#41574 = EDGE_CURVE ( 'NONE', #21699, #9480, #154400, .T. ) ;
#41575 = CARTESIAN_POINT ( 'NONE',  ( 0.3690327605676722023, -1.530577755691145958, -0.9687459989127805704 ) ) ;
#41576 = CARTESIAN_POINT ( 'NONE',  ( 3.892599500454932304, 7.555466827257172113, 0.7216878364870257245 ) ) ;
#41577 = DIRECTION ( 'NONE',  ( 0.000000000000000000, 1.000000000000000000, 0.000000000000000000 ) ) ;
#41578 = EDGE_LOOP ( 'NONE', ( #167068, #197166, #175308, #145820 ) ) ;
#41579 = CARTESIAN_POINT ( 'NONE',  ( 9.042925270190638187, 9.652427024751663254, 0.7216878364870458196 ) ) ;
#41580 = AXIS2_PLACEMENT_3D ( 'NONE', #157578, #60056, #192173 ) ;
#41581 = CARTESIAN_POINT ( 'NONE',  ( 7.884230021546724920, 9.157022099014721306, 1.199719254218462483 ) ) ;
#41582 = CARTESIAN_POINT ( 'NONE',  ( 6.538697978567284963, -1.477089011224671955, 1.219511253712385335 ) ) ;
#41583 = CARTESIAN_POINT ( 'NONE',  ( 3.212919216758630014, 6.692230152952963529, 0.000000000000000000 ) ) ;
#41584 = LINE ( 'NONE', #38357, #176883 ) ;
#41585 =( BOUNDED_CURVE ( )  B_SPLINE_CURVE ( 2, ( #102315, #200854, #54635, #155342, #119703, #21036, #87135, #153206, #48518 ),
 .UNSPECIFIED., .F., .T. ) 
 B_SPLINE_CURVE_WITH_KNOTS ( ( 3, 2, 2, 2, 3 ),
 ( 0.9553571428571427937, 0.9583333333333333703, 0.9642857142857143016, 0.9702380952380952328, 0.9732142857142856984 ),
 .UNSPECIFIED. ) 
 CURVE ( )  GEOMETRIC_REPRESENTATION_ITEM ( )  RATIONAL_B_SPLINE_CURVE ( ( 0.9330127018922194093, 0.9330127018922180770, 1.000000000000000000, 0.8660254037844387076, 1.000000000000000000, 0.8660254037844387076, 1.000000000000000000, 0.9330127018922194093, 0.9330127018922194093 ) ) 
 REPRESENTATION_ITEM ( '' )  );
#41586 = CARTESIAN_POINT ( 'NONE',  ( 8.536830278099042602, 13.11138575775759563, -0.7998128361456352531 ) ) ;
#41587 = ADVANCED_FACE ( 'NONE', ( #8137 ), #63772, .F. ) ;
#41588 = DIRECTION ( 'NONE',  ( -0.7592566023652993490, 0.6507913734559652719, 0.000000000000000000 ) ) ;
#41590 = ORIENTED_EDGE ( 'NONE', *, *, #107353, .T. ) ;
#41589 = CARTESIAN_POINT ( 'NONE',  ( 3.524756749872944628, 7.056040608253000279, -0.7216878364870267237 ) ) ;
#41591 = CARTESIAN_POINT ( 'NONE',  ( -7.158341918335454857, 10.33485409049125003, 1.082531754730549967 ) ) ;
#41592 = CARTESIAN_POINT ( 'NONE',  ( 3.133815226704575796, -1.450665623810345473, -1.602838778681406007 ) ) ;
#41593 = ADVANCED_FACE ( 'NONE', ( #44941, #129459 ), #64368, .T. ) ;
#41594 = CARTESIAN_POINT ( 'NONE',  ( -6.455090533882201775, 8.624301270986276080, -1.443375672974066548 ) ) ;
#41595 = CARTESIAN_POINT ( 'NONE',  ( 7.865138509703455405, 8.348618814175074121, -0.7216878364870317197 ) ) ;
#41596 = CARTESIAN_POINT ( 'NONE',  ( -2.117044542028253318, 5.621635732341564662, -0.7998128361456281477 ) ) ;
#41597 = CARTESIAN_POINT ( 'NONE',  ( 6.124025070245508573, -1.016541136310184390, -1.516163765885633286 ) ) ;
#41598 = CARTESIAN_POINT ( 'NONE',  ( 10.48252959204799772, 8.670818378862373166, 6.558037413528325033 ) ) ;
#41599 = CARTESIAN_POINT ( 'NONE',  ( 1.352734582195244561, -1.556726207391207817, 1.209420702486432297 ) ) ;
#41600 = CARTESIAN_POINT ( 'NONE',  ( 3.533378866418676711, -0.1359047358975660202, 1.907598245988059826 ) ) ;
#41601 = EDGE_LOOP ( 'NONE', ( #151332, #153689 ) ) ;
#41602 = CARTESIAN_POINT ( 'NONE',  ( -3.543819121313565468, 14.48034520796839253, -11.47346693582755606 ) ) ;
#41603 = CARTESIAN_POINT ( 'NONE',  ( 5.248484213797577347, -1.954463446003468885, -0.2428638724455249587 ) ) ;
#41604 = VERTEX_POINT ( 'NONE', #31878 ) ;
#41605 = CARTESIAN_POINT ( 'NONE',  ( 5.776890131463271238, 1.792767593593114439, -0.7471807142077312447 ) ) ;
#41606 = EDGE_LOOP ( 'NONE', ( #118169, #85260, #119661, #14728 ) ) ;
#41607 = CARTESIAN_POINT ( 'NONE',  ( -5.960744811863571968, 6.983232364376142698, 1.199719254218452935 ) ) ;
#41609 = CARTESIAN_POINT ( 'NONE',  ( -0.3282377607281434240, 1.363835450998170051, 1.224999999999967892 ) ) ;
#41608 = CARTESIAN_POINT ( 'NONE',  ( -4.716257332707368910, 6.595662536282280719, -1.599625672291271394 ) ) ;
#41610 = CARTESIAN_POINT ( 'NONE',  ( 6.604230223188150894, 9.758666789477915771, -1.082531754730548412 ) ) ;
#41612 = ORIENTED_EDGE ( 'NONE', *, *, #86559, .T. ) ;
#41611 = CARTESIAN_POINT ( 'NONE',  ( 3.422422624566554994, -0.7774026117220147469, -1.747318718686732275 ) ) ;
#41613 = CARTESIAN_POINT ( 'NONE',  ( 1.009129827085092135, 1.670030910484705755, -1.442630471070925458 ) ) ;
#41614 = CARTESIAN_POINT ( 'NONE',  ( 9.574107575049746188, 3.767509416808712430, -7.159700411437375678 ) ) ;
#41615 = CARTESIAN_POINT ( 'NONE',  ( 6.111982388360997831, -0.6759622889470856544, 1.896349411511048855 ) ) ;
#41616 = DIRECTION ( 'NONE',  ( 1.224646799147343346E-16, 0.000000000000000000, -1.000000000000000000 ) ) ;
#41617 = CARTESIAN_POINT ( 'NONE',  ( 6.481070005604858686, -0.09514881109910081070, -1.823337098959529001 ) ) ;
#41618 = CARTESIAN_POINT ( 'NONE',  ( 1.680221237283368696, -1.148429780529091948, -1.722445320287042447 ) ) ;
#41619 = CARTESIAN_POINT ( 'NONE',  ( -7.413611068574208041, 7.543634422958360730, 0.7998128361456341429 ) ) ;
#41620 = CARTESIAN_POINT ( 'NONE',  ( -5.733196416021622888, 7.293175961584016598, -1.208997762321398550 ) ) ;
#41621 = CARTESIAN_POINT ( 'NONE',  ( -0.1296875068448159751, 0.001480089298542403009, -1.826395826379861864 ) ) ;
#41622 = CARTESIAN_POINT ( 'NONE',  ( 6.789956943122251509, -0.7972922127613899512, 1.690610701080223821 ) ) ;
#41623 = CARTESIAN_POINT ( 'NONE',  ( 5.124091990960999432, 8.065525525174782828, -1.199719254218452047 ) ) ;
#41624 =( NAMED_UNIT ( * ) SI_UNIT ( $, .STERADIAN. ) SOLID_ANGLE_UNIT ( ) );
#41625 = CARTESIAN_POINT ( 'NONE',  ( 3.919715808126649659, 7.587102519540811940, 0.000000000000000000 ) ) ;
#41626 = CARTESIAN_POINT ( 'NONE',  ( 1.874158809982179319, 3.299964346911585356, -0.3999999999999993006 ) ) ;
#41627 = COLOUR_RGB ( '', 0.72549020, 0.75294118, 0.79215686) ;
#41628 = FACE_OUTER_BOUND ( 'NONE', #139788, .T. ) ;
#41629 = CARTESIAN_POINT ( 'NONE',  ( -1.364683531250014514, 11.40104166700806410, -0.7879004041258335089 ) ) ;
#41631 = CARTESIAN_POINT ( 'NONE',  ( -5.444481204339554736, 8.509589284108232121, 1.199719254218454489 ) ) ;
#41630 = CARTESIAN_POINT ( 'NONE',  ( 6.825078400183573812, 0.002648415797040087893, 1.855566311045192540 ) ) ;
#41632 = CARTESIAN_POINT ( 'NONE',  ( 5.115702696222887980, 0.1348363893083539267, 1.728983578677806499 ) ) ;
#41633 = CARTESIAN_POINT ( 'NONE',  ( -3.242371291962510504, 6.934516940598226320, 1.040834085586084257E-14 ) ) ;
#41634 = CARTESIAN_POINT ( 'NONE',  ( 2.922783962489564846, -1.430918204188264875, 1.496350883549990352 ) ) ;
#41635 = CARTESIAN_POINT ( 'NONE',  ( 3.884452219389774363, -0.6659801820031689967, -2.009805269316313314 ) ) ;
#41636 = CARTESIAN_POINT ( 'NONE',  ( 7.233438648090761980, 8.397765496649418182, 1.199719254218462483 ) ) ;
#41637 = CARTESIAN_POINT ( 'NONE',  ( -1.364683531250012516, 3.738541667008087099, -0.7879004041258300672 ) ) ;
#41638 = CARTESIAN_POINT ( 'NONE',  ( 1.235132629255174974, -0.04286028942791567098, -1.969139623717565790 ) ) ;
#41639 = CARTESIAN_POINT ( 'NONE',  ( 6.001708393183096568, 6.086876045059843143, 0.6039332608892417076 ) ) ;
#41641 = CARTESIAN_POINT ( 'NONE',  ( -0.1229892814952095459, -1.709044814581164973, -0.8582256167319823881 ) ) ;
#41640 = CARTESIAN_POINT ( 'NONE',  ( -1.737500000000000266, -1.458333333333332371, -3.009438278150923907 ) ) ;
#41642 = CARTESIAN_POINT ( 'NONE',  ( 4.224787546089771695, 0.1105535957067731723, 2.289718640476182898 ) ) ;
#41643 = CARTESIAN_POINT ( 'NONE',  ( 2.244514701088017539, 0.3993153960501935051, 1.781317584591130432 ) ) ;
#41644 = CARTESIAN_POINT ( 'NONE',  ( 6.066347387471824781, 6.042103138330730872, -0.7998128361456481317 ) ) ;
#41645 = CARTESIAN_POINT ( 'NONE',  ( 5.463572716182819811, 8.357623354646536384, 1.082531754730558626 ) ) ;
#41646 = CARTESIAN_POINT ( 'NONE',  ( -7.802881099864745984, 9.062115023719057305, -1.199719254218446718 ) ) ;
#41647 = CARTESIAN_POINT ( 'NONE',  ( 2.777592571122803555, 0.2913108041502753820, -1.991885045997557224 ) ) ;
#41648 = CARTESIAN_POINT ( 'NONE',  ( 3.819154011256303161, -1.728040176127441985, -0.9287006429716244682 ) ) ;
#41649 = CARTESIAN_POINT ( 'NONE',  ( -8.843996274815957293, 9.212417163573759282, 1.040834085586084257E-14 ) ) ;
#41650 = CARTESIAN_POINT ( 'NONE',  ( -5.900823170445743671, 7.907379670318584353, 1.599625672291269396 ) ) ;
#41651 = CARTESIAN_POINT ( 'NONE',  ( 11.33772463945037146, 19.00000000000000000, 3.679999999999999272 ) ) ;
#41653 = CARTESIAN_POINT ( 'NONE',  ( 4.996827606291168955, 1.470251540571869020, -0.9849021259363596181 ) ) ;
#41652 = CARTESIAN_POINT ( 'NONE',  ( 6.421832395068366672, 1.204883778905677216, -1.708312069947721668 ) ) ;
#41654 = CARTESIAN_POINT ( 'NONE',  ( -1.743066579297358008E-15, 2.187499999999992006, -1.225000000000032951 ) ) ;
#41655 = EDGE_CURVE ( 'NONE', #103805, #91287, #27301, .T. ) ;
#41656 = CARTESIAN_POINT ( 'NONE',  ( 0.9904705247469265394, -0.5356807779838267392, -2.124848333686576662 ) ) ;
#41657 = CARTESIAN_POINT ( 'NONE',  ( 5.630708778567339756, -1.570753007681056079, 0.7496256940079452091 ) ) ;
#41658 = CARTESIAN_POINT ( 'NONE',  ( 8.239604668803105270, 10.63595808506888396, -1.599625672291268286 ) ) ;
#41659 = CARTESIAN_POINT ( 'NONE',  ( 0.1333692844072559558, 0.7140749627707367875, -2.136770008611441618 ) ) ;
#41660 = CARTESIAN_POINT ( 'NONE',  ( 6.205746375452622310, 2.143286971341977765, 0.8312943217957665665 ) ) ;
#41661 = CARTESIAN_POINT ( 'NONE',  ( 0.1333692844072559003, 5.722267537706915874, -2.647605121726896105 ) ) ;
#41662 = CARTESIAN_POINT ( 'NONE',  ( 5.553917692138156781, 1.528130387303320514, -0.8190655202615308994 ) ) ;
#41663 =( BOUNDED_SURFACE ( )  B_SPLINE_SURFACE ( 3, 3, ( 
 ( #137683, #188543, #203704, #156056, #7644, #92145, #55351, #205854, #174457, #57486, #123647 ),
 ( #108437, #189609, #22820, #158199, #191728, #59610, #41255, #43384, #107365, #91071, #88935 ),
 ( #9789, #173386, #8723, #24969, #157132, #75863, #141970, #125766, #94274, #61748, #66764 ),
 ( #29253, #193868, #30323, #80120, #12979, #159241, #11919, #111633, #60672, #133980, #183750 ),
 ( #51636, #77992, #150205, #50556, #95345, #198910, #177644, #1777, #132905, #76915, #117760 ),
 ( #45517, #211176, #126835, #161395, #79054, #194943, #182676, #28179, #145171, #96408, #162458 ),
 ( #67834, #62802, #146225, #14034, #699, #116677, #160315, #34297, #209036, #18031, #93209 ) ),
 .UNSPECIFIED., .T., .F., .F. ) 
 B_SPLINE_SURFACE_WITH_KNOTS ( ( 4, 3, 4 ),
 ( 4, 1, 1, 1, 1, 1, 1, 1, 4 ),
 ( 0.000000000000000000, 0.5000000000000000000, 1.000000000000000000 ),
 ( 0.000000000000000000, 0.2254494161556361009, 0.3971188491599597081, 0.5240836380151728813, 0.6154273167216615104, 0.6803253696226415626, 0.7282602231486813293, 0.7688932809586735972, 1.000000000000000000 ),
 .UNSPECIFIED. ) 
 GEOMETRIC_REPRESENTATION_ITEM ( )  RATIONAL_B_SPLINE_SURFACE ( (
 ( 1.000000000000000222, 1.000000000000000222, 0.9999999999999995559, 1.000000000000000666, 0.9999999999999997780, 0.9999999999999997780, 1.000000000000000000, 1.000000000000000000, 1.000000000000000000, 1.000000000000000000, 1.000000000000000000),
 ( 0.3333333333333334259, 0.3333333333333334259, 0.3333333333333332593, 0.3333333333333335369, 0.3333333333333333148, 0.3333333333333333148, 0.3333333333333334259, 0.3333333333333333703, 0.3333333333333333148, 0.3333333333333333703, 0.3333333333333333703),
 ( 0.3333333333333334259, 0.3333333333333334259, 0.3333333333333332593, 0.3333333333333335369, 0.3333333333333333148, 0.3333333333333333148, 0.3333333333333334259, 0.3333333333333333703, 0.3333333333333333148, 0.3333333333333333703, 0.3333333333333333703),
 ( 1.000000000000000222, 1.000000000000000222, 0.9999999999999995559, 1.000000000000000666, 0.9999999999999997780, 0.9999999999999997780, 1.000000000000000000, 1.000000000000000000, 1.000000000000000000, 1.000000000000000000, 1.000000000000000000),
 ( 0.3333333333333334259, 0.3333333333333334259, 0.3333333333333332593, 0.3333333333333335369, 0.3333333333333333148, 0.3333333333333333148, 0.3333333333333334259, 0.3333333333333333703, 0.3333333333333333148, 0.3333333333333333703, 0.3333333333333333703),
 ( 0.3333333333333334259, 0.3333333333333334259, 0.3333333333333332593, 0.3333333333333335369, 0.3333333333333333148, 0.3333333333333333148, 0.3333333333333334259, 0.3333333333333333703, 0.3333333333333333148, 0.3333333333333333703, 0.3333333333333333703),
 ( 1.000000000000000222, 1.000000000000000222, 0.9999999999999995559, 1.000000000000000666, 0.9999999999999997780, 0.9999999999999997780, 1.000000000000000000, 1.000000000000000000, 1.000000000000000000, 1.000000000000000000, 1.000000000000000000) ) ) 
 REPRESENTATION_ITEM ( '' )  SURFACE ( )  );
#41664 = MECHANICAL_DESIGN_GEOMETRIC_PRESENTATION_REPRESENTATION (  '', ( #159145 ), #69287 ) ;
#41665 = CARTESIAN_POINT ( 'NONE',  ( 6.057114314241694331, 1.778561107892376647, -1.245054071093915304 ) ) ;
#41666 = CYLINDRICAL_SURFACE ( 'NONE', #61930, 1.500000000000000222 ) ;
#41667 = CARTESIAN_POINT ( 'NONE',  ( 0.05801502780489272565, 1.224741999009547833, 1.726997829920233540 ) ) ;
#41668 = CARTESIAN_POINT ( 'NONE',  ( 3.906250000000001776, 1.895863743163997084, -0.7852924748301890467 ) ) ;
#41669 = CARTESIAN_POINT ( 'NONE',  ( 6.727182134110196721, 7.051813866762763006, 2.787205683092201181 ) ) ;
#41670 = CARTESIAN_POINT ( 'NONE',  ( 4.700175447307747945, -1.925963193209312418, -0.04779502591981815707 ) ) ;
#41671 = CARTESIAN_POINT ( 'NONE',  ( 1.499999999999997113, 11.42708333401612997, -0.8660254037844378194 ) ) ;
#41672 = CARTESIAN_POINT ( 'NONE',  ( 0.7158630905677393352, 1.819291361130066287, 1.274270043568943800 ) ) ;
#41673 = ORIENTED_EDGE ( 'NONE', *, *, #82844, .F. ) ;
#41674 = CARTESIAN_POINT ( 'NONE',  ( 0.7499999999999920064, 4.983333333333353821, 1.299038105676669330 ) ) ;
#41675 = CARTESIAN_POINT ( 'NONE',  ( 5.834086172582112262, 5.700855377634248100, 1.040834085586084257E-14 ) ) ;
#41676 = CARTESIAN_POINT ( 'NONE',  ( 7.494959990256193194, 7.638541498254023843, -0.7998128361456281477 ) ) ;
#41677 = CARTESIAN_POINT ( 'NONE',  ( 2.332966905468473406, 1.448476307009987307, -1.684171307209429314 ) ) ;
#41678 = CARTESIAN_POINT ( 'NONE',  ( -8.026063749610047537, 11.34719622697832264, -1.082531754730543971 ) ) ;
#41679 = CARTESIAN_POINT ( 'NONE',  ( 4.379563740902463920, 4.008367186281499350, -0.1129952432600847406 ) ) ;
#41680 = CARTESIAN_POINT ( 'NONE',  ( 5.653386867218496370, 9.539442411822841805, 1.040834085586084257E-14 ) ) ;
#41681 = EDGE_CURVE ( 'NONE', #150870, #108531, #92958, .T. ) ;
#41682 = CARTESIAN_POINT ( 'NONE',  ( -8.120970824461345217, 12.41829036193951730, 0.7216878364870458196 ) ) ;
#41683 = CARTESIAN_POINT ( 'NONE',  ( 5.560252395380198998, 9.501061871336672127, 0.7216878364870317197 ) ) ;
#41684 = CARTESIAN_POINT ( 'NONE',  ( 0.7564826839323666174, 1.942540863013635821, -0.5404934282097761944 ) ) ;
#41686 = CARTESIAN_POINT ( 'NONE',  ( 6.496538660071067284, 2.039668932145132008, 0.3065683105917779705 ) ) ;
#41685 = CARTESIAN_POINT ( 'NONE',  ( 9.023114925094663619, 10.48572115315399245, 1.199719254218453823 ) ) ;
#41687 = CARTESIAN_POINT ( 'NONE',  ( -10.90688615205346856, -6.291672674598600246, 8.483881999699072196E-15 ) ) ;
#41688 = CARTESIAN_POINT ( 'NONE',  ( 7.661766205054107992, 8.111351125417501251, -0.7216878364870317197 ) ) ;
#41689 = CARTESIAN_POINT ( 'NONE',  ( -1.402160292154681736E-14, 1.696875000341421469, -1.575800808251659024 ) ) ;
#41690 = CARTESIAN_POINT ( 'NONE',  ( 0.9481069621972251227, 0.5063937300482551640, 1.695761627633844304 ) ) ;
#41691 = CARTESIAN_POINT ( 'NONE',  ( 0.2115648487451895210, 1.930418618556551946, 0.5826528611774861588 ) ) ;
#41692 = CARTESIAN_POINT ( 'NONE',  ( 5.056098682708163317, -1.255628792201430644, 1.205468413292756669 ) ) ;
#41693 = CARTESIAN_POINT ( 'NONE',  ( 3.755682109644884026, 2.274985096322924338, -0.2814536430481278662 ) ) ;
#41694 = CARTESIAN_POINT ( 'NONE',  ( -0.6823417656250246877, 0.05104166700808931978, 1.181850606188755259 ) ) ;
#41695 = CARTESIAN_POINT ( 'NONE',  ( 2.238008233095424515, 0.4029187984595939409, 1.796341404040911804 ) ) ;
#41696 = CARTESIAN_POINT ( 'NONE',  ( 9.935427640716063991, 10.48575375712389679, -0.7998128361456281477 ) ) ;
#41697 = CARTESIAN_POINT ( 'NONE',  ( 0.000000000000000000, 3.999999999999994671, 12.00000000000000355 ) ) ;
#41698 = CARTESIAN_POINT ( 'NONE',  ( 2.942213871598580166, 1.811567870905493205, 0.2252638538085757203 ) ) ;
#41699 = CARTESIAN_POINT ( 'NONE',  ( 3.463517678199812266, -1.944071305346905643, -0.5350885120067662148 ) ) ;
#41700 = CARTESIAN_POINT ( 'NONE',  ( -9.398826802771548472, 11.98838390803207865, -1.599625672291263179 ) ) ;
#41702 = CARTESIAN_POINT ( 'NONE',  ( 0.000000000000000000, 3.000000000000002665, 0.000000000000000000 ) ) ;
#41701 = CARTESIAN_POINT ( 'NONE',  ( 3.942437297418455611, 2.251314906739984245, 0.2249487974115715883 ) ) ;
#41703 = CARTESIAN_POINT ( 'NONE',  ( 4.981522283868931034, 1.966010104637575751, -0.7553895412903822715 ) ) ;
#41704 = CARTESIAN_POINT ( 'NONE',  ( 8.985344024325859991, 14.65809313286843185, 7.243008760641457044 ) ) ;
#41705 = CARTESIAN_POINT ( 'NONE',  ( 2.734898984476673789, -1.980466496001157317, -0.6033880717724803278 ) ) ;
#41706 = CARTESIAN_POINT ( 'NONE',  ( 3.330499290451326200, 7.037332938835193730, -0.7998128361456291469 ) ) ;
#41707 = CARTESIAN_POINT ( 'NONE',  ( -5.558564015327489343E-14, 0.6093750003414449834, -1.570758158831798257 ) ) ;
#41708 = CARTESIAN_POINT ( 'NONE',  ( 4.494861206476631565, -2.057060146276223023, -0.5143016718046622415 ) ) ;
#41709 = B_SPLINE_CURVE_WITH_KNOTS ( 'NONE', 3,
 ( #143632, #128496, #14629, #164110 ),
 .UNSPECIFIED., .F., .F.,
 ( 4, 4 ),
 ( 1.569810930355607827E-17, 0.0001726908832627367966 ),
 .UNSPECIFIED. ) ;
#41711 = CARTESIAN_POINT ( 'NONE',  ( 0.5395173010800574653, -1.361483316988669978, -1.363248745070398726 ) ) ;
#41710 = CARTESIAN_POINT ( 'NONE',  ( -2.887523529586332405, 5.352232636950553513, 1.082531754730560403 ) ) ;
#41712 = CARTESIAN_POINT ( 'NONE',  ( -5.503684012504701961, 5.385662534202396934, 0.000000000000000000 ) ) ;
#41713 = CARTESIAN_POINT ( 'NONE',  ( 7.411503528164766763, 11.79850454950093841, 1.040834085586084257E-14 ) ) ;
#41714 = CARTESIAN_POINT ( 'NONE',  ( 5.194182247366869731, 7.153241603385088965, 1.443375672974064550 ) ) ;
#41715 = CARTESIAN_POINT ( 'NONE',  ( 5.007133299032078710, 6.576657384445655730, 1.236533897214306066 ) ) ;
#41716 = CARTESIAN_POINT ( 'NONE',  ( -3.475000000000000533, -0.6562499990440846531, 0.000000000000000000 ) ) ;
#41717 = CARTESIAN_POINT ( 'NONE',  ( -3.405069135326500351, 7.124331091189553433, 1.040834085586084257E-14 ) ) ;
#41718 = CARTESIAN_POINT ( 'NONE',  ( 0.9498388403609931974, -2.005144016916958982, 0.9564107486674018332 ) ) ;
#41719 = CARTESIAN_POINT ( 'NONE',  ( 2.450341380362738075, 2.105475501793910631, 0.05272098179117353650 ) ) ;
#41720 = CARTESIAN_POINT ( 'NONE',  ( -5.113360211009450040, 5.994616996712990975, -1.199719254218453823 ) ) ;
#41721 = CARTESIAN_POINT ( 'NONE',  ( 7.239163954692881653, 10.53310948286200599, -1.199719254218441611 ) ) ;
#41722 = CARTESIAN_POINT ( 'NONE',  ( 6.842638030098166624, -1.824918384715786823, -0.3633994975895912805 ) ) ;
#41723 = CARTESIAN_POINT ( 'NONE',  ( 6.265839547809997079, 10.46189657242035587, 0.7998128361456462443 ) ) ;
#41724 = CARTESIAN_POINT ( 'NONE',  ( 11.86687215968023601, 9.990577876942188240, 1.056395335932121871 ) ) ;
#41725 = CARTESIAN_POINT ( 'NONE',  ( -7.119440060951841787, 7.478637290631501067, 0.000000000000000000 ) ) ;
#41726 = CARTESIAN_POINT ( 'NONE',  ( -8.026063749610047537, 11.34719622697832264, -1.082531754730543971 ) ) ;
#41727 = CARTESIAN_POINT ( 'NONE',  ( -0.1929003719821283658, -0.4722129235960635940, -2.074948700427194481 ) ) ;
#41728 = SURFACE_STYLE_FILL_AREA ( #192199 ) ;
#41730 = CARTESIAN_POINT ( 'NONE',  ( 2.928120951529111338, 1.047165451586975049, 1.658829547137883775 ) ) ;
#41729 = CARTESIAN_POINT ( 'NONE',  ( 1.224999999999993427, -0.8750000000000077716, -3.989863994746656317E-14 ) ) ;
#41731 = CARTESIAN_POINT ( 'NONE',  ( 1.710078970767275885, -2.145365142986368934, 0.2646356489638818088 ) ) ;
#41733 = CARTESIAN_POINT ( 'NONE',  ( -5.584559075236136039, 6.202510182859402477, -0.8982034194818852013 ) ) ;
#41732 = CARTESIAN_POINT ( 'NONE',  ( -5.093022980588950865, 5.970890227889075419, -1.199719254218453823 ) ) ;
#41734 = CARTESIAN_POINT ( 'NONE',  ( -1.364683531250012516, 1.280208333674755172, 0.7879004041258379498 ) ) ;
#41735 = CARTESIAN_POINT ( 'NONE',  ( 3.362975788648288944, 1.697558991927169192, -0.3826393865087075463 ) ) ;
#41736 = CARTESIAN_POINT ( 'NONE',  ( 5.341549334104176872, 9.175631956522799726, 0.7216878364870438212 ) ) ;
#41737 = CARTESIAN_POINT ( 'NONE',  ( -11.33520460194134394, 5.279085700950885141, -5.677819296561938955 ) ) ;
#41739 = ORIENTED_EDGE ( 'NONE', *, *, #170196, .T. ) ;
#41738 = EDGE_CURVE ( 'NONE', #132336, #176259, #82560, .T. ) ;
#41740 = CARTESIAN_POINT ( 'NONE',  ( 1.932970024460831882, 1.034005469613193062, 1.730602090182407959 ) ) ;
#41741 = CARTESIAN_POINT ( 'NONE',  ( 6.825078400183544503, 3.684911640780349718, 2.658296617506946458 ) ) ;
#41742 = CARTESIAN_POINT ( 'NONE',  ( 0.6202742476981680797, -1.157488721396517040, -1.825510493854154426 ) ) ;
#41743 = CARTESIAN_POINT ( 'NONE',  ( 2.729320057108883368, -1.840128979258702557, 0.7079907272262278006 ) ) ;
#41746 = EDGE_LOOP ( 'NONE', ( #92048, #50092, #93957, #174674, #105968, #13310, #213228, #156894 ) ) ;
#41745 = CARTESIAN_POINT ( 'NONE',  ( -4.014622883422329203, 6.737458226417744278, -1.082531754730546636 ) ) ;
#41744 = DIRECTION ( 'NONE',  ( 1.000000000000000000, 0.000000000000000000, 0.000000000000000000 ) ) ;
#41747 = CARTESIAN_POINT ( 'NONE',  ( -6.102578539482539810, 6.292298848917299736, 0.000000000000000000 ) ) ;
#41748 = CARTESIAN_POINT ( 'NONE',  ( 5.013482942003290255, 9.071090208970993274, -0.7998128361456481317 ) ) ;
#41749 = CARTESIAN_POINT ( 'NONE',  ( -4.606738333593328072, 8.596554832492683929, 0.7998128361456281477 ) ) ;
#41750 = CARTESIAN_POINT ( 'NONE',  ( 1.981123565540498177, -1.847491841353067210, -0.8164113852280636685 ) ) ;
#41751 = DIRECTION ( 'NONE',  ( -0.000000000000000000, -1.000000000000000000, -0.000000000000000000 ) ) ;
#41752 = CARTESIAN_POINT ( 'NONE',  ( 5.754963864978503985, -1.823789643192383014, 1.413694633616706886 ) ) ;
#41753 = CARTESIAN_POINT ( 'NONE',  ( 6.865691018405424728, -0.4312029709039078007, 1.920920986087648163 ) ) ;
#41754 = CARTESIAN_POINT ( 'NONE',  ( 3.010546455304231372, 0.6564385890225448161, 1.848828695667027677 ) ) ;
#41755 = CARTESIAN_POINT ( 'NONE',  ( 7.899597058256738968, 12.36794700127490820, 1.040834085586084257E-14 ) ) ;
#41756 = CARTESIAN_POINT ( 'NONE',  ( 0.8267963299631932994, 0.8146243292815741333, -1.844710905833810255 ) ) ;
#41757 = ORIENTED_EDGE ( 'NONE', *, *, #170416, .T. ) ;
#41758 = CARTESIAN_POINT ( 'NONE',  ( 2.378245518041781636, -2.112004366230528785, -0.1507482023494610135 ) ) ;
#41760 = CARTESIAN_POINT ( 'NONE',  ( -7.854251061018346469, 8.057714414143200443, -0.7998128361456291469 ) ) ;
#41759 = CARTESIAN_POINT ( 'NONE',  ( -10.64229060209977540, 1.016282880930358790, 6.144329343916601793 ) ) ;
#41761 = CARTESIAN_POINT ( 'NONE',  ( 2.290725937607818175, 1.422998120520948984, 1.168276728405498455 ) ) ;
#41762 = ORIENTED_EDGE ( 'NONE', *, *, #25593, .F. ) ;
#41763 = CARTESIAN_POINT ( 'NONE',  ( -8.459397779922852578, 11.95671561229694824, 1.199719254218453823 ) ) ;
#41764 = CARTESIAN_POINT ( 'NONE',  ( 10.19611990457454453, 10.80814481035635310, 6.242388940945101439 ) ) ;
#41765 = CARTESIAN_POINT ( 'NONE',  ( 3.199588043238619228, 1.915454767000431602, -0.9102714984489732597 ) ) ;
#41766 = CARTESIAN_POINT ( 'NONE',  ( -0.02968770228140016343, 0.003472272166151618711, -1.826291111852257343 ) ) ;
#41767 = CARTESIAN_POINT ( 'NONE',  ( -1.500000000000011324, 4.660416667349484676, -0.8660254037844313801 ) ) ;
#41768 = CARTESIAN_POINT ( 'NONE',  ( 7.100719765255169236, 9.307259030929609267, -1.599625672291262513 ) ) ;
#41769 = CARTESIAN_POINT ( 'NONE',  ( 7.686546744304875389, 7.932335721302671949, 0.7998128361456291469 ) ) ;
#41770 = CARTESIAN_POINT ( 'NONE',  ( 4.639950097937448170, 0.8846809987467202374, -1.861387103252240660 ) ) ;
#41771 = AXIS2_PLACEMENT_3D ( 'NONE', #128003, #75952, #176656 ) ;
#41773 = CARTESIAN_POINT ( 'NONE',  ( 1.593040506729075823, -0.6195558395927207584, 1.734028948791266345 ) ) ;
#41772 = CARTESIAN_POINT ( 'NONE',  ( -7.985916173649233230, 9.275655943134292869, -1.199719254218446718 ) ) ;
#41774 = CARTESIAN_POINT ( 'NONE',  ( -1.001543065824772872E-14, 4.571875000341418804, 1.575800808251672791 ) ) ;
#41775 = CARTESIAN_POINT ( 'NONE',  ( -0.02244404828160087226, 1.323617703852699057, -2.440988974267483957 ) ) ;
#41776 = CARTESIAN_POINT ( 'NONE',  ( -2.973437390567118310, 6.691037065628751002, -0.02693349654502708024 ) ) ;
#41777 = CARTESIAN_POINT ( 'NONE',  ( 2.854315967138055132, 6.433244981884085334, -0.2941531795266367211 ) ) ;
#41778 = CARTESIAN_POINT ( 'NONE',  ( 1.049787907720298286, -1.741764784136769162, -1.355102641770723704 ) ) ;
#41779 = CARTESIAN_POINT ( 'NONE',  ( 3.796368952254399964, -2.259583311708447617, -0.1157369865004975740 ) ) ;
#41780 = CARTESIAN_POINT ( 'NONE',  ( -7.537970219518075332, 10.77775377520434574, -1.082531754730543971 ) ) ;
#41781 = CARTESIAN_POINT ( 'NONE',  ( 3.357467859903106255, -1.375039365347962450, -1.179588011891503418 ) ) ;
#41782 = EDGE_CURVE ( 'NONE', #47758, #8679, #124253, .T. ) ;
#41783 = CARTESIAN_POINT ( 'NONE',  ( 2.993272137104509678, -0.3688056758139393043, 1.879696595719517083 ) ) ;
#41784 = CARTESIAN_POINT ( 'NONE',  ( 4.158688916442685013, -0.6465363538536235133, -1.966910096795893681 ) ) ;
#41785 = CARTESIAN_POINT ( 'NONE',  ( 0.6823417656249899377, 2.905208333674754062, 1.181850606188765695 ) ) ;
#41786 = AXIS2_PLACEMENT_3D ( 'NONE', #33905, #182280, #131468 ) ;
#41787 = CARTESIAN_POINT ( 'NONE',  ( 2.430492692261185805, 1.911874441976011640, 0.4805678379448170001 ) ) ;
#41788 = CARTESIAN_POINT ( 'NONE',  ( 1.465712096425618949, 1.898328545170711035, -0.3267402372346754902 ) ) ;
#41789 = CARTESIAN_POINT ( 'NONE',  ( 3.397188523315307407, 1.473948685399184333, 1.151750840393983344 ) ) ;
#41790 = CARTESIAN_POINT ( 'NONE',  ( 2.420946758181366842, 1.505949115154591400, -1.748677306438247703 ) ) ;
#41791 = CARTESIAN_POINT ( 'NONE',  ( 4.228838981530287811, -1.735973604985484142, -0.6712095357626171044 ) ) ;
#41792 = CARTESIAN_POINT ( 'NONE',  ( 0.6823417656249899377, 3.926041667008085767, -1.181850606188754593 ) ) ;
#41793 = CARTESIAN_POINT ( 'NONE',  ( -3.924195396151603177, 6.665646164563756138, 1.199719254218464037 ) ) ;
#41794 = CARTESIAN_POINT ( 'NONE',  ( 7.447506452608354088, 7.583179037664891098, 0.7998128361456341429 ) ) ;
#41795 = DIRECTION ( 'NONE',  ( 0.000000000000000000, 0.000000000000000000, -1.000000000000000000 ) ) ;
#41796 = CARTESIAN_POINT ( 'NONE',  ( 0.1004013553109489865, -2.105664478878019441, -0.04916207707313274139 ) ) ;
#41797 = CARTESIAN_POINT ( 'NONE',  ( 3.023105065722954787, 5.510411095776657220, 1.082531754730546636 ) ) ;
#41799 = DIRECTION ( 'NONE',  ( 1.000000000000000000, -3.135042426464105837E-15, 0.000000000000000000 ) ) ;
#41798 = CARTESIAN_POINT ( 'NONE',  ( 0.6823417656249899377, 3.488541667008085323, -1.181850606188754593 ) ) ;
#41800 = CARTESIAN_POINT ( 'NONE',  ( -1.843739406749240750, 8.928444911142053186, -0.7749999999999996891 ) ) ;
#41801 = CARTESIAN_POINT ( 'NONE',  ( 1.547299434221154124, 0.2130619955753136618, 2.109896976817266179 ) ) ;
#41802 = CARTESIAN_POINT ( 'NONE',  ( 0.4924518904856821089, -1.118466686806585342, 1.681619975139287515 ) ) ;
#41803 = CARTESIAN_POINT ( 'NONE',  ( -0.6823417656250003738, 0.9677083336747521747, -1.181850606188749264 ) ) ;
#41804 = CARTESIAN_POINT ( 'NONE',  ( -4.934804725694231564, 5.819988937140460727, -1.082531754730544860 ) ) ;
#41805 = CARTESIAN_POINT ( 'NONE',  ( 6.145923705696426431, 6.064665832934283962, 0.7998128361456341429 ) ) ;
#41806 = ADVANCED_FACE ( 'NONE', ( #100061 ), #183436, .T. ) ;
#41807 = CARTESIAN_POINT ( 'NONE',  ( 1.511231465835579879, 1.905624552496063995, 1.020381674553122231 ) ) ;
#41810 = CARTESIAN_POINT ( 'NONE',  ( 4.365362273920250225, 5.155639410070820716, 1.082531754730560403 ) ) ;
#41809 = CARTESIAN_POINT ( 'NONE',  ( 6.825078400183554272, 2.980425674467934272, 2.309322343017068402 ) ) ;
#41808 = CARTESIAN_POINT ( 'NONE',  ( 5.574337433874081427, 6.532423756721743580, -1.199719254218452047 ) ) ;
#41811 = CARTESIAN_POINT ( 'NONE',  ( -0.2104748580754413345, 7.629137130509052511, -2.703678718140525739 ) ) ;
#41812 = CARTESIAN_POINT ( 'NONE',  ( 5.313685493615880162, -1.282986534165726944, -1.555701818360885280 ) ) ;
#41814 = CARTESIAN_POINT ( 'NONE',  ( -6.916067756302494374, 7.241369601873926420, 0.000000000000000000 ) ) ;
#41813 = CARTESIAN_POINT ( 'NONE',  ( -10.00555417720528872, 10.77549408293541866, 0.7216878364870438212 ) ) ;
#41815 = CARTESIAN_POINT ( 'NONE',  ( 1.220146605508150803E-14, 11.46875000068279604, -1.499999999999998446 ) ) ;
#41817 = CARTESIAN_POINT ( 'NONE',  ( -1.364683531250000748, 11.10937500034139802, 0.000000000000000000 ) ) ;
#41816 = CARTESIAN_POINT ( 'NONE',  ( 0.6380306694902828646, -1.602208245511031803, -1.597717328844779239 ) ) ;
#41818 = CARTESIAN_POINT ( 'NONE',  ( -10.15913717534155047, 10.74674821418697057, 0.7998128361456462443 ) ) ;
#41820 = CARTESIAN_POINT ( 'NONE',  ( 0.3158528693416655653, 0.9839445311579012587, -1.643420606830671815 ) ) ;
#41819 = CARTESIAN_POINT ( 'NONE',  ( -4.243338890952892406, 7.894386439512932618, -0.7216878364870257245 ) ) ;
#41821 = CARTESIAN_POINT ( 'NONE',  ( -1.402160292154681736E-14, 0.6343750003414162508, 1.575800808251672791 ) ) ;
#41822 = DIRECTION ( 'NONE',  ( 0.000000000000000000, 1.000000000000000000, 0.000000000000000000 ) ) ;
#41823 = CARTESIAN_POINT ( 'NONE',  ( 1.500000000000001332, 8.875000000000001776, 0.000000000000000000 ) ) ;
#41824 = CARTESIAN_POINT ( 'NONE',  ( 3.439825841515719240, 0.7741550462027242396, -1.541462414610708764 ) ) ;
#41825 = CARTESIAN_POINT ( 'NONE',  ( 2.925527285498711549, 6.635141943048991742, 0.7998128361456281477 ) ) ;
#41826 = CARTESIAN_POINT ( 'NONE',  ( 6.099189001301251523, 8.209082816308541197, 1.599625672291268286 ) ) ;
#41827 = CARTESIAN_POINT ( 'NONE',  ( 1.071160155259534674, 1.707552549077664183, -0.4648152392626672680 ) ) ;
#41828 = CARTESIAN_POINT ( 'NONE',  ( 1.488932678171340118, -1.912290114023627252, -0.6292827167945020950 ) ) ;
#41829 = CARTESIAN_POINT ( 'NONE',  ( 6.983263157960366563, -0.003091553303710344557, 1.945923119799706669 ) ) ;
#41830 = CARTESIAN_POINT ( 'NONE',  ( 3.645738483435243982, -1.669485028154977790, -1.443228448415982079 ) ) ;
#41831 = ORIENTED_EDGE ( 'NONE', *, *, #56390, .F. ) ;
#41833 = CARTESIAN_POINT ( 'NONE',  ( 8.880227426826641235, 10.42298208846167284, 1.082531754730549967 ) ) ;
#41832 = CIRCLE ( 'NONE', #90360, 0.08000000000000020983 ) ;
#41835 = CARTESIAN_POINT ( 'NONE',  ( 2.970327539257538341, -1.987051465770898417, -0.3419137282784574516 ) ) ;
#41834 = CARTESIAN_POINT ( 'NONE',  ( 3.844477943020713440, 1.133112341739877849, -1.792160191984671691 ) ) ;
#41837 = VERTEX_POINT ( 'NONE', #50247 ) ;
#41836 = CARTESIAN_POINT ( 'NONE',  ( 3.304753640158542893, -0.3582801770840525757, -1.775609565582184191 ) ) ;
#41838 = CARTESIAN_POINT ( 'NONE',  ( 4.064412189046650248, 7.963840997188264659, 0.7998128361456271485 ) ) ;
#41839 = EDGE_LOOP ( 'NONE', ( #30531, #53319, #26065, #3703 ) ) ;
#41840 = CARTESIAN_POINT ( 'NONE',  ( 1.252583056964752029, -1.476889893665521702, 1.148006582770304096 ) ) ;
#41841 = CARTESIAN_POINT ( 'NONE',  ( 6.059193749186201572, -1.568369423792463024, -0.9343120793870243190 ) ) ;
#41843 = CARTESIAN_POINT ( 'NONE',  ( 2.483477273924311834, -0.5967159848992757976, 1.820515277383168540 ) ) ;
#41842 = CARTESIAN_POINT ( 'NONE',  ( -3.521367211247373508, 5.131347717920458962, -1.599625672291256295 ) ) ;
#41844 = CARTESIAN_POINT ( 'NONE',  ( 1.257518954444997838, 3.239770990628810576, 0.7750000000000152323 ) ) ;
#41845 = PRESENTATION_STYLE_ASSIGNMENT (( #190189 ) ) ;
#41846 = ADVANCED_FACE ( 'NONE', ( #1457 ), #182357, .T. ) ;
#41847 = CARTESIAN_POINT ( 'NONE',  ( 0.6823417656249899377, 1.155208333674752286, 1.181850606188755259 ) ) ;
#41848 = CARTESIAN_POINT ( 'NONE',  ( 2.391594655221662258, 3.742896273583267597, -11.51132696612780748 ) ) ;
#41849 = CARTESIAN_POINT ( 'NONE',  ( 6.699137298928153683, 7.948653282571920720, 1.082531754730549967 ) ) ;
#41850 = EDGE_CURVE ( 'NONE', #37457, #145929, #175781, .T. ) ;
#41851 = CARTESIAN_POINT ( 'NONE',  ( -3.011319516011047082, 6.527306845405913549, 0.7216878364870328300 ) ) ;
#41852 = CARTESIAN_POINT ( 'NONE',  ( -5.966470118465691641, 9.118576350588734059, -1.199719254218452047 ) ) ;
#41853 = CARTESIAN_POINT ( 'NONE',  ( 3.252298345715322725, 0.9499829135306799843, -1.895951488860507128 ) ) ;
#41855 = CARTESIAN_POINT ( 'NONE',  ( -10.16827420574893814, 6.288608293322982767, 5.589418380748610637 ) ) ;
#41854 = CARTESIAN_POINT ( 'NONE',  ( -0.02948999725182251813, 4.092753722544117956, -2.481335295887850290 ) ) ;
#41856 =( BOUNDED_SURFACE ( )  B_SPLINE_SURFACE ( 1, 2, ( 
 ( #77530, #144715, #159854, #209646, #128514, #14649, #81798, #65520, #163068, #94876, #80743, #210727, #45063, #127448, #146831, #62353, #504, #148931, #53559, #66572, #153194, #152136, #37306, #17832, #199792, #67637, #84988, #86059, #2643, #50365, #181420, #132714, #115429, #82855, #150006, #34105, #1576, #166242, #165177, #116488, #51437, #136959, #100177, #99128, #83915, #184609, #3704, #49312, #169442, #87124, #16771, #198719, #133784, #35158, #183551, #118622, #119692, #68717, #33050, #69780, #182477, #167317, #117557, #101235, #18904, #151079, #134838, #200841, #135889, #4766, #52492, #36226, #102305, #201907, #185677, #168378, #21027, #19975, #103380, #70843, #6915, #5845, #54626, #123990, #23167, #107718, #205122, #120773, #108785, #170503, #206200, #202986, #204040, #189957, #157484, #56765, #7995, #139095, #106633, #174811, #22086, #173745, #88197, #26387, #74087, #154271, #105536, #104456, #71916, #25322, #172662, #24237, #156408, #140178, #138025, #186753, #41607, #57828, #72992, #55689, #121845, #171570, #38375, #187816, #122931, #91423, #191010, #75153, #90339, #39442, #9079, #89283, #155331, #188888, #40529, #141263, #207271, #58902, #125055, #42678, #92499, #158538, #10135, #76210, #78342, #160670, #177996, #179063, #95695, #143390, #59961, #27457, #208330, #175869, #28535, #127193, #94627, #44810, #43742, #209388, #144465, #15460, #193160, #192076, #110914, #63166, #96765, #142320, #48013, #180122, #109855, #93555, #12265, #128266, #62107, #211531, #146584, #161750, #126116, #162816, #61032, #45872, #210469, #159599, #194228, #111994, #176920, #11197, #14393, #31747, #29610, #13341, #79416, #80484, #212601, #145533, #114130, #129332, #77278, #195308, #46939, #113057, #30682, #64239, #130383, #196373, #97820, #163885, #2393, #201665, #69535, #53312, #164928, #200601, #147629, #115181, #103135, #19733, #169193, #51184, #18663, #150831, #16520, #99935, #33854, #68472, #182230, #1333, #32801, #84743, #149756, #181176, #134600, #52248, #67394, #199542, #117307, #132473, #257, #183303, #81546 ),
 ( #165997, #198475, #133535, #102066, #35985, #17582, #119444, #83665, #82603, #34910, #100982, #98875, #50120, #116241, #167071, #135642, #168131, #185432, #118375, #37052, #213647, #184363, #85812, #151891, #3466, #65273, #131419, #49061, #197419, #148688, #66328, #7745, #189706, #22919, #40275, #171323, #138849, #207020, #202737, #205955, #54388, #141012, #106385, #120526, #137782, #136712, #104208, #139928, #204866, #56521, #188644, #172408, #186505, #152948, #156164, #23996, #105287, #170255, #38136, #203800, #4523, #86881, #39195, #57588, #8827, #107469, #122681, #5589, #73832, #71668, #21840, #87948, #89034, #20786, #154022, #55446, #25071, #121598, #124805, #123745, #74904, #187570, #155089, #6675, #90099, #41359, #173495, #72752, #70598, #91173, #157232, #58651, #190764, #42428, #108533, #125870, #94374, #195046, #30428, #12020, #47762, #174563, #13080, #59710, #176668, #175617, #158298, #142069, #92252, #28280, #208083, #10943, #191829, #144219, #96514, #193970, #162563, #130135, #128016, #212341, #79160, #192896, #112802, #44552, #14135, #145276, #80228, #45618, #159346, #61849, #111735, #110668, #177741, #60780, #9889, #43492, #160415, #29356, #26139, #146326, #78092, #62905, #77017, #75966, #129075, #178815, #143146, #109612, #46684, #63982, #209141, #126939, #211282, #196124, #210213, #95450, #27204, #93311, #161500, #81300, #35727, #115986, #51996, #7, #113876, #31496, #67142, #147377, #101803, #100734, #99675, #82348, #167872, #19470, #97571, #50927, #1077, #163628, #213404, #85547, #151637, #197170, #18407, #179871, #65025, #135387, #118122, #201408, #83412, #117052, #183049, #48806, #132214, #66072, #34664, #198223, #33605, #131180, #166813, #181974, #114923, #84483, #150573, #165745, #17331, #149494, #164679, #32543, #133276, #15209, #16264, #180922, #98618, #199284, #2135, #148439, #3204, #68211, #69273, #134342, #49859, #200347, #184107, #90905, #172146, #71408, #205685, #137520, #189449, #106123, #41091, #138584, #37872, #154826, #72483, #203537, #204607, #153757, #102875, #86618, #38940 ) ),
 .UNSPECIFIED., .F., .F., .T. ) 
 B_SPLINE_SURFACE_WITH_KNOTS ( ( 2, 2 ),
 ( 3, 2, 2, 2, 2, 2, 2, 2, 2, 2, 2, 2, 2, 2, 2, 2, 2, 2, 2, 2, 2, 2, 2, 2, 2, 2, 2, 2, 2, 2, 2, 2, 2, 2, 2, 2, 2, 2, 2, 2, 2, 2, 2, 2, 2, 2, 2, 2, 2, 2, 2, 2, 2, 2, 2, 2, 2, 2, 2, 2, 2, 2, 2, 2, 2, 2, 2, 2, 2, 2, 2, 2, 2, 2, 2, 2, 2, 2, 2, 2, 2, 2, 2, 2, 2, 2, 2, 2, 2, 2, 2, 2, 2, 2, 2, 2, 2, 2, 2, 2, 2, 2, 2, 2, 2, 2, 2, 2, 2, 2, 2, 2, 2, 2, 2, 2, 2, 2, 2, 2, 3 ),
 ( 0.000000000000000000, 1.000000000000000000 ),
 ( 0.000000000000000000, 0.008333333333333333218, 0.01666666666666666644, 0.02500000000000000139, 0.03333333333333333287, 0.04166666666666666435, 0.05000000000000000278, 0.05833333333333333426, 0.06666666666666666574, 0.07499999999999999722, 0.08333333333333332871, 0.09166666666666666019, 0.1000000000000000056, 0.1083333333333333370, 0.1166666666666666685, 0.1250000000000000000, 0.1333333333333333315, 0.1416666666666666630, 0.1499999999999999944, 0.1583333333333333259, 0.1666666666666666574, 0.1749999999999999889, 0.1833333333333333204, 0.1916666666666666796, 0.2000000000000000111, 0.2083333333333333426, 0.2166666666666666741, 0.2250000000000000056, 0.2333333333333333370, 0.2416666666666666685, 0.2500000000000000000, 0.2583333333333333592, 0.2666666666666666630, 0.2750000000000000222, 0.2833333333333333259, 0.2916666666666666852, 0.2999999999999999889, 0.3083333333333333481, 0.3166666666666666519, 0.3250000000000000111, 0.3333333333333333148, 0.3416666666666666741, 0.3499999999999999778, 0.3583333333333333370, 0.3666666666666666408, 0.3750000000000000000, 0.3833333333333333592, 0.3916666666666666630, 0.4000000000000000222, 0.4083333333333333259, 0.4166666666666666852, 0.4249999999999999889, 0.4333333333333333481, 0.4416666666666666519, 0.4500000000000000111, 0.4583333333333333148, 0.4666666666666666741, 0.4749999999999999778, 0.4833333333333333370, 0.4916666666666666408, 0.5000000000000000000, 0.5083333333333333037, 0.5166666666666667185, 0.5250000000000000222, 0.5333333333333333259, 0.5416666666666666297, 0.5500000000000000444, 0.5583333333333333481, 0.5666666666666666519, 0.5749999999999999556, 0.5833333333333333703, 0.5916666666666666741, 0.5999999999999999778, 0.6083333333333332815, 0.6166666666666666963, 0.6250000000000000000, 0.6333333333333333037, 0.6416666666666667185, 0.6500000000000000222, 0.6583333333333333259, 0.6666666666666666297, 0.6750000000000000444, 0.6833333333333333481, 0.6916666666666666519, 0.6999999999999999556, 0.7083333333333333703, 0.7166666666666666741, 0.7249999999999999778, 0.7333333333333332815, 0.7416666666666666963, 0.7500000000000000000, 0.7583333333333333037, 0.7666666666666667185, 0.7750000000000000222, 0.7833333333333333259, 0.7916666666666666297, 0.8000000000000000444, 0.8083333333333333481, 0.8166666666666666519, 0.8249999999999999556, 0.8333333333333333703, 0.8416666666666666741, 0.8499999999999999778, 0.8583333333333332815, 0.8666666666666666963, 0.8750000000000000000, 0.8833333333333333037, 0.8916666666666667185, 0.9000000000000000222, 0.9083333333333333259, 0.9166666666666666297, 0.9250000000000000444, 0.9333333333333333481, 0.9416666666666666519, 0.9499999999999999556, 0.9583333333333333703, 0.9666666666666666741, 0.9749999999999999778, 0.9833333333333332815, 0.9916666666666666963, 1.000000000000000000 ),
 .UNSPECIFIED. ) 
 GEOMETRIC_REPRESENTATION_ITEM ( )  RATIONAL_B_SPLINE_SURFACE ( (
 ( 1.000000000000000000, 0.8660254037844387076, 1.000000000000000000, 0.8660254037844387076, 1.000000000000000000, 0.8660254037844387076, 1.000000000000000000, 0.8660254037844387076, 1.000000000000000000, 0.8660254037844387076, 1.000000000000000000, 0.8660254037844387076, 1.000000000000000000, 0.8660254037844387076, 1.000000000000000000, 0.8660254037844387076, 1.000000000000000000, 0.8660254037844387076, 1.000000000000000000, 0.8660254037844387076, 1.000000000000000000, 0.8660254037844387076, 1.000000000000000000, 0.8660254037844387076, 1.000000000000000000, 0.8660254037844387076, 1.000000000000000000, 0.8660254037844387076, 1.000000000000000000, 0.8660254037844387076, 1.000000000000000000, 0.8660254037844387076, 1.000000000000000000, 0.8660254037844387076, 1.000000000000000000, 0.8660254037844387076, 1.000000000000000000, 0.8660254037844387076, 1.000000000000000000, 0.8660254037844387076, 1.000000000000000000, 0.8660254037844387076, 1.000000000000000000, 0.8660254037844387076, 1.000000000000000000, 0.8660254037844387076, 1.000000000000000000, 0.8660254037844387076, 1.000000000000000000, 0.8660254037844387076, 1.000000000000000000, 0.8660254037844387076, 1.000000000000000000, 0.8660254037844387076, 1.000000000000000000, 0.8660254037844387076, 1.000000000000000000, 0.8660254037844387076, 1.000000000000000000, 0.8660254037844387076, 1.000000000000000000, 0.8660254037844387076, 1.000000000000000000, 0.8660254037844387076, 1.000000000000000000, 0.8660254037844387076, 1.000000000000000000, 0.8660254037844387076, 1.000000000000000000, 0.8660254037844387076, 1.000000000000000000, 0.8660254037844387076, 1.000000000000000000, 0.8660254037844387076, 1.000000000000000000, 0.8660254037844387076, 1.000000000000000000, 0.8660254037844387076, 1.000000000000000000, 0.8660254037844387076, 1.000000000000000000, 0.8660254037844387076, 1.000000000000000000, 0.8660254037844387076, 1.000000000000000000, 0.8660254037844387076, 1.000000000000000000, 0.8660254037844387076, 1.000000000000000000, 0.8660254037844387076, 1.000000000000000000, 0.8660254037844387076, 1.000000000000000000, 0.8660254037844387076, 1.000000000000000000, 0.8660254037844387076, 1.000000000000000000, 0.8660254037844387076, 1.000000000000000000, 0.8660254037844387076, 1.000000000000000000, 0.8660254037844387076, 1.000000000000000000, 0.8660254037844387076, 1.000000000000000000, 0.8660254037844387076, 1.000000000000000000, 0.8660254037844387076, 1.000000000000000000, 0.8660254037844387076, 1.000000000000000000, 0.8660254037844387076, 1.000000000000000000, 0.8660254037844387076, 1.000000000000000000, 0.8660254037844387076, 1.000000000000000000, 0.8660254037844387076, 1.000000000000000000, 0.8660254037844387076, 1.000000000000000000, 0.8660254037844387076, 1.000000000000000000, 0.8660254037844387076, 1.000000000000000000, 0.8660254037844387076, 1.000000000000000000, 0.8660254037844387076, 1.000000000000000000, 0.8660254037844387076, 1.000000000000000000, 0.8660254037844387076, 1.000000000000000000, 0.8660254037844387076, 1.000000000000000000, 0.8660254037844387076, 1.000000000000000000, 0.8660254037844387076, 1.000000000000000000, 0.8660254037844387076, 1.000000000000000000, 0.8660254037844387076, 1.000000000000000000, 0.8660254037844387076, 1.000000000000000000, 0.8660254037844387076, 1.000000000000000000, 0.8660254037844387076, 1.000000000000000000, 0.8660254037844387076, 1.000000000000000000, 0.8660254037844387076, 1.000000000000000000, 0.8660254037844387076, 1.000000000000000000, 0.8660254037844387076, 1.000000000000000000, 0.8660254037844387076, 1.000000000000000000, 0.8660254037844387076, 1.000000000000000000, 0.8660254037844387076, 1.000000000000000000, 0.8660254037844387076, 1.000000000000000000, 0.8660254037844387076, 1.000000000000000000, 0.8660254037844387076, 1.000000000000000000, 0.8660254037844387076, 1.000000000000000000, 0.8660254037844387076, 1.000000000000000000, 0.8660254037844387076, 1.000000000000000000, 0.8660254037844387076, 1.000000000000000000, 0.8660254037844387076, 1.000000000000000000, 0.8660254037844387076, 1.000000000000000000, 0.8660254037844387076, 1.000000000000000000, 0.8660254037844387076, 1.000000000000000000, 0.8660254037844387076, 1.000000000000000000, 0.8660254037844387076, 1.000000000000000000, 0.8660254037844387076, 1.000000000000000000, 0.8660254037844387076, 1.000000000000000000, 0.8660254037844387076, 1.000000000000000000, 0.8660254037844387076, 1.000000000000000000, 0.8660254037844387076, 1.000000000000000000, 0.8660254037844387076, 1.000000000000000000, 0.8660254037844387076, 1.000000000000000000, 0.8660254037844387076, 1.000000000000000000, 0.8660254037844387076, 1.000000000000000000, 0.8660254037844387076, 1.000000000000000000, 0.8660254037844387076, 1.000000000000000000, 0.8660254037844387076, 1.000000000000000000, 0.8660254037844387076, 1.000000000000000000, 0.8660254037844387076, 1.000000000000000000, 0.8660254037844387076, 1.000000000000000000, 0.8660254037844387076, 1.000000000000000000, 0.8660254037844387076, 1.000000000000000000, 0.8660254037844387076, 1.000000000000000000, 0.8660254037844387076, 1.000000000000000000, 0.8660254037844387076, 1.000000000000000000, 0.8660254037844387076, 1.000000000000000000, 0.8660254037844387076, 1.000000000000000000, 0.8660254037844387076, 1.000000000000000000, 0.8660254037844387076, 1.000000000000000000, 0.8660254037844387076, 1.000000000000000000, 0.8660254037844387076, 1.000000000000000000),
 ( 1.000000000000000000, 0.8660254037844387076, 1.000000000000000000, 0.8660254037844387076, 1.000000000000000000, 0.8660254037844387076, 1.000000000000000000, 0.8660254037844387076, 1.000000000000000000, 0.8660254037844387076, 1.000000000000000000, 0.8660254037844387076, 1.000000000000000000, 0.8660254037844387076, 1.000000000000000000, 0.8660254037844387076, 1.000000000000000000, 0.8660254037844387076, 1.000000000000000000, 0.8660254037844387076, 1.000000000000000000, 0.8660254037844387076, 1.000000000000000000, 0.8660254037844387076, 1.000000000000000000, 0.8660254037844387076, 1.000000000000000000, 0.8660254037844387076, 1.000000000000000000, 0.8660254037844387076, 1.000000000000000000, 0.8660254037844387076, 1.000000000000000000, 0.8660254037844387076, 1.000000000000000000, 0.8660254037844387076, 1.000000000000000000, 0.8660254037844387076, 1.000000000000000000, 0.8660254037844387076, 1.000000000000000000, 0.8660254037844387076, 1.000000000000000000, 0.8660254037844387076, 1.000000000000000000, 0.8660254037844387076, 1.000000000000000000, 0.8660254037844387076, 1.000000000000000000, 0.8660254037844387076, 1.000000000000000000, 0.8660254037844387076, 1.000000000000000000, 0.8660254037844387076, 1.000000000000000000, 0.8660254037844387076, 1.000000000000000000, 0.8660254037844387076, 1.000000000000000000, 0.8660254037844387076, 1.000000000000000000, 0.8660254037844387076, 1.000000000000000000, 0.8660254037844387076, 1.000000000000000000, 0.8660254037844387076, 1.000000000000000000, 0.8660254037844387076, 1.000000000000000000, 0.8660254037844387076, 1.000000000000000000, 0.8660254037844387076, 1.000000000000000000, 0.8660254037844387076, 1.000000000000000000, 0.8660254037844387076, 1.000000000000000000, 0.8660254037844387076, 1.000000000000000000, 0.8660254037844387076, 1.000000000000000000, 0.8660254037844387076, 1.000000000000000000, 0.8660254037844387076, 1.000000000000000000, 0.8660254037844387076, 1.000000000000000000, 0.8660254037844387076, 1.000000000000000000, 0.8660254037844387076, 1.000000000000000000, 0.8660254037844387076, 1.000000000000000000, 0.8660254037844387076, 1.000000000000000000, 0.8660254037844387076, 1.000000000000000000, 0.8660254037844387076, 1.000000000000000000, 0.8660254037844387076, 1.000000000000000000, 0.8660254037844387076, 1.000000000000000000, 0.8660254037844387076, 1.000000000000000000, 0.8660254037844387076, 1.000000000000000000, 0.8660254037844387076, 1.000000000000000000, 0.8660254037844387076, 1.000000000000000000, 0.8660254037844387076, 1.000000000000000000, 0.8660254037844387076, 1.000000000000000000, 0.8660254037844387076, 1.000000000000000000, 0.8660254037844387076, 1.000000000000000000, 0.8660254037844387076, 1.000000000000000000, 0.8660254037844387076, 1.000000000000000000, 0.8660254037844387076, 1.000000000000000000, 0.8660254037844387076, 1.000000000000000000, 0.8660254037844387076, 1.000000000000000000, 0.8660254037844387076, 1.000000000000000000, 0.8660254037844387076, 1.000000000000000000, 0.8660254037844387076, 1.000000000000000000, 0.8660254037844387076, 1.000000000000000000, 0.8660254037844387076, 1.000000000000000000, 0.8660254037844387076, 1.000000000000000000, 0.8660254037844387076, 1.000000000000000000, 0.8660254037844387076, 1.000000000000000000, 0.8660254037844387076, 1.000000000000000000, 0.8660254037844387076, 1.000000000000000000, 0.8660254037844387076, 1.000000000000000000, 0.8660254037844387076, 1.000000000000000000, 0.8660254037844387076, 1.000000000000000000, 0.8660254037844387076, 1.000000000000000000, 0.8660254037844387076, 1.000000000000000000, 0.8660254037844387076, 1.000000000000000000, 0.8660254037844387076, 1.000000000000000000, 0.8660254037844387076, 1.000000000000000000, 0.8660254037844387076, 1.000000000000000000, 0.8660254037844387076, 1.000000000000000000, 0.8660254037844387076, 1.000000000000000000, 0.8660254037844387076, 1.000000000000000000, 0.8660254037844387076, 1.000000000000000000, 0.8660254037844387076, 1.000000000000000000, 0.8660254037844387076, 1.000000000000000000, 0.8660254037844387076, 1.000000000000000000, 0.8660254037844387076, 1.000000000000000000, 0.8660254037844387076, 1.000000000000000000, 0.8660254037844387076, 1.000000000000000000, 0.8660254037844387076, 1.000000000000000000, 0.8660254037844387076, 1.000000000000000000, 0.8660254037844387076, 1.000000000000000000, 0.8660254037844387076, 1.000000000000000000, 0.8660254037844387076, 1.000000000000000000, 0.8660254037844387076, 1.000000000000000000, 0.8660254037844387076, 1.000000000000000000, 0.8660254037844387076, 1.000000000000000000, 0.8660254037844387076, 1.000000000000000000, 0.8660254037844387076, 1.000000000000000000, 0.8660254037844387076, 1.000000000000000000, 0.8660254037844387076, 1.000000000000000000, 0.8660254037844387076, 1.000000000000000000, 0.8660254037844387076, 1.000000000000000000, 0.8660254037844387076, 1.000000000000000000, 0.8660254037844387076, 1.000000000000000000, 0.8660254037844387076, 1.000000000000000000, 0.8660254037844387076, 1.000000000000000000, 0.8660254037844387076, 1.000000000000000000, 0.8660254037844387076, 1.000000000000000000, 0.8660254037844387076, 1.000000000000000000, 0.8660254037844387076, 1.000000000000000000, 0.8660254037844387076, 1.000000000000000000, 0.8660254037844387076, 1.000000000000000000, 0.8660254037844387076, 1.000000000000000000, 0.8660254037844387076, 1.000000000000000000, 0.8660254037844387076, 1.000000000000000000) ) ) 
 REPRESENTATION_ITEM ( '' )  SURFACE ( )  );
#41857 = CARTESIAN_POINT ( 'NONE',  ( 4.235589135538409877, -1.357111243005538759, -1.430095230664797379 ) ) ;
#41858 = CARTESIAN_POINT ( 'NONE',  ( -0.1755273284492936958, -0.8636782348834280976, -1.816524446017355743 ) ) ;
#41859 = ORIENTED_EDGE ( 'NONE', *, *, #172644, .F. ) ;
#41860 = CARTESIAN_POINT ( 'NONE',  ( -0.1056256405159265443, -0.9088113327815927622, -1.910082645617340757 ) ) ;
#41861 = CARTESIAN_POINT ( 'NONE',  ( 1.715371797147913435, -1.774658612622433296, -1.066089629202723765 ) ) ;
#41862 = CARTESIAN_POINT ( 'NONE',  ( 5.169401708560450004, 9.252995436621013425, 0.000000000000000000 ) ) ;
#41863 = ORIENTED_EDGE ( 'NONE', *, *, #189117, .F. ) ;
#41864 = CARTESIAN_POINT ( 'NONE',  ( 4.369470645354133431, 8.319742529546998000, 0.7998128361456271485 ) ) ;
#41865 = CARTESIAN_POINT ( 'NONE',  ( 6.526270840131753737, 8.707344961610770540, -1.599625672291283607 ) ) ;
#41867 = CARTESIAN_POINT ( 'NONE',  ( 5.168682875307768931, 7.053215992657626110, -1.599625672291256295 ) ) ;
#41866 = CARTESIAN_POINT ( 'NONE',  ( 3.925792317461401559, 1.118293097838483074, -1.766204078809136657 ) ) ;
#41868 = CARTESIAN_POINT ( 'NONE',  ( 7.361151057576892143, 7.552707420120024828, 0.7998128361456291469 ) ) ;
#41870 = ORIENTED_EDGE ( 'NONE', *, *, #175293, .T. ) ;
#41869 = CARTESIAN_POINT ( 'NONE',  ( 0.2932429122153769052, 1.690905606409907058, -0.6502662643994570058 ) ) ;
#41871 = CARTESIAN_POINT ( 'NONE',  ( 5.830760709146560750, 2.125890151018691832, 0.5921790101122563765 ) ) ;
#41872 = CARTESIAN_POINT ( 'NONE',  ( -10.91804383151480451, 0.000000000000000000, 0.1905751639681829146 ) ) ;
#41873 = CARTESIAN_POINT ( 'NONE',  ( 4.102700518754747172, -0.6894086160392081108, -2.096397988278507096 ) ) ;
#41874 = CARTESIAN_POINT ( 'NONE',  ( 8.067265095331215718, 9.370563018429956870, 1.199719254218462483 ) ) ;
#41875 = CARTESIAN_POINT ( 'NONE',  ( -1.364683531250014514, 8.651041667008067648, -0.7879004041258335089 ) ) ;
#41876 = CARTESIAN_POINT ( 'NONE',  ( 2.719282321824310511, 1.616554633311767297, 1.021241153818429614 ) ) ;
#41877 = CARTESIAN_POINT ( 'NONE',  ( 8.127223016387999266, 11.56917838817298616, 1.199719254218460707 ) ) ;
#41878 = CARTESIAN_POINT ( 'NONE',  ( 5.564915762860970005, 1.570151797963925233, -1.349580972669261358 ) ) ;
#41880 = CARTESIAN_POINT ( 'NONE',  ( 2.747127081003514881, -1.797865629537301668, 1.199965651887124896 ) ) ;
#41879 = CARTESIAN_POINT ( 'NONE',  ( 1.506030227042737701, 8.670273769332156988, -2.548074190919165094 ) ) ;
#41881 = CARTESIAN_POINT ( 'NONE',  ( 5.671465802443460547, 1.304529079428708549, 1.760837017921567771 ) ) ;
#41882 = VERTEX_POINT ( 'NONE', #117441 ) ;
#41883 = ORIENTED_EDGE ( 'NONE', *, *, #19647, .T. ) ;
#41884 = CARTESIAN_POINT ( 'NONE',  ( 1.737499999999999378, -2.172916665710750816, -3.009438278150925683 ) ) ;
#41885 = CARTESIAN_POINT ( 'NONE',  ( -3.459282556586562585E-15, 3.603753425775780617, 11.89624657422421627 ) ) ;
#41886 = CARTESIAN_POINT ( 'NONE',  ( 4.899292406491845497, 6.809203455697518947, -1.599625672291273171 ) ) ;
#41887 = CARTESIAN_POINT ( 'NONE',  ( 3.285556943750000070, -2.471874999522040373, 0.000000000000000000 ) ) ;
#41888 = AXIS2_PLACEMENT_3D ( 'NONE', #200400, #182023, #67194 ) ;
#41889 = CARTESIAN_POINT ( 'NONE',  ( -8.378575743565381373, 8.877352577022161739, 0.7216878364870438212 ) ) ;
#41890 = CARTESIAN_POINT ( 'NONE',  ( 3.888156192069020634, 7.758209000714329839, 1.040834085586084257E-14 ) ) ;
#41891 = CARTESIAN_POINT ( 'NONE',  ( 6.192251260771239885, 1.025525066348543568, -1.798363755310352197 ) ) ;
#41892 = CARTESIAN_POINT ( 'NONE',  ( 4.090394749938445429, -1.905694808957728137, -0.2815942358586983607 ) ) ;
#41893 = CARTESIAN_POINT ( 'NONE',  ( 0.5445462702219765472, -1.458543044971000402, 1.392561646250379814 ) ) ;
#41894 = SURFACE_SIDE_STYLE ('',( #158823 ) ) ;
#41895 = CARTESIAN_POINT ( 'NONE',  ( 6.587282531393223728, 8.778525268082516320, 1.599625672291268286 ) ) ;
#41896 = CARTESIAN_POINT ( 'NONE',  ( 2.609770642201841184, 0.3830433331901660354, 0.000000000000000000 ) ) ;
#41897 = CARTESIAN_POINT ( 'NONE',  ( 0.6389542677898361056, -1.877638805159736579, 1.129783718924075364 ) ) ;
#41898 = CARTESIAN_POINT ( 'NONE',  ( 5.479063914364931343, -0.04889757770590653918, -1.825204647902956889 ) ) ;
#41899 = PRODUCT_DEFINITION_SHAPE ( 'NONE', 'NONE',  #196048 ) ;
#41900 = CARTESIAN_POINT ( 'NONE',  ( 6.265276383290871109, 7.442482214328385304, -1.082531754730548412 ) ) ;
#41901 = CARTESIAN_POINT ( 'NONE',  ( 4.677199806590210507, 4.559080650551097236, -0.7216878364870197293 ) ) ;
#41902 = CARTESIAN_POINT ( 'NONE',  ( -6.168033539574333979, 6.160736982450306876, 0.7998128361456281477 ) ) ;
#41903 = CARTESIAN_POINT ( 'NONE',  ( 4.797606254389322089, 6.690569611577942943, 1.599625672291268286 ) ) ;
#41904 = ORIENTED_EDGE ( 'NONE', *, *, #166426, .F. ) ;
#41906 = CARTESIAN_POINT ( 'NONE',  ( 5.713144883995101786, 1.643398218655172105, -1.162588118691459949 ) ) ;
#41905 = CARTESIAN_POINT ( 'NONE',  ( 2.559893532628489954, -1.268187297466142338, 1.335118840784771166 ) ) ;
#41907 = CARTESIAN_POINT ( 'NONE',  ( 0.7908558668072614983, -2.181831595417762504, 0.7228866375666581634 ) ) ;
#41908 = CARTESIAN_POINT ( 'NONE',  ( 6.227397112613878960, 0.1477489091250457076, -1.956280406615627854 ) ) ;
#41909 = CARTESIAN_POINT ( 'NONE',  ( -6.230135280679522936, 7.227244901336242755, 1.199719254218450271 ) ) ;
#41910 = CARTESIAN_POINT ( 'NONE',  ( -5.876765390786736099, 6.215699210118543760, -0.5395277504373359179 ) ) ;
#41911 = CARTESIAN_POINT ( 'NONE',  ( -3.785751206713858785, 5.439795712631356750, 1.599625672291267398 ) ) ;
#41912 = FACE_OUTER_BOUND ( 'NONE', #166768, .T. ) ;
#41913 = CARTESIAN_POINT ( 'NONE',  ( -3.637330350216213759, 7.465578851886037093, -0.7998128361456481317 ) ) ;
#41915 = CARTESIAN_POINT ( 'NONE',  ( 1.674454752297813265, -1.775319108138155633, -0.5897529795871117031 ) ) ;
#41914 = CARTESIAN_POINT ( 'NONE',  ( 2.859016124132291115, 0.3040538821531354463, -2.068378887337805949 ) ) ;
#41916 = CARTESIAN_POINT ( 'NONE',  ( 2.020861031540205133, 2.010896488828680440, -0.1455087364366919322 ) ) ;
#41917 = CARTESIAN_POINT ( 'NONE',  ( 8.107412671292031803, 11.44210330227398487, 1.082531754730557072 ) ) ;
#41918 = VERTEX_POINT ( 'NONE', #150958 ) ;
#41919 = CARTESIAN_POINT ( 'NONE',  ( -1.364683531249997417, 3.821875000341416584, 1.214306433183764966E-14 ) ) ;
#41920 = CARTESIAN_POINT ( 'NONE',  ( 2.471852389601780331, -1.665955342129191274, -0.5037381675307306406 ) ) ;
#41921 = VECTOR ( 'NONE', #47178, 1000.000000000000000 ) ;
#41922 = CARTESIAN_POINT ( 'NONE',  ( 4.449046963578762615, 8.342305224150557308, -0.7998128361456231517 ) ) ;
#41923 = DIRECTION ( 'NONE',  ( 0.000000000000000000, 0.000000000000000000, 1.000000000000000000 ) ) ;
#41924 = CARTESIAN_POINT ( 'NONE',  ( 2.736579049320194468, 0.2108767276123752754, 1.711865116355310246 ) ) ;
#41925 = CARTESIAN_POINT ( 'NONE',  ( 2.982162443640325566, -2.159563097825706990, -0.3721831821169723775 ) ) ;
#41926 = CARTESIAN_POINT ( 'NONE',  ( 5.039771180630152614, -1.558841386063321455, -1.562417271110942307 ) ) ;
#41927 = CARTESIAN_POINT ( 'NONE',  ( -11.76696981052429614, 4.673730779118267620, -4.995440715239801044 ) ) ;
#41928 = CARTESIAN_POINT ( 'NONE',  ( 2.553800759094803308, 1.675875371511101886, 1.380159786156359258 ) ) ;
#41929 = CARTESIAN_POINT ( 'NONE',  ( 1.154616158753757338, -1.440623569337009968, 1.121372061650728558 ) ) ;
#41930 = CARTESIAN_POINT ( 'NONE',  ( 3.925106927653505995, -1.840236814299311741, 1.047156446301507948 ) ) ;
#41931 = CARTESIAN_POINT ( 'NONE',  ( 6.639320575229255006, 7.629137130509086262, 2.596737603865982624 ) ) ;
#41932 = ORIENTED_EDGE ( 'NONE', *, *, #53132, .F. ) ;
#41934 = CARTESIAN_POINT ( 'NONE',  ( -1.364683531250012516, 1.092708333674754506, 0.7879004041258379498 ) ) ;
#41933 = CARTESIAN_POINT ( 'NONE',  ( 4.159948666787936844, 1.080635193647750292, 2.021704573604603095 ) ) ;
#41935 = LINE ( 'NONE', #90682, #178233 ) ;
#41936 = CARTESIAN_POINT ( 'NONE',  ( 4.487912541323413329, 5.194651705420806564, 1.199719254218462483 ) ) ;
#41937 = VECTOR ( 'NONE', #23971, 1000.000000000000000 ) ;
#41938 = CARTESIAN_POINT ( 'NONE',  ( 0.2234921222181683598, 1.847112181986635626, 1.041312259928407702 ) ) ;
#41939 = CARTESIAN_POINT ( 'NONE',  ( -5.043269954603569083, 7.867270132804026872, 1.082531754730560403 ) ) ;
#41940 = CARTESIAN_POINT ( 'NONE',  ( 4.528060117284244512, 4.385084346360807572, 0.7216878364870317197 ) ) ;
#41941 = CARTESIAN_POINT ( 'NONE',  ( -5.355107487273497391, 9.191449801886996340, 0.7216878364870458196 ) ) ;
#41942 = CARTESIAN_POINT ( 'NONE',  ( 3.716343503921665459, 6.389465617000312569, -1.082531754730549967 ) ) ;
#41943 = ORIENTED_EDGE ( 'NONE', *, *, #37763, .F. ) ;
#41944 = CARTESIAN_POINT ( 'NONE',  ( 4.570935502227962743, -0.9480417383296577682, 1.779625852769652905 ) ) ;
#41946 = CARTESIAN_POINT ( 'NONE',  ( 3.028243468416950357, 1.099549687589720826, 1.744862417660711262 ) ) ;
#41945 = CARTESIAN_POINT ( 'NONE',  ( 7.149227073107712549, 7.235186428247455837, -0.7998128361456281477 ) ) ;
#41947 = CARTESIAN_POINT ( 'NONE',  ( 4.000000000000012434, 5.499999999999998224, 0.7500000000000006661 ) ) ;
#41948 = CARTESIAN_POINT ( 'NONE',  ( 4.868786560638896255, 5.813244087901094481, 1.082531754730549078 ) ) ;
#41949 = CARTESIAN_POINT ( 'NONE',  ( 0.000000000000000000, -3.696874999522040017, -3.793834371823813001 ) ) ;
#41950 = CARTESIAN_POINT ( 'NONE',  ( -1.201851678989727383E-14, 5.696875000341416140, -1.575800808251660134 ) ) ;
#41951 = CARTESIAN_POINT ( 'NONE',  ( 6.175747540105122724, -1.175446681380667213, 1.849350104233343783 ) ) ;
#41952 = CARTESIAN_POINT ( 'NONE',  ( 3.639296212489909532, 0.7283784247123014088, 1.880435045658496618 ) ) ;
#41953 = CARTESIAN_POINT ( 'NONE',  ( 2.981803241483144351, -1.814435276338403735, -0.3121031562058202424 ) ) ;
#41954 = CARTESIAN_POINT ( 'NONE',  ( 7.820355676984174664, 8.018169799436671852, -0.7998128361456281477 ) ) ;
#41955 = CARTESIAN_POINT ( 'NONE',  ( 6.247073575888860475, -1.540555741078741825, 0.9791950884799265342 ) ) ;
#41956 = CARTESIAN_POINT ( 'NONE',  ( -5.865874016206865882, 9.995270118883347266, 0.000000000000000000 ) ) ;
#41957 = CARTESIAN_POINT ( 'NONE',  ( 0.6853298295916141480, -0.2782767918169821164, -2.245138299566074913 ) ) ;
#41958 = CARTESIAN_POINT ( 'NONE',  ( 2.086679739605776351, -2.065639965682735557, -0.4097663305358787977 ) ) ;
#41959 = CARTESIAN_POINT ( 'NONE',  ( -6.798487682609798632, 6.896266815991691779, 0.7998128361456341429 ) ) ;
#41960 = CARTESIAN_POINT ( 'NONE',  ( 8.589254009457354400, 9.979550084910457031, -1.199719254218446718 ) ) ;
#41961 = CARTESIAN_POINT ( 'NONE',  ( 5.682275777458829502, 9.643422483761748154, 0.7216878364870317197 ) ) ;
#41962 = DIRECTION ( 'NONE',  ( 0.000000000000000000, 0.000000000000000000, 1.000000000000000000 ) ) ;
#41963 = CARTESIAN_POINT ( 'NONE',  ( -5.540478329478883524, 9.615641817700700145, 0.000000000000000000 ) ) ;
#41964 = FACE_OUTER_BOUND ( 'NONE', #187378, .T. ) ;
#41965 = CARTESIAN_POINT ( 'NONE',  ( 7.904040366642695048, 9.284097184913720824, 1.082531754730558626 ) ) ;
#41966 = CARTESIAN_POINT ( 'NONE',  ( 4.420695050690802930, 7.093836324768183488, -1.099706215833176515 ) ) ;
#41967 = CARTESIAN_POINT ( 'NONE',  ( -4.680589345215810049, 6.483773540883647435, -1.599625672291256295 ) ) ;
#41969 = CARTESIAN_POINT ( 'NONE',  ( 3.639129310729662503, 2.110331241038451822, 0.6939571745526812441 ) ) ;
#41968 = CARTESIAN_POINT ( 'NONE',  ( 2.109781586379317897, 1.642293606977158538, 1.341614810521203349 ) ) ;
#41970 = CARTESIAN_POINT ( 'NONE',  ( 0.7092355107721182161, -0.3178641103029449244, 2.168156088950490723 ) ) ;
#41971 = CARTESIAN_POINT ( 'NONE',  ( 0.7509353727821498348, 0.6442623716619542140, 2.110749664216593047 ) ) ;
#41972 = CARTESIAN_POINT ( 'NONE',  ( -5.123001941117347080, 7.070197912760590064, 1.599625672291263179 ) ) ;
#41973 = CARTESIAN_POINT ( 'NONE',  ( 4.914483161888778540, 0.7490505147796695518, 1.813437088826752142 ) ) ;
#41974 = CARTESIAN_POINT ( 'NONE',  ( 8.971744963941056028, 11.49012176272984931, 1.599625672291281386 ) ) ;
#41975 = CARTESIAN_POINT ( 'NONE',  ( -5.471750928372196121, 6.276313537582185909, 1.010767274114855008 ) ) ;
#41976 = EDGE_CURVE ( 'NONE', #133576, #140589, #34594, .T. ) ;
#41977 = CARTESIAN_POINT ( 'NONE',  ( 4.234184546134326155, 3.834303480111807882, -0.3975762604357939156 ) ) ;
#41978 = CARTESIAN_POINT ( 'NONE',  ( -1.402160292154681736E-14, 0.6968750003414164729, -1.575800808251659024 ) ) ;
#41979 = CARTESIAN_POINT ( 'NONE',  ( -3.038435823238377687, 6.558942537171132514, -0.7216878364870458196 ) ) ;
#41981 = ORIENTED_EDGE ( 'NONE', *, *, #173052, .F. ) ;
#41980 = CARTESIAN_POINT ( 'NONE',  ( -5.097502569058210753, 7.930541516334467467, -1.082531754730549967 ) ) ;
#41982 = CIRCLE ( 'NONE', #121511, 1.240450515248286534 ) ;
#41983 = CARTESIAN_POINT ( 'NONE',  ( 3.920270587443940080, -2.114697630030224929, 0.1593259359235904837 ) ) ;
#41984 = CARTESIAN_POINT ( 'NONE',  ( -5.496904935697871863, 5.377753611261092637, 0.7998128361456281477 ) ) ;
#41985 = CARTESIAN_POINT ( 'NONE',  ( 5.858325616802108726, 0.8718737102157668728, 1.978260574764856283 ) ) ;
#41986 = CARTESIAN_POINT ( 'NONE',  ( 4.493604616018744835, -1.840970053361364656, -0.04044509776383875543 ) ) ;
#41987 = UNCERTAINTY_MEASURE_WITH_UNIT (LENGTH_MEASURE( 1.000000000000000082E-05 ), #14906, 'distance_accuracy_value', 'NONE');
#41988 = AXIS2_PLACEMENT_3D ( 'NONE', #79396, #29590, #160646 ) ;
#41989 = CARTESIAN_POINT ( 'NONE',  ( -5.590496338642190643, 6.198678163000841401, 0.8915474099989786350 ) ) ;
#41990 = CARTESIAN_POINT ( 'NONE',  ( 0.6823417656249899377, 1.155208333674752286, 1.181850606188755259 ) ) ;
#41991 = CARTESIAN_POINT ( 'NONE',  ( 0.2920125592734872932, 1.448600077496174476, -0.9643754397266665057 ) ) ;
#41993 = EDGE_CURVE ( 'NONE', #67541, #43310, #6835, .T. ) ;
#41992 = CARTESIAN_POINT ( 'NONE',  ( 6.827182134110231893, 2.454327069706051745, 2.294502690501096787 ) ) ;
#41994 = CARTESIAN_POINT ( 'NONE',  ( 3.877268743828276243, 4.586196958296845594, 1.082531754730560403 ) ) ;
#41995 = CARTESIAN_POINT ( 'NONE',  ( 11.84692183557065626, 6.792745295355079094, 1.971868844856123681 ) ) ;
#41996 = CARTESIAN_POINT ( 'NONE',  ( 4.592742373648754040, -0.4705147408641910944, -2.109722102427157964 ) ) ;
#41997 = EDGE_CURVE ( 'NONE', #206526, #174410, #72182, .T. ) ;
#41998 = CARTESIAN_POINT ( 'NONE',  ( 5.712267477471262289, -1.587595409608580255, -1.242535230690837489 ) ) ;
#41999 = CARTESIAN_POINT ( 'NONE',  ( -7.171900071504729191, 11.31104115015678779, -0.7216878364870267237 ) ) ;
#42000 = CARTESIAN_POINT ( 'NONE',  ( 3.573254463033649131, 0.05508235185803719847, -2.161170636208443963 ) ) ;
#42001 = CARTESIAN_POINT ( 'NONE',  ( 3.514874812717229347, 1.780701125067783108, 0.8461077801947043397 ) ) ;
#42002 = CARTESIAN_POINT ( 'NONE',  ( 0.2577194443907256383, 2.166829308800602316, -0.3276212646995610989 ) ) ;
#42003 = CARTESIAN_POINT ( 'NONE',  ( 1.079649059555651824, -0.05968906897618533880, -2.306965765669062751 ) ) ;
#42004 = CARTESIAN_POINT ( 'NONE',  ( 3.163408073613428684, 0.3057118896435347954, -2.037866251177067323 ) ) ;
#42005 = CARTESIAN_POINT ( 'NONE',  ( 5.284693219347969873, 1.710810618512406789, -0.9191280305995457311 ) ) ;
#42007 = ORIENTED_EDGE ( 'NONE', *, *, #179256, .T. ) ;
#42006 = CARTESIAN_POINT ( 'NONE',  ( -6.358410854684777291, 10.36197039720016022, -0.7216878364870267237 ) ) ;
#42008 = CARTESIAN_POINT ( 'NONE',  ( -7.144220599758281054, 7.299621885998258897, 0.7998128361456341429 ) ) ;
#42009 = CYLINDRICAL_SURFACE ( 'NONE', #22991, 2.000000000000000000 ) ;
#42011 = ORIENTED_EDGE ( 'NONE', *, *, #81569, .F. ) ;
#42010 = CARTESIAN_POINT ( 'NONE',  ( -5.191846479390389568, 5.021852078902356631, 0.7998128361456281477 ) ) ;
#42012 = CARTESIAN_POINT ( 'NONE',  ( -8.649738815394339753, 9.193709494155953621, 1.040834085586084257E-14 ) ) ;
#42013 = CARTESIAN_POINT ( 'NONE',  ( 1.905583573826599597, 1.834846665736546756, 1.225745012653912891 ) ) ;
#42014 = CARTESIAN_POINT ( 'NONE',  ( 1.001543065824772753E-15, -3.959374999522043304, 3.793834371823811669 ) ) ;
#42015 = CARTESIAN_POINT ( 'NONE',  ( 6.332860960579021814, -1.861707940517230764, -0.6185968553879470644 ) ) ;
#42016 = CARTESIAN_POINT ( 'NONE',  ( 6.539320575229258914, 2.958022083381315781, 2.556018433155104574 ) ) ;
#42017 = CARTESIAN_POINT ( 'NONE',  ( 1.499999999999990896, 4.306250000682819490, 1.214306433183764966E-14 ) ) ;
#42018 = CARTESIAN_POINT ( 'NONE',  ( 4.477916600690244664, 7.270601638097409669, -1.256879854437189969 ) ) ;
#42020 = CARTESIAN_POINT ( 'NONE',  ( -10.98194350564911659, -7.666862915010147717, 0.6300133639306291222 ) ) ;
#42019 = CARTESIAN_POINT ( 'NONE',  ( -5.994696786504495556, 7.186261032347766253, -1.212264510017725394 ) ) ;
#42021 = CARTESIAN_POINT ( 'NONE',  ( 4.910013284106277354, 1.267360923890372693, -1.335742228452965863 ) ) ;
#42022 = ORIENTED_EDGE ( 'NONE', *, *, #24501, .T. ) ;
#42023 = CARTESIAN_POINT ( 'NONE',  ( 2.413025777909239000, 1.840395853916647173, 0.9276406582674895374 ) ) ;
#42024 = CARTESIAN_POINT ( 'NONE',  ( -1.360316468750046859, 0.3697916670080757529, -0.7853790794159101196 ) ) ;
#42025 = CARTESIAN_POINT ( 'NONE',  ( -6.826694039680798021, 7.923230120171105284, -1.199719254218446718 ) ) ;
#42026 = DIRECTION ( 'NONE',  ( 0.7978120914393087570, -0.6029061840396366945, 2.113174082329822227E-15 ) ) ;
#42027 = CARTESIAN_POINT ( 'NONE',  ( 4.985647801523278133, 6.839675073242382553, -1.599625672291256295 ) ) ;
#42028 = CARTESIAN_POINT ( 'NONE',  ( 0.8837498274346058391, 1.383631269908250472, 1.527543229604712893 ) ) ;
#42030 = CARTESIAN_POINT ( 'NONE',  ( 5.249485218566787736, 1.838879873951341004, -0.09611505855997715120 ) ) ;
#42029 = LINE ( 'NONE', #108141, #159463 ) ;
#42031 = CARTESIAN_POINT ( 'NONE',  ( 6.120616281565444794, 9.228137197546649517, -1.199719254218440723 ) ) ;
#42032 = CARTESIAN_POINT ( 'NONE',  ( -4.911999630574282349, 4.728820931584174048, 0.4272946817465201885 ) ) ;
#42033 = CARTESIAN_POINT ( 'NONE',  ( -6.791708605802965870, 6.888357893050385705, -0.7998128361456362523 ) ) ;
#42035 = EDGE_LOOP ( 'NONE', ( #60899, #11888, #104877, #63561, #55660, #103365, #43012, #69389 ) ) ;
#42034 = CARTESIAN_POINT ( 'NONE',  ( -6.658747417465793461, -6.682123388833676181, -6.935047222998397487 ) ) ;
#42036 = CARTESIAN_POINT ( 'NONE',  ( 4.617920694193921705, -2.164688156338661962, 0.4286357439418769788 ) ) ;
#42037 = CARTESIAN_POINT ( 'NONE',  ( 6.919229411136463170, -0.1667645622517479609, 2.226262756130835463 ) ) ;
#42038 = CARTESIAN_POINT ( 'NONE',  ( 3.661342437515973547, 1.897110692972364454, -0.6839366698164971448 ) ) ;
#42039 = CARTESIAN_POINT ( 'NONE',  ( -6.399085315970155285, 6.567947078161039620, -0.7216878364870278340 ) ) ;
#42040 = CARTESIAN_POINT ( 'NONE',  ( -0.05268457437105152075, -1.747710896673961622, 0.7768168958157274373 ) ) ;
#42041 = CARTESIAN_POINT ( 'NONE',  ( -0.2409995289980038091, -0.004801160710915519658, -2.000252362011435636 ) ) ;
#42042 = CARTESIAN_POINT ( 'NONE',  ( 0.07536363704233395300, 5.720741966631408104, -2.738263776839637842 ) ) ;
#42043 = CARTESIAN_POINT ( 'NONE',  ( 5.988906256519172189, -1.817303134770717365, -0.5954205699960082310 ) ) ;
#42044 = CARTESIAN_POINT ( 'NONE',  ( 2.972313222866368676, 6.545497292499366182, 0.5012468031770876964 ) ) ;
#42045 = VECTOR ( 'NONE', #112957, 1000.000000000000000 ) ;
#42046 = CARTESIAN_POINT ( 'NONE',  ( 0.6197280442463182215, -0.9970892369244135356, -1.582582228963416160 ) ) ;
#42047 = CARTESIAN_POINT ( 'NONE',  ( 2.536342520008515233, 0.6839386381054488595, 1.897109991223707937 ) ) ;
#42049 = CARTESIAN_POINT ( 'NONE',  ( 3.932330475907989342, 1.126754335618613379, -1.779114833428483866 ) ) ;
#42048 = CARTESIAN_POINT ( 'NONE',  ( -9.016335848287868160, 10.47781223021269170, 1.199719254218462483 ) ) ;
#42050 = CARTESIAN_POINT ( 'NONE',  ( 8.471147050440139381, 8.777426401801974976, -0.7998128361456281477 ) ) ;
#42052 = CARTESIAN_POINT ( 'NONE',  ( -9.040589502214116280, 9.441775928871617651, 0.7998128361456462443 ) ) ;
#42051 = CARTESIAN_POINT ( 'NONE',  ( 1.499999999999987566, -0.2249999999999821587, 0.000000000000000000 ) ) ;
#42053 = CARTESIAN_POINT ( 'NONE',  ( 4.517835093568582927, -0.5347929126107499043, 1.947652422195633504 ) ) ;
#42054 = CARTESIAN_POINT ( 'NONE',  ( -1.364683531249997417, 4.259375000341424133, 1.214306433183764966E-14 ) ) ;
#42055 = CARTESIAN_POINT ( 'NONE',  ( 9.585251415181632595, 10.28514086057449184, 0.000000000000000000 ) ) ;
#42056 = EDGE_CURVE ( 'NONE', #13289, #37994, #140905, .T. ) ;
#42057 = CARTESIAN_POINT ( 'NONE',  ( 4.358765367649009903, -1.604958417591015207, 1.448176592534822005 ) ) ;
#42058 = CARTESIAN_POINT ( 'NONE',  ( 6.444921918449731280, 8.612437886315108315, 1.599625672291268286 ) ) ;
#42059 = CARTESIAN_POINT ( 'NONE',  ( 0.7499999999999902300, 5.316666666666685082, -1.299038105676658228 ) ) ;
#42060 = CARTESIAN_POINT ( 'NONE',  ( 6.367489420273535039, 7.457767740854454708, -1.199719254218452047 ) ) ;
#42061 = CARTESIAN_POINT ( 'NONE',  ( 8.771762197917315262, 10.29643932140079166, -1.082531754730543083 ) ) ;
#42063 = CARTESIAN_POINT ( 'NONE',  ( -1.813562444701080523, 2.470692551218654387, -2.500000000000000444 ) ) ;
#42062 = CARTESIAN_POINT ( 'NONE',  ( 1.434277768017662824, 1.292756205793591517, 1.744237601605197252 ) ) ;
#42065 = CARTESIAN_POINT ( 'NONE',  ( 0.9777802892061361328, -1.796362506263927017, -0.4033719513514141264 ) ) ;
#42064 = CARTESIAN_POINT ( 'NONE',  ( -6.575341312947811545, 6.773579074634973551, 1.040834085586084257E-14 ) ) ;
#42066 = CARTESIAN_POINT ( 'NONE',  ( 1.364683531249988535, 2.113541667008087099, 0.7879004041258500513 ) ) ;
#42067 = CARTESIAN_POINT ( 'NONE',  ( 3.122796855005858241, 0.05607861761174406934, 2.191015320347329709 ) ) ;
#42068 = CARTESIAN_POINT ( 'NONE',  ( 6.883263157960358924, 7.052235917045241997, 2.651962373728885325 ) ) ;
#42069 = CARTESIAN_POINT ( 'NONE',  ( 3.819400769403025198, -0.1694044215128273911, 2.256236840065691585 ) ) ;
#42070 = CARTESIAN_POINT ( 'NONE',  ( -6.398558430645608475, 9.552403038140164782, -1.199719254218440723 ) ) ;
#42071 = CARTESIAN_POINT ( 'NONE',  ( 4.557827498477605488, 1.164984774316142113, 1.645760986912048640 ) ) ;
#42072 = CARTESIAN_POINT ( 'NONE',  ( -1.364683531250012516, 4.801041667008083991, -0.7879004041258300672 ) ) ;
#42073 = CARTESIAN_POINT ( 'NONE',  ( 6.403672513108120690, 6.804938187689173468, -0.5019199613840990004 ) ) ;
#42074 = AXIS2_PLACEMENT_3D ( 'NONE', #92478, #6897, #171552 ) ;
#42075 = CARTESIAN_POINT ( 'NONE',  ( -1.500000000000001110, 12.77083333333333215, 0.8660254037844419273 ) ) ;
#42076 = CARTESIAN_POINT ( 'NONE',  ( 6.536439455564168277, 6.798469917679251573, 0.7216878364870328300 ) ) ;
#42077 = EDGE_CURVE ( 'NONE', #86477, #113056, #38260, .T. ) ;
#42078 = CARTESIAN_POINT ( 'NONE',  ( 4.428786516960594000, 0.08554295028175006033, 1.767770697671824820 ) ) ;
#42079 = CARTESIAN_POINT ( 'NONE',  ( 1.008971530259877403, 1.594680585555088292, -1.375637761830387440 ) ) ;
#42081 = CARTESIAN_POINT ( 'NONE',  ( -1.201851678989727383E-14, 1.462500000000018119, 1.732050807568877637 ) ) ;
#42080 = CARTESIAN_POINT ( 'NONE',  ( -0.6823417656250003738, 10.90104166700806765, 1.181850606188754593 ) ) ;
#42082 = CARTESIAN_POINT ( 'NONE',  ( 0.9417814284814338688, 1.320271805612409421, 1.461702747868667496 ) ) ;
#42083 = DIRECTION ( 'NONE',  ( 1.000000000000000000, -0.000000000000000000, 1.779758311459929752E-16 ) ) ;
#42084 = CARTESIAN_POINT ( 'NONE',  ( -0.4396008313320713401, 7.377972292137100929, -2.042906170116811637 ) ) ;
#42085 = ORIENTED_EDGE ( 'NONE', *, *, #67181, .F. ) ;
#42086 = CARTESIAN_POINT ( 'NONE',  ( 5.653386867218496370, 9.539442411822841805, 1.040834085586084257E-14 ) ) ;
#42087 = CIRCLE ( 'NONE', #201123, 9.479622692290801567 ) ;
#42088 = CARTESIAN_POINT ( 'NONE',  ( 9.423080456697809026, 10.95234760669099749, -1.199719254218446718 ) ) ;
#42089 = CARTESIAN_POINT ( 'NONE',  ( 5.032044620589739559, 0.9611010790777809731, -1.604743002217932313 ) ) ;
#42090 = ORIENTED_EDGE ( 'NONE', *, *, #68660, .T. ) ;
#42091 = CARTESIAN_POINT ( 'NONE',  ( 3.977443466873981759, -0.1572589350618113779, 2.064370724987254047 ) ) ;
#42092 = CARTESIAN_POINT ( 'NONE',  ( 1.224999999999991651, 2.124999999999967137, -3.469446951953614189E-14 ) ) ;
#42093 = CARTESIAN_POINT ( 'NONE',  ( -6.414416072596845986, 8.576847732820027659, -1.443375672974066548 ) ) ;
#42094 = CARTESIAN_POINT ( 'NONE',  ( 2.678940061867811195, -0.9218674704012446153, -1.992856458623322835 ) ) ;
#42095 = CARTESIAN_POINT ( 'NONE',  ( 7.553864141108259211, 11.96459193126834464, 1.040834085586084257E-14 ) ) ;
#42096 = CARTESIAN_POINT ( 'NONE',  ( -8.805130697071332335, 12.36007068230351358, 1.199719254218462483 ) ) ;
#42097 = CARTESIAN_POINT ( 'NONE',  ( 7.530627977747744062, 7.750430493652658015, -0.7998128361456341429 ) ) ;
#42098 = CARTESIAN_POINT ( 'NONE',  ( -4.911316915444452036, 4.694531097513658935, -0.3529309010900701926 ) ) ;
#42099 = EDGE_CURVE ( 'NONE', #185232, #47534, #145448, .T. ) ;
#42100 = CARTESIAN_POINT ( 'NONE',  ( -0.6823417656250246877, -1.198958332991911790, 1.181850606188755259 ) ) ;
#42101 = CARTESIAN_POINT ( 'NONE',  ( 4.193769882565239193, -1.351282707657221582, -1.422545440481419510 ) ) ;
#42102 = ADVANCED_FACE ( 'NONE', ( #206079 ), #76092, .T. ) ;
#42103 = CARTESIAN_POINT ( 'NONE',  ( 2.389999771189327937, -0.002812746694069029330, 2.016288306988550438 ) ) ;
#42104 = CARTESIAN_POINT ( 'NONE',  ( -3.284818356260900796, 7.054314858938165678, 0.7998128361456352531 ) ) ;
#42105 = CARTESIAN_POINT ( 'NONE',  ( 4.074186250656476993, 7.493853916489129574, -0.5595503573846259959 ) ) ;
#42106 = CARTESIAN_POINT ( 'NONE',  ( 1.247088714334358972, -1.471066981041386335, -1.155250539242147045 ) ) ;
#42107 = CARTESIAN_POINT ( 'NONE',  ( -1.364683531249997417, 5.259375000341425022, 1.214306433183764966E-14 ) ) ;
#42108 = CARTESIAN_POINT ( 'NONE',  ( 2.742442218595582570, 1.114876114576800248, -1.676130933394081923 ) ) ;
#42110 = CARTESIAN_POINT ( 'NONE',  ( 3.163770493730236666, 1.345063228294058000, 1.635049775249038051 ) ) ;
#42109 = CARTESIAN_POINT ( 'NONE',  ( -6.561783159334145132, 6.757761228752363181, -0.7216878364870278340 ) ) ;
#42111 = B_SPLINE_CURVE_WITH_KNOTS ( 'NONE', 3,
 ( #106912, #129589, #111188, #164144, #196637, #16788, #46142, #28807, #148949, #112256 ),
 .UNSPECIFIED., .F., .F.,
 ( 4, 2, 2, 2, 4 ),
 ( 0.000000000000000000, 0.0002299353307164190533, 0.0004598706614328381065, 0.0006898059921492572140, 0.0009197413228656762130 ),
 .UNSPECIFIED. ) ;
#42112 = CARTESIAN_POINT ( 'NONE',  ( 0.000000000000000000, -13.99999999999999822, 0.000000000000000000 ) ) ;
#42113 = CARTESIAN_POINT ( 'NONE',  ( 4.668459276380106715, -0.8822503692092443783, -1.873099891353036561 ) ) ;
#42114 = CARTESIAN_POINT ( 'NONE',  ( 7.828907357248368726, 8.098423103070084395, 0.7998128361456281477 ) ) ;
#42116 = CARTESIAN_POINT ( 'NONE',  ( 0.000000000000000000, 9.719999999999998863, 0.000000000000000000 ) ) ;
#42115 = CARTESIAN_POINT ( 'NONE',  ( 0.5387614761330473678, -1.791220285616751173, 1.078087367808887365 ) ) ;
#42118 = ORIENTED_EDGE ( 'NONE', *, *, #206271, .T. ) ;
#42117 = CARTESIAN_POINT ( 'NONE',  ( 5.297797529045338294, -0.6555159417414997414, 1.704002486358429325 ) ) ;
#42119 = CARTESIAN_POINT ( 'NONE',  ( 7.052212457402625922, 11.37933163361175382, -0.7998128361456291469 ) ) ;
#42120 = DIRECTION ( 'NONE',  ( 0.7592566023652996821, 0.6507913734559648278, 0.000000000000000000 ) ) ;
#42121 = CARTESIAN_POINT ( 'NONE',  ( 5.816084710138182068, 5.887779704690343507, -0.7216878364870008555 ) ) ;
#42122 = CARTESIAN_POINT ( 'NONE',  ( -10.80846816847880909, 4.295462489797631456, 4.678010962757586100 ) ) ;
#42123 = CARTESIAN_POINT ( 'NONE',  ( -1.364683531250010740, 11.94270833367473017, 0.7879004041258445001 ) ) ;
#42124 = CARTESIAN_POINT ( 'NONE',  ( 6.164708882046985750, 0.6044385376218417427, 1.814302210532907411 ) ) ;
#42125 = CARTESIAN_POINT ( 'NONE',  ( -7.808606406466886973, 11.19745900993164511, 1.199719254218453823 ) ) ;
#42126 = CARTESIAN_POINT ( 'NONE',  ( 5.524057522564145728, 8.532151978711786100, 1.199719254218462483 ) ) ;
#42127 = AXIS2_PLACEMENT_3D ( 'NONE', #22930, #26151, #159358 ) ;
#42128 = CARTESIAN_POINT ( 'NONE',  ( -11.89317557362582534, 11.26275843837606061, -1.599935658896117774 ) ) ;
#42129 = CARTESIAN_POINT ( 'NONE',  ( 4.175548122884573665, 3.973820352894515295, 1.214306433183764966E-14 ) ) ;
#42130 = CARTESIAN_POINT ( 'NONE',  ( -3.469446951953614189E-15, 8.999999999999998224, -0.7749999999999996891 ) ) ;
#42131 = CARTESIAN_POINT ( 'NONE',  ( 3.876741858503734761, 6.610283703974623393, 1.199719254218462483 ) ) ;
#42132 = ORIENTED_EDGE ( 'NONE', *, *, #177985, .T. ) ;
#42133 = CARTESIAN_POINT ( 'NONE',  ( -7.273023059088104425, 7.449891421883056530, 0.000000000000000000 ) ) ;
#42134 = CARTESIAN_POINT ( 'NONE',  ( 5.185172808627552143, 1.650094130669476522, 1.158673036085342112 ) ) ;
#42135 = CARTESIAN_POINT ( 'NONE',  ( -0.04277205541327071259, -9.414847940711862151, -9.500256024741366545 ) ) ;
#42136 = CARTESIAN_POINT ( 'NONE',  ( -6.470902446588409518, 6.777469385738574381, 0.2989120342885512871 ) ) ;
#42137 = CARTESIAN_POINT ( 'NONE',  ( -6.399085315970155285, 6.567947078161039620, -0.7216878364870278340 ) ) ;
#42138 = CARTESIAN_POINT ( 'NONE',  ( 8.270110514656016321, 12.59228666716665401, 0.7216878364870438212 ) ) ;
#42139 = CARTESIAN_POINT ( 'NONE',  ( 1.920693274676561924, -1.396391452584997417, 1.389085034315578060 ) ) ;
#42140 = CARTESIAN_POINT ( 'NONE',  ( 2.847279977023515318, 0.2930488483154705670, -1.994874153863256172 ) ) ;
#42141 = CARTESIAN_POINT ( 'NONE',  ( -5.859094939400033120, 9.987361195942037639, -0.7998128361456231517 ) ) ;
#42142 = CARTESIAN_POINT ( 'NONE',  ( 6.727182134110196721, 7.629137130509074716, 2.689055895399253160 ) ) ;
#42143 = CARTESIAN_POINT ( 'NONE',  ( 3.925867417771063739, 1.172880473742785812, -1.850976771919823793 ) ) ;
#42144 = LINE ( 'NONE', #159070, #32879 ) ;
#42145 = CARTESIAN_POINT ( 'NONE',  ( 2.450113916266524416, 1.925923877722035105, 0.04935297016485720029 ) ) ;
#42146 = CARTESIAN_POINT ( 'NONE',  ( -8.025536864285518490, 11.45054454405341282, -1.199719254218446718 ) ) ;
#42147 =( LENGTH_UNIT ( ) NAMED_UNIT ( * ) SI_UNIT ( .MILLI., .METRE. ) );
#42148 = CARTESIAN_POINT ( 'NONE',  ( 0.1333542156527530165, 6.948072531064762636, -2.641009269961028139 ) ) ;
#42149 = DIRECTION ( 'NONE',  ( 0.000000000000000000, 0.000000000000000000, -1.000000000000000000 ) ) ;
#42150 = CARTESIAN_POINT ( 'NONE',  ( 7.527801604085637699, 9.805521176231838609, 1.599625672291281386 ) ) ;
#42151 = CARTESIAN_POINT ( 'NONE',  ( 4.822949958159288286, 6.649860922651058992, -1.599625672291256295 ) ) ;
#42152 = CARTESIAN_POINT ( 'NONE',  ( -2.440293211016301606E-15, 1.312499999999991118, 1.224999999999973888 ) ) ;
#42153 = CARTESIAN_POINT ( 'NONE',  ( 5.722950238744200391, 7.770137593325314285, 1.443375672974065660 ) ) ;
#42154 = ORIENTED_EDGE ( 'NONE', *, *, #23613, .F. ) ;
#42156 = CARTESIAN_POINT ( 'NONE',  ( 3.176434313366371942, 0.9072602101105414762, 1.797144717478225795 ) ) ;
#42155 = CARTESIAN_POINT ( 'NONE',  ( 5.864778394761136049, 0.1288883805774850844, -1.836796581567698539 ) ) ;
#42157 = CARTESIAN_POINT ( 'NONE',  ( 4.042538402956846966, 2.165829419810465950, -0.7696314825454602104 ) ) ;
#42159 = CARTESIAN_POINT ( 'NONE',  ( 3.027998222813840901, 0.9912708380838133326, 1.574746995948882455 ) ) ;
#42158 = CARTESIAN_POINT ( 'NONE',  ( -0.1288028175206907822, 7.629137130509059617, -2.873994896247424435 ) ) ;
#42160 = CARTESIAN_POINT ( 'NONE',  ( -3.285556943750000070, -1.159374999522042815, 0.000000000000000000 ) ) ;
#42161 = CARTESIAN_POINT ( 'NONE',  ( 8.881784197001254049E-17, 3.500000000000000888, -1.600000000000005196 ) ) ;
#42162 = CARTESIAN_POINT ( 'NONE',  ( 6.451426615364327155, -1.705040744490589066, 0.8662930942644477827 ) ) ;
#42163 = CARTESIAN_POINT ( 'NONE',  ( -6.995117189646935962, 10.24838825697502109, 1.199719254218453823 ) ) ;
#42164 = CARTESIAN_POINT ( 'NONE',  ( -3.851925040058333582, 7.508013290127760087, -0.7216878364870458196 ) ) ;
#42165 = CARTESIAN_POINT ( 'NONE',  ( 5.987849877204276083, -2.080749957983673681, -0.2039560948884494573 ) ) ;
#42166 = CARTESIAN_POINT ( 'NONE',  ( 6.263503779833467178, 9.290876262238963790, -1.082531754730537088 ) ) ;
#42167 = EDGE_LOOP ( 'NONE', ( #178880, #79817, #34951, #157819 ) ) ;
#42168 = CARTESIAN_POINT ( 'NONE',  ( -1.500000000000077494, 7.388542872122511262, 4.154462424328213110 ) ) ;
#42170 = CARTESIAN_POINT ( 'NONE',  ( 5.379888026524302980, 5.170957540566797128, -0.7998128361456211532 ) ) ;
#42169 = CARTESIAN_POINT ( 'NONE',  ( 4.778146133183440725, 8.258034039491356282, 0.8222960688244035365 ) ) ;
#42171 = CARTESIAN_POINT ( 'NONE',  ( 6.516207646108923335, -0.8203346053292108753, -1.517322292280029350 ) ) ;
#42172 = CARTESIAN_POINT ( 'NONE',  ( -5.759516327706961647, 5.613857225279885732, -0.7998128361456221525 ) ) ;
#42173 = CARTESIAN_POINT ( 'NONE',  ( 1.107607643408299314, -0.04344470770747606292, 1.733769432050970449 ) ) ;
#42174 = DIRECTION ( 'NONE',  ( -0.9782075119097244364, 0.1245777785627091433, -0.1661037047502772757 ) ) ;
#42175 = EDGE_CURVE ( 'NONE', #75662, #126440, #166550, .T. ) ;
#42176 = CARTESIAN_POINT ( 'NONE',  ( 3.188928480291414846, 8.980740528189164351, -2.451733079074511767 ) ) ;
#42177 = CARTESIAN_POINT ( 'NONE',  ( 6.280164127638760085, -1.199209930833704085, -1.809645864181265384 ) ) ;
#42178 = CARTESIAN_POINT ( 'NONE',  ( 4.353998665852670591, 1.825246345946249571, -0.04724550102237072557 ) ) ;
#42179 = CARTESIAN_POINT ( 'NONE',  ( 2.658977320520792720, 1.578554556127611530, -1.164590279592196298 ) ) ;
#42180 = DIRECTION ( 'NONE',  ( -1.000000000000000000, 0.000000000000000000, 0.000000000000000000 ) ) ;
#42181 = CARTESIAN_POINT ( 'NONE',  ( 0.000000000000000000, 0.000000000000000000, 9.579665964948883783 ) ) ;
#42182 = CARTESIAN_POINT ( 'NONE',  ( 8.751951852821344247, 10.16936423550178503, -1.199719254218446718 ) ) ;
#42183 = CARTESIAN_POINT ( 'NONE',  ( 3.932379033323248230, -1.091282289853046317, -1.817994770353311473 ) ) ;
#42184 = CARTESIAN_POINT ( 'NONE',  ( 9.348761378620915607, 13.52553930298125096, -7.449808453853658641 ) ) ;
#42185 = CARTESIAN_POINT ( 'NONE',  ( 4.207966135563057541, 7.175396087857926375, 1.156120096431498379 ) ) ;
#42186 =( GEOMETRIC_REPRESENTATION_CONTEXT ( 3 ) GLOBAL_UNCERTAINTY_ASSIGNED_CONTEXT ( ( #120879 ) ) GLOBAL_UNIT_ASSIGNED_CONTEXT ( ( #10082, #148366, #173690 ) ) REPRESENTATION_CONTEXT ( 'NONE', 'WORKASPACE' ) );
#42187 = CARTESIAN_POINT ( 'NONE',  ( -4.684235067853224521, 6.877467941869524815, -1.224209591347114046 ) ) ;
#42188 = CARTESIAN_POINT ( 'NONE',  ( 1.200149190772631158, 0.8425179731405306738, -1.891261800508976298 ) ) ;
#42190 = CARTESIAN_POINT ( 'NONE',  ( -1.500000000000015099, 14.76041666734946567, -0.8660254037844309360 ) ) ;
#42189 = CARTESIAN_POINT ( 'NONE',  ( -9.912081330994999107, 3.481540842592264706, 6.783330821352332229 ) ) ;
#42192 = ORIENTED_EDGE ( 'NONE', *, *, #47373, .F. ) ;
#42191 = CARTESIAN_POINT ( 'NONE',  ( 3.862163208519187929, 0.7476031731964963845, -2.091851990882629408 ) ) ;
#42193 = CARTESIAN_POINT ( 'NONE',  ( 2.004881263662112723, -2.228613174808518060, 0.5628491883087839431 ) ) ;
#42195 = CARTESIAN_POINT ( 'NONE',  ( 6.789892339975323488, -1.342670783288713698, -1.565829586757736758 ) ) ;
#42194 = CARTESIAN_POINT ( 'NONE',  ( 9.246297574839974942, 11.81043314211192019, 1.443375672974076540 ) ) ;
#42197 = CARTESIAN_POINT ( 'NONE',  ( 3.475000000000000533, -0.1458333333333326765, -2.006292185433951047 ) ) ;
#42196 = CARTESIAN_POINT ( 'NONE',  ( 3.718679271898170491, 7.560485927181699317, 0.7998128361456271485 ) ) ;
#42198 = LINE ( 'NONE', #125642, #9426 ) ;
#42199 = DIRECTION ( 'NONE',  ( 0.04267330865764933784, 4.780913106218958965E-15, 0.9990890794760041160 ) ) ;
#42200 = CARTESIAN_POINT ( 'NONE',  ( -9.578206935409053102, -9.746166700193986898, 0.1671882239534360770 ) ) ;
#42201 = CARTESIAN_POINT ( 'NONE',  ( -0.2106725631050020975, 5.721452923065615259, -2.597767226077936087 ) ) ;
#42202 = CARTESIAN_POINT ( 'NONE',  ( 2.572937677043420912, 0.08726698667262809683, -1.722694834735357894 ) ) ;
#42203 = CARTESIAN_POINT ( 'NONE',  ( 2.184780103950241248, 1.616692242240840960, -1.205043568535242304 ) ) ;
#42204 = CARTESIAN_POINT ( 'NONE',  ( 3.075713870353123713, 2.149355976742998831, -0.7065000242163150812 ) ) ;
#42205 = CARTESIAN_POINT ( 'NONE',  ( 5.092451870646586443, -2.090052423365583500, -0.2586305528886819194 ) ) ;
#42206 = CARTESIAN_POINT ( 'NONE',  ( -5.966997003790228682, 8.054858819212300958, -1.443375672974066548 ) ) ;
#42207 = CARTESIAN_POINT ( 'NONE',  ( 3.901397652722672582, -0.5159380698404272270, 1.692823668428977912 ) ) ;
#42209 = CARTESIAN_POINT ( 'NONE',  ( -0.02880301295727759683, -0.006976478922920535501, -2.273770288744044521 ) ) ;
#42208 = CARTESIAN_POINT ( 'NONE',  ( 3.567203813726958828, 6.215469311773181182, 1.082531754730549078 ) ) ;
#42210 = CARTESIAN_POINT ( 'NONE',  ( 5.437399513225577685, 0.7426265630364609072, -1.684910612069365321 ) ) ;
#42211 = CARTESIAN_POINT ( 'NONE',  ( -2.611917148927046295, 6.198987107056845858, 1.040834085586084257E-14 ) ) ;
#42212 = CARTESIAN_POINT ( 'NONE',  ( 6.439759776366780208, 6.615400615290456088, 0.7216878364870317197 ) ) ;
#42213 = CARTESIAN_POINT ( 'NONE',  ( -1.500000000000013101, 3.879166666666685970, -0.8660254037844313801 ) ) ;
#42214 = COLOUR_RGB ( '', 0.40784314, 0.44705882, 0.49803922) ;
#42215 = CARTESIAN_POINT ( 'NONE',  ( 5.085950966588184130, -2.174626929279792176, -0.2704268894557353975 ) ) ;
#42216 = DIRECTION ( 'NONE',  ( -0.6507913734559641616, -0.7592566023653004592, 0.000000000000000000 ) ) ;
#42217 = CARTESIAN_POINT ( 'NONE',  ( -5.973546839618155246, 15.51882391377835368, 10.41731636723813814 ) ) ;
#42218 = CARTESIAN_POINT ( 'NONE',  ( 5.441872305809390298, 1.387781221417656141, 1.536568222347669987 ) ) ;
#42219 = DIRECTION ( 'NONE',  ( 0.000000000000000000, -1.000000000000000000, 0.000000000000000000 ) ) ;
#42220 = CARTESIAN_POINT ( 'NONE',  ( -0.6823417656250212460, 4.051041667008085767, 1.181850606188767472 ) ) ;
#42221 = CARTESIAN_POINT ( 'NONE',  ( 3.229043484313653511, 0.04796440165338172745, 1.926065231962639679 ) ) ;
#42222 = CARTESIAN_POINT ( 'NONE',  ( 1.364683531249996529, 9.963541667008065872, 0.7879004041258405033 ) ) ;
#42223 = CARTESIAN_POINT ( 'NONE',  ( -3.389175213736311587, 4.977123720824209840, 1.443375672974064550 ) ) ;
#42224 = CARTESIAN_POINT ( 'NONE',  ( 6.398696098476772676, -2.079943653215409416, -0.4123558718646391785 ) ) ;
#42225 = ORIENTED_EDGE ( 'NONE', *, *, #22536, .T. ) ;
#42227 = SURFACE_STYLE_USAGE ( .BOTH. , #109416 ) ;
#42226 = DIRECTION ( 'NONE',  ( 0.3281536732072464768, 0.000000000000000000, 0.9446243521954066358 ) ) ;
#42228 = CARTESIAN_POINT ( 'NONE',  ( 5.040934186182656873, 4.775511393501539636, 1.040834085586084257E-14 ) ) ;
#42229 = CARTESIAN_POINT ( 'NONE',  ( 5.682275777458851707, 6.762314840857718501, 1.082531754730549078 ) ) ;
#42230 = DIRECTION ( 'NONE',  ( 1.276756478318932585E-15, -1.000000000000000000, 1.665334536937738262E-16 ) ) ;
#42231 = DIRECTION ( 'NONE',  ( 0.000000000000000000, 0.000000000000000000, 1.000000000000000000 ) ) ;
#42232 = CARTESIAN_POINT ( 'NONE',  ( 9.286972035236624734, 11.85788667924133399, -1.443375672974058777 ) ) ;
#42234 = EDGE_CURVE ( 'NONE', #182554, #210172, #73727, .T. ) ;
#42233 = CARTESIAN_POINT ( 'NONE',  ( 0.8538673084422104820, -0.7095216264049221122, 1.829241926910141203 ) ) ;
#42235 = CARTESIAN_POINT ( 'NONE',  ( -0.6823417656250003738, 1.780208333674752952, -1.181850606188749264 ) ) ;
#42236 = CARTESIAN_POINT ( 'NONE',  ( -1.499999999999997780, 3.650000000000021227, 1.214306433183764966E-14 ) ) ;
#42237 = ADVANCED_FACE ( 'NONE', ( #88077 ), #75029, .T. ) ;
#42238 = CARTESIAN_POINT ( 'NONE',  ( 5.758247127753066685, -1.962046631956643195, -0.001586170976335121285 ) ) ;
#42239 = CARTESIAN_POINT ( 'NONE',  ( -8.025536864285518490, 11.45054454405341282, -1.199719254218446718 ) ) ;
#42240 = CARTESIAN_POINT ( 'NONE',  ( -4.568734577680875653, 8.274014740695587733, -0.7216878364870257245 ) ) ;
#42241 = CARTESIAN_POINT ( 'NONE',  ( 0.5325469457231490900, 1.160272198634606955, -1.942242498246045113 ) ) ;
#42243 = EDGE_LOOP ( 'NONE', ( #64766, #78974, #23402, #207936 ) ) ;
#42242 = LINE ( 'NONE', #74722, #191702 ) ;
#42244 = CARTESIAN_POINT ( 'NONE',  ( 0.6823417656249899377, 5.176041667008086655, -1.181850606188754593 ) ) ;
#42245 = CARTESIAN_POINT ( 'NONE',  ( 0.5087955169046609605, 1.624258005607306599, 0.9276666955444978768 ) ) ;
#42246 = CARTESIAN_POINT ( 'NONE',  ( 5.676976676600826721, -0.7816020568793962120, -1.547713907698013092 ) ) ;
#42248 = CARTESIAN_POINT ( 'NONE',  ( 3.298540952264991777, 1.726358142885858316, -1.349911518210664241 ) ) ;
#42247 = CARTESIAN_POINT ( 'NONE',  ( -1.360316468750054852, 0.9114583336747262843, 0.7853790794158720390 ) ) ;
#42249 = CARTESIAN_POINT ( 'NONE',  ( 4.999205796216253717, 1.921780780153565793, -1.277121366954391934 ) ) ;
#42250 = CARTESIAN_POINT ( 'NONE',  ( 6.573517591324530507, 1.973370851288195338, -0.5938938365465350477 ) ) ;
#42251 = CARTESIAN_POINT ( 'NONE',  ( 2.044773883198697462, -1.559800846558807130, -1.156617037343915966 ) ) ;
#42252 = CARTESIAN_POINT ( 'NONE',  ( -4.568734577680880093, 7.313645526394248364, -1.082531754730548412 ) ) ;
#42253 = CARTESIAN_POINT ( 'NONE',  ( -1.471045507628332367E-16, 2.000000000000001776, 2.650000000000008349 ) ) ;
#42255 = ADVANCED_FACE ( 'NONE', ( #107596 ), #12534, .T. ) ;
#42254 = CARTESIAN_POINT ( 'NONE',  ( 5.344028447597857223, -1.346983732444573256, -1.637812552581649594 ) ) ;
#42256 = FACE_OUTER_BOUND ( 'NONE', #73332, .T. ) ;
#42257 = CARTESIAN_POINT ( 'NONE',  ( 3.568982563115063567, -0.9913999084223242830, 1.755768870528086056 ) ) ;
#42258 = CARTESIAN_POINT ( 'NONE',  ( -4.731432421044877934, 6.543090462684225450, -1.443375672974051449 ) ) ;
#42259 = CARTESIAN_POINT ( 'NONE',  ( -6.149505192250180663, 9.332117270003974951, -1.199719254218452047 ) ) ;
#42260 = CARTESIAN_POINT ( 'NONE',  ( 9.642873567817520808, 12.27310513391906532, 1.599625672291279388 ) ) ;
#42261 = CARTESIAN_POINT ( 'NONE',  ( 1.541335573940459058, -1.321205422867760548, -1.260230113935792318 ) ) ;
#42262 = CARTESIAN_POINT ( 'NONE',  ( -5.611095471209320174, 7.639640364534566075, 1.599625672291263179 ) ) ;
#42263 = CARTESIAN_POINT ( 'NONE',  ( -5.224688093219837626, 7.188831756880171397, -1.599625672291271394 ) ) ;
#42264 = CARTESIAN_POINT ( 'NONE',  ( -5.032163277954181169, 7.944720250727295152, 1.129701600186810095 ) ) ;
#42265 = VERTEX_POINT ( 'NONE', #41485 ) ;
#42266 = CARTESIAN_POINT ( 'NONE',  ( 5.295800851330623615, -0.7439313745516599186, 1.922114966912706224 ) ) ;
#42267 = CARTESIAN_POINT ( 'NONE',  ( -6.739811759324828344, 8.956476034002674780, -1.443375672974066548 ) ) ;
#42268 = UNCERTAINTY_MEASURE_WITH_UNIT (LENGTH_MEASURE( 1.000000000000000082E-05 ), #55053, 'distance_accuracy_value', 'NONE');
#42269 = CARTESIAN_POINT ( 'NONE',  ( -4.416205349749324327, 6.175325546172740765, 1.599625672291267398 ) ) ;
#42270 = CARTESIAN_POINT ( 'NONE',  ( -5.327428015527048366, 5.180030537728460338, -0.7998128361456362523 ) ) ;
#42271 = CARTESIAN_POINT ( 'NONE',  ( 4.160810511097835729, 0.5408905907967902493, 1.945810383981197544 ) ) ;
#42272 = CARTESIAN_POINT ( 'NONE',  ( 5.391355351084783365, -0.05288786341082692827, -2.220837934544753089 ) ) ;
#42274 = CARTESIAN_POINT ( 'NONE',  ( 10.05978679165993839, 10.83876546646586014, 0.7216878364870438212 ) ) ;
#42273 = CARTESIAN_POINT ( 'NONE',  ( -7.533490631048818109, 8.818102486758951031, -1.199719254218452047 ) ) ;
#42275 = CARTESIAN_POINT ( 'NONE',  ( 4.496500501226593727, 8.397667684739696270, 0.7998128361456462443 ) ) ;
#42276 = CARTESIAN_POINT ( 'NONE',  ( 4.293860741714614626, -0.7905101867788848491, 1.903454510683154188 ) ) ;
#42277 = CARTESIAN_POINT ( 'NONE',  ( 4.149064681782777875, 0.9530105817698063531, 1.777011888912001014 ) ) ;
#42278 = VERTEX_POINT ( 'NONE', #173627 ) ;
#42279 =( BOUNDED_CURVE ( )  B_SPLINE_CURVE ( 3, ( #113110, #193219, #176977, #31802 ),
 .UNSPECIFIED., .F., .T. ) 
 B_SPLINE_CURVE_WITH_KNOTS ( ( 4, 4 ),
 ( 1.683648326080136037, 1.706346174174820041 ),
 .UNSPECIFIED. ) 
 CURVE ( )  GEOMETRIC_REPRESENTATION_ITEM ( )  RATIONAL_B_SPLINE_CURVE ( ( 1.000000000000000000, 0.9999570677684579412, 0.9999570677684579412, 1.000000000000000000 ) ) 
 REPRESENTATION_ITEM ( '' )  );
#42280 = CARTESIAN_POINT ( 'NONE',  ( 1.911686719268467005, 3.274494700676901182, -0.4236673858377861812 ) ) ;
#42281 = CARTESIAN_POINT ( 'NONE',  ( 3.357615597678655917, 7.068968630600412695, 0.7998128361456321445 ) ) ;
#42282 = MECHANICAL_DESIGN_GEOMETRIC_PRESENTATION_REPRESENTATION (  '', ( #156377 ), #153115 ) ;
#42284 = ORIENTED_EDGE ( 'NONE', *, *, #18887, .T. ) ;
#42283 = CARTESIAN_POINT ( 'NONE',  ( 1.419999999999989049, 6.200000000000045475, -2.873333333333328632 ) ) ;
#42285 = CARTESIAN_POINT ( 'NONE',  ( 4.754190777897029818, 8.299541367957775861, -0.7767638722561143183 ) ) ;
#42286 = CARTESIAN_POINT ( 'NONE',  ( 3.989611116449209405, 1.913510565032714883, 0.6351021849077125303 ) ) ;
#42287 = CARTESIAN_POINT ( 'NONE',  ( 2.150122221082468865, -1.423577340559305071, 1.167554138749151926 ) ) ;
#42288 = COLOUR_RGB ( '', 0.40784314, 0.44705882, 0.49803922) ;
#42289 = CARTESIAN_POINT ( 'NONE',  ( 1.401454987343775382, 1.884297621475890416, -1.332007787593261883 ) ) ;
#42290 = CARTESIAN_POINT ( 'NONE',  ( 5.273195401072370281, 5.116759154198018855, -0.7998128361456481317 ) ) ;
#42291 = CARTESIAN_POINT ( 'NONE',  ( 4.042369558984196587, 2.150769235480045616, 0.2162802025119994753 ) ) ;
#42292 = CARTESIAN_POINT ( 'NONE',  ( -4.876128802409253282, 8.840567369452784874, 0.7998128361456481317 ) ) ;
#42293 = CARTESIAN_POINT ( 'NONE',  ( 3.234050759648151363, -2.122446487128562875, -0.8823414489649589187 ) ) ;
#42294 = ORIENTED_EDGE ( 'NONE', *, *, #126911, .F. ) ;
#42295 = CARTESIAN_POINT ( 'NONE',  ( 3.486133158594716510E-16, 2.437499999999986677, -1.225000000000021849 ) ) ;
#42296 = CARTESIAN_POINT ( 'NONE',  ( 1.305301652190330675, -0.4579020413679709689, 1.813615928118620380 ) ) ;
#42297 = CARTESIAN_POINT ( 'NONE',  ( 5.172717120832922788, -1.856099020970953806, -0.6648386725634397587 ) ) ;
#42299 = CARTESIAN_POINT ( 'NONE',  ( 8.961576348508637935, 11.47825837805867799, -1.443375672974052559 ) ) ;
#42298 = CARTESIAN_POINT ( 'NONE',  ( 1.364683531249990311, 4.613541667008083103, 0.7879004041258500513 ) ) ;
#42301 = CARTESIAN_POINT ( 'NONE',  ( 0.6278963055918493907, -2.094311335337955882, 0.6960538111202837497 ) ) ;
#42300 = CARTESIAN_POINT ( 'NONE',  ( -5.870844209917351009, 6.808071985447069707, -1.199719254218446718 ) ) ;
#42302 = CARTESIAN_POINT ( 'NONE',  ( -1.426714497269032655, 7.396188545894244015, -4.272650097712488382 ) ) ;
#42303 = CARTESIAN_POINT ( 'NONE',  ( 3.683011284406639607, 7.448596931783069586, 0.7998128361456321445 ) ) ;
#42304 = CARTESIAN_POINT ( 'NONE',  ( -4.238895582566952314, 8.097128612970093897, 1.040834085586084257E-14 ) ) ;
#42305 = CARTESIAN_POINT ( 'NONE',  ( 6.639320575229294086, -0.003630812595115453199, 2.203388474976493594 ) ) ;
#42306 = CARTESIAN_POINT ( 'NONE',  ( 4.785985848584410896, -0.9303070431277806751, 1.738173387191404684 ) ) ;
#42307 = CARTESIAN_POINT ( 'NONE',  ( 5.654963871297442601, -1.822634436652656342, 1.415334302069543027 ) ) ;
#42308 = CARTESIAN_POINT ( 'NONE',  ( 5.705462897529653965, -1.467230705000615032, -1.144726319735862585 ) ) ;
#42309 = CARTESIAN_POINT ( 'NONE',  ( 3.274340622259350742, -1.012630945124261661, -1.796778529651460898 ) ) ;
#42310 = CARTESIAN_POINT ( 'NONE',  ( 6.561783159334121152, 8.678499657355050800, -1.443375672974057666 ) ) ;
#42311 = EDGE_CURVE ( 'NONE', #195242, #136958, #190892, .T. ) ;
#42312 = CARTESIAN_POINT ( 'NONE',  ( 5.982890925380405456, 10.20206618957764100, 0.000000000000000000 ) ) ;
#42313 = CARTESIAN_POINT ( 'NONE',  ( 6.548225005276093746, 9.623051025255367819, -1.082531754730537976 ) ) ;
#42314 = CARTESIAN_POINT ( 'NONE',  ( 1.364683531249990311, 3.196875000341416140, 1.214306433183764966E-14 ) ) ;
#42315 = CARTESIAN_POINT ( 'NONE',  ( 0.05503291520805564385, -6.406027784105803313, -11.00000000000011902 ) ) ;
#42316 = CARTESIAN_POINT ( 'NONE',  ( 6.439759776366780208, 6.615400615290456088, 0.7216878364870317197 ) ) ;
#42317 = CARTESIAN_POINT ( 'NONE',  ( 5.037629062015871462, 2.027634951229041693, -0.7768168075839574360 ) ) ;
#42318 = CARTESIAN_POINT ( 'NONE',  ( 0.4170821662628897974, 3.033599471985628959, -0.4170821662629418114 ) ) ;
#42320 = CARTESIAN_POINT ( 'NONE',  ( 4.229911503591711863, 1.806553461410321582, 0.3548724298726435022 ) ) ;
#42319 = FACE_OUTER_BOUND ( 'NONE', #55148, .T. ) ;
#42321 = CARTESIAN_POINT ( 'NONE',  ( -0.6823417656250212460, 5.551041667008087543, 1.181850606188767472 ) ) ;
#42322 = CARTESIAN_POINT ( 'NONE',  ( 6.356982542327763497, 0.3766756592470664744, -2.158781491689326426 ) ) ;
#42323 = DIRECTION ( 'NONE',  ( -0.7592566023653004592, -0.6507913734559639396, -0.000000000000000000 ) ) ;
#42324 = CARTESIAN_POINT ( 'NONE',  ( 0.4743659920835150978, 1.303974419552447639, 1.848657746038349092 ) ) ;
#42325 = CARTESIAN_POINT ( 'NONE',  ( -4.022959435666734862, 7.784601250164370434, 0.4788606935734913694 ) ) ;
#42326 = DIRECTION ( 'NONE',  ( 1.000000000000000000, 0.000000000000000000, 0.000000000000000000 ) ) ;
#42327 = CARTESIAN_POINT ( 'NONE',  ( 5.820234798683411981, 7.319712794923219690, 1.284739950006764220 ) ) ;
#42328 = AXIS2_PLACEMENT_3D ( 'NONE', #2086, #167823, #54079 ) ;
#42329 = CARTESIAN_POINT ( 'NONE',  ( -3.485854892044994102, 7.080931450778859215, -0.7216878364870458196 ) ) ;
#42330 = CARTESIAN_POINT ( 'NONE',  ( 1.499999999999821032, 7.388542872122531691, -4.154462424328212222 ) ) ;
#42331 = CARTESIAN_POINT ( 'NONE',  ( 0.3030915354301273457, -0.4787081777068747934, 1.703804975073195394 ) ) ;
#42332 =( BOUNDED_SURFACE ( )  B_SPLINE_SURFACE ( 1, 2, ( 
 ( #108807, #174830, #26409, #59982, #208351, #126135, #192097, #11218, #175888, #27479, #93579, #143412, #139113, #106654, #209406, #61053, #127212, #172681, #81564, #182251, #79435, #98895, #148707, #113077, #196392, #129349, #277, #48035, #96786, #114149, #66349, #147650, #132493, #78363, #210490, #128286, #194248, #201686, #36003, #117329, #119464, #2415, #84765, #86902, #67413, #53331, #107213, #4543, #124555, #101005, #73574, #102084, #69553, #169214, #166018, #183327, #19752, #205698, #85833, #167094, #184384, #185452, #37074, #168153, #20805, #151911, #156981, #200622, #150851, #139675, #173235, #52271, #90917, #118398, #34933, #199563, #152969, #57333, #123497, #189461, #206766, #41104, #1352, #8570, #74650, #42170, #58400, #17604, #149776, #190513, #83688, #133554, #51207, #183866, #33349, #130924, #182795, #180668, #35481, #51754, #99431, #179616, #34414, #32294, #196917, #101558, #164425, #100486, #1891, #98360, #16009, #19226, #166561, #18150, #97310, #81041, #84237, #85304, #151390, #47502, #2960, #135148, #113611, #147126, #114256, #196500, #1455, #15585, #65398, #180252, #35036, #166123, #50245, #30816, #96895, #380, #31876, #66454, #181300, #116365, #198598, #212728, #81672, #52377, #100059, #182355, #80619, #33983, #2521, #131544, #67520, #117438, #147758, #83795, #197546, #99003, #162944, #165058, #16650, #133665, #199666, #18783, #68594, #200726, #82735, #140052, #38258, #4651, #156288, #136834, #169322, #205001, #103261, #6795, #120652, #56645, #202860, #53433, #203927, #185557, #172537, #122809, #104332, #102190, #21967, #20906, #119570, #90224, #87002, #186631, #72872, #153074, #135770, #188768, #70721, #54508, #168257, #19856, #88075, #7872, #40408, #184488, #171456, #154149, #5716, #71793, #55575, #69662, #155214, #121729, #187694, #39323, #106510, #105418, #23045, #57711, #36105, #89161, #138978, #73960, #206077, #85943, #93434, #8948, #42555, #145409, #44680, #60907, #173625, #110792, #95575, #92376, #160541, #61982, #107593, #159474, #141140, #190889, #189833, #191948, #10013, #27332, #176794, #128136, #12147, #78220, #194100, #79291, #43614, #76089, #161625, #142191, #108658, #111867, #26260, #13218, #109732, #123868, #208206, #58773, #28409, #175739, #11072, #94503, #41482, #207150, #124928, #99808, #131304, #64114, #81423, #98748, #164805, #65148, #16398, #197295, #51058, #97696, #130256, #116109, #67270, #114003, #133408, #196247, #146455, #96636, #179998, #80356, #212470, #181052, #100862, #47891, #112930, #49990, #32668, #150705, #31622, #63039, #46816, #48936, #199413, #117182, #178943, #183183, #147504, #213525, #82476, #132, #30557, #163754, #84616, #132345, #66200, #162690, #198350, #34787, #15334, #165873, #149625, #115055, #182100, #33731, #17459, #129206, #83544, #1207, #166947, #18539, #195183, #39073, #105159, #171198, #172280, #70469, #36924, #188513, #169063, #201538, #22788, #69409, #88906, #152822, #154958, #20660, #151769, #55323, #4398, #54259, #153895, #2267, #168003, #136586, #6544, #202606, #3339, #86752, #38006, #104078, #120396, #170127, #186371, #204739, #103007, #135516, #121474, #72622, #53186, #138721, #119314, #85681, #35859, #185301, #19609, #21712, #87823, #40143, #5464, #52125, #203674, #71544, #89974, #137654, #68343, #200479, #187445, #56388, #122552, #118254, #106256, #23867, #134477, #184235, #101938, #210078, #127885, #141941, #73698, #59577, #108403, #173356, #193836, #92112, #191695, #44418, #8690, #107332, #205824, #109475, #175483, #123616, #41227, #93178, #204962, #36360, #197799, #151205, #105675, #171702, #203113, #7044, #107847, #27944, #42088, #157967, #156897, #61509, #192558, #76687, #144935, #57251, #175282, #8485, #92972, #59378, #159017, #26869, #207751, #140670, #10611, #108202, #125534, #44214, #173150, #60437, #209869, #110335, #12736, #43161, #123411, #176338, #107127, #95101, #78811, #206685, #94040, #191493, #109274, #160079, #11681, #161149, #24732, #29016, #90834, #77755, #143877, #127674, #193634, #189376, #45276, #111397, #177401, #41019, #211253, #41586, #141243, #129044, #24219, #91405, #207252, #58879, #172115 ),
 ( #42129, #136425, #124510, #205655, #108241, #186206, #57291, #103918, #123455, #24774, #104992, #154796, #206727, #21549, #71378, #55159, #72453, #23709, #7452, #189417, #156938, #8527, #74608, #140712, #58355, #96206, #159053, #76723, #47453, #126632, #97265, #192596, #176377, #127712, #194739, #12774, #78848, #26905, #162256, #10647, #110372, #46376, #209908, #141779, #129833, #61545, #112495, #30116, #13842, #79918, #113568, #94078, #146028, #63679, #160117, #193672, #77794, #207787, #45315, #111435, #177438, #59415, #125571, #191532, #43196, #109309, #175319, #93010, #84191, #64737, #198980, #101511, #1848, #118894, #149194, #36504, #18105, #213105, #201118, #184879, #32246, #182750, #83113, #131919, #166513, #769, #52760, #130880, #135104, #196874, #48511, #214145, #67907, #66835, #163320, #150278, #65771, #34368, #116751, #17036, #114631, #197929, #99387, #134053, #49555, #100442, #68986, #132978, #50625, #180623, #148143, #164382, #200061, #85256, #51713, #98317, #80995, #82050, #15966, #117832, #115681, #181675, #14901, #147083, #2913, #183823, #33302, #165439, #35435, #167582, #19181, #151344, #168643, #20245, #3981, #102583, #86331, #152402, #145765, #113292, #179301, #81781, #147864, #34090, #182461, #165160, #95930, #100161, #30922, #163051, #133766, #80724, #51420, #146815, #48244, #213880, #82838, #99110, #181406, #96998, #166225, #14630, #196603, #33032, #65501, #117541, #1561, #131649, #148913, #16755, #488, #66556, #199774, #212834, #132698, #198704, #64471, #197652, #130612, #50349, #49299, #114358, #115414, #116469, #17813, #83899, #149989, #15696, #98057, #67622, #183535, #180353, #47179, #161986, #164111, #13576, #31979, #79649, #211766, #63404, #129557, #195543, #18888, #69764, #35141, #23149, #101216, #39426, #3687, #119673, #36209, #52476, #102288, #167301, #168361, #53540, #186735, #120226, #36752, #135353, #203500, #115944, #19431, #1035, #151597, #134302, #201370, #85511, #83367, #34626, #137486, #185127, #53010, #165703, #119145, #87655, #84446, #152647, #202434, #99635, #3165, #17292, #183009, #181933, #118083, #2097, #69236, #102838, #54088, #4232, #70302, #136418, #71370, #184070, #150534, #153723, #68171, #100695, #186199, #166773, #37834, #51961, #103911, #200310, #50887, #168894, #35689, #167832, #20497, #33564, #67099, #101765, #169956, #86582, #117010, #21543, #5292, #149453, #133235, #199240, #18369, #41053, #72446, #88733, #7443, #189411, #6376, #107162, #154789, #138547, #38902, #56219, #171027, #122382, #39978, #173187, #188339, #187274, #73524, #106086, #90870, #172109, #55153, #104986, #23702, #24767, #121300, #155857, #89812, #139626, #205649, #57286, #123449, #7970, #172637, #154245, #152110, #88173, #4744, #37284, #74060, #136935, #171546, #5818, #189934, #140152, #71893, #72970, #23142, #155309, #89259, #123966, #87100, #56740, #122908, #202963, #138001, #153169, #188866, #55666, #186728, #121822, #40505, #6891, #106609, #24212, #187791, #22063, #39420, #105514, #104430, #185653, #139075, #70820, #54603, #90315, #135863, #156386, #206176, #41579, #107694, #19951, #86035, #3682, #69759, #53534, #119666, #103357, #169419, #21003, #120751, #38352, #170477, #214400, #75129, #148401, #9053, #141238, #76186, #15168, #96474, #49819, #163586, #142294, #47717, #130090, #30387, #58872, #208305, #112762, #81256, #59935, #196085, #82306, #162522, #146290, #207246, #158514, #174785, #212302, #98577, #31451, #108760, #91399, #126090, #42650, #179831, #125029, #192051, #66029, #25297, #16223, #97529, #132178, #157459, #147335, #198184, #213364, #64985, #43715, #178775, #164639, #190986, #26359, #14095, #80185, #63935, #113833, #131141, #197129, #114882, #48767, #180882, #32503, #190576, #36069, #168217, #141886, #88846, #59518, #154903, #56333, #7555, #90983, #107277, #189521, #118465, #42232, #102151, #204682, #172223, #200686, #72563, #40086, #157045, #6487, #57393, #9701, #89917, #73642, #68556, #138661, #19816, #139740, #25948, #173296, #122492, #18745, #188454, #184451, #24878, #134683, #106197, #75779, #167158, #158111, #8633, #207895, #191636, #74714, #125676 ) ),
 .UNSPECIFIED., .F., .F., .T. ) 
 B_SPLINE_SURFACE_WITH_KNOTS ( ( 2, 2 ),
 ( 3, 2, 2, 2, 2, 2, 2, 2, 2, 2, 2, 2, 2, 2, 2, 2, 2, 2, 2, 2, 2, 2, 2, 2, 2, 2, 2, 2, 2, 2, 2, 2, 2, 2, 2, 2, 2, 2, 2, 2, 2, 2, 2, 2, 2, 2, 2, 2, 2, 2, 2, 2, 2, 2, 2, 2, 2, 2, 2, 2, 2, 2, 2, 2, 2, 2, 2, 2, 2, 2, 2, 2, 2, 2, 2, 2, 2, 2, 2, 2, 2, 2, 2, 2, 2, 2, 2, 2, 2, 2, 2, 2, 2, 2, 2, 2, 2, 2, 2, 2, 2, 2, 2, 2, 2, 2, 2, 2, 2, 2, 2, 2, 2, 2, 2, 2, 2, 2, 2, 2, 2, 2, 2, 2, 2, 2, 2, 2, 2, 2, 2, 2, 2, 2, 2, 2, 2, 2, 2, 2, 2, 2, 2, 2, 2, 2, 2, 2, 2, 2, 2, 2, 2, 2, 2, 2, 2, 2, 2, 2, 2, 2, 2, 2, 2, 2, 2, 2, 2, 2, 2, 2, 2, 2, 2, 2, 2, 2, 2, 2, 2, 2, 2, 2, 2, 2, 2, 2, 2, 2, 2, 2, 2, 2, 2, 2, 2, 2, 2, 2, 2, 2, 2, 2, 2, 2, 2, 2, 2, 2, 2, 2, 2, 2, 2, 2, 2, 2, 2, 2, 2, 2, 2, 2, 2, 2, 2, 2, 2, 2, 2, 2, 2, 2, 2, 2, 2, 2, 2, 2, 3 ),
 ( 0.000000000000000000, 1.000000000000000000 ),
 ( 0.000000000000000000, 0.004166666666666666609, 0.008333333333333333218, 0.01250000000000000069, 0.01666666666666666644, 0.02083333333333333218, 0.02500000000000000139, 0.02916666666666666713, 0.03333333333333333287, 0.03749999999999999861, 0.04166666666666666435, 0.04583333333333333010, 0.05000000000000000278, 0.05416666666666666852, 0.05833333333333333426, 0.06250000000000000000, 0.06666666666666666574, 0.07083333333333333148, 0.07499999999999999722, 0.07916666666666666297, 0.08333333333333332871, 0.08749999999999999445, 0.09166666666666666019, 0.09583333333333333981, 0.1000000000000000056, 0.1041666666666666713, 0.1083333333333333370, 0.1125000000000000028, 0.1166666666666666685, 0.1208333333333333343, 0.1250000000000000000, 0.1291666666666666796, 0.1333333333333333315, 0.1375000000000000111, 0.1416666666666666630, 0.1458333333333333426, 0.1499999999999999944, 0.1541666666666666741, 0.1583333333333333259, 0.1625000000000000056, 0.1666666666666666574, 0.1708333333333333370, 0.1749999999999999889, 0.1791666666666666685, 0.1833333333333333204, 0.1875000000000000000, 0.1916666666666666796, 0.1958333333333333315, 0.2000000000000000111, 0.2041666666666666630, 0.2083333333333333426, 0.2124999999999999944, 0.2166666666666666741, 0.2208333333333333259, 0.2250000000000000056, 0.2291666666666666574, 0.2333333333333333370, 0.2374999999999999889, 0.2416666666666666685, 0.2458333333333333204, 0.2500000000000000000, 0.2541666666666666519, 0.2583333333333333592, 0.2625000000000000111, 0.2666666666666666630, 0.2708333333333333148, 0.2750000000000000222, 0.2791666666666666741, 0.2833333333333333259, 0.2874999999999999778, 0.2916666666666666852, 0.2958333333333333370, 0.2999999999999999889, 0.3041666666666666408, 0.3083333333333333481, 0.3125000000000000000, 0.3166666666666666519, 0.3208333333333333592, 0.3250000000000000111, 0.3291666666666666630, 0.3333333333333333148, 0.3375000000000000222, 0.3416666666666666741, 0.3458333333333333259, 0.3499999999999999778, 0.3541666666666666852, 0.3583333333333333370, 0.3624999999999999889, 0.3666666666666666408, 0.3708333333333333481, 0.3750000000000000000, 0.3791666666666666519, 0.3833333333333333592, 0.3875000000000000111, 0.3916666666666666630, 0.3958333333333333148, 0.4000000000000000222, 0.4041666666666666741, 0.4083333333333333259, 0.4124999999999999778, 0.4166666666666666852, 0.4208333333333333370, 0.4249999999999999889, 0.4291666666666666408, 0.4333333333333333481, 0.4375000000000000000, 0.4416666666666666519, 0.4458333333333333592, 0.4500000000000000111, 0.4541666666666666630, 0.4583333333333333148, 0.4625000000000000222, 0.4666666666666666741, 0.4708333333333333259, 0.4749999999999999778, 0.4791666666666666852, 0.4833333333333333370, 0.4874999999999999889, 0.4916666666666666408, 0.4958333333333333481, 0.5000000000000000000, 0.5041666666666666519, 0.5083333333333333037, 0.5124999999999999556, 0.5166666666666667185, 0.5208333333333333703, 0.5250000000000000222, 0.5291666666666666741, 0.5333333333333333259, 0.5374999999999999778, 0.5416666666666666297, 0.5458333333333332815, 0.5500000000000000444, 0.5541666666666666963, 0.5583333333333333481, 0.5625000000000000000, 0.5666666666666666519, 0.5708333333333333037, 0.5749999999999999556, 0.5791666666666667185, 0.5833333333333333703, 0.5875000000000000222, 0.5916666666666666741, 0.5958333333333333259, 0.5999999999999999778, 0.6041666666666666297, 0.6083333333333332815, 0.6125000000000000444, 0.6166666666666666963, 0.6208333333333333481, 0.6250000000000000000, 0.6291666666666666519, 0.6333333333333333037, 0.6374999999999999556, 0.6416666666666667185, 0.6458333333333333703, 0.6500000000000000222, 0.6541666666666666741, 0.6583333333333333259, 0.6624999999999999778, 0.6666666666666666297, 0.6708333333333332815, 0.6750000000000000444, 0.6791666666666666963, 0.6833333333333333481, 0.6875000000000000000, 0.6916666666666666519, 0.6958333333333333037, 0.6999999999999999556, 0.7041666666666667185, 0.7083333333333333703, 0.7125000000000000222, 0.7166666666666666741, 0.7208333333333333259, 0.7249999999999999778, 0.7291666666666666297, 0.7333333333333332815, 0.7375000000000000444, 0.7416666666666666963, 0.7458333333333333481, 0.7500000000000000000, 0.7541666666666666519, 0.7583333333333333037, 0.7624999999999999556, 0.7666666666666667185, 0.7708333333333333703, 0.7750000000000000222, 0.7791666666666666741, 0.7833333333333333259, 0.7874999999999999778, 0.7916666666666666297, 0.7958333333333332815, 0.8000000000000000444, 0.8041666666666666963, 0.8083333333333333481, 0.8125000000000000000, 0.8166666666666666519, 0.8208333333333333037, 0.8249999999999999556, 0.8291666666666667185, 0.8333333333333333703, 0.8375000000000000222, 0.8416666666666666741, 0.8458333333333333259, 0.8499999999999999778, 0.8541666666666666297, 0.8583333333333332815, 0.8625000000000000444, 0.8666666666666666963, 0.8708333333333333481, 0.8750000000000000000, 0.8791666666666666519, 0.8833333333333333037, 0.8874999999999999556, 0.8916666666666667185, 0.8958333333333333703, 0.9000000000000000222, 0.9041666666666666741, 0.9083333333333333259, 0.9124999999999999778, 0.9166666666666666297, 0.9208333333333332815, 0.9250000000000000444, 0.9291666666666666963, 0.9333333333333333481, 0.9375000000000000000, 0.9416666666666666519, 0.9458333333333333037, 0.9499999999999999556, 0.9541666666666667185, 0.9583333333333333703, 0.9625000000000000222, 0.9666666666666666741, 0.9708333333333333259, 0.9749999999999999778, 0.9791666666666666297, 0.9833333333333332815, 0.9875000000000000444, 0.9916666666666666963, 0.9958333333333333481, 1.000000000000000000 ),
 .UNSPECIFIED. ) 
 GEOMETRIC_REPRESENTATION_ITEM ( )  RATIONAL_B_SPLINE_SURFACE ( (
 ( 1.000000000000000000, 0.8660254037844387076, 1.000000000000000000, 0.8660254037844387076, 1.000000000000000000, 0.8660254037844387076, 1.000000000000000000, 0.8660254037844387076, 1.000000000000000000, 0.8660254037844387076, 1.000000000000000000, 0.8660254037844387076, 1.000000000000000000, 0.8660254037844387076, 1.000000000000000000, 0.8660254037844387076, 1.000000000000000000, 0.8660254037844387076, 1.000000000000000000, 0.8660254037844387076, 1.000000000000000000, 0.8660254037844387076, 1.000000000000000000, 0.8660254037844387076, 1.000000000000000000, 0.8660254037844387076, 1.000000000000000000, 0.8660254037844387076, 1.000000000000000000, 0.8660254037844387076, 1.000000000000000000, 0.8660254037844387076, 1.000000000000000000, 0.8660254037844387076, 1.000000000000000000, 0.8660254037844387076, 1.000000000000000000, 0.8660254037844387076, 1.000000000000000000, 0.8660254037844387076, 1.000000000000000000, 0.8660254037844387076, 1.000000000000000000, 0.8660254037844387076, 1.000000000000000000, 0.8660254037844387076, 1.000000000000000000, 0.8660254037844387076, 1.000000000000000000, 0.8660254037844387076, 1.000000000000000000, 0.8660254037844387076, 1.000000000000000000, 0.8660254037844387076, 1.000000000000000000, 0.8660254037844387076, 1.000000000000000000, 0.8660254037844387076, 1.000000000000000000, 0.8660254037844387076, 1.000000000000000000, 0.8660254037844387076, 1.000000000000000000, 0.8660254037844387076, 1.000000000000000000, 0.8660254037844387076, 1.000000000000000000, 0.8660254037844387076, 1.000000000000000000, 0.8660254037844387076, 1.000000000000000000, 0.8660254037844387076, 1.000000000000000000, 0.8660254037844387076, 1.000000000000000000, 0.8660254037844387076, 1.000000000000000000, 0.8660254037844387076, 1.000000000000000000, 0.8660254037844387076, 1.000000000000000000, 0.8660254037844387076, 1.000000000000000000, 0.8660254037844387076, 1.000000000000000000, 0.8660254037844387076, 1.000000000000000000, 0.8660254037844387076, 1.000000000000000000, 0.8660254037844387076, 1.000000000000000000, 0.8660254037844387076, 1.000000000000000000, 0.8660254037844387076, 1.000000000000000000, 0.8660254037844387076, 1.000000000000000000, 0.8660254037844387076, 1.000000000000000000, 0.8660254037844387076, 1.000000000000000000, 0.8660254037844387076, 1.000000000000000000, 0.8660254037844387076, 1.000000000000000000, 0.8660254037844387076, 1.000000000000000000, 0.8660254037844387076, 1.000000000000000000, 0.8660254037844387076, 1.000000000000000000, 0.8660254037844387076, 1.000000000000000000, 0.8660254037844387076, 1.000000000000000000, 0.8660254037844387076, 1.000000000000000000, 0.8660254037844387076, 1.000000000000000000, 0.8660254037844387076, 1.000000000000000000, 0.8660254037844387076, 1.000000000000000000, 0.8660254037844387076, 1.000000000000000000, 0.8660254037844387076, 1.000000000000000000, 0.8660254037844387076, 1.000000000000000000, 0.8660254037844387076, 1.000000000000000000, 0.8660254037844387076, 1.000000000000000000, 0.8660254037844387076, 1.000000000000000000, 0.8660254037844387076, 1.000000000000000000, 0.8660254037844387076, 1.000000000000000000, 0.8660254037844387076, 1.000000000000000000, 0.8660254037844387076, 1.000000000000000000, 0.8660254037844387076, 1.000000000000000000, 0.8660254037844387076, 1.000000000000000000, 0.8660254037844387076, 1.000000000000000000, 0.8660254037844387076, 1.000000000000000000, 0.8660254037844387076, 1.000000000000000000, 0.8660254037844387076, 1.000000000000000000, 0.8660254037844387076, 1.000000000000000000, 0.8660254037844387076, 1.000000000000000000, 0.8660254037844387076, 1.000000000000000000, 0.8660254037844387076, 1.000000000000000000, 0.8660254037844387076, 1.000000000000000000, 0.8660254037844387076, 1.000000000000000000, 0.8660254037844387076, 1.000000000000000000, 0.8660254037844387076, 1.000000000000000000, 0.8660254037844387076, 1.000000000000000000, 0.8660254037844387076, 1.000000000000000000, 0.8660254037844387076, 1.000000000000000000, 0.8660254037844387076, 1.000000000000000000, 0.8660254037844387076, 1.000000000000000000, 0.8660254037844387076, 1.000000000000000000, 0.8660254037844387076, 1.000000000000000000, 0.8660254037844387076, 1.000000000000000000, 0.8660254037844387076, 1.000000000000000000, 0.8660254037844387076, 1.000000000000000000, 0.8660254037844387076, 1.000000000000000000, 0.8660254037844387076, 1.000000000000000000, 0.8660254037844387076, 1.000000000000000000, 0.8660254037844387076, 1.000000000000000000, 0.8660254037844387076, 1.000000000000000000, 0.8660254037844387076, 1.000000000000000000, 0.8660254037844387076, 1.000000000000000000, 0.8660254037844387076, 1.000000000000000000, 0.8660254037844387076, 1.000000000000000000, 0.8660254037844387076, 1.000000000000000000, 0.8660254037844387076, 1.000000000000000000, 0.8660254037844387076, 1.000000000000000000, 0.8660254037844387076, 1.000000000000000000, 0.8660254037844387076, 1.000000000000000000, 0.8660254037844387076, 1.000000000000000000, 0.8660254037844387076, 1.000000000000000000, 0.8660254037844387076, 1.000000000000000000, 0.8660254037844387076, 1.000000000000000000, 0.8660254037844387076, 1.000000000000000000, 0.8660254037844387076, 1.000000000000000000, 0.8660254037844387076, 1.000000000000000000, 0.8660254037844387076, 1.000000000000000000, 0.8660254037844387076, 1.000000000000000000, 0.8660254037844387076, 1.000000000000000000, 0.8660254037844387076, 1.000000000000000000, 0.8660254037844387076, 1.000000000000000000, 0.8660254037844387076, 1.000000000000000000, 0.8660254037844387076, 1.000000000000000000, 0.8660254037844387076, 1.000000000000000000, 0.8660254037844387076, 1.000000000000000000, 0.8660254037844387076, 1.000000000000000000, 0.8660254037844387076, 1.000000000000000000, 0.8660254037844387076, 1.000000000000000000, 0.8660254037844387076, 1.000000000000000000, 0.8660254037844387076, 1.000000000000000000, 0.8660254037844387076, 1.000000000000000000, 0.8660254037844387076, 1.000000000000000000, 0.8660254037844387076, 1.000000000000000000, 0.8660254037844387076, 1.000000000000000000, 0.8660254037844387076, 1.000000000000000000, 0.8660254037844387076, 1.000000000000000000, 0.8660254037844387076, 1.000000000000000000, 0.8660254037844387076, 1.000000000000000000, 0.8660254037844387076, 1.000000000000000000, 0.8660254037844387076, 1.000000000000000000, 0.8660254037844387076, 1.000000000000000000, 0.8660254037844387076, 1.000000000000000000, 0.8660254037844387076, 1.000000000000000000, 0.8660254037844387076, 1.000000000000000000, 0.8660254037844387076, 1.000000000000000000, 0.8660254037844387076, 1.000000000000000000, 0.8660254037844387076, 1.000000000000000000, 0.8660254037844387076, 1.000000000000000000, 0.8660254037844387076, 1.000000000000000000, 0.8660254037844387076, 1.000000000000000000, 0.8660254037844387076, 1.000000000000000000, 0.8660254037844387076, 1.000000000000000000, 0.8660254037844387076, 1.000000000000000000, 0.8660254037844387076, 1.000000000000000000, 0.8660254037844387076, 1.000000000000000000, 0.8660254037844387076, 1.000000000000000000, 0.8660254037844387076, 1.000000000000000000, 0.8660254037844387076, 1.000000000000000000, 0.8660254037844387076, 1.000000000000000000, 0.8660254037844387076, 1.000000000000000000, 0.8660254037844387076, 1.000000000000000000, 0.8660254037844387076, 1.000000000000000000, 0.8660254037844387076, 1.000000000000000000, 0.8660254037844387076, 1.000000000000000000, 0.8660254037844387076, 1.000000000000000000, 0.8660254037844387076, 1.000000000000000000, 0.8660254037844387076, 1.000000000000000000, 0.8660254037844387076, 1.000000000000000000, 0.8660254037844387076, 1.000000000000000000, 0.8660254037844387076, 1.000000000000000000, 0.8660254037844387076, 1.000000000000000000, 0.8660254037844387076, 1.000000000000000000, 0.8660254037844387076, 1.000000000000000000, 0.8660254037844387076, 1.000000000000000000, 0.8660254037844387076, 1.000000000000000000, 0.8660254037844387076, 1.000000000000000000, 0.8660254037844387076, 1.000000000000000000, 0.8660254037844387076, 1.000000000000000000, 0.8660254037844387076, 1.000000000000000000, 0.8660254037844387076, 1.000000000000000000, 0.8660254037844387076, 1.000000000000000000, 0.8660254037844387076, 1.000000000000000000, 0.8660254037844387076, 1.000000000000000000, 0.8660254037844387076, 1.000000000000000000, 0.8660254037844387076, 1.000000000000000000, 0.8660254037844387076, 1.000000000000000000, 0.8660254037844387076, 1.000000000000000000, 0.8660254037844387076, 1.000000000000000000, 0.8660254037844387076, 1.000000000000000000, 0.8660254037844387076, 1.000000000000000000, 0.8660254037844387076, 1.000000000000000000, 0.8660254037844387076, 1.000000000000000000, 0.8660254037844387076, 1.000000000000000000, 0.8660254037844387076, 1.000000000000000000, 0.8660254037844387076, 1.000000000000000000, 0.8660254037844387076, 1.000000000000000000, 0.8660254037844387076, 1.000000000000000000, 0.8660254037844387076, 1.000000000000000000, 0.8660254037844387076, 1.000000000000000000, 0.8660254037844387076, 1.000000000000000000, 0.8660254037844387076, 1.000000000000000000, 0.8660254037844387076, 1.000000000000000000, 0.8660254037844387076, 1.000000000000000000, 0.8660254037844387076, 1.000000000000000000, 0.8660254037844387076, 1.000000000000000000, 0.8660254037844387076, 1.000000000000000000, 0.8660254037844387076, 1.000000000000000000, 0.8660254037844387076, 1.000000000000000000, 0.8660254037844387076, 1.000000000000000000, 0.8660254037844387076, 1.000000000000000000, 0.8660254037844387076, 1.000000000000000000, 0.8660254037844387076, 1.000000000000000000, 0.8660254037844387076, 1.000000000000000000, 0.8660254037844387076, 1.000000000000000000, 0.8660254037844387076, 1.000000000000000000, 0.8660254037844387076, 1.000000000000000000, 0.8660254037844387076, 1.000000000000000000, 0.8660254037844387076, 1.000000000000000000, 0.8660254037844387076, 1.000000000000000000, 0.8660254037844387076, 1.000000000000000000, 0.8660254037844387076, 1.000000000000000000, 0.8660254037844387076, 1.000000000000000000, 0.8660254037844387076, 1.000000000000000000, 0.8660254037844387076, 1.000000000000000000, 0.8660254037844387076, 1.000000000000000000, 0.8660254037844387076, 1.000000000000000000, 0.8660254037844387076, 1.000000000000000000, 0.8660254037844387076, 1.000000000000000000, 0.8660254037844387076, 1.000000000000000000, 0.8660254037844387076, 1.000000000000000000, 0.8660254037844387076, 1.000000000000000000, 0.8660254037844387076, 1.000000000000000000, 0.8660254037844387076, 1.000000000000000000, 0.8660254037844387076, 1.000000000000000000, 0.8660254037844387076, 1.000000000000000000, 0.8660254037844387076, 1.000000000000000000, 0.8660254037844387076, 1.000000000000000000, 0.8660254037844387076, 1.000000000000000000, 0.8660254037844387076, 1.000000000000000000, 0.8660254037844387076, 1.000000000000000000),
 ( 1.000000000000000000, 0.8660254037844387076, 1.000000000000000000, 0.8660254037844387076, 1.000000000000000000, 0.8660254037844387076, 1.000000000000000000, 0.8660254037844387076, 1.000000000000000000, 0.8660254037844387076, 1.000000000000000000, 0.8660254037844387076, 1.000000000000000000, 0.8660254037844387076, 1.000000000000000000, 0.8660254037844387076, 1.000000000000000000, 0.8660254037844387076, 1.000000000000000000, 0.8660254037844387076, 1.000000000000000000, 0.8660254037844387076, 1.000000000000000000, 0.8660254037844387076, 1.000000000000000000, 0.8660254037844387076, 1.000000000000000000, 0.8660254037844387076, 1.000000000000000000, 0.8660254037844387076, 1.000000000000000000, 0.8660254037844387076, 1.000000000000000000, 0.8660254037844387076, 1.000000000000000000, 0.8660254037844387076, 1.000000000000000000, 0.8660254037844387076, 1.000000000000000000, 0.8660254037844387076, 1.000000000000000000, 0.8660254037844387076, 1.000000000000000000, 0.8660254037844387076, 1.000000000000000000, 0.8660254037844387076, 1.000000000000000000, 0.8660254037844387076, 1.000000000000000000, 0.8660254037844387076, 1.000000000000000000, 0.8660254037844387076, 1.000000000000000000, 0.8660254037844387076, 1.000000000000000000, 0.8660254037844387076, 1.000000000000000000, 0.8660254037844387076, 1.000000000000000000, 0.8660254037844387076, 1.000000000000000000, 0.8660254037844387076, 1.000000000000000000, 0.8660254037844387076, 1.000000000000000000, 0.8660254037844387076, 1.000000000000000000, 0.8660254037844387076, 1.000000000000000000, 0.8660254037844387076, 1.000000000000000000, 0.8660254037844387076, 1.000000000000000000, 0.8660254037844387076, 1.000000000000000000, 0.8660254037844387076, 1.000000000000000000, 0.8660254037844387076, 1.000000000000000000, 0.8660254037844387076, 1.000000000000000000, 0.8660254037844387076, 1.000000000000000000, 0.8660254037844387076, 1.000000000000000000, 0.8660254037844387076, 1.000000000000000000, 0.8660254037844387076, 1.000000000000000000, 0.8660254037844387076, 1.000000000000000000, 0.8660254037844387076, 1.000000000000000000, 0.8660254037844387076, 1.000000000000000000, 0.8660254037844387076, 1.000000000000000000, 0.8660254037844387076, 1.000000000000000000, 0.8660254037844387076, 1.000000000000000000, 0.8660254037844387076, 1.000000000000000000, 0.8660254037844387076, 1.000000000000000000, 0.8660254037844387076, 1.000000000000000000, 0.8660254037844387076, 1.000000000000000000, 0.8660254037844387076, 1.000000000000000000, 0.8660254037844387076, 1.000000000000000000, 0.8660254037844387076, 1.000000000000000000, 0.8660254037844387076, 1.000000000000000000, 0.8660254037844387076, 1.000000000000000000, 0.8660254037844387076, 1.000000000000000000, 0.8660254037844387076, 1.000000000000000000, 0.8660254037844387076, 1.000000000000000000, 0.8660254037844387076, 1.000000000000000000, 0.8660254037844387076, 1.000000000000000000, 0.8660254037844387076, 1.000000000000000000, 0.8660254037844387076, 1.000000000000000000, 0.8660254037844387076, 1.000000000000000000, 0.8660254037844387076, 1.000000000000000000, 0.8660254037844387076, 1.000000000000000000, 0.8660254037844387076, 1.000000000000000000, 0.8660254037844387076, 1.000000000000000000, 0.8660254037844387076, 1.000000000000000000, 0.8660254037844387076, 1.000000000000000000, 0.8660254037844387076, 1.000000000000000000, 0.8660254037844387076, 1.000000000000000000, 0.8660254037844387076, 1.000000000000000000, 0.8660254037844387076, 1.000000000000000000, 0.8660254037844387076, 1.000000000000000000, 0.8660254037844387076, 1.000000000000000000, 0.8660254037844387076, 1.000000000000000000, 0.8660254037844387076, 1.000000000000000000, 0.8660254037844387076, 1.000000000000000000, 0.8660254037844387076, 1.000000000000000000, 0.8660254037844387076, 1.000000000000000000, 0.8660254037844387076, 1.000000000000000000, 0.8660254037844387076, 1.000000000000000000, 0.8660254037844387076, 1.000000000000000000, 0.8660254037844387076, 1.000000000000000000, 0.8660254037844387076, 1.000000000000000000, 0.8660254037844387076, 1.000000000000000000, 0.8660254037844387076, 1.000000000000000000, 0.8660254037844387076, 1.000000000000000000, 0.8660254037844387076, 1.000000000000000000, 0.8660254037844387076, 1.000000000000000000, 0.8660254037844387076, 1.000000000000000000, 0.8660254037844387076, 1.000000000000000000, 0.8660254037844387076, 1.000000000000000000, 0.8660254037844387076, 1.000000000000000000, 0.8660254037844387076, 1.000000000000000000, 0.8660254037844387076, 1.000000000000000000, 0.8660254037844387076, 1.000000000000000000, 0.8660254037844387076, 1.000000000000000000, 0.8660254037844387076, 1.000000000000000000, 0.8660254037844387076, 1.000000000000000000, 0.8660254037844387076, 1.000000000000000000, 0.8660254037844387076, 1.000000000000000000, 0.8660254037844387076, 1.000000000000000000, 0.8660254037844387076, 1.000000000000000000, 0.8660254037844387076, 1.000000000000000000, 0.8660254037844387076, 1.000000000000000000, 0.8660254037844387076, 1.000000000000000000, 0.8660254037844387076, 1.000000000000000000, 0.8660254037844387076, 1.000000000000000000, 0.8660254037844387076, 1.000000000000000000, 0.8660254037844387076, 1.000000000000000000, 0.8660254037844387076, 1.000000000000000000, 0.8660254037844387076, 1.000000000000000000, 0.8660254037844387076, 1.000000000000000000, 0.8660254037844387076, 1.000000000000000000, 0.8660254037844387076, 1.000000000000000000, 0.8660254037844387076, 1.000000000000000000, 0.8660254037844387076, 1.000000000000000000, 0.8660254037844387076, 1.000000000000000000, 0.8660254037844387076, 1.000000000000000000, 0.8660254037844387076, 1.000000000000000000, 0.8660254037844387076, 1.000000000000000000, 0.8660254037844387076, 1.000000000000000000, 0.8660254037844387076, 1.000000000000000000, 0.8660254037844387076, 1.000000000000000000, 0.8660254037844387076, 1.000000000000000000, 0.8660254037844387076, 1.000000000000000000, 0.8660254037844387076, 1.000000000000000000, 0.8660254037844387076, 1.000000000000000000, 0.8660254037844387076, 1.000000000000000000, 0.8660254037844387076, 1.000000000000000000, 0.8660254037844387076, 1.000000000000000000, 0.8660254037844387076, 1.000000000000000000, 0.8660254037844387076, 1.000000000000000000, 0.8660254037844387076, 1.000000000000000000, 0.8660254037844387076, 1.000000000000000000, 0.8660254037844387076, 1.000000000000000000, 0.8660254037844387076, 1.000000000000000000, 0.8660254037844387076, 1.000000000000000000, 0.8660254037844387076, 1.000000000000000000, 0.8660254037844387076, 1.000000000000000000, 0.8660254037844387076, 1.000000000000000000, 0.8660254037844387076, 1.000000000000000000, 0.8660254037844387076, 1.000000000000000000, 0.8660254037844387076, 1.000000000000000000, 0.8660254037844387076, 1.000000000000000000, 0.8660254037844387076, 1.000000000000000000, 0.8660254037844387076, 1.000000000000000000, 0.8660254037844387076, 1.000000000000000000, 0.8660254037844387076, 1.000000000000000000, 0.8660254037844387076, 1.000000000000000000, 0.8660254037844387076, 1.000000000000000000, 0.8660254037844387076, 1.000000000000000000, 0.8660254037844387076, 1.000000000000000000, 0.8660254037844387076, 1.000000000000000000, 0.8660254037844387076, 1.000000000000000000, 0.8660254037844387076, 1.000000000000000000, 0.8660254037844387076, 1.000000000000000000, 0.8660254037844387076, 1.000000000000000000, 0.8660254037844387076, 1.000000000000000000, 0.8660254037844387076, 1.000000000000000000, 0.8660254037844387076, 1.000000000000000000, 0.8660254037844387076, 1.000000000000000000, 0.8660254037844387076, 1.000000000000000000, 0.8660254037844387076, 1.000000000000000000, 0.8660254037844387076, 1.000000000000000000, 0.8660254037844387076, 1.000000000000000000, 0.8660254037844387076, 1.000000000000000000, 0.8660254037844387076, 1.000000000000000000, 0.8660254037844387076, 1.000000000000000000, 0.8660254037844387076, 1.000000000000000000, 0.8660254037844387076, 1.000000000000000000, 0.8660254037844387076, 1.000000000000000000, 0.8660254037844387076, 1.000000000000000000, 0.8660254037844387076, 1.000000000000000000, 0.8660254037844387076, 1.000000000000000000, 0.8660254037844387076, 1.000000000000000000, 0.8660254037844387076, 1.000000000000000000, 0.8660254037844387076, 1.000000000000000000, 0.8660254037844387076, 1.000000000000000000, 0.8660254037844387076, 1.000000000000000000, 0.8660254037844387076, 1.000000000000000000, 0.8660254037844387076, 1.000000000000000000, 0.8660254037844387076, 1.000000000000000000, 0.8660254037844387076, 1.000000000000000000, 0.8660254037844387076, 1.000000000000000000, 0.8660254037844387076, 1.000000000000000000, 0.8660254037844387076, 1.000000000000000000, 0.8660254037844387076, 1.000000000000000000, 0.8660254037844387076, 1.000000000000000000, 0.8660254037844387076, 1.000000000000000000, 0.8660254037844387076, 1.000000000000000000, 0.8660254037844387076, 1.000000000000000000, 0.8660254037844387076, 1.000000000000000000, 0.8660254037844387076, 1.000000000000000000, 0.8660254037844387076, 1.000000000000000000, 0.8660254037844387076, 1.000000000000000000, 0.8660254037844387076, 1.000000000000000000, 0.8660254037844387076, 1.000000000000000000, 0.8660254037844387076, 1.000000000000000000, 0.8660254037844387076, 1.000000000000000000, 0.8660254037844387076, 1.000000000000000000, 0.8660254037844387076, 1.000000000000000000, 0.8660254037844387076, 1.000000000000000000, 0.8660254037844387076, 1.000000000000000000, 0.8660254037844387076, 1.000000000000000000, 0.8660254037844387076, 1.000000000000000000, 0.8660254037844387076, 1.000000000000000000, 0.8660254037844387076, 1.000000000000000000, 0.8660254037844387076, 1.000000000000000000, 0.8660254037844387076, 1.000000000000000000, 0.8660254037844387076, 1.000000000000000000, 0.8660254037844387076, 1.000000000000000000, 0.8660254037844387076, 1.000000000000000000, 0.8660254037844387076, 1.000000000000000000, 0.8660254037844387076, 1.000000000000000000, 0.8660254037844387076, 1.000000000000000000, 0.8660254037844387076, 1.000000000000000000, 0.8660254037844387076, 1.000000000000000000, 0.8660254037844387076, 1.000000000000000000, 0.8660254037844387076, 1.000000000000000000, 0.8660254037844387076, 1.000000000000000000, 0.8660254037844387076, 1.000000000000000000, 0.8660254037844387076, 1.000000000000000000, 0.8660254037844387076, 1.000000000000000000, 0.8660254037844387076, 1.000000000000000000, 0.8660254037844387076, 1.000000000000000000, 0.8660254037844387076, 1.000000000000000000, 0.8660254037844387076, 1.000000000000000000, 0.8660254037844387076, 1.000000000000000000, 0.8660254037844387076, 1.000000000000000000, 0.8660254037844387076, 1.000000000000000000, 0.8660254037844387076, 1.000000000000000000, 0.8660254037844387076, 1.000000000000000000, 0.8660254037844387076, 1.000000000000000000, 0.8660254037844387076, 1.000000000000000000) ) ) 
 REPRESENTATION_ITEM ( '' )  SURFACE ( )  );
#42333 = CARTESIAN_POINT ( 'NONE',  ( 5.479157358542966705, -1.820838119324312165, -0.8587918944957111389 ) ) ;
#42334 = CARTESIAN_POINT ( 'NONE',  ( 4.482942347612929979, 8.381849838857084123, 1.040834085586084257E-14 ) ) ;
#42335 = CARTESIAN_POINT ( 'NONE',  ( 4.419037640130375699, 1.924477966361681780, 0.8556825127635151462 ) ) ;
#42336 = CARTESIAN_POINT ( 'NONE',  ( 2.935058904569508353, -1.567653816607515127, -1.100626458259999385 ) ) ;
#42337 = CARTESIAN_POINT ( 'NONE',  ( -0.02244404828160087226, 4.081832076214893412, -2.743766916979750281 ) ) ;
#42338 = CARTESIAN_POINT ( 'NONE',  ( 4.228926779721821738, -1.836881627057206590, -0.7110872907168819257 ) ) ;
#42339 = CARTESIAN_POINT ( 'NONE',  ( 5.888927314555610693, -1.919185580196127283, -0.6297945592430991280 ) ) ;
#42340 = CARTESIAN_POINT ( 'NONE',  ( 2.254581950620972997, -1.447608085528677480, 1.184820545849271767 ) ) ;
#42343 = ORIENTED_EDGE ( 'NONE', *, *, #191143, .F. ) ;
#42342 = CARTESIAN_POINT ( 'NONE',  ( 1.476665317443916603, -1.350161712199383413, 1.354623164920423450 ) ) ;
#42341 = CARTESIAN_POINT ( 'NONE',  ( 5.514166437991733005, -0.7808720426115691726, -1.538077146617151669 ) ) ;
#42345 = CARTESIAN_POINT ( 'NONE',  ( 5.029711800989886683, 4.970344644017389513, 1.040834085586084257E-14 ) ) ;
#42344 = CARTESIAN_POINT ( 'NONE',  ( 1.893488989520499377, 1.919108310403025985, -1.089527612406354873 ) ) ;
#42346 = CARTESIAN_POINT ( 'NONE',  ( 0.6823417656249899377, 2.155208333674753174, 1.181850606188767472 ) ) ;
#42347 = CARTESIAN_POINT ( 'NONE',  ( 6.215287892896892430, -1.681934637451238279, -1.009743211781432670 ) ) ;
#42348 = CARTESIAN_POINT ( 'NONE',  ( 8.762647353133951711, 9.117510088278095282, 1.040834085586084257E-14 ) ) ;
#42349 = CARTESIAN_POINT ( 'NONE',  ( -7.173763318588814109, -6.681223591462385869, 7.173763318588837201 ) ) ;
#42350 = DIRECTION ( 'NONE',  ( 0.000000000000000000, 1.000000000000000000, 0.000000000000000000 ) ) ;
#42351 = CARTESIAN_POINT ( 'NONE',  ( -0.4000000000001999734, 2.876379076189460093, -2.023857702507711132 ) ) ;
#42352 = CIRCLE ( 'NONE', #177152, 0.08000000000000041800 ) ;
#42353 = FACE_OUTER_BOUND ( 'NONE', #107157, .T. ) ;
#42354 = CIRCLE ( 'NONE', #31976, 0.04999999999999972522 ) ;
#42355 = ORIENTED_EDGE ( 'NONE', *, *, #4802, .T. ) ;
#42356 = CARTESIAN_POINT ( 'NONE',  ( 1.979048004138800998, 1.930994533390210544, 0.7472069620131777112 ) ) ;
#42357 = CARTESIAN_POINT ( 'NONE',  ( 0.7499999999999885647, 2.816666666666689522, -1.299038105676658228 ) ) ;
#42358 = CARTESIAN_POINT ( 'NONE',  ( 6.647575389402066826, 6.649926130590872120, 1.040834085586084257E-14 ) ) ;
#42359 = CARTESIAN_POINT ( 'NONE',  ( 3.230585741806197841, 6.991043475407723307, 0.7998128361456271485 ) ) ;
#42360 = CARTESIAN_POINT ( 'NONE',  ( 6.305353446217972113, 1.845220813986702124, -1.044706065825385943 ) ) ;
#42361 = CARTESIAN_POINT ( 'NONE',  ( 1.499999999999990896, 5.775000000000023448, 1.040834085586084414E-14 ) ) ;
#42362 = EDGE_CURVE ( 'NONE', #210405, #65799, #99892, .T. ) ;
#42363 = CARTESIAN_POINT ( 'NONE',  ( 1.364683531249988757, 2.384375000341422357, 1.214306433183764966E-14 ) ) ;
#42365 = CARTESIAN_POINT ( 'NONE',  ( 9.924205255523292024, 10.68058700763975466, -0.7216878364870257245 ) ) ;
#42364 = CARTESIAN_POINT ( 'NONE',  ( 1.448815997565456204, 7.903552007303736637, 10.65195286442483358 ) ) ;
#42366 = CARTESIAN_POINT ( 'NONE',  ( 5.501327308730313170, 1.985796898448642933, 0.3474119236192701465 ) ) ;
#42367 = CARTESIAN_POINT ( 'NONE',  ( 5.137857799264941683, 1.913235287650059790, -0.1005462703686579862 ) ) ;
#42368 = CARTESIAN_POINT ( 'NONE',  ( 6.539320575229278454, 0.5749733277502915296, 2.156147827957733742 ) ) ;
#42369 = CARTESIAN_POINT ( 'NONE',  ( 2.683357600500847262, 1.551837136583393839, 1.547750905674146971 ) ) ;
#42370 = CARTESIAN_POINT ( 'NONE',  ( -1.500000000000015099, 10.51041666734946389, -0.8660254037844309360 ) ) ;
#42371 = CARTESIAN_POINT ( 'NONE',  ( -1.499999999999997780, 1.681250000682817047, 0.000000000000000000 ) ) ;
#42372 = CARTESIAN_POINT ( 'NONE',  ( 5.220952493833380004, 1.521736800665099976, -1.318127947290965052 ) ) ;
#42373 = CARTESIAN_POINT ( 'NONE',  ( 1.740342883905017013, 1.098329146349947827, -1.565357986077076990 ) ) ;
#42374 = CARTESIAN_POINT ( 'NONE',  ( -4.855791571988752331, 8.816840600628864877, 0.7998128361456481317 ) ) ;
#42375 = EDGE_CURVE ( 'NONE', #177940, #105963, #113885, .T. ) ;
#42377 = CARTESIAN_POINT ( 'NONE',  ( 0.05236148938883232462, -1.314980595004966002, 1.528755779884483523 ) ) ;
#42376 =( NAMED_UNIT ( * ) SI_UNIT ( $, .STERADIAN. ) SOLID_ANGLE_UNIT ( ) );
#42378 = CARTESIAN_POINT ( 'NONE',  ( 1.364683531250000303, 9.317708333674735499, -0.7879004041258355073 ) ) ;
#42380 = CARTESIAN_POINT ( 'NONE',  ( -6.818824913030298696, 6.919993584815607335, 0.7998128361456341429 ) ) ;
#42379 = CARTESIAN_POINT ( 'NONE',  ( 3.333613130510120648, 0.9378223671878234136, -1.868666107883134142 ) ) ;
#42382 = ORIENTED_EDGE ( 'NONE', *, *, #115310, .F. ) ;
#42381 = CARTESIAN_POINT ( 'NONE',  ( 2.379564082050821483, 1.058669913282745956, 1.361546577445968964 ) ) ;
#42383 = CARTESIAN_POINT ( 'NONE',  ( 6.240501835383900797, 1.219778281852833546, -1.734492557903525300 ) ) ;
#42384 = CARTESIAN_POINT ( 'NONE',  ( 5.341022448779654930, 8.318611059296550536, 1.199719254218462483 ) ) ;
#42385 = CONICAL_SURFACE ( 'NONE', #211793, 7.034482758620711706, 0.8621700546672336207 ) ;
#42386 = DIRECTION ( 'NONE',  ( -0.8164965809277262565, 8.702247276351162783E-15, 0.5773502691896256200 ) ) ;
#42387 = CARTESIAN_POINT ( 'NONE',  ( 10.51596412982177853, 13.61340918268422939, -3.553961965504329523 ) ) ;
#42388 = CARTESIAN_POINT ( 'NONE',  ( 11.49966000274960898, 9.857671544352703208, -3.429881629453144232 ) ) ;
#42389 = CARTESIAN_POINT ( 'NONE',  ( 4.645640190976921602, 8.571663989448405019, 1.040834085586084257E-14 ) ) ;
#42390 = DIRECTION ( 'NONE',  ( 0.000000000000000000, 1.000000000000000000, 0.000000000000000000 ) ) ;
#42391 = ORIENTED_EDGE ( 'NONE', *, *, #54338, .T. ) ;
#42392 = CARTESIAN_POINT ( 'NONE',  ( 3.334412561109405537, 1.147067551318830203, -1.402027596893473449 ) ) ;
#42393 = VERTEX_POINT ( 'NONE', #60910 ) ;
#42394 = CARTESIAN_POINT ( 'NONE',  ( 4.715538499454675403, 4.395883092318884522, 1.214306433183764966E-14 ) ) ;
#42395 = CARTESIAN_POINT ( 'NONE',  ( 3.725458348705031231, 7.568394850123006279, -1.734723475976807094E-15 ) ) ;
#42396 = CARTESIAN_POINT ( 'NONE',  ( 3.703588720873185469, 1.314418127562553940, 1.246746269480051073 ) ) ;
#42397 = CARTESIAN_POINT ( 'NONE',  ( 6.539320575229270460, 2.052047842581938841, 2.303245992296603983 ) ) ;
#42398 = CYLINDRICAL_SURFACE ( 'NONE', #62604, 0.09999999999999982514 ) ;
#42399 = CARTESIAN_POINT ( 'NONE',  ( 5.891550962509589873, 5.977563058329811163, 0.05700887847147687038 ) ) ;
#42400 = EDGE_CURVE ( 'NONE', #49550, #61752, #145413, .T. ) ;
#42402 = CARTESIAN_POINT ( 'NONE',  ( -1.402160292154681736E-14, 14.67187500034139980, 1.575800808251682339 ) ) ;
#42401 = CARTESIAN_POINT ( 'NONE',  ( 3.771788145607783527, -1.833817148065859604, 0.3161742572238452897 ) ) ;
#42403 = CARTESIAN_POINT ( 'NONE',  ( 1.985809494836645817, -1.915157380443854418, 0.04907906824581054206 ) ) ;
#42404 = CARTESIAN_POINT ( 'NONE',  ( 0.5690311950540331010, 0.1842100624489529104, -1.816270042949569730 ) ) ;
#42405 = CARTESIAN_POINT ( 'NONE',  ( 4.827066317303362553, 8.099069806723665721, 0.8733865547906801696 ) ) ;
#42406 = CARTESIAN_POINT ( 'NONE',  ( -10.47022434975266592, 4.009060182194922994, -5.775464948712724755 ) ) ;
#42407 = ADVANCED_FACE ( 'NONE', ( #160545 ), #194104, .F. ) ;
#42408 = CARTESIAN_POINT ( 'NONE',  ( 6.162627863271451290, 6.966383021533493647, 0.9102919922300183320 ) ) ;
#42409 = CARTESIAN_POINT ( 'NONE',  ( -0.7500000000000179856, 8.541666666666669627, 1.299038105676658228 ) ) ;
#42410 = CARTESIAN_POINT ( 'NONE',  ( 7.721398836998391246, 0.000000000000000000, 7.721398836998372595 ) ) ;
#42411 = DIRECTION ( 'NONE',  ( 3.330669073875478989E-16, -3.540251991789410786E-16, -1.000000000000000000 ) ) ;
#42412 = CARTESIAN_POINT ( 'NONE',  ( 5.666945020832160118, 9.555260257705446847, 0.7216878364870438212 ) ) ;
#42413 = CARTESIAN_POINT ( 'NONE',  ( 5.330891317213126257, -1.853047821147445484, -0.6673286768130722857 ) ) ;
#42414 = CARTESIAN_POINT ( 'NONE',  ( -5.362413449404877852, 6.214902764849178141, -1.199719254218446718 ) ) ;
#42415 = CARTESIAN_POINT ( 'NONE',  ( 4.989037339704528229, 4.922891105851139315, 1.040834085586084257E-14 ) ) ;
#42416 = CARTESIAN_POINT ( 'NONE',  ( 0.3926704732973253509, 1.736993494895492152, -1.163127744158433119 ) ) ;
#42417 = CARTESIAN_POINT ( 'NONE',  ( 6.071306304379397112, 0.1413743337459697769, -1.921272325444240980 ) ) ;
#42418 = CARTESIAN_POINT ( 'NONE',  ( -4.882907879216086933, 8.848476292394087395, -0.7998128361456281477 ) ) ;
#42419 = CARTESIAN_POINT ( 'NONE',  ( 1.799542586263824795, -0.6183211656001773582, 1.717807299235304619 ) ) ;
#42420 = CARTESIAN_POINT ( 'NONE',  ( 1.858336453454629611, 2.200810804183956026, -0.1644699235988852648 ) ) ;
#42421 = FACE_OUTER_BOUND ( 'NONE', #82580, .T. ) ;
#42422 = CARTESIAN_POINT ( 'NONE',  ( 0.6856317642073318508, 1.842354612247762091, -0.5124485439033445999 ) ) ;
#42423 = ORIENTED_EDGE ( 'NONE', *, *, #99041, .F. ) ;
#42424 = CARTESIAN_POINT ( 'NONE',  ( 0.2386330332824412315, -1.909482672672847992, -0.4822418261516500659 ) ) ;
#42425 = CARTESIAN_POINT ( 'NONE',  ( 3.140110198738320424, 0.4743784485543530716, 1.883105278476588706 ) ) ;
#42426 = ORIENTED_EDGE ( 'NONE', *, *, #79797, .T. ) ;
#42427 = CARTESIAN_POINT ( 'NONE',  ( 5.346851039111009563, 6.199209027673978412, 2.419999999999999485 ) ) ;
#42429 = CARTESIAN_POINT ( 'NONE',  ( 6.912964126797830566, -1.438640208141970245, 1.180240733875538517 ) ) ;
#42428 = CARTESIAN_POINT ( 'NONE',  ( -5.143339171537843590, 7.093924681584509173, 1.599625672291263179 ) ) ;
#42430 = CARTESIAN_POINT ( 'NONE',  ( 5.422335090822693715, 5.290755458906732933, 0.000000000000000000 ) ) ;
#42431 = CARTESIAN_POINT ( 'NONE',  ( 8.387690588348714726, 12.93738945304888333, 1.040834085586084257E-14 ) ) ;
#42432 = CARTESIAN_POINT ( 'NONE',  ( -4.749098946536820520, 8.762642214260091933, 0.7998128361456281477 ) ) ;
#42433 = CARTESIAN_POINT ( 'NONE',  ( 3.105210138592546798, -0.4252477525170209605, 2.149737936336936883 ) ) ;
#42434 = DIRECTION ( 'NONE',  ( 1.214306433183764966E-17, 1.000000000000000000, 5.200009205990155575E-32 ) ) ;
#42435 = CARTESIAN_POINT ( 'NONE',  ( 6.016786309414542622, 10.24161080428416426, 0.7998128361456341429 ) ) ;
#42436 = DIRECTION ( 'NONE',  ( 0.000000000000000000, -1.000000000000000000, 0.000000000000000000 ) ) ;
#42437 = CARTESIAN_POINT ( 'NONE',  ( 3.035583632137848653, -1.226507576337819483, -1.352503160878690380 ) ) ;
#42438 = PRESENTATION_STYLE_ASSIGNMENT (( #189719 ) ) ;
#42439 = CARTESIAN_POINT ( 'NONE',  ( -10.33094986393327197, 11.15512238411806578, 0.7216878364870438212 ) ) ;
#42440 = AXIS2_PLACEMENT_3D ( 'NONE', #156604, #120971, #59081 ) ;
#42441 = CARTESIAN_POINT ( 'NONE',  ( -5.594533863947632746, 7.496198557292433229, -1.347124935377568722 ) ) ;
#42442 = FACE_OUTER_BOUND ( 'NONE', #61707, .T. ) ;
#42443 = CARTESIAN_POINT ( 'NONE',  ( 7.567422294721922960, 11.98040977715095323, 0.7998128361456462443 ) ) ;
#42444 = AXIS2_PLACEMENT_3D ( 'NONE', #120941, #103545, #169606 ) ;
#42445 = CARTESIAN_POINT ( 'NONE',  ( 0.5395173010800574653, -1.361483316988669978, -1.363248745070398726 ) ) ;
#42446 = CARTESIAN_POINT ( 'NONE',  ( 5.330891710049517229, -1.845885424482188286, -0.6645199359083459045 ) ) ;
#42447 = CARTESIAN_POINT ( 'NONE',  ( 1.500000000000001332, 14.87500000000000000, 0.000000000000000000 ) ) ;
#42448 = CARTESIAN_POINT ( 'NONE',  ( -5.689618019229208734, 9.789638122409414223, 0.7998128361456481317 ) ) ;
#42449 = CARTESIAN_POINT ( 'NONE',  ( 4.961394147597008697, 7.875711374583454827, -1.199719254218452047 ) ) ;
#42450 = CARTESIAN_POINT ( 'NONE',  ( 4.458633810090739225, -1.957822973221786444, -0.9849130632908836835 ) ) ;
#42451 = CARTESIAN_POINT ( 'NONE',  ( 3.686212053427321056, 6.121915856213854923, 1.284222742053100941 ) ) ;
#42452 = CARTESIAN_POINT ( 'NONE',  ( -3.795919822146293754, 4.491289883001181593, -1.082531754730549967 ) ) ;
#42453 = CARTESIAN_POINT ( 'NONE',  ( 4.961816271168416392, -0.5573412460852051886, 1.993729458732765858 ) ) ;
#42454 = CARTESIAN_POINT ( 'NONE',  ( 1.364683531249988757, 2.196875000341415252, 1.214306433183764966E-14 ) ) ;
#42455 = CARTESIAN_POINT ( 'NONE',  ( 4.711759750379289180, 2.199509664246365848, 0.6680300025654511975 ) ) ;
#42456 = CARTESIAN_POINT ( 'NONE',  ( 5.775410249741494972, 8.721433810464993996, -1.082531754730537088 ) ) ;
#42457 = CARTESIAN_POINT ( 'NONE',  ( 4.828112100242277549, 6.726159765073026264, -1.443375672974068769 ) ) ;
#42458 = CARTESIAN_POINT ( 'NONE',  ( 0.7973255588549054140, 1.877056169618742443, 1.315483550797888812 ) ) ;
#42459 = CARTESIAN_POINT ( 'NONE',  ( -11.55950211276791428, 13.87999999999998302, 3.221476510067114329 ) ) ;
#42460 = CARTESIAN_POINT ( 'NONE',  ( -6.882699257592852504, 8.058845884393651460, -1.199719254218452047 ) ) ;
#42461 = CARTESIAN_POINT ( 'NONE',  ( 4.804598357785225815, 1.690330731384475094, 0.9558792251623483560 ) ) ;
#42462 = VERTEX_POINT ( 'NONE', #161629 ) ;
#42463 = CARTESIAN_POINT ( 'NONE',  ( 8.202319746143333035, 12.51319743723517952, -0.7216878364870328300 ) ) ;
#42464 = ORIENTED_EDGE ( 'NONE', *, *, #5717, .F. ) ;
#42465 = CARTESIAN_POINT ( 'NONE',  ( 5.150612376422202487, 1.885107930906554152, 0.3209214958604587054 ) ) ;
#42466 = CARTESIAN_POINT ( 'NONE',  ( 6.211878148792838061, -1.711051158068075839, 0.2163953478501578487 ) ) ;
#42467 = CARTESIAN_POINT ( 'NONE',  ( 5.419157771004846857, -1.820987890746316173, 0.8666037247077316152 ) ) ;
#42469 = CARTESIAN_POINT ( 'NONE',  ( -3.187575512988701565, 6.732938841879847480, 0.000000000000000000 ) ) ;
#42468 = CARTESIAN_POINT ( 'NONE',  ( -9.691380875670077444, 10.20103253123691189, 0.7998128361456462443 ) ) ;
#42470 = CARTESIAN_POINT ( 'NONE',  ( -3.285556943749998737, -2.267708332855375986, 1.896917185911908499 ) ) ;
#42472 = CARTESIAN_POINT ( 'NONE',  ( 0.4613126893583847643, 1.751520745650859912, -0.2531317886874852041 ) ) ;
#42471 = CARTESIAN_POINT ( 'NONE',  ( 1.535224857807856669, -1.515203476157600537, -1.440707689706053563 ) ) ;
#42473 = CARTESIAN_POINT ( 'NONE',  ( 5.520157785563180930, -1.821743191724470634, 0.8647220171385738841 ) ) ;
#42475 = CARTESIAN_POINT ( 'NONE',  ( 3.468945898361298408, 0.05672114714776231581, -2.291715584554415930 ) ) ;
#42474 = CARTESIAN_POINT ( 'NONE',  ( 4.115782150200256950, 6.959440387612411349, 1.199719254218452047 ) ) ;
#42476 = CARTESIAN_POINT ( 'NONE',  ( 1.886251080576596406, 1.515106702303461894, -0.8561229301769134326 ) ) ;
#42477 = AXIS2_PLACEMENT_3D ( 'NONE', #63418, #159850, #164124 ) ;
#42478 = CARTESIAN_POINT ( 'NONE',  ( 3.111701630267147412, 1.674174984267240429, 1.301503359413098249 ) ) ;
#42479 = DIRECTION ( 'NONE',  ( -0.2553555850663286608, -0.9650793847679529636, 0.05844062175698114953 ) ) ;
#42480 = CARTESIAN_POINT ( 'NONE',  ( 1.739138385086140159, -1.644397438216003593, -0.5498640316261136363 ) ) ;
#42481 = CARTESIAN_POINT ( 'NONE',  ( 1.360316468749971808, 2.567708333674758148, -0.7853790794159301036 ) ) ;
#42482 = CARTESIAN_POINT ( 'NONE',  ( 2.154548830654204217, -0.4927303200079625745, -1.794580903941452865 ) ) ;
#42483 = CARTESIAN_POINT ( 'NONE',  ( 2.330757530436095237, -1.336968151498512336, 1.710609410560095522 ) ) ;
#42484 = CARTESIAN_POINT ( 'NONE',  ( 3.239470508323912146, 0.4852670486454255250, -1.957170429962351577 ) ) ;
#42485 = CARTESIAN_POINT ( 'NONE',  ( 4.312500000000001776, 1.451031289061289531, 1.451031289060941587 ) ) ;
#42486 = CARTESIAN_POINT ( 'NONE',  ( -1.402160292154681736E-14, 1.868750000682816381, -1.732050807568863648 ) ) ;
#42487 = CARTESIAN_POINT ( 'NONE',  ( 1.465712096425618949, 1.898328545170711035, -0.3267402372346754902 ) ) ;
#42488 = CARTESIAN_POINT ( 'NONE',  ( 0.6823417656249969321, 14.52604166700806410, -1.181850606188757036 ) ) ;
#42489 = CARTESIAN_POINT ( 'NONE',  ( 3.287547529179511319, 0.05108950329585186523, -2.220969887641692342 ) ) ;
#42490 = ORIENTED_EDGE ( 'NONE', *, *, #192621, .T. ) ;
#42491 = CARTESIAN_POINT ( 'NONE',  ( -0.2108831679770960255, 0.2438762813419328990, -1.931650693707862132 ) ) ;
#42492 = CARTESIAN_POINT ( 'NONE',  ( 0.7499999999999885647, 0.8166666666666877461, -1.299038105676652899 ) ) ;
#42493 = CARTESIAN_POINT ( 'NONE',  ( 7.396136491454752715, 8.587579647240744407, 1.199719254218462483 ) ) ;
#42494 = B_SPLINE_CURVE_WITH_KNOTS ( 'NONE', 3,
 ( #186169, #19402, #199207, #50854, #86552, #100664 ),
 .UNSPECIFIED., .F., .F.,
 ( 4, 2, 4 ),
 ( 0.000000000000000000, 0.001225895755212360596, 0.002451791510424720759 ),
 .UNSPECIFIED. ) ;
#42495 = CARTESIAN_POINT ( 'NONE',  ( -1.402160292154681736E-14, 0.1968750003414221628, -1.575800808251665908 ) ) ;
#42496 = CARTESIAN_POINT ( 'NONE',  ( 5.678047454291774265, 2.188620968312010362, -0.3794988778502098592 ) ) ;
#42498 = ADVANCED_FACE ( 'NONE', ( #93438, #193030 ), #94507, .T. ) ;
#42497 = CARTESIAN_POINT ( 'NONE',  ( 5.125427350195786325, 0.1941421753944693185, -1.952251141935714918 ) ) ;
#42500 = CARTESIAN_POINT ( 'NONE',  ( -7.076992996653451939, 7.358839372291564374, 0.7216878364870317197 ) ) ;
#42499 = CARTESIAN_POINT ( 'NONE',  ( 9.625925876022625616, 11.29296361252366765, -1.082531754730537088 ) ) ;
#42501 = CARTESIAN_POINT ( 'NONE',  ( 6.204402397823557180, -0.8056473179405240215, -2.114295379420629839 ) ) ;
#42502 = CIRCLE ( 'NONE', #97844, 12.00000000000000178 ) ;
#42504 = AXIS2_PLACEMENT_3D ( 'NONE', #154439, #171745, #72089 ) ;
#42503 = CARTESIAN_POINT ( 'NONE',  ( -6.631346530859867805, 6.909194838857525944, 0.000000000000000000 ) ) ;
#42505 = CARTESIAN_POINT ( 'NONE',  ( 1.785667050844968351, -1.942997710132963407, 0.6927838567832644845 ) ) ;
#42506 = CARTESIAN_POINT ( 'NONE',  ( -5.636439174979254396, 7.598931675607687453, -1.599625672291256295 ) ) ;
#42507 = EDGE_LOOP ( 'NONE', ( #71226, #205815, #193872, #50731 ) ) ;
#42508 = CARTESIAN_POINT ( 'NONE',  ( 1.499999999999989120, 2.035416667349480679, 0.8660254037844524744 ) ) ;
#42509 = CARTESIAN_POINT ( 'NONE',  ( -1.201851678989727383E-14, 4.759375000341419693, -1.575800808251660134 ) ) ;
#42510 = CARTESIAN_POINT ( 'NONE',  ( 3.831198023013999698, -1.729401117988647929, 0.7132991360168300377 ) ) ;
#42511 = CARTESIAN_POINT ( 'NONE',  ( 3.023724745236521017, -1.528101708971361106, 0.8198667277116710173 ) ) ;
#42512 = CARTESIAN_POINT ( 'NONE',  ( 6.286699343557897279, 1.907799665397521105, -1.078441415684105120 ) ) ;
#42513 = CARTESIAN_POINT ( 'NONE',  ( 0.5345543961663907773, 1.132513062451316221, -1.893880525681296723 ) ) ;
#42514 = CARTESIAN_POINT ( 'NONE',  ( 4.722262070665103728, 2.001137821747037915, 0.6055792653000735548 ) ) ;
#42515 = CARTESIAN_POINT ( 'NONE',  ( 5.947205882781483766, 0.5613781043299302942, -1.859040749089553524 ) ) ;
#42516 = CARTESIAN_POINT ( 'NONE',  ( 9.289939459345561090, 13.86364823901540788, 7.523963912448549785 ) ) ;
#42517 = CARTESIAN_POINT ( 'NONE',  ( 0.3437500000590538174, 1.895863741711102612, 0.7852924748299703328 ) ) ;
#42518 = CARTESIAN_POINT ( 'NONE',  ( -0.01695367945527340853, -2.016028864686558730, -0.04667425414178058563 ) ) ;
#42520 = EDGE_CURVE ( 'NONE', #195087, #142577, #75757, .T. ) ;
#42519 = FILL_AREA_STYLE ('',( #190858 ) ) ;
#42521 = SURFACE_SIDE_STYLE ('',( #204968 ) ) ;
#42523 =( NAMED_UNIT ( * ) PLANE_ANGLE_UNIT ( ) SI_UNIT ( $, .RADIAN. ) );
#42522 = AXIS2_PLACEMENT_3D ( 'NONE', #31549, #213455, #65079 ) ;
#42524 = CARTESIAN_POINT ( 'NONE',  ( -7.492852449846775897, 11.89341162479659531, 0.000000000000000000 ) ) ;
#42525 = CARTESIAN_POINT ( 'NONE',  ( 8.145751363712157911, 8.397798100619326078, -0.7998128361456281477 ) ) ;
#42526 = CARTESIAN_POINT ( 'NONE',  ( 0.000000000000000000, 4.000000000000003553, 0.000000000000000000 ) ) ;
#42527 = CARTESIAN_POINT ( 'NONE',  ( 3.861776535121093090, 1.811678901967550326, -0.2252020330209548171 ) ) ;
#42528 = CARTESIAN_POINT ( 'NONE',  ( 1.800138458411651765, -0.7431416638853625134, 2.077998897882806784 ) ) ;
#42529 = ORIENTED_EDGE ( 'NONE', *, *, #208952, .F. ) ;
#42530 = B_SPLINE_CURVE_WITH_KNOTS ( 'NONE', 3,
 ( #184341, #15436, #100958, #198451, #165972, #114106, #148666, #232, #31721, #50097 ),
 .UNSPECIFIED., .F., .F.,
 ( 4, 3, 3, 4 ),
 ( 1.084202172485514786E-19, 3.125153504173336036E-05, 6.280295210142521956E-05, 9.436679189892625938E-05 ),
 .UNSPECIFIED. ) ;
#42531 = CARTESIAN_POINT ( 'NONE',  ( -3.973948422136981407, 5.729635473950147606, -1.443375672974066548 ) ) ;
#42532 = CARTESIAN_POINT ( 'NONE',  ( 1.642778471875000035, -2.763541666188709556, -2.845375778867859751 ) ) ;
#42533 = CARTESIAN_POINT ( 'NONE',  ( -7.212047647465563038, 10.50147379109678880, -1.199719254218446718 ) ) ;
#42534 = CARTESIAN_POINT ( 'NONE',  ( 1.529563250702131727, -0.2428666551740152890, 2.005035470024270960 ) ) ;
#42536 = CARTESIAN_POINT ( 'NONE',  ( 11.88168329227127096, 9.719999999999982876, 1.685799833707125606 ) ) ;
#42535 = VECTOR ( 'NONE', #166839, 1000.000000000000000 ) ;
#42537 = ORIENTED_EDGE ( 'NONE', *, *, #155510, .T. ) ;
#42538 = CARTESIAN_POINT ( 'NONE',  ( -4.228163802615396705, 6.026220084508304708, -1.599625672291271394 ) ) ;
#42539 = CARTESIAN_POINT ( 'NONE',  ( 2.729178580549945110, 0.09652143117058623045, -1.858595261477024918 ) ) ;
#42540 = CARTESIAN_POINT ( 'NONE',  ( 4.054051625686104998, 4.688480637177271149, -1.199719254218446718 ) ) ;
#42541 = CARTESIAN_POINT ( 'NONE',  ( 11.55950211276791251, 9.719999999999982876, 3.221476510067110777 ) ) ;
#42542 = ORIENTED_EDGE ( 'NONE', *, *, #54037, .F. ) ;
#42543 = ORIENTED_EDGE ( 'NONE', *, *, #126711, .F. ) ;
#42544 = CARTESIAN_POINT ( 'NONE',  ( -9.508345801885592863, 9.987491611821676329, 0.7998128361456462443 ) ) ;
#42545 = CARTESIAN_POINT ( 'NONE',  ( 4.441915170580639227, 0.7783198120194650960, -1.651611053696280695 ) ) ;
#42548 = ORIENTED_EDGE ( 'NONE', *, *, #121060, .F. ) ;
#42547 = CARTESIAN_POINT ( 'NONE',  ( -5.285102783734889620, 6.572932445422958736, -1.390504041276509062 ) ) ;
#42546 = CARTESIAN_POINT ( 'NONE',  ( -3.654804927335652209, 6.421633627603656080, 1.199719254218452935 ) ) ;
#42549 = CARTESIAN_POINT ( 'NONE',  ( 6.252685474373055996, 7.003816019006632310, -0.9791501464874209359 ) ) ;
#42550 = CARTESIAN_POINT ( 'NONE',  ( 0.7019813383442319310, -1.220362748482771487, -1.231932065070516558 ) ) ;
#42551 = CARTESIAN_POINT ( 'NONE',  ( 5.806566994037906326, 1.625791660643903791, 0.8640615347050364381 ) ) ;
#42552 = CARTESIAN_POINT ( 'NONE',  ( 4.688248866636615553, -1.090845489383242883, 2.033590232148785759 ) ) ;
#42553 = CARTESIAN_POINT ( 'NONE',  ( 5.890091390494168522, 5.836471141856793388, 0.000000000000000000 ) ) ;
#42554 = CARTESIAN_POINT ( 'NONE',  ( 6.538358481810655043, 2.137031053877674225, 0.3242996077847115632 ) ) ;
#42555 = CARTESIAN_POINT ( 'NONE',  ( 5.686755365928134687, 8.721966129303114101, 1.199719254218462483 ) ) ;
#42556 = CARTESIAN_POINT ( 'NONE',  ( 5.817770776407988009, -1.817369610395104695, 1.406990027747441419 ) ) ;
#42557 = CARTESIAN_POINT ( 'NONE',  ( -1.565491486567922363, -3.232243495192119731, 2.892400742676151104 ) ) ;
#42558 = CARTESIAN_POINT ( 'NONE',  ( -3.006876207180748217, 6.730049018344652190, -0.7998128361456481317 ) ) ;
#42559 = CARTESIAN_POINT ( 'NONE',  ( 5.313307075269409374, -0.2735208697075517947, 1.850433306854900817 ) ) ;
#42560 = ORIENTED_EDGE ( 'NONE', *, *, #13809, .T. ) ;
#42562 = CARTESIAN_POINT ( 'NONE',  ( -5.984998465789844069, 5.947196063035064206, 0.7998128361456281477 ) ) ;
#42561 = CARTESIAN_POINT ( 'NONE',  ( 2.531394148431935776, -0.1834752923718513118, 1.903540536635806912 ) ) ;
#42563 = CARTESIAN_POINT ( 'NONE',  ( 4.424592250794217030, 1.359014646446855767, -1.738718759629574118 ) ) ;
#42564 = CARTESIAN_POINT ( 'NONE',  ( 4.469977352714805008, -0.9950975051371075963, 1.868896417504315677 ) ) ;
#42565 = CARTESIAN_POINT ( 'NONE',  ( -1.225000000000003864, 0.8125000006827948207, -3.469446951953614189E-15 ) ) ;
#42566 = CARTESIAN_POINT ( 'NONE',  ( 6.883263157960405998, 2.961743250487959056, 2.498998094365055600 ) ) ;
#42567 = CARTESIAN_POINT ( 'NONE',  ( -0.2108831679771203116, 0.7314853703891763814, -1.979988191570913880 ) ) ;
#42568 = CARTESIAN_POINT ( 'NONE',  ( 5.519577934094852978, 7.532869904567736974, 1.443375672974064550 ) ) ;
#42569 = CARTESIAN_POINT ( 'NONE',  ( -5.777182852754558340, 5.912670547734647286, 0.000000000000000000 ) ) ;
#42570 = CARTESIAN_POINT ( 'NONE',  ( 1.923324260599985402, 2.153519634812319783, 0.8294600792757185204 ) ) ;
#42571 = CARTESIAN_POINT ( 'NONE',  ( 2.031626174157370457, 1.878314540015123102, -0.5664888411779643862 ) ) ;
#42572 = DIRECTION ( 'NONE',  ( 0.000000000000000000, 1.000000000000000000, 0.000000000000000000 ) ) ;
#42573 = CARTESIAN_POINT ( 'NONE',  ( 6.526245194314398645, 1.055377990298064450, 1.771961156250308145 ) ) ;
#42574 = CARTESIAN_POINT ( 'NONE',  ( 4.880572111239557920, 4.796348339308675435, -0.7216878364870197293 ) ) ;
#42575 = CARTESIAN_POINT ( 'NONE',  ( 4.083220446344194343, 1.622485107653489633, 1.197306254465977826 ) ) ;
#42576 = CARTESIAN_POINT ( 'NONE',  ( 4.848976215542928792, 5.686169002002086970, 1.199719254218452047 ) ) ;
#42577 = ORIENTED_EDGE ( 'NONE', *, *, #36782, .F. ) ;
#42578 = CARTESIAN_POINT ( 'NONE',  ( 4.399625206644591557, -1.976670321813909892, 0.3981083777728141038 ) ) ;
#42579 = CARTESIAN_POINT ( 'NONE',  ( -10.32183501870554387, 10.93656236477829502, 0.7998128361456462443 ) ) ;
#42580 = FACE_OUTER_BOUND ( 'NONE', #56307, .T. ) ;
#42581 = CARTESIAN_POINT ( 'NONE',  ( 9.049177462117294013, 12.64479190819049670, -1.199719254218446718 ) ) ;
#42582 = CARTESIAN_POINT ( 'NONE',  ( 2.501036472447940362, 0.4719354416190780777, 2.119019701963683833 ) ) ;
#42583 = CARTESIAN_POINT ( 'NONE',  ( 4.692003678781083487, 7.631698837623355658, -1.199719254218450271 ) ) ;
#42584 = CARTESIAN_POINT ( 'NONE',  ( -1.797327170199077839, 14.52975892672686342, -11.89862072626474898 ) ) ;
#42585 =( NAMED_UNIT ( * ) PLANE_ANGLE_UNIT ( ) SI_UNIT ( $, .RADIAN. ) );
#42586 = CARTESIAN_POINT ( 'NONE',  ( 2.055717040066493695, 1.865871300129381183, -0.1328275987748789300 ) ) ;
#42587 = CARTESIAN_POINT ( 'NONE',  ( 6.204392391313840349, -0.7715976231806520591, -2.019385000091134419 ) ) ;
#42589 = CARTESIAN_POINT ( 'NONE',  ( 0.4019237886466778820, 8.354914550367425363, 1.500000000000001554 ) ) ;
#42588 = CARTESIAN_POINT ( 'NONE',  ( -0.02244404828160087226, 1.995160441984781041, -2.602654351998904492 ) ) ;
#42590 = CARTESIAN_POINT ( 'NONE',  ( -1.402160292154681736E-14, 0.1968750003414221628, -1.575800808251665908 ) ) ;
#42591 = EDGE_LOOP ( 'NONE', ( #100847, #12155, #44292, #140439 ) ) ;
#42592 = CARTESIAN_POINT ( 'NONE',  ( 3.721269560815092525, 1.641568950759502377, 0.9805937191851579193 ) ) ;
#42593 = VECTOR ( 'NONE', #178493, 1000.000000000000000 ) ;
#42594 = CARTESIAN_POINT ( 'NONE',  ( 4.258513496744737559, -1.310932089386746879, 1.189237179687177015 ) ) ;
#42595 = CARTESIAN_POINT ( 'NONE',  ( 1.506358462150747091, -1.903157483220425883, -0.1863595701613318389 ) ) ;
#42596 = CARTESIAN_POINT ( 'NONE',  ( -4.603156847039612920, 5.329103395422994716, 1.199719254218462483 ) ) ;
#42597 = CARTESIAN_POINT ( 'NONE',  ( -0.1181432109131977104, -1.915350881444439102, -0.04437447078771068754 ) ) ;
#42598 = CARTESIAN_POINT ( 'NONE',  ( 0.7499999999999867883, -0.1833333333333131421, -1.299038105676652899 ) ) ;
#42599 = CARTESIAN_POINT ( 'NONE',  ( 0.9067890187421032699, 0.5993529260880943177, 1.981728858978973218 ) ) ;
#42600 = CARTESIAN_POINT ( 'NONE',  ( 1.499999999999989120, 5.504166666666685970, 0.8660254037844524744 ) ) ;
#42601 = CARTESIAN_POINT ( 'NONE',  ( 6.719622092096638966, -1.813896567892055112, 0.4569536213836836169 ) ) ;
#42602 = CARTESIAN_POINT ( 'NONE',  ( 1.717148762710469789, -0.2249250470785572054, 1.811706739299999924 ) ) ;
#42604 = CARTESIAN_POINT ( 'NONE',  ( 4.954704567260191261, 7.963257648925383236, 1.029694947009308859 ) ) ;
#42603 = CARTESIAN_POINT ( 'NONE',  ( 5.672569038193632451, -1.402732290180560337, 1.703733612381942653 ) ) ;
#42605 = CARTESIAN_POINT ( 'NONE',  ( -0.6823417656250246877, -0.1989583329919109023, 1.181850606188755259 ) ) ;
#42606 = CARTESIAN_POINT ( 'NONE',  ( 3.543474241949475356, 1.865888119384132127, -0.8795106731672995837 ) ) ;
#42607 = CARTESIAN_POINT ( 'NONE',  ( -6.256197817702116026, 9.386315656372753224, -1.199719254218440723 ) ) ;
#42608 = CARTESIAN_POINT ( 'NONE',  ( 7.540305987494599016, 11.94877408538573427, -0.7998128361456291469 ) ) ;
#42609 = CARTESIAN_POINT ( 'NONE',  ( 1.499577476386907637, 3.250920186034359727, -0.09296422598485129529 ) ) ;
#42610 = CARTESIAN_POINT ( 'NONE',  ( -0.1000000000000080685, -9.999999999999994671, -10.91954211494235238 ) ) ;
#42611 = CARTESIAN_POINT ( 'NONE',  ( 5.830888582329017744, 8.960397891762626799, -1.199719254218452047 ) ) ;
#42612 = CARTESIAN_POINT ( 'NONE',  ( 5.828598057497599960, -1.316348130051235410, 1.597988563933512074 ) ) ;
#42613 = CARTESIAN_POINT ( 'NONE',  ( 1.364683531249988757, 0.6968750003414209138, 0.000000000000000000 ) ) ;
#42614 = CARTESIAN_POINT ( 'NONE',  ( 2.759224924868249662, -1.879262701025650850, -1.068020781904190253 ) ) ;
#42615 = CARTESIAN_POINT ( 'NONE',  ( -4.864640111294652236, 8.076240785039992431, 0.9165970657895030627 ) ) ;
#42617 = CARTESIAN_POINT ( 'NONE',  ( 2.031626174157370457, 1.878314540015123102, -0.5664888411779643862 ) ) ;
#42616 = CARTESIAN_POINT ( 'NONE',  ( 2.824872690137433029, 1.461285568133148693, -1.394416722739227898 ) ) ;
#42618 = CARTESIAN_POINT ( 'NONE',  ( 6.620655732516645742, 7.051964633898824886, 2.771890290588132189 ) ) ;
#42621 = CARTESIAN_POINT ( 'NONE',  ( 6.155038550924144758, 8.203964280876741455, 1.443375672974076540 ) ) ;
#42620 = CARTESIAN_POINT ( 'NONE',  ( 3.475000000000000533, -1.604166666666667629, 2.006292185433948827 ) ) ;
#42619 = PRESENTATION_STYLE_ASSIGNMENT (( #176865 ) ) ;
#42622 = CARTESIAN_POINT ( 'NONE',  ( -7.781453819600577582, 8.043060642480948985, 0.000000000000000000 ) ) ;
#42623 = CARTESIAN_POINT ( 'NONE',  ( 1.745327705122714956, 0.3399549603602426417, -1.987498286102694411 ) ) ;
#42625 = CARTESIAN_POINT ( 'NONE',  ( 5.829655996829377962, 1.081331853127937448, -1.906115348727636549 ) ) ;
#42624 = CARTESIAN_POINT ( 'NONE',  ( -4.218558352146454915, 8.073401844146177453, 1.040834085586084257E-14 ) ) ;
#42626 = CARTESIAN_POINT ( 'NONE',  ( 1.499999999999990896, 5.556250000682820378, 1.214306433183764966E-14 ) ) ;
#42627 = CARTESIAN_POINT ( 'NONE',  ( 6.029550621839829816, -0.2273517531893587407, 1.898748578088353733 ) ) ;
#42628 = CARTESIAN_POINT ( 'NONE',  ( -11.97297122925973767, 12.30125079326911042, 0.8121202983519304475 ) ) ;
#42629 = EDGE_CURVE ( 'NONE', #50158, #211239, #202984, .T. ) ;
#42630 = CARTESIAN_POINT ( 'NONE',  ( 6.005898860729467437, 7.069598761348265370, -1.082531754730543083 ) ) ;
#42632 = CARTESIAN_POINT ( 'NONE',  ( 3.532827515057835654, -1.646827434736859441, 1.163287548526056980 ) ) ;
#42631 = CARTESIAN_POINT ( 'NONE',  ( -9.612367721964622191, 10.31677655182129527, -0.7216878364870267237 ) ) ;
#42633 = CARTESIAN_POINT ( 'NONE',  ( -1.500000000000011324, 4.170833333333359150, 0.8660254037844403729 ) ) ;
#42634 = CARTESIAN_POINT ( 'NONE',  ( 0.6823417656249969321, 14.08854166700806232, -1.181850606188757036 ) ) ;
#42635 = CARTESIAN_POINT ( 'NONE',  ( 4.893404818765360709, 1.279633041931761639, 1.156618277182480892 ) ) ;
#42636 = CARTESIAN_POINT ( 'NONE',  ( 5.528692779322568640, 9.672168352510192690, 0.7998128361456341429 ) ) ;
#42637 = AXIS2_PLACEMENT_3D ( 'NONE', #145810, #111207, #211817 ) ;
#42638 = CARTESIAN_POINT ( 'NONE',  ( 9.625925876022625616, 11.29296361252366765, -1.082531754730537088 ) ) ;
#42639 = CYLINDRICAL_SURFACE ( 'NONE', #150746, 0.08000000000000020983 ) ;
#42640 = CARTESIAN_POINT ( 'NONE',  ( 4.165207536865437099, 0.2314014899743311315, -1.856129391651973215 ) ) ;
#42641 = DIRECTION ( 'NONE',  ( 0.7071067811865465735, 0.7071067811865483499, 8.659560562354921765E-17 ) ) ;
#42642 = CARTESIAN_POINT ( 'NONE',  ( 1.586871713678970730, 1.994102569620255228, 0.5559867524188369936 ) ) ;
#42643 = CARTESIAN_POINT ( 'NONE',  ( 6.795378861676105053, -1.851214886592133846, 0.9271815693319698237 ) ) ;
#42644 = CARTESIAN_POINT ( 'NONE',  ( 4.903208829997618423, 5.749440385532527564, -1.199719254218450271 ) ) ;
#42645 = CARTESIAN_POINT ( 'NONE',  ( -4.355418974009601207, 3.138960640472630459, -0.7749999999999935829 ) ) ;
#42646 = CARTESIAN_POINT ( 'NONE',  ( 0.1404700283944440298, 1.733558474490008772, 0.5260085833052421389 ) ) ;
#42647 = CARTESIAN_POINT ( 'NONE',  ( 6.333067150914820864, 6.561202228921677815, 0.7216878364870328300 ) ) ;
#42648 = CARTESIAN_POINT ( 'NONE',  ( 10.26863146610705613, 10.84983613121963941, 6.215114292131002749 ) ) ;
#42649 = ORIENTED_EDGE ( 'NONE', *, *, #180280, .T. ) ;
#42650 = CARTESIAN_POINT ( 'NONE',  ( 8.717529583462646059, 11.19353715217169309, 1.443375672974076540 ) ) ;
#42652 = CARTESIAN_POINT ( 'NONE',  ( 8.762647353133951711, 9.117510088278095282, 1.040834085586084257E-14 ) ) ;
#42651 = CARTESIAN_POINT ( 'NONE',  ( 1.012071980069819910, 1.959787197952606252, -0.09269708818125664551 ) ) ;
#42653 = CARTESIAN_POINT ( 'NONE',  ( 5.290618452874795707, 1.447395081947447704, -1.254909122497225971 ) ) ;
#42654 = AXIS2_PLACEMENT_3D ( 'NONE', #82400, #84537, #132264 ) ;
#42655 = CARTESIAN_POINT ( 'NONE',  ( -11.41381675112459959, 13.39999999999999325, 3.704697986577257129 ) ) ;
#42656 = DIRECTION ( 'NONE',  ( -0.000000000000000000, 1.000000000000000000, 0.000000000000000000 ) ) ;
#42657 = ADVANCED_FACE ( 'NONE', ( #47897 ), #20400, .T. ) ;
#42658 = DIRECTION ( 'NONE',  ( -1.000000000000000000, 0.000000000000000000, 0.000000000000000000 ) ) ;
#42660 = VERTEX_POINT ( 'NONE', #64119 ) ;
#42659 = CARTESIAN_POINT ( 'NONE',  ( 4.853455804012228647, 4.764712647543454693, 0.7216878364870317197 ) ) ;
#42661 = CARTESIAN_POINT ( 'NONE',  ( -8.405692050792730186, 9.869357483088723626, 1.082531754730558626 ) ) ;
#42662 = CARTESIAN_POINT ( 'NONE',  ( 3.555696680978126079, 0.5271953485486252644, -2.096301903996622862 ) ) ;
#42663 = CARTESIAN_POINT ( 'NONE',  ( -5.157951095356222204, 4.982307464195829816, 0.000000000000000000 ) ) ;
#42664 = CARTESIAN_POINT ( 'NONE',  ( 5.546694241766559230, 9.485244025454063532, 0.000000000000000000 ) ) ;
#42665 = CARTESIAN_POINT ( 'NONE',  ( -2.103486388414573138, 5.605817886458954291, 1.040834085586084257E-14 ) ) ;
#42666 = CARTESIAN_POINT ( 'NONE',  ( 4.858326754937916547, 0.6996357133068829004, 1.686392194618462570 ) ) ;
#42667 = CIRCLE ( 'NONE', #104967, 0.07999999999999998779 ) ;
#42668 = CARTESIAN_POINT ( 'NONE',  ( 11.23288463952165550, 7.775932670961701376, -5.438141635970919374 ) ) ;
#42669 = CARTESIAN_POINT ( 'NONE',  ( 0.8605430240068573378, -1.430899983082928761, 1.356264857227080567 ) ) ;
#42670 = CARTESIAN_POINT ( 'NONE',  ( 3.480628297764537304, -1.280852673386581264, 1.420289963180096260 ) ) ;
#42671 = ORIENTED_EDGE ( 'NONE', *, *, #41266, .F. ) ;
#42672 = CARTESIAN_POINT ( 'NONE',  ( -9.367496997901325173, 14.48154074412966175, -7.499999999620646562 ) ) ;
#42673 = CARTESIAN_POINT ( 'NONE',  ( 5.213322861785598228, -1.662839039401903696, -1.055205849181278799 ) ) ;
#42674 = VERTEX_POINT ( 'NONE', #175743 ) ;
#42676 = B_SPLINE_CURVE_WITH_KNOTS ( 'NONE', 3,
 ( #169828, #84307, #150392, #87524, #51825, #134163, #56087, #104848, #5159, #170894, #200172, #137351, #22486, #203368 ),
 .UNSPECIFIED., .F., .F.,
 ( 4, 2, 2, 2, 2, 2, 4 ),
 ( 0.001872291076883575130, 0.002107054070182344009, 0.002341817063481112671, 0.002811343050078650863, 0.003280869036676186019, 0.003515632029974954248, 0.003750395023273722043 ),
 .UNSPECIFIED. ) ;
#42675 = CARTESIAN_POINT ( 'NONE',  ( 6.058146487192490603, -1.370253782545840293, 1.376481248621561182 ) ) ;
#42677 = EDGE_LOOP ( 'NONE', ( #111729, #182209, #116212, #29471 ) ) ;
#42678 = CARTESIAN_POINT ( 'NONE',  ( -6.798487682609798632, 6.896266815991691779, 0.7998128361456341429 ) ) ;
#42680 = CARTESIAN_POINT ( 'NONE',  ( 7.100579091572746471, -6.583980363594995389, -6.484567079770767961 ) ) ;
#42679 = CARTESIAN_POINT ( 'NONE',  ( -4.339491684825780737, 7.220434844675483355, -1.199719254218455378 ) ) ;
#42681 = CARTESIAN_POINT ( 'NONE',  ( 7.797347741190739256, 8.269529584243604958, 0.7216878364870267237 ) ) ;
#42683 = ORIENTED_EDGE ( 'NONE', *, *, #188635, .F. ) ;
#42682 = CARTESIAN_POINT ( 'NONE',  ( 3.475170734053119048, -1.687717282722025924, -0.8990902037325496643 ) ) ;
#42684 = VECTOR ( 'NONE', #202834, 1000.000000000000114 ) ;
#42685 = CARTESIAN_POINT ( 'NONE',  ( -15.75000000000000000, 13.79999999999999893, 0.6999999999999992895 ) ) ;
#42686 = CARTESIAN_POINT ( 'NONE',  ( 9.574755896318496440, 4.231292707087964011, -7.158835548396402793 ) ) ;
#42687 = CARTESIAN_POINT ( 'NONE',  ( 4.670568766136569572, 0.7725349690445941775, 1.859148924064259356 ) ) ;
#42688 = CARTESIAN_POINT ( 'NONE',  ( 0.3461162505575273163, 7.159215625956777629, 1.970439023737499351 ) ) ;
#42690 = CARTESIAN_POINT ( 'NONE',  ( 5.489470343000498076, -0.4852711138302409077, 1.957169415941109047 ) ) ;
#42689 = CARTESIAN_POINT ( 'NONE',  ( 6.322862864304120478, 1.705426906915354035, 0.6521430802832667295 ) ) ;
#42691 = CARTESIAN_POINT ( 'NONE',  ( 6.727182134110208267, 1.290711256955964448, 1.927001067762003750 ) ) ;
#42692 = CARTESIAN_POINT ( 'NONE',  ( 1.926316106172959230, 1.062450747350886848, 1.776810178100460824 ) ) ;
#42693 = CARTESIAN_POINT ( 'NONE',  ( -7.576308911938196999, 7.733448573549685179, 0.7998128361456462443 ) ) ;
#42694 = CARTESIAN_POINT ( 'NONE',  ( -5.686128154004278734, 7.329579007619248188, -1.223094714244008729 ) ) ;
#42695 = DIRECTION ( 'NONE',  ( -0.5996521035822321988, -0.8002608041566222630, 0.000000000000000000 ) ) ;
#42696 = CARTESIAN_POINT ( 'NONE',  ( 6.684453402082996654, -1.835023323784425564, -0.3624468955198830722 ) ) ;
#42697 = CARTESIAN_POINT ( 'NONE',  ( 6.419949431270806528, 7.448694743692793274, 1.199719254218462483 ) ) ;
#42698 =( NAMED_UNIT ( * ) PLANE_ANGLE_UNIT ( ) SI_UNIT ( $, .RADIAN. ) );
#42699 = CARTESIAN_POINT ( 'NONE',  ( 4.529832720741620022, 7.338536369956936589, -1.082531754730548412 ) ) ;
#42700 = DIRECTION ( 'NONE',  ( 0.000000000000000000, 0.000000000000000000, -1.000000000000000000 ) ) ;
#42701 = CARTESIAN_POINT ( 'NONE',  ( -1.402160292154681736E-14, 11.48437500034139980, 1.575800808251682339 ) ) ;
#42703 = CARTESIAN_POINT ( 'NONE',  ( -5.986807348886189040, 9.142303119412650503, -1.199719254218452047 ) ) ;
#42702 = CARTESIAN_POINT ( 'NONE',  ( 6.825078400183556937, 1.302289051367941708, 1.872899343898648983 ) ) ;
#42704 = CARTESIAN_POINT ( 'NONE',  ( 4.623498406067056088, 0.3027793956022621913, 1.707322668435699242 ) ) ;
#42705 = CARTESIAN_POINT ( 'NONE',  ( -3.730464822054482710, 7.503959392372201442, 1.040834085586084257E-14 ) ) ;
#42706 = CARTESIAN_POINT ( 'NONE',  ( 2.307561340129569150, -1.660171796135110567, -1.236610361758017973 ) ) ;
#42707 = CARTESIAN_POINT ( 'NONE',  ( 3.638375168990032549, 0.7640726493506818651, 1.974712724135726516 ) ) ;
#42708 = CARTESIAN_POINT ( 'NONE',  ( 6.591235234537977661, 10.84152487360300299, 0.7998128361456462443 ) ) ;
#42709 = DIRECTION ( 'NONE',  ( 0.000000000000000000, 0.000000000000000000, -1.000000000000000000 ) ) ;
#42710 = CARTESIAN_POINT ( 'NONE',  ( 1.867950311876313219, -1.955179860842346296, 0.2357939167430597172 ) ) ;
#42711 = CARTESIAN_POINT ( 'NONE',  ( 6.103366240126457676, 6.022929404904433071, 0.2034074856576886248 ) ) ;
#42713 = LINE ( 'NONE', #155362, #94453 ) ;
#42712 = CARTESIAN_POINT ( 'NONE',  ( -3.475000000000000533, -2.450000000000000622, 0.000000000000000000 ) ) ;
#42714 = CARTESIAN_POINT ( 'NONE',  ( 3.908379099077957886, 1.621946506101832775, -1.620046465671644675 ) ) ;
#42715 = CARTESIAN_POINT ( 'NONE',  ( 1.611646134362737959, -1.812087876328593916, 0.2219229778191167957 ) ) ;
#42716 = CARTESIAN_POINT ( 'NONE',  ( 5.559725510055676168, 8.644040974110419384, 1.199719254218451159 ) ) ;
#42717 = CARTESIAN_POINT ( 'NONE',  ( 5.897433631820129918, 8.863794422890064695, -1.082531754730537976 ) ) ;
#42718 = CARTESIAN_POINT ( 'NONE',  ( -8.694856585065634746, 9.038420858865048757, 0.7998128361456462443 ) ) ;
#42719 = CARTESIAN_POINT ( 'NONE',  ( 3.023692480417307316, -0.3885771752702297799, 1.975188976417296072 ) ) ;
#42720 = CARTESIAN_POINT ( 'NONE',  ( 2.184356868638567928, 1.133688150830698627, -1.600809071968431807 ) ) ;
#42721 = CARTESIAN_POINT ( 'NONE',  ( -7.374745490829552885, 10.69128794168811680, -1.199719254218446718 ) ) ;
#42722 = CARTESIAN_POINT ( 'NONE',  ( -7.237355071596549116, 7.338002426484427687, 1.040834085586084257E-14 ) ) ;
#42723 = CARTESIAN_POINT ( 'NONE',  ( 0.07536363704230969462, 1.333366039338843789, -2.397125032416930424 ) ) ;
#42725 = CARTESIAN_POINT ( 'NONE',  ( 3.150976108479891735, -1.446007784402236318, -1.020181273144848744 ) ) ;
#42724 = CARTESIAN_POINT ( 'NONE',  ( 4.927721519287828755, 1.075078395752477878, -1.792878403059654513 ) ) ;
#42726 = CARTESIAN_POINT ( 'NONE',  ( 0.6674790882334172837, 16.00000000000000711, 11.66566053519463786 ) ) ;
#42727 = CARTESIAN_POINT ( 'NONE',  ( 6.123008101752742682, -2.160436397662615970, 0.7664941572692751670 ) ) ;
#42728 = CARTESIAN_POINT ( 'NONE',  ( 6.122986541590657694, -1.636244173936936885, 0.5932577488661006093 ) ) ;
#42729 = CARTESIAN_POINT ( 'NONE',  ( 8.697719238366680372, 10.10609285197134533, 1.199719254218462483 ) ) ;
#42730 = CARTESIAN_POINT ( 'NONE',  ( 5.871801794802778751, -0.3338885390306855494, -2.274238935559732333 ) ) ;
#42731 = CARTESIAN_POINT ( 'NONE',  ( 2.971361445535975143, 6.558719713395274376, 0.4765173780192366593 ) ) ;
#42732 = CARTESIAN_POINT ( 'NONE',  ( 5.430864382934267987, 0.8560856307190685133, 1.507619432454242681 ) ) ;
#42733 = CARTESIAN_POINT ( 'NONE',  ( 6.368375356916068597, -1.978549699825098429, -0.3886382054163611821 ) ) ;
#42734 = AXIS2_PLACEMENT_3D ( 'NONE', #80554, #64307, #146652 ) ;
#42735 = CARTESIAN_POINT ( 'NONE',  ( 5.564936049989869460, 1.647787920686558438, -1.413916910601682897 ) ) ;
#42736 = CARTESIAN_POINT ( 'NONE',  ( 2.184835310096557404, 5.700724961754617404, 1.040834085586084257E-14 ) ) ;
#42737 = CARTESIAN_POINT ( 'NONE',  ( -0.06503379110851194300, -1.696408147887063178, 1.266814603907985504 ) ) ;
#42738 = CARTESIAN_POINT ( 'NONE',  ( 6.125000000000003553, -2.052068128417929849, 3.487440458529189440E-13 ) ) ;
#42739 = PRESENTATION_LAYER_ASSIGNMENT (  '', '', ( #170729 ) ) ;
#42740 = CARTESIAN_POINT ( 'NONE',  ( 11.07790593930098311, 9.799999999999998934, -0.7000000000000009548 ) ) ;
#42741 = CARTESIAN_POINT ( 'NONE',  ( 4.911117597291495329, 1.675855952751242883, 0.9498910403669177382 ) ) ;
#42742 = CARTESIAN_POINT ( 'NONE',  ( 1.499999999999997113, 11.67708333401613174, -0.8660254037844378194 ) ) ;
#42743 = CARTESIAN_POINT ( 'NONE',  ( -0.07508257667859614959, -0.9546805890920804227, -2.003339222774684458 ) ) ;
#42744 = VERTEX_POINT ( 'NONE', #77153 ) ;
#42745 = CARTESIAN_POINT ( 'NONE',  ( -1.001543065824772872E-14, 4.462500000000024336, 1.732050807568877637 ) ) ;
#42746 = CARTESIAN_POINT ( 'NONE',  ( 3.635557746758808495, 7.393234471193928847, -0.7998128361456291469 ) ) ;
#42747 = CARTESIAN_POINT ( 'NONE',  ( 6.120616281565444794, 9.228137197546649517, -1.199719254218440723 ) ) ;
#42748 = CARTESIAN_POINT ( 'NONE',  ( 2.192296887966191488, 1.369148959659401754, 1.749082743080948799 ) ) ;
#42750 = EDGE_CURVE ( 'NONE', #70481, #65102, #71971, .T. ) ;
#42749 = FACE_OUTER_BOUND ( 'NONE', #195568, .T. ) ;
#42751 = CARTESIAN_POINT ( 'NONE',  ( 6.643132081016124069, 7.813037518349371879, 1.082531754730558626 ) ) ;
#42752 = CARTESIAN_POINT ( 'NONE',  ( -9.964879715919934711, 10.72804054476916313, 0.7216878364870438212 ) ) ;
#42753 = VECTOR ( 'NONE', #210863, 1000.000000000000000 ) ;
#42754 = CARTESIAN_POINT ( 'NONE',  ( 7.024532985656136930, 8.328281583754568729, 1.082531754730549967 ) ) ;
#42755 = CARTESIAN_POINT ( 'NONE',  ( 0.2994542103806375200, 1.388483683912977495, -1.462447666687356485 ) ) ;
#42757 = CARTESIAN_POINT ( 'NONE',  ( 5.037578369333176376, 1.925844591945893747, -0.7392275334625797445 ) ) ;
#42756 = CARTESIAN_POINT ( 'NONE',  ( 7.540305987494599016, 11.94877408538573427, -0.7998128361456291469 ) ) ;
#42758 = CARTESIAN_POINT ( 'NONE',  ( -10.99970480911017745, -6.304485801116145538, -0.08058605610350685899 ) ) ;
#42759 = CARTESIAN_POINT ( 'NONE',  ( 5.980555156959511898, 9.991415093179179863, -0.7216878364870458196 ) ) ;
#42760 = DIRECTION ( 'NONE',  ( 0.000000000000000000, -1.000000000000000000, 0.000000000000000000 ) ) ;
#42761 = CARTESIAN_POINT ( 'NONE',  ( 1.364683531249986537, 1.405208333674755838, -0.7879004041258239610 ) ) ;
#42762 = CARTESIAN_POINT ( 'NONE',  ( 1.299667926800106121, -1.769921777095804671, -0.007132476793576813211 ) ) ;
#42763 = CARTESIAN_POINT ( 'NONE',  ( -0.06968618116158857567, -1.560424145883563929, -1.276814929289785239 ) ) ;
#42764 = CARTESIAN_POINT ( 'NONE',  ( 5.935049520445493165, -1.266825670006064275, -1.193719461430408968 ) ) ;
#42765 = CARTESIAN_POINT ( 'NONE',  ( 3.790815982946276641, 1.936215313137353178, -1.226956277148362862 ) ) ;
#42766 = CARTESIAN_POINT ( 'NONE',  ( -1.364683531250000748, -0.7406249996585803075, 0.000000000000000000 ) ) ;
#42767 = CARTESIAN_POINT ( 'NONE',  ( 1.939159035295745959, 0.7054217538491479589, -1.700835786604155242 ) ) ;
#42768 = CARTESIAN_POINT ( 'NONE',  ( 9.236128959407556849, 11.79856975744075598, -1.599625672291262513 ) ) ;
#42769 =( NAMED_UNIT ( * ) SI_UNIT ( $, .STERADIAN. ) SOLID_ANGLE_UNIT ( ) );
#42770 = CARTESIAN_POINT ( 'NONE',  ( 3.012524388372894713, 1.323457619556423381, -1.257707024427484388 ) ) ;
#42771 = CARTESIAN_POINT ( 'NONE',  ( 3.990861413484114273, -2.010826503599131065, 0.1511389102963680842 ) ) ;
#42772 = CARTESIAN_POINT ( 'NONE',  ( -10.17947440576205054, 10.77047498301088346, 0.7998128361456462443 ) ) ;
#42774 = CARTESIAN_POINT ( 'NONE',  ( -11.48806469435255373, 12.26910227127551245, -3.468902948106704631 ) ) ;
#42773 = CARTESIAN_POINT ( 'NONE',  ( 1.815646767810099149, -0.2761031220132881270, 2.245556248662975207 ) ) ;
#42775 = CARTESIAN_POINT ( 'NONE',  ( 5.227606396355295892, -2.000638224736817516, 0.6578950869102012655 ) ) ;
#42776 = CARTESIAN_POINT ( 'NONE',  ( 9.798003133828602884, 14.76688263464874851, 7.816136467581006997 ) ) ;
#42777 = CARTESIAN_POINT ( 'NONE',  ( 2.225130849662222410, -1.891980959128433781, -0.8411517639917851508 ) ) ;
#42778 = CARTESIAN_POINT ( 'NONE',  ( 3.520313441042647540, 7.258782781191745137, 0.7998128361456321445 ) ) ;
#42779 = CARTESIAN_POINT ( 'NONE',  ( -0.6801582343750438575, 0.1302083336747333897, -1.178068619123883165 ) ) ;
#42780 = CARTESIAN_POINT ( 'NONE',  ( 4.740951199079581180, 2.029406658027664623, 0.6148427566107574904 ) ) ;
#42781 = CARTESIAN_POINT ( 'NONE',  ( 1.172347479525590375, -1.222655876604409553, 1.488804252732379485 ) ) ;
#42782 = CARTESIAN_POINT ( 'NONE',  ( -5.829079699232685208, 5.765290835385048496, 0.000000000000000000 ) ) ;
#42783 = CARTESIAN_POINT ( 'NONE',  ( 7.248805684800777804, 11.60869039890961218, 1.040834085586084257E-14 ) ) ;
#42784 = CARTESIAN_POINT ( 'NONE',  ( 5.112833325684902341, 7.058334528089426740, -1.443375672974078761 ) ) ;
#42785 = CARTESIAN_POINT ( 'NONE',  ( 1.737500000000001155, -0.8895833323774166024, 3.009438278150922130 ) ) ;
#42786 = CARTESIAN_POINT ( 'NONE',  ( -4.880045225915050189, 7.780804299287790826, 1.199719254218464037 ) ) ;
#42787 = CARTESIAN_POINT ( 'NONE',  ( 5.801066647469003357, -0.3129311994157328303, -2.097281602037828208 ) ) ;
#42788 = CARTESIAN_POINT ( 'NONE',  ( 2.432770431885710405, 2.042423857386191255, 0.5128348284264750978 ) ) ;
#42789 = CARTESIAN_POINT ( 'NONE',  ( -3.657667580636712934, 7.489305620709952649, -0.7998128361456481317 ) ) ;
#42790 = CARTESIAN_POINT ( 'NONE',  ( 6.401421083946654100, 10.62007503124645957, -0.7998128361456291469 ) ) ;
#42791 = CARTESIAN_POINT ( 'NONE',  ( 6.315283160355378733, -1.595611397598785564, -0.9574585435550940771 ) ) ;
#42792 = CARTESIAN_POINT ( 'NONE',  ( 7.396136491454752715, 8.587579647240744407, 1.199719254218462483 ) ) ;
#42793 = CARTESIAN_POINT ( 'NONE',  ( 0.000000000000000000, 9.799999999999998934, 0.000000000000000000 ) ) ;
#42794 = CARTESIAN_POINT ( 'NONE',  ( -3.311934663488232733, 7.085950550703385531, -0.7998128361456481317 ) ) ;
#42796 = EDGE_LOOP ( 'NONE', ( #12763, #164484 ) ) ;
#42795 = CARTESIAN_POINT ( 'NONE',  ( -9.327646496521992958, 9.984601788804893019, -0.7216878364870267237 ) ) ;
#42797 = CARTESIAN_POINT ( 'NONE',  ( -0.2104748580754166598, -0.006608320950483163522, -2.103482951484026753 ) ) ;
#42798 = DIRECTION ( 'NONE',  ( 0.6483454320283799088, 0.000000000000000000, -0.7613463080411786432 ) ) ;
#42800 = CARTESIAN_POINT ( 'NONE',  ( 3.877359892829432386, -0.1466975079335990917, 1.956454564409334296 ) ) ;
#42799 = CARTESIAN_POINT ( 'NONE',  ( 1.224999999999984768, -0.1250000000000139888, -4.857225732735059864E-14 ) ) ;
#42801 = CARTESIAN_POINT ( 'NONE',  ( 0.5323697292517782786, 1.110078392871534314, -1.854780036684190669 ) ) ;
#42803 = CARTESIAN_POINT ( 'NONE',  ( -5.355516094498059765, 6.520963868127283014, 1.360184235745926618 ) ) ;
#42802 = CARTESIAN_POINT ( 'NONE',  ( -3.935609729716867289, 7.813571461303467913, 0.7998128361456352531 ) ) ;
#42805 = ADVANCED_FACE ( 'NONE', ( #97701 ), #114009, .T. ) ;
#42804 = CARTESIAN_POINT ( 'NONE',  ( -0.6823417656250003738, 2.217708333674753174, -1.181850606188749264 ) ) ;
#42806 = CARTESIAN_POINT ( 'NONE',  ( 2.677380959318215847, -0.8946470780417746793, 1.492600998661142375 ) ) ;
#42807 = CARTESIAN_POINT ( 'NONE',  ( 5.151735183512854199, 8.954182114166247430, -0.7216878364870257245 ) ) ;
#42808 = CARTESIAN_POINT ( 'NONE',  ( -11.24554337403377069, 7.016168494911984688, 5.610835997672845465 ) ) ;
#42809 = AXIS2_PLACEMENT_3D ( 'NONE', #186403, #119349, #169094 ) ;
#42810 = CARTESIAN_POINT ( 'NONE',  ( 2.073592080879012478, 1.495823877299466087, -1.351946161731142126 ) ) ;
#42811 = CARTESIAN_POINT ( 'NONE',  ( -10.98535488200955079, 12.34177443252770168, -1.593017372382190766 ) ) ;
#42813 = AXIS2_PLACEMENT_3D ( 'NONE', #131454, #2428, #103167 ) ;
#42812 = CARTESIAN_POINT ( 'NONE',  ( -5.472651281771599763, 6.413789912602166687, 1.199719254218452935 ) ) ;
#42814 = CARTESIAN_POINT ( 'NONE',  ( 2.201972163173575137, -1.971069923813788982, 0.04663598398449429056 ) ) ;
#42815 = EDGE_CURVE ( 'NONE', #185401, #195170, #163761, .T. ) ;
#42816 = VECTOR ( 'NONE', #133631, 1000.000000000000000 ) ;
#42818 = CARTESIAN_POINT ( 'NONE',  ( -5.817857314039913241, 5.960124085900898372, 0.000000000000000000 ) ) ;
#42817 = CARTESIAN_POINT ( 'NONE',  ( 5.836178160628028522, -1.067892152678026951, -1.586260290404594597 ) ) ;
#42819 = CARTESIAN_POINT ( 'NONE',  ( -4.787437638956927977, 7.639075441208117212, -1.082531754730549967 ) ) ;
#42820 = CARTESIAN_POINT ( 'NONE',  ( 5.027041095616958444, 9.086908054853605421, 0.000000000000000000 ) ) ;
#42821 = CARTESIAN_POINT ( 'NONE',  ( -5.926849427829407269, 6.943687749669614995, -1.199719254218453823 ) ) ;
#42822 = CARTESIAN_POINT ( 'NONE',  ( 0.9967468350138152244, -1.970926226424707606, -0.4403189329902043037 ) ) ;
#42823 = CARTESIAN_POINT ( 'NONE',  ( 4.704316113817540668, 5.551085556617666228, -1.082531754730548412 ) ) ;
#42824 = CARTESIAN_POINT ( 'NONE',  ( 5.702268328713489431, -2.307758713666784534, -0.007378162171353326235 ) ) ;
#42825 = CARTESIAN_POINT ( 'NONE',  ( 6.496542546517183325, 1.940334402339534581, 0.2891159199209930031 ) ) ;
#42826 = CARTESIAN_POINT ( 'NONE',  ( 2.799599750139214471, -1.450362073461785473, -1.321114446766240347 ) ) ;
#42827 = CARTESIAN_POINT ( 'NONE',  ( 7.560643217915098191, 11.97250085420964716, -0.7998128361456291469 ) ) ;
#42828 = CARTESIAN_POINT ( 'NONE',  ( 0.2115648487451895210, 1.930418618556551946, 0.5826528611774862698 ) ) ;
#42829 = EDGE_LOOP ( 'NONE', ( #178922, #66633, #198179 ) ) ;
#42830 = CARTESIAN_POINT ( 'NONE',  ( 0.7962977453638077074, -0.9578387366565711547, -1.888411434433327374 ) ) ;
#42832 = CARTESIAN_POINT ( 'NONE',  ( -7.369020184227459858, 8.555943955475521889, 1.199719254218450271 ) ) ;
#42831 = CARTESIAN_POINT ( 'NONE',  ( -3.948449050077848632, 5.629609863222681199, 1.599625672291267398 ) ) ;
#42833 = CARTESIAN_POINT ( 'NONE',  ( 2.519273208346615611, -1.059988974693906405, -1.505194322970206944 ) ) ;
#42834 = ORIENTED_EDGE ( 'NONE', *, *, #85714, .F. ) ;
#42835 = CARTESIAN_POINT ( 'NONE',  ( 9.576657467935302037, 12.68194475294117574, 7.234045051690152661 ) ) ;
#42836 = CARTESIAN_POINT ( 'NONE',  ( 2.514065211524143084, -0.6609878990531635745, 2.015050547854141172 ) ) ;
#42837 = CARTESIAN_POINT ( 'NONE',  ( -1.201851678989727383E-14, 3.993750000682817713, 1.732050807568877637 ) ) ;
#42838 = CARTESIAN_POINT ( 'NONE',  ( 6.753933077901968396, 11.03133902419432566, 0.7998128361456462443 ) ) ;
#42839 = CARTESIAN_POINT ( 'NONE',  ( 7.095713291905693332, 9.371694488680407886, 1.599625672291268286 ) ) ;
#42840 = CARTESIAN_POINT ( 'NONE',  ( 4.147771190963340793, 0.6980094919085011451, -1.939086781881957933 ) ) ;
#42842 = CARTESIAN_POINT ( 'NONE',  ( 0.8547319020580852467, 0.3593373433725781108, -1.805665335529122784 ) ) ;
#42841 = CARTESIAN_POINT ( 'NONE',  ( -7.446452682403657874, 9.710614100936176385, -1.599625672291263179 ) ) ;
#42843 = CARTESIAN_POINT ( 'NONE',  ( -1.201851678989727383E-14, 5.196875000341422357, -1.575800808251660134 ) ) ;
#42844 = SURFACE_SIDE_STYLE ('',( #103553 ) ) ;
#42845 = CARTESIAN_POINT ( 'NONE',  ( -1.445368642221011024, 8.714907460504111469, 2.589984629573252928 ) ) ;
#42846 = CARTESIAN_POINT ( 'NONE',  ( -11.88237951145550575, 13.75680652621284317, 0.9087114598430686696 ) ) ;
#42847 = CARTESIAN_POINT ( 'NONE',  ( 1.524350002934187653, -1.228176919886795782, -1.833354347511229498 ) ) ;
#42848 = CARTESIAN_POINT ( 'NONE',  ( 2.390224264847177871, -0.9692217175977213550, 2.044435098530998474 ) ) ;
#42849 = CARTESIAN_POINT ( 'NONE',  ( -9.341204650135658483, 10.00041963468749984, 1.040834085586084257E-14 ) ) ;
#42850 = CARTESIAN_POINT ( 'NONE',  ( 2.583996913715621790, 0.9723193252555061283, 1.528341728153536305 ) ) ;
#42851 = CARTESIAN_POINT ( 'NONE',  ( 2.641684811942858424, 1.906066497734011378, -0.1923337340370822046 ) ) ;
#42852 = CARTESIAN_POINT ( 'NONE',  ( 3.930184216435282707, 1.147649575447948100, 1.722966636330313550 ) ) ;
#42853 = CARTESIAN_POINT ( 'NONE',  ( -1.364683531250012516, 2.551041667008089320, -0.7879004041258289570 ) ) ;
#42854 = CARTESIAN_POINT ( 'NONE',  ( 3.256668630020958410, -1.493913901992610205, 1.286540209188108630 ) ) ;
#42855 = CARTESIAN_POINT ( 'NONE',  ( 6.639296574806412110, -1.719437650081551139, 0.8690664522189944785 ) ) ;
#42856 = CARTESIAN_POINT ( 'NONE',  ( 4.487079325084206260, 1.670935625628103605, -0.8411387520786617333 ) ) ;
#42858 = CARTESIAN_POINT ( 'NONE',  ( 5.010605496441194795, 7.906410611435644498, -1.080668833775387139 ) ) ;
#42857 = CARTESIAN_POINT ( 'NONE',  ( 2.508792734928457335, -0.8846401781386037388, -2.131589412884911106 ) ) ;
#42859 = CARTESIAN_POINT ( 'NONE',  ( 3.385049140913086507, 0.04320281034062402326, 1.860716667189839635 ) ) ;
#42860 = CARTESIAN_POINT ( 'NONE',  ( -0.6823417656249969321, 3.967708333674754950, -1.181850606188749264 ) ) ;
#42861 = CARTESIAN_POINT ( 'NONE',  ( -3.761497552787613330, 6.475832013972435242, 1.199719254218464037 ) ) ;
#42862 = CARTESIAN_POINT ( 'NONE',  ( 5.276094334012385367, 9.307193822989793475, 1.040834085586084257E-14 ) ) ;
#42863 = CARTESIAN_POINT ( 'NONE',  ( 11.16489891154632907, 3.742896273583259159, -3.684481756086981363 ) ) ;
#42864 =( BOUNDED_CURVE ( )  B_SPLINE_CURVE ( 2, ( #21240, #155554, #87346, #22308, #172880, #73206, #153413, #138244, #54847 ),
 .UNSPECIFIED., .F., .T. ) 
 B_SPLINE_CURVE_WITH_KNOTS ( ( 3, 2, 2, 2, 3 ),
 ( 0.01562500000000010061, 0.02083333333333333218, 0.03125000000000000000, 0.04166666666666666435, 0.04687499999999993755 ),
 .UNSPECIFIED. ) 
 CURVE ( )  GEOMETRIC_REPRESENTATION_ITEM ( )  RATIONAL_B_SPLINE_CURVE ( ( 0.9330127018922194093, 0.9330127018922207416, 1.000000000000000000, 0.8660254037844387076, 1.000000000000000000, 0.8660254037844387076, 1.000000000000000000, 0.9330127018922200755, 0.9330127018922192983 ) ) 
 REPRESENTATION_ITEM ( '' )  );
#42865 = CARTESIAN_POINT ( 'NONE',  ( 0.8035136555551088966, 1.722860008830621847, 1.211028463478396988 ) ) ;
#42866 = CARTESIAN_POINT ( 'NONE',  ( -1.001543065824772872E-14, 4.384375000341417916, 1.575800808251672791 ) ) ;
#42867 = CARTESIAN_POINT ( 'NONE',  ( 6.397764797294555272, -0.7349420381566433846, 2.032942830986879557 ) ) ;
#42868 = CARTESIAN_POINT ( 'NONE',  ( 2.549219474610735947, 0.2639673528169217964, 2.104066465523121376 ) ) ;
#42869 = CARTESIAN_POINT ( 'NONE',  ( 0.07057728186875102117, 0.7769860399358395897, 1.864564603342239835 ) ) ;
#42870 = CARTESIAN_POINT ( 'NONE',  ( 1.364683531249988757, -0.1156249996585798079, 0.000000000000000000 ) ) ;
#42871 = CARTESIAN_POINT ( 'NONE',  ( -3.470524135418300737, 6.032400010421219427, -1.082531754730549967 ) ) ;
#42872 = CARTESIAN_POINT ( 'NONE',  ( 0.7905619602705875604, -2.145198653374354336, -0.2653712149464776959 ) ) ;
#42875 = CARTESIAN_POINT ( 'NONE',  ( 2.575685996916329046, 5.948791396470269888, 0.7216878364870438212 ) ) ;
#42874 = CARTESIAN_POINT ( 'NONE',  ( 3.285556943750000514, -0.3135416661887098777, 1.896917185911906500 ) ) ;
#42873 = CARTESIAN_POINT ( 'NONE',  ( 7.361151057576892143, 7.552707420120024828, 0.7998128361456291469 ) ) ;
#42876 = CARTESIAN_POINT ( 'NONE',  ( -4.329849954717889915, 6.144853928627882489, 1.599625672291270506 ) ) ;
#42877 = CARTESIAN_POINT ( 'NONE',  ( 5.190638768449240992, 1.523797776992100284, -1.320824044268428255 ) ) ;
#42879 = CARTESIAN_POINT ( 'NONE',  ( -6.577113915960828727, 9.727031097712693253, -1.082531754730549967 ) ) ;
#42878 = CARTESIAN_POINT ( 'NONE',  ( -9.653042183249970876, 11.32459930428888306, -1.082531754730539753 ) ) ;
#42881 = CARTESIAN_POINT ( 'NONE',  ( 1.364683531249997417, 10.23437500034139802, 2.602085213965210642E-15 ) ) ;
#42880 = CARTESIAN_POINT ( 'NONE',  ( 5.787991602622606813, -0.9759734195362681497, 1.928925553883020338 ) ) ;
#42882 = CARTESIAN_POINT ( 'NONE',  ( -9.110189153378817295, 12.71597221466224603, 1.199719254218462483 ) ) ;
#42883 = EDGE_CURVE ( 'NONE', #99015, #112384, #10047, .T. ) ;
#42885 = CARTESIAN_POINT ( 'NONE',  ( 0.1576404624921414199, 1.103540182269863612, 1.565583644703759436 ) ) ;
#42884 = CARTESIAN_POINT ( 'NONE',  ( -5.463572716182839351, 7.397254140345190798, 1.443375672974064550 ) ) ;
#42886 = CARTESIAN_POINT ( 'NONE',  ( 1.364683531249986537, 1.217708333674754950, -0.7879004041258239610 ) ) ;
#42887 = CARTESIAN_POINT ( 'NONE',  ( 0.08053691275167890185, 14.48195938056239385, 11.99972973886013961 ) ) ;
#42888 = FACE_OUTER_BOUND ( 'NONE', #80257, .T. ) ;
#42889 = CARTESIAN_POINT ( 'NONE',  ( 3.105755298912396878, -1.722902020775359144, 0.08520973767557615819 ) ) ;
#42890 = CARTESIAN_POINT ( 'NONE',  ( 5.833751235630055376, 10.02806988486892514, 0.7998128361456331437 ) ) ;
#42891 = CARTESIAN_POINT ( 'NONE',  ( 6.554440917563797875, 6.611545590104705994, -0.7998128361456481317 ) ) ;
#42892 = CARTESIAN_POINT ( 'NONE',  ( 1.364683531249988757, -0.3031249996585799744, 0.000000000000000000 ) ) ;
#42893 = CARTESIAN_POINT ( 'NONE',  ( 1.246904684444858136, -1.390570190391905658, -1.094529049636628226 ) ) ;
#42894 = CARTESIAN_POINT ( 'NONE',  ( 2.068995670861985658, -1.554830924100785161, 1.278664071131753843 ) ) ;
#42895 = CARTESIAN_POINT ( 'NONE',  ( 0.4373225248172890045, -5.223431457505089526, 10.96785329849812385 ) ) ;
#42896 = CARTESIAN_POINT ( 'NONE',  ( 4.348781676370103710, 0.5853419563807431558, 2.127667884090424621 ) ) ;
#42897 = ORIENTED_EDGE ( 'NONE', *, *, #161474, .T. ) ;
#42898 = CARTESIAN_POINT ( 'NONE',  ( 4.934241560730721510, 4.721313007132757811, 0.000000000000000000 ) ) ;
#42899 = CARTESIAN_POINT ( 'NONE',  ( 6.927853306458731986, 11.02631992426980112, 0.7216878364870438212 ) ) ;
#42901 = CARTESIAN_POINT ( 'NONE',  ( 2.741814726283864800, 2.006445297011373974, -0.2004551355171620974 ) ) ;
#42900 = CARTESIAN_POINT ( 'NONE',  ( 3.387459763963754700, 0.05019612904376415108, -2.120051327867578550 ) ) ;
#42903 = EDGE_LOOP ( 'NONE', ( #123987, #881 ) ) ;
#42902 = CARTESIAN_POINT ( 'NONE',  ( 3.849720854566369255, -1.253557171431567863, -1.308061721885760198 ) ) ;
#42904 = CARTESIAN_POINT ( 'NONE',  ( 5.061990249855835344, 6.999017606288844284, -1.599625672291273171 ) ) ;
#42905 = ORIENTED_EDGE ( 'NONE', *, *, #209983, .F. ) ;
#42906 = CARTESIAN_POINT ( 'NONE',  ( 0.1626889888870358680, -1.668787113083155305, -0.8454427722031019332 ) ) ;
#42907 = ADVANCED_FACE ( 'NONE', ( #29487 ), #13222, .T. ) ;
#42908 = CARTESIAN_POINT ( 'NONE',  ( 5.795480788678070816, 1.385457615097264394, 1.189071861804301466 ) ) ;
#42910 = CARTESIAN_POINT ( 'NONE',  ( 2.553800400642152635, 1.028702656226655465, 1.615903109786074099 ) ) ;
#42909 = CARTESIAN_POINT ( 'NONE',  ( -3.090368948911150770, 5.692848642783215674, 1.199719254218462483 ) ) ;
#42911 = SURFACE_SIDE_STYLE ('',( #191247 ) ) ;
#42912 = DIRECTION ( 'NONE',  ( 0.000000000000000000, 0.000000000000000000, -1.000000000000000000 ) ) ;
#42913 = CARTESIAN_POINT ( 'NONE',  ( 0.6823417656249882723, 1.738541667008083991, -1.181850606188749264 ) ) ;
#42914 = CARTESIAN_POINT ( 'NONE',  ( -5.777182852754558340, 5.912670547734647286, 0.000000000000000000 ) ) ;
#42915 = CARTESIAN_POINT ( 'NONE',  ( 6.292392690518195941, 8.434487120394948079, -1.443375672974078761 ) ) ;
#42916 = CARTESIAN_POINT ( 'NONE',  ( -5.397554552016258889, 7.390509292142662723, 1.443375672974058777 ) ) ;
#42917 = CARTESIAN_POINT ( 'NONE',  ( -7.208094944320834863, 8.438474185576302133, -1.199719254218452047 ) ) ;
#42918 = CARTESIAN_POINT ( 'NONE',  ( 2.830460552442021438, -1.048868820301660953, -1.842999677239331113 ) ) ;
#42920 = CARTESIAN_POINT ( 'NONE',  ( -11.24554337403377069, 7.016168494911984688, 5.610835997672845465 ) ) ;
#42919 = CARTESIAN_POINT ( 'NONE',  ( -0.1294898018151836583, 0.7212281881416956475, -2.008332099035778917 ) ) ;
#42921 = CARTESIAN_POINT ( 'NONE',  ( 4.218015588379292247, -1.010805368333337562, -1.692340417948991371 ) ) ;
#42922 = CARTESIAN_POINT ( 'NONE',  ( 0.2111898618733127897, 1.671471951565723035, -1.121848769376234234 ) ) ;
#42923 = ORIENTED_EDGE ( 'NONE', *, *, #37862, .T. ) ;
#42924 = CARTESIAN_POINT ( 'NONE',  ( 6.210183267806027807, 1.217293573752244784, -1.732272713164469735 ) ) ;
#42925 = CARTESIAN_POINT ( 'NONE',  ( 8.628381312412237492, 13.71601666663510066, 8.341747646421527662 ) ) ;
#42926 = CARTESIAN_POINT ( 'NONE',  ( 1.346235217667652417, -0.9325981557438846048, 1.848514419461377845 ) ) ;
#42927 = CARTESIAN_POINT ( 'NONE',  ( 3.204954726155031963, -0.3781314774268499379, 1.904617838069742275 ) ) ;
#42928 = ORIENTED_EDGE ( 'NONE', *, *, #202990, .T. ) ;
#42929 = CARTESIAN_POINT ( 'NONE',  ( 5.234329823327693809, 8.264412672927770487, 1.199719254218451159 ) ) ;
#42930 = CARTESIAN_POINT ( 'NONE',  ( 6.658989722967328717, 7.797851427330578566, 1.199719254218452935 ) ) ;
#42932 = CARTESIAN_POINT ( 'NONE',  ( 4.496500501226593727, 8.397667684739696270, 0.7998128361456462443 ) ) ;
#42931 = CARTESIAN_POINT ( 'NONE',  ( 3.767594164193796669, 1.161519562870310329, 1.738068047407430816 ) ) ;
#42934 = AXIS2_PLACEMENT_3D ( 'NONE', #158213, #140921, #43398 ) ;
#42933 = CARTESIAN_POINT ( 'NONE',  ( 3.228249973385329596, 6.780392379009261283, -1.734723475976807094E-15 ) ) ;
#42936 = ORIENTED_EDGE ( 'NONE', *, *, #72745, .T. ) ;
#42935 = CARTESIAN_POINT ( 'NONE',  ( 0.6447925058646056806, 0.1317677938489550116, 1.806752140514777283 ) ) ;
#42937 = CARTESIAN_POINT ( 'NONE',  ( 5.303435803989668074, 1.802500012205746183, 1.273053691228965389 ) ) ;
#42938 = CARTESIAN_POINT ( 'NONE',  ( -0.1969747848977146110, -6.717152734873772069, -10.87166355890665415 ) ) ;
#42939 = CARTESIAN_POINT ( 'NONE',  ( 2.749284697512776710, -1.835294401387000285, 1.225074929180599570 ) ) ;
#42940 = CARTESIAN_POINT ( 'NONE',  ( 8.097244055859613709, 10.46987070330147063, -1.599625672291262513 ) ) ;
#42941 = FACE_OUTER_BOUND ( 'NONE', #53527, .T. ) ;
#42942 = CARTESIAN_POINT ( 'NONE',  ( 2.508343198132975349, -1.907285675847451234, -0.1387974571645037292 ) ) ;
#42943 =( BOUNDED_CURVE ( )  B_SPLINE_CURVE ( 3, ( #140890, #206901, #93194, #174442 ),
 .UNSPECIFIED., .F., .T. ) 
 B_SPLINE_CURVE_WITH_KNOTS ( ( 4, 4 ),
 ( 1.570796326794846154, 2.479086375273363618 ),
 .UNSPECIFIED. ) 
 CURVE ( )  GEOMETRIC_REPRESENTATION_ITEM ( )  RATIONAL_B_SPLINE_CURVE ( ( 1.000000000000000000, 0.9324242863012337512, 0.9324242863012337512, 1.000000000000000000 ) ) 
 REPRESENTATION_ITEM ( '' )  );
#42944 = CARTESIAN_POINT ( 'NONE',  ( 8.062294901620731480, 12.55776115186623620, 1.040834085586084257E-14 ) ) ;
#42945 = CARTESIAN_POINT ( 'NONE',  ( 5.758279222819879806, -2.070544812512797428, -0.003756845764937844813 ) ) ;
#42947 = CARTESIAN_POINT ( 'NONE',  ( 3.116266767097406909, -1.064116542966097922, -1.881565754655416756 ) ) ;
#42946 = CARTESIAN_POINT ( 'NONE',  ( -3.020739592526671125, 6.452503409769998477, 0.6179323767311885041 ) ) ;
#42948 = CARTESIAN_POINT ( 'NONE',  ( 5.302338810847701644, 1.659911028786088538, -1.431018553749352051 ) ) ;
#42949 = ORIENTED_EDGE ( 'NONE', *, *, #15710, .F. ) ;
#42950 = VERTEX_POINT ( 'NONE', #14269 ) ;
#42951 = LINE ( 'NONE', #30960, #190334 ) ;
#42952 = CARTESIAN_POINT ( 'NONE',  ( -9.516228778038660963, -8.176227079964615285, 0.3870642018030935882 ) ) ;
#42953 = CARTESIAN_POINT ( 'NONE',  ( 3.147653791585713901, 8.920000000000001705, -2.500000000000002220 ) ) ;
#42954 = CARTESIAN_POINT ( 'NONE',  ( 3.888156192069020634, 7.758209000714329839, 1.040834085586084257E-14 ) ) ;
#42955 = CARTESIAN_POINT ( 'NONE',  ( -3.285556943749998737, -2.267708332855375986, 1.896917185911908721 ) ) ;
#42956 = CARTESIAN_POINT ( 'NONE',  ( -4.004454267989906668, 5.765225627445230927, 1.599625672291270506 ) ) ;
#42957 = TOROIDAL_SURFACE ( 'NONE', #63644, 8.300000000000000711, 0.2000000000000000111 ) ;
#42958 = CARTESIAN_POINT ( 'NONE',  ( -8.893785580884703279, 10.43879993486270585, 1.082531754730558626 ) ) ;
#42959 = CARTESIAN_POINT ( 'NONE',  ( 6.547661840756936691, 6.603636667163397256, 0.7998128361456352531 ) ) ;
#42960 = CARTESIAN_POINT ( 'NONE',  ( 5.858279169847476098, -2.070434559870216074, -0.005763162253501209233 ) ) ;
#42961 = CARTESIAN_POINT ( 'NONE',  ( 4.459546661884671970, 0.4205705884572363829, -1.879884317620848178 ) ) ;
#42962 = CARTESIAN_POINT ( 'NONE',  ( 0.2632962822839111650, 1.880428227362867633, -0.7283992291491693249 ) ) ;
#42963 =( GEOMETRIC_REPRESENTATION_CONTEXT ( 3 ) GLOBAL_UNCERTAINTY_ASSIGNED_CONTEXT ( ( #165334 ) ) GLOBAL_UNIT_ASSIGNED_CONTEXT ( ( #158740, #142518, #192278 ) ) REPRESENTATION_CONTEXT ( 'NONE', 'WORKASPACE' ) );
#42964 = CARTESIAN_POINT ( 'NONE',  ( -15.75000000000000000, 12.69999999999998153, 3.199999999999997957 ) ) ;
#42965 = CARTESIAN_POINT ( 'NONE',  ( 6.912678218121202534, 9.158153569265168770, 1.599625672291268286 ) ) ;
#42966 = CARTESIAN_POINT ( 'NONE',  ( -5.132810702184136709, 6.527128546466574477, -1.246928735940135313 ) ) ;
#42967 = CARTESIAN_POINT ( 'NONE',  ( 5.489095164188675824, 0.1408790922432824055, 1.964433151921646470 ) ) ;
#42968 = CARTESIAN_POINT ( 'NONE',  ( 0.1116237293282626442, -2.148295633857814746, 0.4319020730012904097 ) ) ;
#42969 = CARTESIAN_POINT ( 'NONE',  ( 4.951681858558426796, 0.5695450498939165218, -1.734646904759745700 ) ) ;
#42970 = CARTESIAN_POINT ( 'NONE',  ( 5.370438244788902971, 9.279612028980123384, -0.7216878364870458196 ) ) ;
#42971 = CARTESIAN_POINT ( 'NONE',  ( 4.324687812634892659, 5.108185871904570519, 1.082531754730560403 ) ) ;
#42972 = CARTESIAN_POINT ( 'NONE',  ( -6.805266759416629618, 6.904175738932996964, 0.000000000000000000 ) ) ;
#42973 = CARTESIAN_POINT ( 'NONE',  ( 5.499767588998890844, 6.445425604367387429, 1.199719254218451159 ) ) ;
#42974 = ORIENTED_EDGE ( 'NONE', *, *, #147140, .T. ) ;
#42976 = CARTESIAN_POINT ( 'NONE',  ( 5.976820168803962829, -1.420628428873932814, 1.426715538211227763 ) ) ;
#42975 = CARTESIAN_POINT ( 'NONE',  ( 2.173174093899932657, 1.133995793187540180, 1.450494936146892622 ) ) ;
#42977 = CARTESIAN_POINT ( 'NONE',  ( 1.335823321505170025, -1.456863090139989714, 1.777644367010343451 ) ) ;
#42978 = CARTESIAN_POINT ( 'NONE',  ( 6.069191303861535935, 1.728486752094375190, 0.9278679456784575397 ) ) ;
#42979 = CARTESIAN_POINT ( 'NONE',  ( -6.240830780992103755, 6.175390754112560110, 1.040834085586084257E-14 ) ) ;
#42980 = CARTESIAN_POINT ( 'NONE',  ( -4.003117076043361422, 7.684394865269255526, -0.1089946556460293509 ) ) ;
#42981 = CARTESIAN_POINT ( 'NONE',  ( -2.676845263694313637, 5.210404343363602919, -1.199719254218446718 ) ) ;
#42982 = CARTESIAN_POINT ( 'NONE',  ( 0.8540665308606997241, -0.7467690478978536994, 1.931163149162813619 ) ) ;
#42983 = CARTESIAN_POINT ( 'NONE',  ( -4.111865726694519552, 8.019203457777400956, 0.000000000000000000 ) ) ;
#42985 = CARTESIAN_POINT ( 'NONE',  ( 1.129532124359374334, -1.183843481993757774, -1.448407549327054955 ) ) ;
#42984 = CARTESIAN_POINT ( 'NONE',  ( 1.171554334673271303, 1.248344470866637135, 1.676987088486236566 ) ) ;
#42986 = CARTESIAN_POINT ( 'NONE',  ( 1.440779594245532369, 1.198675164295496920, 1.620935466883965503 ) ) ;
#42987 = CARTESIAN_POINT ( 'NONE',  ( -1.201851678989727383E-14, 3.634375000341422357, 1.575800808251672791 ) ) ;
#42988 = CARTESIAN_POINT ( 'NONE',  ( 2.137881509367345778, 0.3822841233627124469, 1.697745509426834332 ) ) ;
#42989 = CARTESIAN_POINT ( 'NONE',  ( 5.823390672269506574, 6.752709524857930745, -1.199719254218446718 ) ) ;
#42990 = CARTESIAN_POINT ( 'NONE',  ( 1.504932104232256984, 8.664796307965634270, 2.552344783041808451 ) ) ;
#42991 = CARTESIAN_POINT ( 'NONE',  ( 2.965164839364425653, 0.2526306750327989015, -1.706137528056344888 ) ) ;
#42992 = CARTESIAN_POINT ( 'NONE',  ( 2.876726420669137863, -0.1638259704515396820, -2.185508879517850112 ) ) ;
#42993 = CARTESIAN_POINT ( 'NONE',  ( 4.670673364294657404, -1.443042178620690841, 1.669811033208345341 ) ) ;
#42994 = CARTESIAN_POINT ( 'NONE',  ( -10.81015953665327345, 5.524082113754967160, -6.547048903644186346 ) ) ;
#42995 = CARTESIAN_POINT ( 'NONE',  ( 2.430757386254971841, -1.338474561058100143, 1.709278666203792652 ) ) ;
#42996 = CARTESIAN_POINT ( 'NONE',  ( 0.8557438351849018243, 1.823752217391808372, -0.08689656109241167270 ) ) ;
#42997 = CARTESIAN_POINT ( 'NONE',  ( 3.802059961758995854, -1.092030603714509551, -1.813900157284773496 ) ) ;
#42998 = CYLINDRICAL_SURFACE ( 'NONE', #170510, 0.7500000000000011102 ) ;
#42999 = EDGE_CURVE ( 'NONE', #100951, #212186, #86273, .T. ) ;
#43000 = ORIENTED_EDGE ( 'NONE', *, *, #37661, .T. ) ;
#43002 = CARTESIAN_POINT ( 'NONE',  ( 1.364683531249988535, 1.926041667008086211, 0.7879004041258500513 ) ) ;
#43001 = CARTESIAN_POINT ( 'NONE',  ( 3.474455725741688372, -2.209678783342132746, -0.6099929035564675139 ) ) ;
#43003 = CARTESIAN_POINT ( 'NONE',  ( 11.35610322553117513, 11.11421628929173089, 3.553412924323500643 ) ) ;
#43004 = CARTESIAN_POINT ( 'NONE',  ( 2.693266070609028784, 6.293894182352508970, 0.000000000000000000 ) ) ;
#43005 = CARTESIAN_POINT ( 'NONE',  ( 6.393255305546848177, -0.1058262492604696708, -2.218914918540932035 ) ) ;
#43006 = CARTESIAN_POINT ( 'NONE',  ( -6.426201623197489887, 6.599582769926260362, 0.7216878364870317197 ) ) ;
#43007 = EDGE_CURVE ( 'NONE', #72859, #180190, #125608, .T. ) ;
#43008 = CARTESIAN_POINT ( 'NONE',  ( 4.419594888374914099, 5.218910793601261311, -1.082531754730548412 ) ) ;
#43009 = CARTESIAN_POINT ( 'NONE',  ( -5.870317324592811303, 8.832158731124840401, -1.082531754730537976 ) ) ;
#43010 = CARTESIAN_POINT ( 'NONE',  ( -11.04536101718726293, 10.19999999999999929, 1.099999999999996758 ) ) ;
#43011 = AXIS2_PLACEMENT_3D ( 'NONE', #139792, #120392, #203670 ) ;
#43012 = ORIENTED_EDGE ( 'NONE', *, *, #190135, .T. ) ;
#43013 = CARTESIAN_POINT ( 'NONE',  ( 3.938125092175647879, -1.678004675797317713, -1.117833462672225497 ) ) ;
#43015 = CARTESIAN_POINT ( 'NONE',  ( 3.819230306994053858, -1.816680642618787145, -0.9767294869839551197 ) ) ;
#43014 = CARTESIAN_POINT ( 'NONE',  ( 5.449487677688982679, 8.445153826357429949, -1.199719254218446718 ) ) ;
#43016 = CARTESIAN_POINT ( 'NONE',  ( 0.000000000000000000, 5.499999999999998224, 0.000000000000000000 ) ) ;
#43017 = CARTESIAN_POINT ( 'NONE',  ( 7.472478939787284169, 8.746922180287201698, 1.199719254218452935 ) ) ;
#43018 = CARTESIAN_POINT ( 'NONE',  ( 3.285556943750000514, -2.763541666188707335, 1.896917185911906500 ) ) ;
#43019 = CARTESIAN_POINT ( 'NONE',  ( -0.6823417656249969321, 4.967708333674755394, -1.181850606188749264 ) ) ;
#43020 = CARTESIAN_POINT ( 'NONE',  ( 5.859372887940716090, 2.159598860408561194, -0.3713886045505072064 ) ) ;
#43021 = CARTESIAN_POINT ( 'NONE',  ( 3.059220373557011818, -1.198860207862334049, 1.621182619130703051 ) ) ;
#43022 = CARTESIAN_POINT ( 'NONE',  ( 1.628196140939692338, 0.1813696128579282696, 1.832309401408799276 ) ) ;
#43023 = ADVANCED_FACE ( 'NONE', ( #49994 ), #148569, .T. ) ;
#43024 = CARTESIAN_POINT ( 'NONE',  ( 7.793239369756836510, 7.986534107671458216, 0.7998128361456341429 ) ) ;
#43025 =( NAMED_UNIT ( * ) PLANE_ANGLE_UNIT ( ) SI_UNIT ( $, .RADIAN. ) );
#43026 = CARTESIAN_POINT ( 'NONE',  ( 5.895480738319402114, 1.384055093596334274, 1.190509915477963698 ) ) ;
#43027 = CARTESIAN_POINT ( 'NONE',  ( -0.1042281025761494367, -0.9885194109933435058, -2.072332397174360352 ) ) ;
#43028 = CARTESIAN_POINT ( 'NONE',  ( -7.172426956829277778, 8.326585190177668849, -1.199719254218452935 ) ) ;
#43030 = CARTESIAN_POINT ( 'NONE',  ( -6.154475385960665790, 6.144919136567696505, 0.000000000000000000 ) ) ;
#43029 = CARTESIAN_POINT ( 'NONE',  ( 5.963815663052111304, 2.230244011310183794, -0.3799797021378086836 ) ) ;
#43031 = CARTESIAN_POINT ( 'NONE',  ( 2.297617436792959378, 1.628516202021938808, 1.335460665606647446 ) ) ;
#43032 = CARTESIAN_POINT ( 'NONE',  ( -6.459533842268148973, 6.500820668926428958, 0.000000000000000000 ) ) ;
#43033 = CARTESIAN_POINT ( 'NONE',  ( 7.401861798056875053, 10.72292363345333399, -1.199719254218441611 ) ) ;
#43034 = CARTESIAN_POINT ( 'NONE',  ( 7.065207446052794715, 9.336104335185329006, -1.443375672974064550 ) ) ;
#43035 = DIRECTION ( 'NONE',  ( 2.220446049250313081E-16, 0.000000000000000000, 1.000000000000000000 ) ) ;
#43036 = CARTESIAN_POINT ( 'NONE',  ( -7.202405917357668663, 9.425892875049191488, 1.599625672291295375 ) ) ;
#43037 = CARTESIAN_POINT ( 'NONE',  ( 0.000000000000000000, -4.500000000000003553, 2.000000000000000000 ) ) ;
#43038 = CARTESIAN_POINT ( 'NONE',  ( 8.581948047326003248, 9.114620264742901767, -0.7216878364870197293 ) ) ;
#43039 = CARTESIAN_POINT ( 'NONE',  ( 4.064005108223194718, 7.741596126659699983, 0.5534810405699239766 ) ) ;
#43040 = CARTESIAN_POINT ( 'NONE',  ( -4.466521540698216164, 7.298359999868178960, -1.199719254218452047 ) ) ;
#43041 = CARTESIAN_POINT ( 'NONE',  ( 3.270003694065525046, 0.5362613544047705183, -2.155619276402853224 ) ) ;
#43042 = CARTESIAN_POINT ( 'NONE',  ( -0.004863692847738298151, -0.4900785244342681368, -2.159743284330918112 ) ) ;
#43043 = CARTESIAN_POINT ( 'NONE',  ( -4.502189528189771472, 7.410248995266807803, -1.199719254218453823 ) ) ;
#43044 = CARTESIAN_POINT ( 'NONE',  ( 4.527533231959700366, 7.369540306339926516, 1.199719254218462483 ) ) ;
#43045 = CARTESIAN_POINT ( 'NONE',  ( 4.211346380768822506, -1.629847038978438079, -1.091715234301626314 ) ) ;
#43046 = CARTESIAN_POINT ( 'NONE',  ( 9.725276259704228821, 10.24057714594344048, 0.7998128361456462443 ) ) ;
#43047 = CARTESIAN_POINT ( 'NONE',  ( -5.626640144655740805, 6.175545741207232098, 0.8476793345565808435 ) ) ;
#43048 = FACE_OUTER_BOUND ( 'NONE', #147921, .T. ) ;
#43049 = CARTESIAN_POINT ( 'NONE',  ( -0.6823417656250003738, 1.217708333674752286, -1.181850606188749264 ) ) ;
#43050 = CARTESIAN_POINT ( 'NONE',  ( -4.665414256878301025, 6.536345614481700927, -1.443375672974066548 ) ) ;
#43052 = ORIENTED_EDGE ( 'NONE', *, *, #63645, .T. ) ;
#43051 = CARTESIAN_POINT ( 'NONE',  ( -6.453317930424837812, 7.591587675992828466, 1.082531754730549967 ) ) ;
#43053 = CARTESIAN_POINT ( 'NONE',  ( 3.990573222356631256, -1.218298518170106925, 1.735533685479621502 ) ) ;
#43054 = CARTESIAN_POINT ( 'NONE',  ( -4.773352600463090845, 7.726605912919016106, 1.199719254218452935 ) ) ;
#43055 = CARTESIAN_POINT ( 'NONE',  ( 4.909125497034264818, 1.879091090907711425, 1.068517025386829467 ) ) ;
#43056 = CARTESIAN_POINT ( 'NONE',  ( 4.476008884455379366, -1.787108923542475525, -0.4427587100873929815 ) ) ;
#43057 = CARTESIAN_POINT ( 'NONE',  ( -5.899211624428097878, 6.007801130575932014, 0.1941222073163356709 ) ) ;
#43058 = CARTESIAN_POINT ( 'NONE',  ( -1.364683531250000748, 1.821875000341421913, 0.000000000000000000 ) ) ;
#43059 = CARTESIAN_POINT ( 'NONE',  ( 6.492160993672303704, -0.4719841783793111145, -1.675048763955745645 ) ) ;
#43060 = CARTESIAN_POINT ( 'NONE',  ( 6.727182134110210043, 6.040083938853186396, 2.305853406558423302 ) ) ;
#43061 = CARTESIAN_POINT ( 'NONE',  ( 3.795919822146273326, 5.451659097302528068, -1.443375672974051449 ) ) ;
#43062 = FACE_BOUND ( 'NONE', #146284, .T. ) ;
#43063 = CARTESIAN_POINT ( 'NONE',  ( 3.749029689823797806, -1.768526636652943296, 1.242828150824742961 ) ) ;
#43064 = CLOSED_SHELL ( 'NONE', ( #14299, #173242, #9464, #194489, #31740, #44454, #55983, #49335, #148103, #15011, #109894, #40294, #49195, #108168, #135667, #13496, #167834, #145855, #207902, #104850, #37045, #47647, #148672, #212987, #47766, #44953, #112326, #2436, #119338, #145352, #89860, #189809, #78890, #90880, #41846, #79763, #206917, #62032, #177972, #176500, #212939, #14641, #89328, #160593, #78978, #10970, #39387, #75222, #145443, #65099, #179249, #93645, #180647, #25914, #85053, #33997, #122879, #84375, #105310, #15650, #31062, #42498, #133859, #125848, #41593, #7421, #174659, #9842, #26177, #104477, #35428, #203317, #206276, #203897, #13914, #129097 ) ) ;
#43065 = CARTESIAN_POINT ( 'NONE',  ( 5.466172646012215530, 1.646588110366095314, 1.163089216160061001 ) ) ;
#43066 = CARTESIAN_POINT ( 'NONE',  ( -8.636180661780672452, 9.177891648273343250, -0.7216878364870267237 ) ) ;
#43067 = CARTESIAN_POINT ( 'NONE',  ( 3.889662759143839299, 1.564074849111227516, 1.492423382767386730 ) ) ;
#43068 = CARTESIAN_POINT ( 'NONE',  ( 3.286357016390834218, -1.941589536447934972, -0.3404988550089679267 ) ) ;
#43069 = EDGE_CURVE ( 'NONE', #176773, #166897, #123353, .T. ) ;
#43070 = SURFACE_STYLE_FILL_AREA ( #143789 ) ;
#43071 = CARTESIAN_POINT ( 'NONE',  ( 1.185104535163916228, -2.251984199834490052, -0.5028348148315447963 ) ) ;
#43072 = CARTESIAN_POINT ( 'NONE',  ( 2.354824746187761164, -1.594966302183076667, 1.304983254080711808 ) ) ;
#43073 = CARTESIAN_POINT ( 'NONE',  ( 5.601106521291020712, -0.4677194688633263264, 1.884795189151499795 ) ) ;
#43076 = ORIENTED_EDGE ( 'NONE', *, *, #212743, .T. ) ;
#43075 = DIRECTION ( 'NONE',  ( 0.000000000000000000, 0.4225362441286110715, -0.9063460279593478219 ) ) ;
#43074 = CARTESIAN_POINT ( 'NONE',  ( -7.307481607641392429, 11.46921960898288972, 0.7216878364870458196 ) ) ;
#43078 = EDGE_CURVE ( 'NONE', #172976, #82895, #41310, .T. ) ;
#43077 = CARTESIAN_POINT ( 'NONE',  ( -6.414942957921379474, 7.513130201443591005, -1.199719254218452047 ) ) ;
#43079 = CARTESIAN_POINT ( 'NONE',  ( 6.610000000000006537, 0.002781820520842553934, 2.000159646111852929 ) ) ;
#43081 = ORIENTED_EDGE ( 'NONE', *, *, #48451, .F. ) ;
#43080 = CARTESIAN_POINT ( 'NONE',  ( -5.330290668828105538, 6.247702530834755130, 1.199719254218452935 ) ) ;
#43082 = CARTESIAN_POINT ( 'NONE',  ( -6.832946231163084860, 10.91559500309152675, 0.000000000000000000 ) ) ;
#43083 = CARTESIAN_POINT ( 'NONE',  ( 2.485638465518677176, 2.017858404210779888, -0.8937526715337427152 ) ) ;
#43084 = CARTESIAN_POINT ( 'NONE',  ( -1.642778471875000035, -0.5177083328553738761, -2.845375778867859751 ) ) ;
#43085 = CARTESIAN_POINT ( 'NONE',  ( 6.157081138237819218, 1.605775322519078729, -1.126676614267435150 ) ) ;
#43086 = CARTESIAN_POINT ( 'NONE',  ( -0.7500000000000179856, 9.041666666666669627, 1.299038105676658228 ) ) ;
#43087 = CARTESIAN_POINT ( 'NONE',  ( -1.001543065824772872E-14, 4.743750000682822154, 1.732050807568877637 ) ) ;
#43089 = CARTESIAN_POINT ( 'NONE',  ( -1.777638883463106279, 0.9165151389911794233, 1.199999999999999734 ) ) ;
#43088 = CARTESIAN_POINT ( 'NONE',  ( 0.1749903794560384862, 2.035240947854660920, -2.372290655319588382 ) ) ;
#43090 = CARTESIAN_POINT ( 'NONE',  ( 5.912015133600425187, 1.233162958052456348, -1.367321061651972869 ) ) ;
#43091 = ORIENTED_EDGE ( 'NONE', *, *, #59071, .T. ) ;
#43092 = CARTESIAN_POINT ( 'NONE',  ( -1.360316468750014884, -0.8593749996585950957, -6.938893903907228378E-15 ) ) ;
#43093 = B_SPLINE_CURVE_WITH_KNOTS ( 'NONE', 3,
 ( #105744, #167505, #104651, #168565, #87322, #36426, #118812, #136081 ),
 .UNSPECIFIED., .F., .F.,
 ( 4, 2, 2, 4 ),
 ( 1.069992374519254186E-15, 0.0004443203323512401174, 0.0006664804985263230895, 0.0008886406647014061157 ),
 .UNSPECIFIED. ) ;
#43094 = CARTESIAN_POINT ( 'NONE',  ( -6.507023659554960204, 9.678945805201045971, 1.199719254218452047 ) ) ;
#43095 = CARTESIAN_POINT ( 'NONE',  ( 11.04536101718726293, 13.50590937888830823, -1.100000000000000311 ) ) ;
#43096 = CARTESIAN_POINT ( 'NONE',  ( 6.293239850429793947, -0.1054838202379469042, -2.118119863012501991 ) ) ;
#43097 = CARTESIAN_POINT ( 'NONE',  ( 8.916861300403269297, 12.70687961389403675, 7.961634759295345809 ) ) ;
#43098 = CARTESIAN_POINT ( 'NONE',  ( 6.145923705696426431, 6.064665832934283962, 0.7998128361456341429 ) ) ;
#43099 = CARTESIAN_POINT ( 'NONE',  ( 0.4267267499857710367, 1.971919523859454237, 0.5989439635904010295 ) ) ;
#43102 = CARTESIAN_POINT ( 'NONE',  ( 4.335397732480402055, 0.7831895168094182846, -1.666506522714307437 ) ) ;
#43101 = CARTESIAN_POINT ( 'NONE',  ( 1.627181624537884286, 0.1412763417478210271, -1.855766238205541097 ) ) ;
#43100 = CARTESIAN_POINT ( 'NONE',  ( -6.381095703207996905, -8.233137084989849086, -7.037870247915946287 ) ) ;
#43103 = CARTESIAN_POINT ( 'NONE',  ( 7.955937213120826357, 8.176348258262782664, 0.7998128361456481317 ) ) ;
#43104 = DIRECTION ( 'NONE',  ( 0.6483454320283812411, 0.000000000000000000, -0.7613463080411777550 ) ) ;
#43105 = CARTESIAN_POINT ( 'NONE',  ( -4.132202957115018727, 8.042930226601317401, 0.000000000000000000 ) ) ;
#43107 = EDGE_LOOP ( 'NONE', ( #17433, #3929, #181485, #124735 ) ) ;
#43106 = CARTESIAN_POINT ( 'NONE',  ( -10.93005900490891413, -6.124285369217943753, 1.138412281109779656E-15 ) ) ;
#43108 = CARTESIAN_POINT ( 'NONE',  ( 4.881566871873391555, 2.059980941486462047, -0.7921658822237286346 ) ) ;
#43109 = CARTESIAN_POINT ( 'NONE',  ( 6.239586896912570069, -1.632293121298231675, -1.566800261409779349 ) ) ;
#43110 = CARTESIAN_POINT ( 'NONE',  ( -4.582292731738899505, 8.289832587096611860, 0.7216878364870458196 ) ) ;
#43111 = CARTESIAN_POINT ( 'NONE',  ( 0.3692113334803036606, -1.616751421056546789, -1.021125667832627260 ) ) ;
#43112 = CARTESIAN_POINT ( 'NONE',  ( 6.245329893291753365, 0.3200292219377436354, -1.888624904781693870 ) ) ;
#43113 = CARTESIAN_POINT ( 'NONE',  ( 3.375617060122621194, 6.882044303544283537, 1.040834085586084257E-14 ) ) ;
#43114 = DIRECTION ( 'NONE',  ( 0.000000000000000000, 0.000000000000000000, 1.000000000000000000 ) ) ;
#43115 = CARTESIAN_POINT ( 'NONE',  ( 5.461546741811521777, -1.510119879425949385, -1.173092037529008369 ) ) ;
#43116 = CIRCLE ( 'NONE', #88079, 0.05000000000000002359 ) ;
#43117 = CARTESIAN_POINT ( 'NONE',  ( 0.5494049127674709432, 0.5909524230637287490, -1.774924738581270089 ) ) ;
#43118 = CARTESIAN_POINT ( 'NONE',  ( 2.061732777098632230, 1.244387006429502396, 1.586668050434843158 ) ) ;
#43120 = CARTESIAN_POINT ( 'NONE',  ( 4.371769818753069359, 2.042916674203521854, -0.5113404140953855537 ) ) ;
#43119 = CARTESIAN_POINT ( 'NONE',  ( -9.352427035328430449, 9.805586384171650849, 1.040834085586084257E-14 ) ) ;
#43121 = AXIS2_PLACEMENT_3D ( 'NONE', #97750, #51108, #163809 ) ;
#43122 = CARTESIAN_POINT ( 'NONE',  ( 7.527801604085637699, 9.805521176231838609, 1.599625672291281386 ) ) ;
#43124 = CARTESIAN_POINT ( 'NONE',  ( -8.636707547105197946, 10.03491254549959777, -1.199719254218446718 ) ) ;
#43123 = CARTESIAN_POINT ( 'NONE',  ( 0.7499999999999867883, -0.1833333333333131421, -1.299038105676652899 ) ) ;
#43125 = CARTESIAN_POINT ( 'NONE',  ( 0.000000000000000000, 0.000000000000000000, 0.000000000000000000 ) ) ;
#43126 = CARTESIAN_POINT ( 'NONE',  ( 2.760026041568770072, 0.7230886973167930387, -1.886116010022680589 ) ) ;
#43127 = CARTESIAN_POINT ( 'NONE',  ( 0.6823417656249917140, 3.342708333674754506, 1.181850606188765695 ) ) ;
#43128 = CARTESIAN_POINT ( 'NONE',  ( 10.22248463502393001, 11.02857961705718282, 0.7216878364870438212 ) ) ;
#43129 = CARTESIAN_POINT ( 'NONE',  ( 4.007220386668823409, 1.851715269821294640, 1.114988852100415651 ) ) ;
#43130 = CARTESIAN_POINT ( 'NONE',  ( 1.394453263437886604E-15, -1.618749999044085230, 3.474999999999999645 ) ) ;
#43131 = CARTESIAN_POINT ( 'NONE',  ( 1.499999999999991118, 5.754166666666685970, 0.8660254037844524744 ) ) ;
#43133 = CARTESIAN_POINT ( 'NONE',  ( -9.617101990990361671, -9.241291349679078948, 0.3048231516917374040 ) ) ;
#43132 = CARTESIAN_POINT ( 'NONE',  ( 5.996449078994045223, 10.21788403546024782, 0.7998128361456331437 ) ) ;
#43134 = B_SPLINE_CURVE_WITH_KNOTS ( 'NONE', 3,
 ( #109756, #176819, #46842, #62008 ),
 .UNSPECIFIED., .F., .F.,
 ( 4, 4 ),
 ( 0.0006335992342242843800, 0.001020988003094342074 ),
 .UNSPECIFIED. ) ;
#43135 =( BOUNDED_SURFACE ( )  B_SPLINE_SURFACE ( 3, 2, ( 
 ( #3207, #168936, #121340 ),
 ( #86621, #105026, #171064 ),
 ( #4271, #22661, #88772 ),
 ( #6414, #26937, #156972 ) ),
 .UNSPECIFIED., .F., .F., .T. ) 
 B_SPLINE_SURFACE_WITH_KNOTS ( ( 4, 4 ),
 ( 3, 3 ),
 ( 0.01133669335851671123, 0.01377857026255084258 ),
 ( 0.000000000000000000, 1.000000000000000000 ),
 .UNSPECIFIED. ) 
 GEOMETRIC_REPRESENTATION_ITEM ( )  RATIONAL_B_SPLINE_SURFACE ( (
 ( 1.000000000000000000, 0.7169883299103944063, 1.000000000000000000),
 ( 1.000000000000000000, 0.7174882367753923074, 1.000000000000000000),
 ( 1.000000000000000000, 0.7180609655871059704, 1.000000000000000000),
 ( 1.000000000000000000, 0.7187540731122940008, 1.000000000000000000) ) ) 
 REPRESENTATION_ITEM ( '' )  SURFACE ( )  );
#43136 = CARTESIAN_POINT ( 'NONE',  ( 9.232739420781973294, 9.873876867108206667, -0.7216878364870257245 ) ) ;
#43138 = CARTESIAN_POINT ( 'NONE',  ( 8.279117182235522066, 15.22768336333823314, -8.688194556162066817 ) ) ;
#43137 = CARTESIAN_POINT ( 'NONE',  ( 1.803425971091272340, -1.834736872252432649, 1.160642024321426380 ) ) ;
#43139 = CIRCLE ( 'NONE', #188424, 6.264285714285709794 ) ;
#43141 = CARTESIAN_POINT ( 'NONE',  ( 0.6613494997313728030, 0.9071737413179328247, 1.602200521169500957 ) ) ;
#43140 = CARTESIAN_POINT ( 'NONE',  ( -5.422898255786186006, 9.270539031818461950, -0.7216878364870207285 ) ) ;
#43142 = CARTESIAN_POINT ( 'NONE',  ( -1.364683531250014514, 1.988541667008086655, -0.7879004041258289570 ) ) ;
#43143 = CARTESIAN_POINT ( 'NONE',  ( 1.611130907606239004, -0.2639259086049255965, 2.175532687872412829 ) ) ;
#43144 = CARTESIAN_POINT ( 'NONE',  ( 6.883263157960390011, 6.036220326785228352, 2.548703601196927515 ) ) ;
#43145 = CARTESIAN_POINT ( 'NONE',  ( 3.415140116862291908, 2.044469143995849780, 0.9693780919050251077 ) ) ;
#43146 = CARTESIAN_POINT ( 'NONE',  ( -5.506582945444718824, 9.576097202994168001, 0.7998128361456481317 ) ) ;
#43147 = CARTESIAN_POINT ( 'NONE',  ( -1.364683531250010295, 4.342708333674753618, 0.7879004041258379498 ) ) ;
#43148 = CARTESIAN_POINT ( 'NONE',  ( 6.124909263556299166, 6.992440323537196356, 0.9511531368890328020 ) ) ;
#43149 = CARTESIAN_POINT ( 'NONE',  ( -0.7500000000000006661, 12.95833333333333570, -1.299038105676657340 ) ) ;
#43150 = CARTESIAN_POINT ( 'NONE',  ( 7.702440666339465558, 8.158804663583751449, -0.7216878364870317197 ) ) ;
#43151 = CARTESIAN_POINT ( 'NONE',  ( 4.217836599137672060, -0.9083132443464863037, -1.518676986326646938 ) ) ;
#43152 = CARTESIAN_POINT ( 'NONE',  ( 8.127223016387999266, 11.56917838817298616, 1.199719254218460707 ) ) ;
#43154 = CONICAL_SURFACE ( 'NONE', #47013, 6.249999999999995559, 0.7853981633974548293 ) ;
#43153 = CARTESIAN_POINT ( 'NONE',  ( 0.6222711621935803628, -1.126682295963852276, -1.779026129514348353 ) ) ;
#43156 = CARTESIAN_POINT ( 'NONE',  ( -0.7500000000000006661, 1.608333333333357373, -1.299038105676652011 ) ) ;
#43155 = CARTESIAN_POINT ( 'NONE',  ( 1.364683531249997417, 10.23437500034139802, 2.602085213965210642E-15 ) ) ;
#43157 = CARTESIAN_POINT ( 'NONE',  ( -3.474632506852224356, 7.275764701294714420, -0.7998128361456481317 ) ) ;
#43158 = CARTESIAN_POINT ( 'NONE',  ( 6.187125092307005580, 1.678016663812756937, 1.117817459622950649 ) ) ;
#43159 = ORIENTED_EDGE ( 'NONE', *, *, #192264, .F. ) ;
#43160 = CARTESIAN_POINT ( 'NONE',  ( 7.944714827928056167, 8.371181508778631652, 0.7216878364870458196 ) ) ;
#43161 = CARTESIAN_POINT ( 'NONE',  ( 9.236128959407556849, 11.79856975744075598, -1.599625672291262513 ) ) ;
#43162 = CARTESIAN_POINT ( 'NONE',  ( 3.696050037196423332, -1.868490534004090931, -0.09263902202472776293 ) ) ;
#43163 = CARTESIAN_POINT ( 'NONE',  ( 4.539934223682924319, 1.348354173984022575, 1.571082123823979826 ) ) ;
#43164 = CARTESIAN_POINT ( 'NONE',  ( -6.089020385868867180, 7.236850217336030511, -1.082531754730549967 ) ) ;
#43165 = CIRCLE ( 'NONE', #18842, 0.09999999999999982514 ) ;
#43166 = CARTESIAN_POINT ( 'NONE',  ( 8.589254009457354400, 9.979550084910457031, -1.199719254218446718 ) ) ;
#43167 = CARTESIAN_POINT ( 'NONE',  ( -10.34217224912604571, 10.96028913360221502, 0.7998128361456462443 ) ) ;
#43168 = CARTESIAN_POINT ( 'NONE',  ( 6.964048179274811012, 8.153752959689313684, 1.199719254218452047 ) ) ;
#43169 = DIRECTION ( 'NONE',  ( 0.000000000000000000, 0.000000000000000000, -1.000000000000000000 ) ) ;
#43170 = CARTESIAN_POINT ( 'NONE',  ( -1.364683531250010295, 5.342708333674750953, 0.7879004041258379498 ) ) ;
#43171 = VECTOR ( 'NONE', #93798, 1000.000000000000000 ) ;
#43172 = CARTESIAN_POINT ( 'NONE',  ( 3.807043925254738781, -1.605251362286563177, 1.127602784832412386 ) ) ;
#43173 = CARTESIAN_POINT ( 'NONE',  ( 1.722029606037442040, -1.727736752315935265, -1.038835718801443653 ) ) ;
#43174 = CARTESIAN_POINT ( 'NONE',  ( -11.41157692552970460, 9.840896629129986195, 3.404533818002359435 ) ) ;
#43175 = CARTESIAN_POINT ( 'NONE',  ( 1.088877184111051832, 1.652420591378000791, -0.8765777015899289815 ) ) ;
#43176 = CARTESIAN_POINT ( 'NONE',  ( -1.364683531250010295, 3.780208333674750953, 0.7879004041258379498 ) ) ;
#43177 = CARTESIAN_POINT ( 'NONE',  ( 3.375247105954663596, -1.777387065663883714, -0.9453995415899820731 ) ) ;
#43179 = CARTESIAN_POINT ( 'NONE',  ( 3.638375168990032549, 0.7640726493506818651, 1.974712724135726516 ) ) ;
#43178 = CARTESIAN_POINT ( 'NONE',  ( -7.226132686403777150, 7.532835677000276675, 1.040834085586084257E-14 ) ) ;
#43180 = CARTESIAN_POINT ( 'NONE',  ( 6.825078400183572924, 7.629137130509068498, 2.744348168701661095 ) ) ;
#43181 = CARTESIAN_POINT ( 'NONE',  ( 5.318829906782316819, -1.502041817331278173, 1.425132596443792643 ) ) ;
#43182 = CARTESIAN_POINT ( 'NONE',  ( 5.969332771766739931, 10.18624834369502885, -0.7998128361456481317 ) ) ;
#43184 = CARTESIAN_POINT ( 'NONE',  ( 11.84668730067608600, 13.39999999999998259, 1.399999999999998357 ) ) ;
#43183 = CARTESIAN_POINT ( 'NONE',  ( 0.06416430596320726876, -1.362578676618180884, 1.585857439420575776 ) ) ;
#43186 = ORIENTED_EDGE ( 'NONE', *, *, #75725, .T. ) ;
#43185 = CARTESIAN_POINT ( 'NONE',  ( 5.473610661177239933, 1.758888005172161373, -0.4887267171112125164 ) ) ;
#43187 = CARTESIAN_POINT ( 'NONE',  ( 9.413438726589914651, 9.876766690643398405, 0.000000000000000000 ) ) ;
#43188 = CARTESIAN_POINT ( 'NONE',  ( 7.712222144931855539, -6.293595771081261780, -7.712222144931889289 ) ) ;
#43189 = CARTESIAN_POINT ( 'NONE',  ( 10.17148340815012020, 11.75186938811109627, -7.510838954888964025 ) ) ;
#43190 = CARTESIAN_POINT ( 'NONE',  ( -11.19490907666120272, 4.805655862119510680, 5.952061394947645745 ) ) ;
#43191 = CARTESIAN_POINT ( 'NONE',  ( -1.364683531250000748, 11.92187500034139980, 0.000000000000000000 ) ) ;
#43192 = CARTESIAN_POINT ( 'NONE',  ( 6.322915745023367506, 1.413667134151237459, -1.287952294376143447 ) ) ;
#43193 = CARTESIAN_POINT ( 'NONE',  ( -7.486073373039941359, 11.88550270185529278, -0.7998128361456291469 ) ) ;
#43194 = CARTESIAN_POINT ( 'NONE',  ( 5.819474248763732760, 7.812472595022922128, -1.599625672291262513 ) ) ;
#43195 = CARTESIAN_POINT ( 'NONE',  ( 1.360316468749964480, 2.796875000341370043, -3.989863994746656317E-14 ) ) ;
#43196 = CARTESIAN_POINT ( 'NONE',  ( 3.619663824724254741, 6.206396314611513532, -1.082531754730543971 ) ) ;
#43197 = CARTESIAN_POINT ( 'NONE',  ( 0.7500000000000006661, 9.833333333333332149, 1.299038105676657340 ) ) ;
#43198 = CARTESIAN_POINT ( 'NONE',  ( 4.172158584703322681, 5.890604320285754980, -1.599625672291256295 ) ) ;
#43199 = VERTEX_POINT ( 'NONE', #169066 ) ;
#43200 = CARTESIAN_POINT ( 'NONE',  ( -4.749098946536820520, 8.762642214260091933, 0.7998128361456281477 ) ) ;
#43201 = EDGE_CURVE ( 'NONE', #152613, #85328, #153925, .T. ) ;
#43202 = CARTESIAN_POINT ( 'NONE',  ( 10.99126615174920651, -5.166862915010145052, -0.4382560683119322009 ) ) ;
#43204 = CARTESIAN_POINT ( 'NONE',  ( 5.993586425693011144, 9.150212042353954800, -1.199719254218452047 ) ) ;
#43203 = CARTESIAN_POINT ( 'NONE',  ( 0.000000000000000000, 0.000000000000000000, 0.000000000000000000 ) ) ;
#43205 = DIRECTION ( 'NONE',  ( 1.000000000000000000, 0.000000000000000000, -1.224646799147353207E-16 ) ) ;
#43206 = CARTESIAN_POINT ( 'NONE',  ( -6.497792602234238934, 6.760263899176822022, -0.1076752790035370722 ) ) ;
#43207 = CARTESIAN_POINT ( 'NONE',  ( -6.751597309925468693, 6.979211071108916364, 0.7216878364870317197 ) ) ;
#43208 = CARTESIAN_POINT ( 'NONE',  ( 4.681643115420508039, 4.356338477612361260, 0.7998128361456341429 ) ) ;
#43209 = CARTESIAN_POINT ( 'NONE',  ( 2.869919493663297683, -1.948696178941822899, 0.2840860843679354764 ) ) ;
#43210 = CARTESIAN_POINT ( 'NONE',  ( 3.075796161730546707, -0.8146103074460913085, 1.844718345957757188 ) ) ;
#43211 = CARTESIAN_POINT ( 'NONE',  ( -7.588813295347149435, 9.876701482703580837, -1.599625672291263179 ) ) ;
#43212 = CARTESIAN_POINT ( 'NONE',  ( 6.727182134110195832, 3.687949058358138466, 2.603069318070629912 ) ) ;
#43213 = CARTESIAN_POINT ( 'NONE',  ( 3.240350661220792183, 0.5327334615983710941, 2.125583950146384904 ) ) ;
#43214 = CARTESIAN_POINT ( 'NONE',  ( 1.852440960305309137, 0.6018503411110776025, 1.830038407220703656 ) ) ;
#43215 = CARTESIAN_POINT ( 'NONE',  ( -7.645908563102897126, 11.00764485934031889, 1.199719254218453823 ) ) ;
#43216 = SURFACE_STYLE_USAGE ( .BOTH. , #29075 ) ;
#43217 = CARTESIAN_POINT ( 'NONE',  ( 0.2331563151865486683, 0.005903526429595904942, -1.945944850731482934 ) ) ;
#43218 = PRESENTATION_STYLE_ASSIGNMENT (( #174285 ) ) ;
#43219 = CARTESIAN_POINT ( 'NONE',  ( 6.934105498385400246, 10.17720795050327354, -1.199719254218441611 ) ) ;
#43220 = CARTESIAN_POINT ( 'NONE',  ( 6.322179702674084467, 6.270297829408224111, 1.040834085586084257E-14 ) ) ;
#43221 = CARTESIAN_POINT ( 'NONE',  ( -1.843739406749240750, 8.920000000000001705, 0.7750000000000013545 ) ) ;
#43222 = CARTESIAN_POINT ( 'NONE',  ( 5.234856708652227297, 7.200695141551334721, 1.443375672974065660 ) ) ;
#43223 = EDGE_LOOP ( 'NONE', ( #192492, #13501, #19205 ) ) ;
#43225 = CARTESIAN_POINT ( 'NONE',  ( 3.352200558804620645, 0.9032658637736007412, -1.799124413793075528 ) ) ;
#43224 = CARTESIAN_POINT ( 'NONE',  ( 6.392148736875968851, -0.4980823202534767624, -1.772533436741857260 ) ) ;
#43226 = CARTESIAN_POINT ( 'NONE',  ( 4.604990120689349098, 0.9883660700816098155, -2.075160223314168828 ) ) ;
#43228 = CARTESIAN_POINT ( 'NONE',  ( 2.904952611580268851, -1.549997479519327648, 1.029535618745812675 ) ) ;
#43227 = CARTESIAN_POINT ( 'NONE',  ( -0.1290005225502675879, -0.006633637972621592160, -2.173875058097324064 ) ) ;
#43229 = CARTESIAN_POINT ( 'NONE',  ( 0.000000000000000000, -0.5468749995220422155, -3.793834371823813001 ) ) ;
#43230 = CARTESIAN_POINT ( 'NONE',  ( -4.587666091342180508, 8.411066132956936059, -0.02982374410689043673 ) ) ;
#43231 = CARTESIAN_POINT ( 'NONE',  ( 6.328373294368253354, -0.9077179077918960948, -1.683272687665722467 ) ) ;
#43232 = CARTESIAN_POINT ( 'NONE',  ( -6.157374318900681764, 10.33535380535947290, 0.7998128361456481317 ) ) ;
#43233 = CARTESIAN_POINT ( 'NONE',  ( -4.611181642423629157, 7.433443445252599702, 1.082531754730549967 ) ) ;
#43234 = CARTESIAN_POINT ( 'NONE',  ( 5.478101502371197640, -2.040020603162643997, -0.4570242091310200427 ) ) ;
#43235 = CARTESIAN_POINT ( 'NONE',  ( 5.327991180490514012, 9.159814110640187579, 1.040834085586084257E-14 ) ) ;
#43236 = CARTESIAN_POINT ( 'NONE',  ( 2.974639739360878554, 6.521327805418967394, -0.5442850241774439546 ) ) ;
#43237 = CARTESIAN_POINT ( 'NONE',  ( 0.000000000000000000, 2.999999999999975131, 0.000000000000000000 ) ) ;
#43238 = CARTESIAN_POINT ( 'NONE',  ( 5.707552393076498198, -0.4128270653469527374, 1.674615006835003639 ) ) ;
#43239 = CARTESIAN_POINT ( 'NONE',  ( -5.935772324684618795, 5.819489221753827657, 0.000000000000000000 ) ) ;
#43240 = CARTESIAN_POINT ( 'NONE',  ( 1.230678901735713593, 1.732143722507371475, 0.08558704247295551015 ) ) ;
#43241 = FILL_AREA_STYLE ('',( #25884 ) ) ;
#43242 = DIRECTION ( 'NONE',  ( 0.000000000000000000, 0.000000000000000000, -1.000000000000000000 ) ) ;
#43243 = CARTESIAN_POINT ( 'NONE',  ( 6.069212964912024333, 1.910890531626436184, 1.030632506159581352 ) ) ;
#43244 = CARTESIAN_POINT ( 'NONE',  ( 4.986841741376339066, -0.2268417095559888130, -1.811474396668552700 ) ) ;
#43245 = CARTESIAN_POINT ( 'NONE',  ( 2.078885752709497492, 1.828579749420869094, 0.7109141669488158177 ) ) ;
#43246 = CARTESIAN_POINT ( 'NONE',  ( -2.969872605471120863, 6.605953636083950364, 2.420000000000000373 ) ) ;
#43247 = CARTESIAN_POINT ( 'NONE',  ( -10.34217224912604571, 10.96028913360221502, 0.7998128361456462443 ) ) ;
#43248 = CARTESIAN_POINT ( 'NONE',  ( 7.293396569147545527, 10.59638086639245280, 1.199719254218460707 ) ) ;
#43249 = CARTESIAN_POINT ( 'NONE',  ( 2.016421337698256711, -2.119947128278206971, 0.05498460973795551987 ) ) ;
#43250 = CARTESIAN_POINT ( 'NONE',  ( -4.134873662487946966, 3.926366815765101936, 1.214306433183764966E-14 ) ) ;
#43251 = VECTOR ( 'NONE', #129882, 1000.000000000000000 ) ;
#43252 = SURFACE_STYLE_FILL_AREA ( #59472 ) ;
#43253 = CARTESIAN_POINT ( 'NONE',  ( -4.639453055371920875, 6.917948375795638150, -1.210149155198399828 ) ) ;
#43254 = CARTESIAN_POINT ( 'NONE',  ( 0.9364849611055334755, -1.153160888946737961, 1.719151461320179042 ) ) ;
#43256 = CARTESIAN_POINT ( 'NONE',  ( 1.499999999999993117, 13.63541666734946034, 0.8660254037844409281 ) ) ;
#43255 = CARTESIAN_POINT ( 'NONE',  ( -10.60962610691052710, 4.146691825315026669, 5.607770086979924962 ) ) ;
#43259 = ORIENTED_EDGE ( 'NONE', *, *, #30625, .T. ) ;
#43258 = CARTESIAN_POINT ( 'NONE',  ( 3.246955274364712540, 2.167573551356954731, 0.4849624922091085866 ) ) ;
#43257 = AXIS2_PLACEMENT_3D ( 'NONE', #18394, #34653, #166802 ) ;
#43260 = CARTESIAN_POINT ( 'NONE',  ( 1.003029240585759263, -2.241230121681879073, 0.5102270476868026039 ) ) ;
#43262 = CARTESIAN_POINT ( 'NONE',  ( 6.350444629809289587, -2.052082384739264409, -0.2080662788188895607 ) ) ;
#43261 = CARTESIAN_POINT ( 'NONE',  ( 2.846322183865124700, 5.408127416896231665, -1.199719254218446718 ) ) ;
#43264 = CARTESIAN_POINT ( 'NONE',  ( 1.001543065824772753E-15, -1.662500000000000533, 4.012584370867899430 ) ) ;
#43263 = CARTESIAN_POINT ( 'NONE',  ( 3.691562964670865199, 7.528850235416478576, -0.7998128361456362523 ) ) ;
#43265 = FACE_OUTER_BOUND ( 'NONE', #66542, .T. ) ;
#43266 = CARTESIAN_POINT ( 'NONE',  ( 5.970224376651540155, -1.750504005202535796, -0.5711807346103907612 ) ) ;
#43267 = ADVANCED_FACE ( 'NONE', ( #83548 ), #182699, .T. ) ;
#43268 = CARTESIAN_POINT ( 'NONE',  ( -0.1102773484824119132, -0.006951161900758253548, -2.203378182130751206 ) ) ;
#43269 = CARTESIAN_POINT ( 'NONE',  ( 2.748708976905740897, -1.435238111852419562, 0.9561691852014215787 ) ) ;
#43270 = CARTESIAN_POINT ( 'NONE',  ( 0.6379081216283180034, 2.014007883293071899, -0.1037844182863178755 ) ) ;
#43271 = CARTESIAN_POINT ( 'NONE',  ( 2.954051123917677213, -2.124883583899921824, -0.8772644825643919342 ) ) ;
#43272 = CARTESIAN_POINT ( 'NONE',  ( 1.880510708721146118, -1.211181421480477693, 1.910737325309288304 ) ) ;
#43273 = CARTESIAN_POINT ( 'NONE',  ( 4.951841757635310870, 0.6616352077237923623, -1.999514825752574332 ) ) ;
#43274 = CARTESIAN_POINT ( 'NONE',  ( -6.970300371201519241, 7.304640985922785212, 0.7216878364870317197 ) ) ;
#43275 = CARTESIAN_POINT ( 'NONE',  ( 3.795971232924668648, -1.767634583600716569, -0.08911788016389800282 ) ) ;
#43277 = CARTESIAN_POINT ( 'NONE',  ( 6.216396969532355321, 2.137338928125806614, 0.8291867496624371059 ) ) ;
#43276 = CARTESIAN_POINT ( 'NONE',  ( 5.356880090730874677, 5.422317325373725794, 0.7216878364870328300 ) ) ;
#43278 = CARTESIAN_POINT ( 'NONE',  ( 4.857273802806507668, 1.820629801081237620, -0.2732171615176108848 ) ) ;
#43279 = CARTESIAN_POINT ( 'NONE',  ( -4.680589345215810049, 6.483773540883647435, -1.599625672291256295 ) ) ;
#43280 = CARTESIAN_POINT ( 'NONE',  ( 5.300874872818830852, 7.207439989753867238, 1.443375672974062551 ) ) ;
#43281 = CARTESIAN_POINT ( 'NONE',  ( 1.499999999999989120, 3.754166666666685082, 0.8660254037844524744 ) ) ;
#43282 = CARTESIAN_POINT ( 'NONE',  ( 4.752002516643937469, 0.8370584164609263800, 2.025481692006773748 ) ) ;
#43283 = CARTESIAN_POINT ( 'NONE',  ( -2.839543107058306592, 5.400218493954923815, -1.199719254218446718 ) ) ;
#43284 = CARTESIAN_POINT ( 'NONE',  ( -10.85353573482952072, -6.836568542495036205, 0.4635785636673775967 ) ) ;
#43285 = EDGE_CURVE ( 'NONE', #19327, #140589, #89084, .T. ) ;
#43286 = CARTESIAN_POINT ( 'NONE',  ( 4.439934286204096914, 1.349936692791346093, 1.569845735447549906 ) ) ;
#43287 = CARTESIAN_POINT ( 'NONE',  ( 0.04025042243083893495, 0.7762349914572730381, 1.861342399428978389 ) ) ;
#43288 = CARTESIAN_POINT ( 'NONE',  ( 0.6823417656249899377, 4.426041667008086655, -1.181850606188754593 ) ) ;
#43289 = CARTESIAN_POINT ( 'NONE',  ( 3.316937275718701894, 1.741877725598478976, 0.8232385001258867296 ) ) ;
#43290 = CARTESIAN_POINT ( 'NONE',  ( 1.364683531250000303, 9.755208333674735499, -0.7879004041258355073 ) ) ;
#43292 = CARTESIAN_POINT ( 'NONE',  ( -2.643476764984671767, 6.027880625883323518, 1.040834085586084257E-14 ) ) ;
#43291 = AXIS2_PLACEMENT_3D ( 'NONE', #145994, #47419, #209874 ) ;
#43293 = CARTESIAN_POINT ( 'NONE',  ( 0.5982529507728174822, 1.497540282193830841, 1.640895070279895895 ) ) ;
#43294 = ORIENTED_EDGE ( 'NONE', *, *, #199736, .T. ) ;
#43295 = CARTESIAN_POINT ( 'NONE',  ( -3.038435823238377687, 6.558942537171132514, -0.7216878364870458196 ) ) ;
#43296 = CARTESIAN_POINT ( 'NONE',  ( 3.680148631105580215, 6.380924938676771241, -1.199719254218446718 ) ) ;
#43297 = CARTESIAN_POINT ( 'NONE',  ( -2.788906526875773208E-15, 11.93750000000000000, -1.499999999999998446 ) ) ;
#43298 = DIRECTION ( 'NONE',  ( 0.7592566023652995710, -0.6507913734559650498, 0.000000000000000000 ) ) ;
#43299 = CARTESIAN_POINT ( 'NONE',  ( 3.931431380944446108, 2.807600633707128424, -0.7749999999999935829 ) ) ;
#43300 = FACE_BOUND ( 'NONE', #9557, .T. ) ;
#43301 = CARTESIAN_POINT ( 'NONE',  ( 1.451531895509536874, 1.483362660712841841, 1.284035263222626844 ) ) ;
#43302 = CARTESIAN_POINT ( 'NONE',  ( 1.364683531249988757, 0.9468750003414211358, 0.000000000000000000 ) ) ;
#43303 = CARTESIAN_POINT ( 'NONE',  ( 11.92619526913699524, 12.57219975838508041, 1.328859060402684644 ) ) ;
#43304 = CARTESIAN_POINT ( 'NONE',  ( 5.582460749670235423, 1.169929261559121247, -1.574690175210855747 ) ) ;
#43305 = CARTESIAN_POINT ( 'NONE',  ( -10.64723070543352712, 11.31619066596094392, 0.7998128361456462443 ) ) ;
#43306 = CARTESIAN_POINT ( 'NONE',  ( -6.521108698048791119, 6.710307690586118312, -0.7216878364870267237 ) ) ;
#43307 = CONICAL_SURFACE ( 'NONE', #164347, 6.249999999999995559, 0.7853981633974548293 ) ;
#43308 = CARTESIAN_POINT ( 'NONE',  ( 6.368072262247213899, 1.106822706796772193, 1.856716078747308263 ) ) ;
#43310 = VERTEX_POINT ( 'NONE', #202611 ) ;
#43309 = CARTESIAN_POINT ( 'NONE',  ( -0.5773502691896261751, -2.500000000000002220, -0.9999999999999991118 ) ) ;
#43311 = CARTESIAN_POINT ( 'NONE',  ( -0.6823417656249969321, 4.467708333674755394, -1.181850606188749264 ) ) ;
#43312 = CARTESIAN_POINT ( 'NONE',  ( 0.8603690976232807319, -1.359099942111790416, 1.285485254608226269 ) ) ;
#43313 = CARTESIAN_POINT ( 'NONE',  ( 6.432912826982137844, 0.8947389043411910770, 1.484938929457087164 ) ) ;
#43314 = EDGE_CURVE ( 'NONE', #211199, #7595, #148448, .T. ) ;
#43316 = CARTESIAN_POINT ( 'NONE',  ( 2.999763140970078901, -2.188934734890151113, 0.1099877568606702771 ) ) ;
#43315 = CARTESIAN_POINT ( 'NONE',  ( -1.752700365193352367E-14, 0.07812500034142640104, -1.570758158831804474 ) ) ;
#43317 = CARTESIAN_POINT ( 'NONE',  ( 4.893776379751743733, 1.706213512276737232, 1.553814486356275060 ) ) ;
#43318 = CARTESIAN_POINT ( 'NONE',  ( 6.239539339872155033, -1.489444859125512277, -1.424447411405028507 ) ) ;
#43319 = CARTESIAN_POINT ( 'NONE',  ( 2.484236259141327618, -0.3323325037456366093, -1.913154051555246316 ) ) ;
#43320 = CARTESIAN_POINT ( 'NONE',  ( -4.839897649954225223, 7.630002444046455778, 1.082531754730560403 ) ) ;
#43321 = EDGE_CURVE ( 'NONE', #173093, #182271, #138186, .T. ) ;
#43322 = CARTESIAN_POINT ( 'NONE',  ( 5.554972086574996304, 0.4156608669513594534, 2.079290889414136423 ) ) ;
#43323 = PRESENTATION_STYLE_ASSIGNMENT (( #175448 ) ) ;
#43324 = CARTESIAN_POINT ( 'NONE',  ( 3.481092415823695774, -2.014232707597499505, -0.09613569647320965861 ) ) ;
#43325 = CARTESIAN_POINT ( 'NONE',  ( -4.243338890952892406, 7.894386439512932618, -0.7216878364870257245 ) ) ;
#43326 = CARTESIAN_POINT ( 'NONE',  ( -6.084577077482911101, 10.32070003369722144, 0.000000000000000000 ) ) ;
#43327 = CARTESIAN_POINT ( 'NONE',  ( 9.531545685607134999, 11.07889037375188401, 1.199719254218450271 ) ) ;
#43328 = CARTESIAN_POINT ( 'NONE',  ( 6.933263157960367629, 7.629137130509066722, 2.653810918356712900 ) ) ;
#43329 = CARTESIAN_POINT ( 'NONE',  ( -6.448838341955544173, 7.552674816150118708, 1.199719254218452047 ) ) ;
#43331 = CARTESIAN_POINT ( 'NONE',  ( -5.981082042284069367, 7.006959133200059142, 1.199719254218452935 ) ) ;
#43330 = CARTESIAN_POINT ( 'NONE',  ( -4.900510728191886933, 8.135641830034209931, 1.034109914766440541 ) ) ;
#43332 = PLANE ( 'NONE',  #30120 ) ;
#43333 = ORIENTED_EDGE ( 'NONE', *, *, #171810, .F. ) ;
#43334 = CARTESIAN_POINT ( 'NONE',  ( 5.664934882792908688, -1.862169278537370465, -0.8832596265169431193 ) ) ;
#43335 = CARTESIAN_POINT ( 'NONE',  ( -5.573810548549546162, 9.516879716700865188, 0.7216878364870267237 ) ) ;
#43336 = CARTESIAN_POINT ( 'NONE',  ( -3.795392936821753604, 6.515376628678959392, -1.199719254218452047 ) ) ;
#43337 = CARTESIAN_POINT ( 'NONE',  ( -3.492107083971660586, 6.231819477012331632, 1.199719254218452935 ) ) ;
#43338 = CARTESIAN_POINT ( 'NONE',  ( 4.319013676512412303, 1.559734590277090716, -1.283057401373039141 ) ) ;
#43339 = CARTESIAN_POINT ( 'NONE',  ( 0.7499999999999902300, 1.233333333333357151, 1.299038105676657340 ) ) ;
#43341 = CARTESIAN_POINT ( 'NONE',  ( 8.351459436338029008, 10.76645531385962862, -1.443375672974063439 ) ) ;
#43340 = CARTESIAN_POINT ( 'NONE',  ( -3.481411583659053566, 7.283673624236017830, 0.000000000000000000 ) ) ;
#43342 = CARTESIAN_POINT ( 'NONE',  ( 5.282873410819217241, 9.315102745931094219, -0.7998128361456281477 ) ) ;
#43343 = CARTESIAN_POINT ( 'NONE',  ( 4.100502863055309533, -0.6448639507273239424, -1.957478828838697504 ) ) ;
#43344 = CARTESIAN_POINT ( 'NONE',  ( 3.182267690267494231, 1.591318367894577701, 1.238320962759748234 ) ) ;
#43345 = ORIENTED_EDGE ( 'NONE', *, *, #81818, .F. ) ;
#43346 = FACE_OUTER_BOUND ( 'NONE', #197298, .T. ) ;
#43347 = CARTESIAN_POINT ( 'NONE',  ( 3.517450787741589036, 6.191110788085444128, -1.199719254218446718 ) ) ;
#43349 = VERTEX_POINT ( 'NONE', #44156 ) ;
#43348 = CARTESIAN_POINT ( 'NONE',  ( -0.4301767877894160375, 8.007958762483717408, -1.954153227243214719 ) ) ;
#43350 = CARTESIAN_POINT ( 'NONE',  ( 2.671249783466634220, -0.7690017779844946499, -1.863883771055181660 ) ) ;
#43351 = CARTESIAN_POINT ( 'NONE',  ( 2.027068592762204080, -1.202062398780713748, -1.394650109237540070 ) ) ;
#43352 = CARTESIAN_POINT ( 'NONE',  ( 1.014821436393667398, -1.042085040243752481, -2.059081925104982336 ) ) ;
#43353 = CARTESIAN_POINT ( 'NONE',  ( 6.059568310664962709, 6.034194215389424798, 0.7998128361456352531 ) ) ;
#43354 = CARTESIAN_POINT ( 'NONE',  ( 3.251412196806032995, -1.765091617811213931, -1.247493029685270649 ) ) ;
#43355 = CARTESIAN_POINT ( 'NONE',  ( -6.901263884555985051, 8.010228272525461435, 1.199719254218450271 ) ) ;
#43356 = CARTESIAN_POINT ( 'NONE',  ( 3.778943494763619793, -2.265100756353163103, 0.3889815702934427688 ) ) ;
#43357 = ORIENTED_EDGE ( 'NONE', *, *, #41548, .T. ) ;
#43358 = CARTESIAN_POINT ( 'NONE',  ( -9.093502852636577316, 1.000000000000000888, -7.666967846417613863 ) ) ;
#43359 = CIRCLE ( 'NONE', #143731, 0.04999999999999969746 ) ;
#43360 = CARTESIAN_POINT ( 'NONE',  ( 0.8482696660519238874, 0.5391449902514727777, 1.791282564952957124 ) ) ;
#43361 = CARTESIAN_POINT ( 'NONE',  ( 5.875845355493965805, 1.173799634058709129, 1.583810875030462695 ) ) ;
#43363 = CARTESIAN_POINT ( 'NONE',  ( 8.337901282279995385, 11.71100668175994386, -1.082531754730543083 ) ) ;
#43362 = CARTESIAN_POINT ( 'NONE',  ( -0.6823417656249969321, 4.717708333674755394, -1.181850606188749264 ) ) ;
#43365 = CARTESIAN_POINT ( 'NONE',  ( 0.6630615684519860498, -1.595754342771567025, 1.524677653706180802 ) ) ;
#43364 = CARTESIAN_POINT ( 'NONE',  ( -5.900823170445743671, 7.907379670318584353, 1.599625672291269396 ) ) ;
#43366 = CARTESIAN_POINT ( 'NONE',  ( -1.500000000000056621, 7.388542872122511262, -4.154462424328199788 ) ) ;
#43367 = CARTESIAN_POINT ( 'NONE',  ( 6.491656622844908853, 6.468020902940851968, 0.7998128361456341429 ) ) ;
#43368 = CARTESIAN_POINT ( 'NONE',  ( -6.586563698140583512, 6.578745824119123675, 1.040834085586084257E-14 ) ) ;
#43369 = CARTESIAN_POINT ( 'NONE',  ( -1.772826578343123405, 4.000000000000045297, -0.4500000000000354272 ) ) ;
#43370 = CARTESIAN_POINT ( 'NONE',  ( 5.559438140644474835, 0.3852295531507047843, -1.933300702130675397 ) ) ;
#43371 = CARTESIAN_POINT ( 'NONE',  ( 4.055530604549876017, -1.917597210323931378, -1.283581016687604270 ) ) ;
#43372 = CARTESIAN_POINT ( 'NONE',  ( 6.197681965292040296, -1.348592564218813905, -1.282738352563756123 ) ) ;
#43373 = CARTESIAN_POINT ( 'NONE',  ( 2.905193444429104321, -1.717358790072313957, 1.142030567362181559 ) ) ;
#43374 = CARTESIAN_POINT ( 'NONE',  ( 5.178851490740187913, 8.985817805931475277, 0.7216878364870438212 ) ) ;
#43375 = CARTESIAN_POINT ( 'NONE',  ( 4.532168488718122390, 8.509556680138327778, 0.7998128361456271485 ) ) ;
#43376 = CARTESIAN_POINT ( 'NONE',  ( 5.422335090822693715, 5.290755458906732933, 0.000000000000000000 ) ) ;
#43377 = CARTESIAN_POINT ( 'NONE',  ( -1.201851678989727383E-14, 1.384375000341419693, 1.575800808251672791 ) ) ;
#43378 = CARTESIAN_POINT ( 'NONE',  ( 11.86145016429273191, 10.19999999999999929, -1.180000000000000604 ) ) ;
#43379 = CARTESIAN_POINT ( 'NONE',  ( 4.758548728272192108, 7.535095368750792666, -1.082531754730549078 ) ) ;
#43380 = CARTESIAN_POINT ( 'NONE',  ( 5.459503713743925069, 1.771904602436706222, 1.254488129281390751 ) ) ;
#43382 = CARTESIAN_POINT ( 'NONE',  ( 3.737712173649463399, 1.832726675769575486, 0.1767833568970395008 ) ) ;
#43381 = CARTESIAN_POINT ( 'NONE',  ( -4.121315508874276112, 4.870918184183829602, -1.082531754730549967 ) ) ;
#43384 = CARTESIAN_POINT ( 'NONE',  ( 6.620655732516631531, 2.063554893983750027, 2.233578047529918287 ) ) ;
#43383 = CARTESIAN_POINT ( 'NONE',  ( -11.89321938400720491, 11.26255278360659595, 1.599605898944226334 ) ) ;
#43385 = CARTESIAN_POINT ( 'NONE',  ( 5.917560222199001352, -1.216239291071326001, -1.822900893127032962 ) ) ;
#43386 = CARTESIAN_POINT ( 'NONE',  ( -0.3866937364864243554, 3.956598013261175772, 11.53692321988874170 ) ) ;
#43387 = CARTESIAN_POINT ( 'NONE',  ( 6.819229412991756334, -0.1648141603832406210, 2.226593352680195537 ) ) ;
#43388 = CARTESIAN_POINT ( 'NONE',  ( -4.233332884224245696, 7.524468121203685023, -1.021403520103405294 ) ) ;
#43389 = CARTESIAN_POINT ( 'NONE',  ( 11.41381675112453387, 10.90000000000000036, -3.704697986577182522 ) ) ;
#43390 = CARTESIAN_POINT ( 'NONE',  ( 6.218145995260431214, 7.027935176161393294, 1.016989286988238206 ) ) ;
#43391 = CARTESIAN_POINT ( 'NONE',  ( -3.309598895067336510, 6.875299454304925284, 0.000000000000000000 ) ) ;
#43392 = CARTESIAN_POINT ( 'NONE',  ( 4.421367491832282504, 5.291255174293369556, 1.082531754730549078 ) ) ;
#43393 = CARTESIAN_POINT ( 'NONE',  ( 0.5316681593682397455, 0.9152217321290991858, -1.514687162473850490 ) ) ;
#43394 = CARTESIAN_POINT ( 'NONE',  ( 5.426436493548534301, -0.9073095142285032555, -1.797119830347380542 ) ) ;
#43395 = CARTESIAN_POINT ( 'NONE',  ( 7.332262146892202459, 7.448727347662698506, -0.7998128361456281477 ) ) ;
#43396 = CARTESIAN_POINT ( 'NONE',  ( 3.751088088702017487, -1.722778774704723181, 1.210957861328536112 ) ) ;
#43397 = CARTESIAN_POINT ( 'NONE',  ( 3.181152667880298157, 1.511915621606011007, 1.176196041047285812 ) ) ;
#43398 = DIRECTION ( 'NONE',  ( 1.000000000000000000, -4.985516615831701596E-16, 0.000000000000000000 ) ) ;
#43399 = CARTESIAN_POINT ( 'NONE',  ( 4.404722228293363351, 0.5232710054461316984, 1.898709409516568192 ) ) ;
#43400 = CARTESIAN_POINT ( 'NONE',  ( 6.011974661143067777, -0.6766988549865710079, 1.903214300750865506 ) ) ;
#43401 = CARTESIAN_POINT ( 'NONE',  ( 1.586564105604048480, -0.2713065988851799393, -1.850747533123621391 ) ) ;
#43404 = ORIENTED_EDGE ( 'NONE', *, *, #80530, .T. ) ;
#43403 = CARTESIAN_POINT ( 'NONE',  ( 1.459083999156213451, -1.613880964290700160, 1.025699646091532857 ) ) ;
#43402 = CARTESIAN_POINT ( 'NONE',  ( 4.758271111750849158, 0.6642134669661412527, 1.592074403417756301 ) ) ;
#43406 = CARTESIAN_POINT ( 'NONE',  ( 4.907688418466886304, 5.788353245375237321, -1.082531754730548412 ) ) ;
#43405 = CARTESIAN_POINT ( 'NONE',  ( 2.719571217284349363, -0.2154062111461417517, 2.196339928330424129 ) ) ;
#43407 = CARTESIAN_POINT ( 'NONE',  ( -1.201851678989727383E-14, 2.634375000341417916, 1.575800808251672791 ) ) ;
#43408 = CARTESIAN_POINT ( 'NONE',  ( 6.461383593301071926, 1.630371061775518271, 1.090930979547571456 ) ) ;
#43409 = CARTESIAN_POINT ( 'NONE',  ( 6.428537391173986038, 10.65171072301167854, 0.7998128361456462443 ) ) ;
#43411 = CARTESIAN_POINT ( 'NONE',  ( -9.604686356149278126, 4.518467169708413778, -7.193747284969076006 ) ) ;
#43410 = MECHANICAL_DESIGN_GEOMETRIC_PRESENTATION_REPRESENTATION (  '', ( #126503 ), #39989 ) ;
#43412 = CARTESIAN_POINT ( 'NONE',  ( 10.51568781791557328, 13.61256730203911758, 3.554797817682051164 ) ) ;
#43413 = CARTESIAN_POINT ( 'NONE',  ( -5.606868911964699720, 5.576453016528778228, -0.3534498849190413350 ) ) ;
#43414 = FACE_OUTER_BOUND ( 'NONE', #773, .T. ) ;
#43415 = ORIENTED_EDGE ( 'NONE', *, *, #37914, .F. ) ;
#43416 = CARTESIAN_POINT ( 'NONE',  ( 1.750525128138082254, -2.060206210462053988, -0.2049951091474821463 ) ) ;
#43418 = CARTESIAN_POINT ( 'NONE',  ( 0.7499999999999902300, 3.816666666666690411, -1.299038105676658228 ) ) ;
#43417 = AXIS2_PLACEMENT_3D ( 'NONE', #73869, #176701, #26170 ) ;
#43419 = CARTESIAN_POINT ( 'NONE',  ( 6.043183783389218355, 8.073467052085995022, 1.599625672291267398 ) ) ;
#43420 = CARTESIAN_POINT ( 'NONE',  ( -7.121056995675673740, 9.330985799753529264, -1.599625672291263179 ) ) ;
#43421 = CARTESIAN_POINT ( 'NONE',  ( 3.555981428534177091, 7.370671776590375757, 0.7998128361456271485 ) ) ;
#43422 = CARTESIAN_POINT ( 'NONE',  ( 0.04752895628580295490, -1.845665702319599921, 0.8205699430347112022 ) ) ;
#43423 = CARTESIAN_POINT ( 'NONE',  ( -1.201851678989727383E-14, 5.837500000000023448, -1.732050807568863648 ) ) ;
#43424 = CARTESIAN_POINT ( 'NONE',  ( -1.364683531250012516, 3.030208333674755394, 0.7879004041258379498 ) ) ;
#43426 = CARTESIAN_POINT ( 'NONE',  ( 3.277320446201373638, 4.846626492033466072, 1.599625672291267398 ) ) ;
#43425 = CARTESIAN_POINT ( 'NONE',  ( 1.423205080756922314, 7.980384757729337863, 10.65537363484301459 ) ) ;
#43427 = CARTESIAN_POINT ( 'NONE',  ( 5.694685421800770087, -1.276849089899323886, -1.560260200769040706 ) ) ;
#43428 = CARTESIAN_POINT ( 'NONE',  ( 4.856599191889834799, -1.806003080954875495, -0.6394761690226327122 ) ) ;
#43429 = DIRECTION ( 'NONE',  ( 0.000000000000000000, 0.000000000000000000, -1.000000000000000000 ) ) ;
#43430 = CARTESIAN_POINT ( 'NONE',  ( 3.105210138592546798, -0.4252477525170209605, 2.149737936336936883 ) ) ;
#43431 = CARTESIAN_POINT ( 'NONE',  ( 0.000000000000000000, 12.29999999999998295, 0.000000000000000000 ) ) ;
#43432 = CARTESIAN_POINT ( 'NONE',  ( 1.499999999999989120, 0.3062500006828158816, 0.000000000000000000 ) ) ;
#43433 = CARTESIAN_POINT ( 'NONE',  ( 5.730732165690560542, 1.348809278943388534, -1.494750323444839601 ) ) ;
#43434 = CARTESIAN_POINT ( 'NONE',  ( 1.089939655121434203, 1.141396045679959004, 1.534244836814010693 ) ) ;
#43435 = CARTESIAN_POINT ( 'NONE',  ( -4.934277840369690971, 7.844075682818238526, -1.199719254218452047 ) ) ;
#43437 = CARTESIAN_POINT ( 'NONE',  ( -0.1058464554703278104, -0.8645191204341062807, -1.819937883007181512 ) ) ;
#43436 = CARTESIAN_POINT ( 'NONE',  ( -2.331639231870358930, 5.664070170583284103, -0.7216878364870267237 ) ) ;
#43438 = CARTESIAN_POINT ( 'NONE',  ( -1.364683531250010295, 10.19270833367473017, 0.7879004041258445001 ) ) ;
#43440 = CARTESIAN_POINT ( 'NONE',  ( -6.306477729012051725, 7.386587434382707151, 1.199719254218452047 ) ) ;
#43439 = CARTESIAN_POINT ( 'NONE',  ( 3.614856758894122724, -0.1514882961727741506, 2.085299387778175806 ) ) ;
#43442 = ORIENTED_EDGE ( 'NONE', *, *, #26426, .F. ) ;
#43441 = CARTESIAN_POINT ( 'NONE',  ( 1.676317214473854067, -1.636236659294947104, -0.5456935059391133658 ) ) ;
#43443 = CARTESIAN_POINT ( 'NONE',  ( 1.499999999999963141, 7.750000000000000000, -9.886859966642596476 ) ) ;
#43444 = CARTESIAN_POINT ( 'NONE',  ( 6.498435699651741615, 6.475929825882159818, -0.7998128361456281477 ) ) ;
#43445 = EDGE_CURVE ( 'NONE', #118697, #61441, #171944, .T. ) ;
#43446 = SURFACE_STYLE_USAGE ( .BOTH. , #95404 ) ;
#43447 = CARTESIAN_POINT ( 'NONE',  ( 7.439168848973789494, -6.700000000000001954, 8.103009739378206788 ) ) ;
#43448 = CARTESIAN_POINT ( 'NONE',  ( -11.78331023100045627, 9.799999999999998934, -1.800000000000001155 ) ) ;
#43449 = CARTESIAN_POINT ( 'NONE',  ( 5.035963992472171746, 7.962709526937818083, 1.199719254218462483 ) ) ;
#43450 = EDGE_LOOP ( 'NONE', ( #169588, #199582, #95288, #23578 ) ) ;
#43451 = CARTESIAN_POINT ( 'NONE',  ( -5.204170427930421283E-15, -2.000000000000001776, -12.26547674076639716 ) ) ;
#43452 = ORIENTED_EDGE ( 'NONE', *, *, #103866, .T. ) ;
#43453 = CARTESIAN_POINT ( 'NONE',  ( 3.105918186854994989, -0.7317858000257486673, 1.657260211903899938 ) ) ;
#43454 = VECTOR ( 'NONE', #193167, 1000.000000000000000 ) ;
#43455 = ORIENTED_EDGE ( 'NONE', *, *, #158613, .F. ) ;
#43456 = CARTESIAN_POINT ( 'NONE',  ( 3.728655938958122196, 4.308852335994623139, -1.199719254218446718 ) ) ;
#43457 = ORIENTED_EDGE ( 'NONE', *, *, #117446, .F. ) ;
#43458 = CARTESIAN_POINT ( 'NONE',  ( 4.980641328173811999, 6.904110530993182948, 1.599625672291269396 ) ) ;
#43459 = CARTESIAN_POINT ( 'NONE',  ( 3.334412561109405537, 1.147067551318830203, -1.402027596893473449 ) ) ;
#43460 = CARTESIAN_POINT ( 'NONE',  ( 6.539320575229245591, 2.459069921018588900, 2.280790101157427419 ) ) ;
#43461 = CARTESIAN_POINT ( 'NONE',  ( -10.99529341469513355, -7.794776013890357014, 0.3288329489800617123 ) ) ;
#43462 = CARTESIAN_POINT ( 'NONE',  ( 5.244386534325491844, 6.400378350754194479, 1.153371672928265479 ) ) ;
#43463 = EDGE_CURVE ( 'NONE', #170139, #145077, #675, .T. ) ;
#43464 = CARTESIAN_POINT ( 'NONE',  ( 4.000341067899515046, 1.851953036565538335, 0.1839423254178795542 ) ) ;
#43465 = ADVANCED_FACE ( 'NONE', ( #16939, #79831 ), #30029, .T. ) ;
#43466 = CARTESIAN_POINT ( 'NONE',  ( 1.686979003181095615, 1.593666142434764454, 1.062572995559516009 ) ) ;
#43467 = CARTESIAN_POINT ( 'NONE',  ( 1.307329191252764922, -0.4475898743878243824, 1.769731943805815222 ) ) ;
#43468 = CARTESIAN_POINT ( 'NONE',  ( 1.500000000000001332, 11.62499999999999645, 0.000000000000000000 ) ) ;
#43469 = DIRECTION ( 'NONE',  ( 0.000000000000000000, 0.000000000000000000, -1.000000000000000000 ) ) ;
#43470 = COLOUR_RGB ( '', 0.66274510, 0.83137255, 0.94901961) ;
#43471 = CARTESIAN_POINT ( 'NONE',  ( 5.606371582794006159, 7.377293116531995487, 1.238817421570908905 ) ) ;
#43472 = CARTESIAN_POINT ( 'NONE',  ( 7.320800350271525758, 15.00158243878686726, 10.35317514277968343 ) ) ;
#43473 = DIRECTION ( 'NONE',  ( -0.9980789807931677027, 0.06195440338564740107, 0.000000000000000000 ) ) ;
#43474 = CARTESIAN_POINT ( 'NONE',  ( -5.905617501100172362, 6.087552950387692619, -0.6644227375040656636 ) ) ;
#43475 = CARTESIAN_POINT ( 'NONE',  ( 7.266807147244743526, 11.42176607185347414, -0.7216878364870267237 ) ) ;
#43476 = CARTESIAN_POINT ( 'NONE',  ( 5.700047960291365179, 0.8015925475840814940, -1.799137058317602067 ) ) ;
#43477 = CARTESIAN_POINT ( 'NONE',  ( -5.752737250900127997, 5.605948302338584099, 0.000000000000000000 ) ) ;
#43478 = CARTESIAN_POINT ( 'NONE',  ( -9.500331257164621235, -7.246166700193446886, -1.011626589619743066E-12 ) ) ;
#43479 = AXIS2_PLACEMENT_3D ( 'NONE', #168425, #201951, #180422 ) ;
#43480 = CARTESIAN_POINT ( 'NONE',  ( 6.703104427915338448, -0.4847493572297522091, 2.145077170986497528 ) ) ;
#43481 = CARTESIAN_POINT ( 'NONE',  ( 8.932124273304774320, 9.315233161810734686, 0.7998128361456462443 ) ) ;
#43482 = CARTESIAN_POINT ( 'NONE',  ( 5.596683124612600757, -0.4680951147424931569, -1.868546797846575513 ) ) ;
#43483 = CARTESIAN_POINT ( 'NONE',  ( -4.693093728624763372, 8.627026450037540428, 0.7998128361456481317 ) ) ;
#43484 = CARTESIAN_POINT ( 'NONE',  ( 1.307329191252764922, -0.4475898743878243824, 1.769731943805815222 ) ) ;
#43485 = CARTESIAN_POINT ( 'NONE',  ( 2.596532132193625664, -2.201043451360765957, -0.1612727490639675743 ) ) ;
#43486 = DIRECTION ( 'NONE',  ( 1.000000000000000000, 0.000000000000000000, 0.000000000000000000 ) ) ;
#43487 = CARTESIAN_POINT ( 'NONE',  ( 0.4746845637013075159, -1.383529810647101455, 1.320479256824915071 ) ) ;
#43488 = CARTESIAN_POINT ( 'NONE',  ( 0.2913706227113096459, -1.802261421121041707, 0.7947621968238273160 ) ) ;
#43489 = CARTESIAN_POINT ( 'NONE',  ( 3.175267148988625721, 1.234016112977231794, 1.499580727898646604 ) ) ;
#43490 = VERTEX_POINT ( 'NONE', #195728 ) ;
#43491 = CARTESIAN_POINT ( 'NONE',  ( 0.5442957877539145173, 1.882187304385819493, -0.7230256762977352869 ) ) ;
#43493 = CARTESIAN_POINT ( 'NONE',  ( 6.965680890820083349, -0.4048625726877760900, 1.822745621051139020 ) ) ;
#43492 = CARTESIAN_POINT ( 'NONE',  ( -5.712781623311813384, 7.758274208654143855, -1.599625672291271394 ) ) ;
#43494 = CARTESIAN_POINT ( 'NONE',  ( 4.037295881819344956, 7.932205305423046582, -0.7998128361456362523 ) ) ;
#43495 = DIRECTION ( 'NONE',  ( 0.000000000000000000, 1.804652791718263484E-16, -1.000000000000000000 ) ) ;
#43496 = CARTESIAN_POINT ( 'NONE',  ( 9.642873567817520808, 12.27310513391906532, 1.599625672291279388 ) ) ;
#43497 = CARTESIAN_POINT ( 'NONE',  ( -5.579343907223557331, 6.467988298970945849, 1.199719254218450271 ) ) ;
#43498 = CARTESIAN_POINT ( 'NONE',  ( -6.587282531393266360, 8.778525268082516320, 1.599625672291269396 ) ) ;
#43499 = CARTESIAN_POINT ( 'NONE',  ( 2.279091853667324141, 2.002311374866962979, -0.8913168663882904408 ) ) ;
#43500 = CARTESIAN_POINT ( 'NONE',  ( 2.412988153552339643, 5.758977245878946327, 0.7216878364870438212 ) ) ;
#43501 = CARTESIAN_POINT ( 'NONE',  ( -10.62873463776380056, 12.30000000000000071, -3.200000000000001510 ) ) ;
#43502 = CARTESIAN_POINT ( 'NONE',  ( -5.810221930991193690E-16, 2.500000000682804036, -1.225000000000023626 ) ) ;
#43503 = CARTESIAN_POINT ( 'NONE',  ( 3.123480263227970344, -1.759325740769552393, 0.4874977319994436287 ) ) ;
#43504 = DIRECTION ( 'NONE',  ( 1.561251128379126077E-17, 1.301042606982605475E-17, 1.000000000000000000 ) ) ;
#43505 = CARTESIAN_POINT ( 'NONE',  ( -4.603156847039612920, 5.329103395422994716, 1.199719254218462483 ) ) ;
#43506 = CARTESIAN_POINT ( 'NONE',  ( -4.941402330188276792, 8.092876352253616901, -1.081280284042404727 ) ) ;
#43507 = CARTESIAN_POINT ( 'NONE',  ( -0.02968770228137588424, 4.095675376368371090, -2.381331788581673159 ) ) ;
#43508 = CARTESIAN_POINT ( 'NONE',  ( 7.781490099239519509, 11.16582331816642260, 1.199719254218460707 ) ) ;
#43509 = CARTESIAN_POINT ( 'NONE',  ( 0.4692025345035084061, 0.1902923850431673669, -1.917074784726199965 ) ) ;
#43510 = CARTESIAN_POINT ( 'NONE',  ( 5.207842308544940124, 0.6190457291245822224, -1.861560318597937913 ) ) ;
#43511 = CARTESIAN_POINT ( 'NONE',  ( 0.7500000000000006661, 14.91666666666666785, -1.299038105676657340 ) ) ;
#43512 = CARTESIAN_POINT ( 'NONE',  ( -6.201965203247477909, 9.323044272842313518, 1.199719254218452047 ) ) ;
#43513 = CARTESIAN_POINT ( 'NONE',  ( 5.148345644887269756, 7.029489223833707001, -1.599625672291256295 ) ) ;
#43514 = CARTESIAN_POINT ( 'NONE',  ( 5.249643141573060667, 2.189086832579402842, -0.1069518675670885766 ) ) ;
#43515 = DIRECTION ( 'NONE',  ( 0.000000000000000000, 0.000000000000000000, -1.000000000000000000 ) ) ;
#43516 = CARTESIAN_POINT ( 'NONE',  ( 4.188381925097388603, 1.111774711627441681, -1.746232563387891679 ) ) ;
#43518 = CARTESIAN_POINT ( 'NONE',  ( 0.6823417656249899377, 1.905208333674752952, 1.181850606188755259 ) ) ;
#43517 = FACE_OUTER_BOUND ( 'NONE', #86542, .T. ) ;
#43519 = ORIENTED_EDGE ( 'NONE', *, *, #127165, .T. ) ;
#43520 = CARTESIAN_POINT ( 'NONE',  ( 4.412867445986612402, -1.413514171388057239, -1.812631114537610166 ) ) ;
#43521 = CARTESIAN_POINT ( 'NONE',  ( 6.304178240674458422, 10.29869901418813782, 1.040834085586084257E-14 ) ) ;
#43523 = DIRECTION ( 'NONE',  ( 0.6507913734559596097, 0.7592566023653043450, 0.000000000000000000 ) ) ;
#43522 = CARTESIAN_POINT ( 'NONE',  ( 5.614485009834906393, 6.683225611963085733, -1.082531754730548412 ) ) ;
#43524 = CARTESIAN_POINT ( 'NONE',  ( -11.41381675112453387, 13.39999999999998259, 3.704697986577180746 ) ) ;
#43525 = CARTESIAN_POINT ( 'NONE',  ( -5.749539660647037032, 8.865490816466966351, 1.199719254218454489 ) ) ;
#43526 = CARTESIAN_POINT ( 'NONE',  ( 4.980387307702104138, -0.2395764092862572303, -1.927055426435628327 ) ) ;
#43527 = VERTEX_POINT ( 'NONE', #48427 ) ;
#43528 = CARTESIAN_POINT ( 'NONE',  ( 9.747949258101261449, 11.43532422494874368, -1.082531754730537088 ) ) ;
#43529 = EDGE_CURVE ( 'NONE', #71781, #142721, #102111, .T. ) ;
#43530 = ORIENTED_EDGE ( 'NONE', *, *, #73420, .F. ) ;
#43531 = CARTESIAN_POINT ( 'NONE',  ( 5.291234991620994421, -0.05314252713351996088, -1.911838368980276925 ) ) ;
#43532 = CARTESIAN_POINT ( 'NONE',  ( 6.000961845343044665, 1.407127125985812466, -0.9971243314716814465 ) ) ;
#43533 = CARTESIAN_POINT ( 'NONE',  ( 4.505092375653735992, -0.09411930587044713137, 2.014432893821124004 ) ) ;
#43535 = DIRECTION ( 'NONE',  ( 0.000000000000000000, 1.000000000000000000, 0.000000000000000000 ) ) ;
#43534 = CARTESIAN_POINT ( 'NONE',  ( -8.479735010343349089, 11.98044238112085758, 1.199719254218453823 ) ) ;
#43536 = CARTESIAN_POINT ( 'NONE',  ( -3.285556943750000070, -2.996874999522041616, 0.000000000000000000 ) ) ;
#43538 = CARTESIAN_POINT ( 'NONE',  ( 0.4789242711138582687, 1.653723610832663393, -0.6310274585415026616 ) ) ;
#43537 = CARTESIAN_POINT ( 'NONE',  ( 1.377023180242874068, 1.931088066391934976, -0.8015266744223081830 ) ) ;
#43539 = CARTESIAN_POINT ( 'NONE',  ( 5.783827325522512552, 1.646840809264274119, -1.163266671679111353 ) ) ;
#43541 = CARTESIAN_POINT ( 'NONE',  ( 2.660454013544113927, -1.579728858233371946, 1.661220326946882375 ) ) ;
#43540 = CARTESIAN_POINT ( 'NONE',  ( 5.585032934186686226, 5.480569609498057382, 0.000000000000000000 ) ) ;
#43542 = CARTESIAN_POINT ( 'NONE',  ( 2.607021377293942344, -1.721407032317923802, 0.2550150930856145970 ) ) ;
#43543 = CARTESIAN_POINT ( 'NONE',  ( 3.094099843433151253, 1.348383549611749332, 1.636666742212993686 ) ) ;
#43544 = CARTESIAN_POINT ( 'NONE',  ( -1.123270288250339588, 3.283552654332833054, 0.7749999999993804067 ) ) ;
#43545 = CARTESIAN_POINT ( 'NONE',  ( 0.6317059331818836165, 0.1778517408326604765, -1.724704385026996079 ) ) ;
#43546 = CARTESIAN_POINT ( 'NONE',  ( -1.360316468750021768, 1.421875000341424222, -4.510281037539698445E-14 ) ) ;
#43547 = CARTESIAN_POINT ( 'NONE',  ( 2.207255083745041979, -1.492367883816644314, -1.111680554738720073 ) ) ;
#43548 =( BOUNDED_CURVE ( )  B_SPLINE_CURVE ( 3, ( #3067, #100597, #50781, #147238 ),
 .UNSPECIFIED., .F., .T. ) 
 B_SPLINE_CURVE_WITH_KNOTS ( ( 4, 4 ),
 ( 0.000000000000000000, 0.4999999999999939493 ),
 .UNSPECIFIED. ) 
 CURVE ( )  GEOMETRIC_REPRESENTATION_ITEM ( )  RATIONAL_B_SPLINE_CURVE ( ( 1.000000000000000000, 0.3333333333333414195, 0.3333333333333333703, 0.9999999999999918954 ) ) 
 REPRESENTATION_ITEM ( '' )  );
#43549 = CARTESIAN_POINT ( 'NONE',  ( 2.822911419172136949, -1.498817844263359067, 1.571052884911597003 ) ) ;
#43550 = CARTESIAN_POINT ( 'NONE',  ( 3.046111529846948329, 0.9110102549910354952, 1.799122713138465279 ) ) ;
#43551 = CARTESIAN_POINT ( 'NONE',  ( 3.593750000000001776, -1.895863743164161841, -0.7852924748297959168 ) ) ;
#43552 = CARTESIAN_POINT ( 'NONE',  ( -1.402160292154681736E-14, 2.118750000682816825, -1.732050807568863648 ) ) ;
#43553 = CARTESIAN_POINT ( 'NONE',  ( 0.3934162593667543950, 1.425226140442600098, 1.296210752655905463 ) ) ;
#43554 = CARTESIAN_POINT ( 'NONE',  ( -1.364683531250010295, 14.13020833367473372, 0.7879004041258445001 ) ) ;
#43555 = CARTESIAN_POINT ( 'NONE',  ( 3.902737194376978636, -2.197594379623767580, -0.3235144178719475128 ) ) ;
#43556 = ORIENTED_EDGE ( 'NONE', *, *, #213928, .T. ) ;
#43557 = CARTESIAN_POINT ( 'NONE',  ( -0.2110808730067326444, 2.048707873362776599, -2.213945011526836204 ) ) ;
#43558 = CARTESIAN_POINT ( 'NONE',  ( -0.7500000000000006661, -0.8916666666666448471, -1.299038105676652011 ) ) ;
#43559 = CARTESIAN_POINT ( 'NONE',  ( 8.052653171512838881, 11.48218023581863001, -1.199719254218446718 ) ) ;
#43560 = CARTESIAN_POINT ( 'NONE',  ( -1.364683531250000748, -0.7406249996585803075, 0.000000000000000000 ) ) ;
#43561 = CARTESIAN_POINT ( 'NONE',  ( 6.029551324705815674, -0.2728526602329122142, 2.204496564233568989 ) ) ;
#43562 = CARTESIAN_POINT ( 'NONE',  ( 4.228923158279327410, -1.829750178516520442, -0.7082015076659911035 ) ) ;
#43564 = CARTESIAN_POINT ( 'NONE',  ( -6.453317930424837812, 7.591587675992828466, 1.082531754730549967 ) ) ;
#43563 = CARTESIAN_POINT ( 'NONE',  ( 8.595506201383999567, 12.97191496834930113, 0.7216878364870438212 ) ) ;
#43565 = CARTESIAN_POINT ( 'NONE',  ( -2.788906526875773208E-15, 9.218750000682799595, -1.499999999999998446 ) ) ;
#43566 = CARTESIAN_POINT ( 'NONE',  ( 5.677129043647218154, -0.04737763303009440846, -2.262073803551585272 ) ) ;
#43567 = CIRCLE ( 'NONE', #71181, 0.08000000000000020983 ) ;
#43568 = CARTESIAN_POINT ( 'NONE',  ( 2.488800817111187946, 2.000174138640842258, 0.5034198422354563274 ) ) ;
#43569 = CARTESIAN_POINT ( 'NONE',  ( -6.905180308061733996, 6.950465202360470052, 0.7998128361456341429 ) ) ;
#43570 = AXIS2_PLACEMENT_3D ( 'NONE', #135747, #83773, #166100 ) ;
#43571 = CARTESIAN_POINT ( 'NONE',  ( 1.499999999999989120, 3.056250000682818158, 1.214306433183764966E-14 ) ) ;
#43572 = CARTESIAN_POINT ( 'NONE',  ( 3.672993792711932048, 0.04889617625786558258, -1.870083761627352015 ) ) ;
#43573 = CARTESIAN_POINT ( 'NONE',  ( 2.373305363469370377, -0.2979590584733567971, -1.708161578628903055 ) ) ;
#43574 = EDGE_CURVE ( 'NONE', #14256, #18033, #34961, .T. ) ;
#43575 = CARTESIAN_POINT ( 'NONE',  ( 6.339412547452306868, 0.8406370108028878851, -2.024118718474729128 ) ) ;
#43576 = CARTESIAN_POINT ( 'NONE',  ( 1.272829778695073299, -1.399090282553701270, 1.706552004499435560 ) ) ;
#43577 = CARTESIAN_POINT ( 'NONE',  ( 6.122988667457554435, -1.827782563270570648, 0.6563872640158885385 ) ) ;
#43579 = ORIENTED_EDGE ( 'NONE', *, *, #54015, .T. ) ;
#43578 = CARTESIAN_POINT ( 'NONE',  ( 8.266504136565099969, 15.18065358759336547, 8.700162761727884941 ) ) ;
#43580 =( NAMED_UNIT ( * ) SI_UNIT ( $, .STERADIAN. ) SOLID_ANGLE_UNIT ( ) );
#43581 = ADVANCED_FACE ( 'NONE', ( #128680 ), #79326, .T. ) ;
#43582 = CARTESIAN_POINT ( 'NONE',  ( 0.07093568767341934533, -0.9480374005119349690, 1.779628194860154222 ) ) ;
#43583 = CARTESIAN_POINT ( 'NONE',  ( -0.01710467543277957581, -1.380256469788909035, 1.610041658517608054 ) ) ;
#43584 = CARTESIAN_POINT ( 'NONE',  ( 0.6801582343749970061, 2.223958333674731946, 1.178068619123799898 ) ) ;
#43585 = CARTESIAN_POINT ( 'NONE',  ( -8.992082194361570302, 11.51384853155376220, 1.599625672291269396 ) ) ;
#43586 = CARTESIAN_POINT ( 'NONE',  ( 7.657657833620182153, 7.828355648845348291, -0.7998128361456281477 ) ) ;
#43587 = FACE_OUTER_BOUND ( 'NONE', #126789, .T. ) ;
#43588 = CARTESIAN_POINT ( 'NONE',  ( 3.598116246361187542, -1.823677485248562435, -0.08826725125678223927 ) ) ;
#43589 = CARTESIAN_POINT ( 'NONE',  ( 2.503190323335769740, 1.772782541628318720, -1.313999973512294472 ) ) ;
#43590 = VERTEX_POINT ( 'NONE', #114540 ) ;
#43591 = CARTESIAN_POINT ( 'NONE',  ( -4.787437638956939523, 5.718337012605431369, -1.082531754730549967 ) ) ;
#43592 = CARTESIAN_POINT ( 'NONE',  ( -3.285556943750000070, -2.996874999522041616, 0.000000000000000000 ) ) ;
#43593 = CARTESIAN_POINT ( 'NONE',  ( -9.006694118179950692, 9.402231314165087284, 1.040834085586084257E-14 ) ) ;
#43594 = CARTESIAN_POINT ( 'NONE',  ( 1.037374617392500031, -0.04523278242563041895, 2.019440925237799167 ) ) ;
#43595 = CARTESIAN_POINT ( 'NONE',  ( 0.8914570141239013257, -0.05588796005432519753, -2.119924415460701983 ) ) ;
#43596 = CARTESIAN_POINT ( 'NONE',  ( -5.152980901645737077, 8.169505597632108262, -1.199719254218453823 ) ) ;
#43597 = CARTESIAN_POINT ( 'NONE',  ( 3.151044791815108770, 1.598572158793242659, -0.9524303787414812872 ) ) ;
#43598 = CARTESIAN_POINT ( 'NONE',  ( 2.530568227245037605, 6.104080031761181857, 0.000000000000000000 ) ) ;
#43599 = CARTESIAN_POINT ( 'NONE',  ( 6.293592298849588929, 1.492257802130890543, -1.356297202127904722 ) ) ;
#43600 = ORIENTED_EDGE ( 'NONE', *, *, #5319, .F. ) ;
#43601 = ORIENTED_EDGE ( 'NONE', *, *, #72745, .F. ) ;
#43602 = CARTESIAN_POINT ( 'NONE',  ( -9.158696461231359720, 10.64389961198009615, 1.199719254218462483 ) ) ;
#43603 = CARTESIAN_POINT ( 'NONE',  ( 3.826616632296374831, 1.734130841282412128, 0.5711148077138239465 ) ) ;
#43604 = VECTOR ( 'NONE', #62529, 1000.000000000000000 ) ;
#43606 = CARTESIAN_POINT ( 'NONE',  ( -5.391520587109122076, 6.494678753518896563, -1.342800935913717852 ) ) ;
#43605 = CARTESIAN_POINT ( 'NONE',  ( -4.132202957115018727, 8.042930226601317401, 0.000000000000000000 ) ) ;
#43607 = CARTESIAN_POINT ( 'NONE',  ( 5.696489930276292135, 7.416392257432566026, -1.320530921439456273 ) ) ;
#43608 = CARTESIAN_POINT ( 'NONE',  ( 6.116564501996816894, 0.5879282371138266905, -1.928457050679150298 ) ) ;
#43609 = CARTESIAN_POINT ( 'NONE',  ( 6.087831982560696353, -1.832735460234231617, -0.1757473516527594259 ) ) ;
#43610 = CARTESIAN_POINT ( 'NONE',  ( 2.980618654443941473, 6.479024054206157679, 0.4184689722446261473 ) ) ;
#43611 = CARTESIAN_POINT ( 'NONE',  ( 4.459805605305016130, 0.5082999457236726526, -2.250878628046268037 ) ) ;
#43612 = CARTESIAN_POINT ( 'NONE',  ( 4.667750024854814050, 8.667735138964429709, -0.7998128361456381397 ) ) ;
#43613 = CARTESIAN_POINT ( 'NONE',  ( 6.889893180375397996, -0.9309023296741396614, 1.948985471107896439 ) ) ;
#43614 = CARTESIAN_POINT ( 'NONE',  ( 6.012151052656117933, 9.101594430485762999, 1.199719254218460707 ) ) ;
#43615 = CARTESIAN_POINT ( 'NONE',  ( 2.384236373620087335, -0.3343274798127248149, -1.912924682550071864 ) ) ;
#43616 = CARTESIAN_POINT ( 'NONE',  ( 6.204520426337317929, -1.658329656736241553, -1.591615412813138564 ) ) ;
#43617 = DIRECTION ( 'NONE',  ( -0.9962287396576089415, 0.08676576675286083729, 0.000000000000000000 ) ) ;
#43618 = CARTESIAN_POINT ( 'NONE',  ( -7.910256278930404505, 8.193330178365746619, -0.7998128361456362523 ) ) ;
#43620 = EDGE_CURVE ( 'NONE', #147186, #119686, #96675, .T. ) ;
#43619 = VECTOR ( 'NONE', #15202, 1000.000000000000114 ) ;
#43621 = CARTESIAN_POINT ( 'NONE',  ( 4.100366707588389836, -0.5864361863821172527, -1.776433678864146382 ) ) ;
#43622 = ORIENTED_EDGE ( 'NONE', *, *, #3938, .F. ) ;
#43625 = CARTESIAN_POINT ( 'NONE',  ( -6.134138155540168391, 6.121192367743780949, 0.000000000000000000 ) ) ;
#43624 = CARTESIAN_POINT ( 'NONE',  ( 1.499999999999989120, 1.785416667349487563, 0.8660254037844524744 ) ) ;
#43623 = CARTESIAN_POINT ( 'NONE',  ( 2.619282413590624525, 1.617716081779559278, 1.019604094833974628 ) ) ;
#43626 = CARTESIAN_POINT ( 'NONE',  ( 4.196070124731249074, -0.8457972711899945928, 2.038567251995755836 ) ) ;
#43627 = CARTESIAN_POINT ( 'NONE',  ( -2.553934817853170728E-14, 1.000000000682808698, -1.414508159514595409 ) ) ;
#43628 = CARTESIAN_POINT ( 'NONE',  ( 6.883263157960382905, 3.691751545928231959, 2.560365603790202282 ) ) ;
#43629 = CARTESIAN_POINT ( 'NONE',  ( -0.2110808730066962846, 2.887681559854797797, -2.286017728802595350 ) ) ;
#43630 = CARTESIAN_POINT ( 'NONE',  ( 4.868786560638885597, 7.733982516503781213, 1.082531754730548412 ) ) ;
#43631 = CARTESIAN_POINT ( 'NONE',  ( -5.411112705185557203, 9.327065566109540740, 0.7216878364870267237 ) ) ;
#43632 = CARTESIAN_POINT ( 'NONE',  ( 2.038291622189229546, 1.949329857042367387, 0.2932346777646984148 ) ) ;
#43633 = CARTESIAN_POINT ( 'NONE',  ( 2.784532256742262568, -1.187036312555936890, 1.978742884264461654 ) ) ;
#43634 = CARTESIAN_POINT ( 'NONE',  ( 2.172246964874047670, -0.9220853831424129510, -1.731647142839589648 ) ) ;
#43635 = CARTESIAN_POINT ( 'NONE',  ( -1.420000000000021911, 6.120000000000041851, 2.580000000000011173 ) ) ;
#43636 = CARTESIAN_POINT ( 'NONE',  ( 6.684441936803141360, 1.192331456891123187, -1.682829884528406428 ) ) ;
#43637 = CARTESIAN_POINT ( 'NONE',  ( 2.873965376416980355, 6.296784005887697155, -0.7216878364870267237 ) ) ;
#43638 = CARTESIAN_POINT ( 'NONE',  ( 3.960172920142067898, -1.157100329752266621, 1.651342637023434090 ) ) ;
#43639 = CARTESIAN_POINT ( 'NONE',  ( 3.528865121306874464, 7.339036084825155015, -0.7998128361456362523 ) ) ;
#43640 = ORIENTED_EDGE ( 'NONE', *, *, #6091, .F. ) ;
#43641 = CARTESIAN_POINT ( 'NONE',  ( 4.311732611912100666, -1.244383703160652610, -1.586670621409623116 ) ) ;
#43642 = CARTESIAN_POINT ( 'NONE',  ( 0.7500000000000006661, 10.16666666666667140, -1.299038105676657340 ) ) ;
#43643 = CYLINDRICAL_SURFACE ( 'NONE', #137595, 0.07999999999999972411 ) ;
#43644 = CARTESIAN_POINT ( 'NONE',  ( -10.48266952940149466, 5.268049057482275366, -5.154014898524191146 ) ) ;
#43645 = CARTESIAN_POINT ( 'NONE',  ( 9.154780037725547714, 11.70366268214508487, 1.599625672291279388 ) ) ;
#43646 = CARTESIAN_POINT ( 'NONE',  ( 2.342849523213458962, -2.128499089237919417, -0.4270345827348878132 ) ) ;
#43647 = CARTESIAN_POINT ( 'NONE',  ( 4.179656494762836516, 8.098292687190454586, -0.7998128361456361413 ) ) ;
#43648 = CARTESIAN_POINT ( 'NONE',  ( 5.375201043168952530, 6.430740811364754173, 1.235622880962461201 ) ) ;
#43649 = CARTESIAN_POINT ( 'NONE',  ( 2.917106759524803472, -0.1871779394605546654, 1.861177454839262113 ) ) ;
#43650 = CARTESIAN_POINT ( 'NONE',  ( 6.151685507011436904, 0.6340151041426717038, -2.066508600247290328 ) ) ;
#43652 = CARTESIAN_POINT ( 'NONE',  ( 6.827182134110246103, 6.039869998172250121, 2.305852349323509021 ) ) ;
#43651 = CARTESIAN_POINT ( 'NONE',  ( -0.02244404828157658613, 0.6916080914694566761, -2.270927585766496559 ) ) ;
#43653 = CARTESIAN_POINT ( 'NONE',  ( 0.6823417656249882723, 0.1760416670080894308, -1.181850606188749264 ) ) ;
#43654 = FILL_AREA_STYLE_COLOUR ( '', #73011 ) ;
#43655 = CARTESIAN_POINT ( 'NONE',  ( 2.895058368816882499, -0.1428820475998151540, -1.907012587803847303 ) ) ;
#43656 = CARTESIAN_POINT ( 'NONE',  ( 3.608038473134207891, -0.7167157551234564217, -1.618410677222481553 ) ) ;
#43657 = CARTESIAN_POINT ( 'NONE',  ( 2.104032245951466429, -0.8162354410432022256, 1.729450509904674416 ) ) ;
#43658 = CARTESIAN_POINT ( 'NONE',  ( -3.906720819032141190, 7.709591388846142479, -0.7998128361456281477 ) ) ;
#43660 = CARTESIAN_POINT ( 'NONE',  ( 0.1631139290103194861, 1.786460926609586330, -0.6921882798058466291 ) ) ;
#43659 = LINE ( 'NONE', #194143, #56174 ) ;
#43661 = CARTESIAN_POINT ( 'NONE',  ( -1.500000000000015099, -0.6208333333333116988, -0.8660254037844383745 ) ) ;
#43662 = CARTESIAN_POINT ( 'NONE',  ( 0.8716356842100521085, -0.3054578492302991721, 2.047597563663336118 ) ) ;
#43663 = CARTESIAN_POINT ( 'NONE',  ( -0.6823417656250246877, -0.6364583329919113464, 1.181850606188755259 ) ) ;
#43664 = CARTESIAN_POINT ( 'NONE',  ( 6.403191318657627029, 1.556466930477506505, 1.037356966126230517 ) ) ;
#43665 = CARTESIAN_POINT ( 'NONE',  ( 1.260069262837599791, 0.7379878962356714034, 1.670071910705408946 ) ) ;
#43667 = CARTESIAN_POINT ( 'NONE',  ( 5.028717893731355026, 7.888467461587344687, 1.094519599958807765 ) ) ;
#43666 = CARTESIAN_POINT ( 'NONE',  ( 5.637410271038987730, -1.996576301129053377, 0.9405272304151901519 ) ) ;
#43668 = CARTESIAN_POINT ( 'NONE',  ( -1.402160292154681736E-14, -0.6781249996585819728, 1.575800808251672791 ) ) ;
#43669 = CARTESIAN_POINT ( 'NONE',  ( 2.998538507119326901, 2.046783137066817027, 0.2552134970664684532 ) ) ;
#43670 = CARTESIAN_POINT ( 'NONE',  ( -7.660520486921249983, 8.896027641951645748, -1.199719254218446718 ) ) ;
#43671 = CARTESIAN_POINT ( 'NONE',  ( 6.889999999999985469, 0.6064005686075202295, 1.774654002403662778 ) ) ;
#43672 = CARTESIAN_POINT ( 'NONE',  ( 8.565000355531088516, 11.01558638625153286, -1.599625672291257406 ) ) ;
#43673 = CARTESIAN_POINT ( 'NONE',  ( 1.425126390603690174, 3.965403223221183548, -0.4909503797921681012 ) ) ;
#43674 = CARTESIAN_POINT ( 'NONE',  ( -0.009341426467593692828, -9.943661027227911120, -10.91969313363969007 ) ) ;
#43675 = CARTESIAN_POINT ( 'NONE',  ( 6.638652492546827766, 7.774124658506663010, 1.199719254218452047 ) ) ;
#43676 = ORIENTED_EDGE ( 'NONE', *, *, #205115, .T. ) ;
#43677 = CARTESIAN_POINT ( 'NONE',  ( 5.178213324540339002, -1.104578422852561914, -1.750899486206449751 ) ) ;
#43678 = CARTESIAN_POINT ( 'NONE',  ( -1.364683531250014514, -0.1989583329919157317, -0.7879004041258359514 ) ) ;
#43679 = CARTESIAN_POINT ( 'NONE',  ( 3.075615952314793233, 2.053625483174918553, -0.6748976972978243394 ) ) ;
#43680 = CARTESIAN_POINT ( 'NONE',  ( -4.907053429147543611, 8.030730943182621928, 0.9696864716568325271 ) ) ;
#43681 = CARTESIAN_POINT ( 'NONE',  ( 2.596358364526121676, -1.036244631391324722, 1.733413072464027316 ) ) ;
#43682 = CARTESIAN_POINT ( 'NONE',  ( 7.552496594302675170, -5.254973434576991842, 7.962224162659105708 ) ) ;
#43683 = PRODUCT_DEFINITION_SHAPE ( 'NONE', 'NONE',  #214413 ) ;
#43685 = CARTESIAN_POINT ( 'NONE',  ( 6.127922243696800386, 10.09306701771420656, -0.7216878364870267237 ) ) ;
#43684 = CARTESIAN_POINT ( 'NONE',  ( -3.474999999999998312, -0.6708333333333343917, 2.006292185433951047 ) ) ;
#43686 = EDGE_CURVE ( 'NONE', #76056, #6089, #165344, .T. ) ;
#43687 = CARTESIAN_POINT ( 'NONE',  ( -6.903036488013351679, 8.082572653217566128, -1.199719254218452047 ) ) ;
#43688 = CARTESIAN_POINT ( 'NONE',  ( 0.9718890779336667451, -0.9023411006064323558, 1.803417998987096427 ) ) ;
#43690 = CARTESIAN_POINT ( 'NONE',  ( 5.548420995840112724, -1.728225626343689925, 1.347513067664840358 ) ) ;
#43689 = CARTESIAN_POINT ( 'NONE',  ( -4.283486466913726254, 7.084819080452935403, -1.199719254218452047 ) ) ;
#43691 = CARTESIAN_POINT ( 'NONE',  ( -1.001543065824772872E-14, 4.993750000682814161, 1.732050807568877637 ) ) ;
#43692 = CARTESIAN_POINT ( 'NONE',  ( 4.728717205193702533, 1.314622909153417174, -1.389140896021365368 ) ) ;
#43693 = CARTESIAN_POINT ( 'NONE',  ( -3.938278094839060994, 7.324765956376747766, 0.6593293099422595782 ) ) ;
#43694 = CARTESIAN_POINT ( 'NONE',  ( 4.433153041544209749, 7.155467067568137551, -1.082531754730548412 ) ) ;
#43696 = CARTESIAN_POINT ( 'NONE',  ( 3.673453983005552814, 1.462458373076291673, 1.388474078538141754 ) ) ;
#43695 = CARTESIAN_POINT ( 'NONE',  ( -9.286972035236630063, 10.89751746493999107, -1.082531754730537976 ) ) ;
#43697 = CARTESIAN_POINT ( 'NONE',  ( -1.364683531250000748, 13.92187500034140157, 0.000000000000000000 ) ) ;
#43698 = CARTESIAN_POINT ( 'NONE',  ( 5.350533963330765808, 0.5041449683875122156, 1.649457517733200040 ) ) ;
#43699 = CARTESIAN_POINT ( 'NONE',  ( 7.198453214212898743, 7.362893269528701268, 0.7998128361456291469 ) ) ;
#43700 = CARTESIAN_POINT ( 'NONE',  ( 10.24960094225127172, 11.06021530882240356, -0.7216878364870257245 ) ) ;
#43701 = CARTESIAN_POINT ( 'NONE',  ( -6.713552092916992287, -7.189371949512880278, -6.722000117220233051 ) ) ;
#43702 = CARTESIAN_POINT ( 'NONE',  ( 4.762891570102392613, -1.670096840553733752, -0.8426394062573672183 ) ) ;
#43703 = DIRECTION ( 'NONE',  ( 0.000000000000000000, 0.000000000000000000, 1.000000000000000000 ) ) ;
#43704 = CARTESIAN_POINT ( 'NONE',  ( 1.411079811451225074, -1.634442866182721277, 1.270590680402396311 ) ) ;
#43705 = CYLINDRICAL_SURFACE ( 'NONE', #18825, 3.150000000000000799 ) ;
#43706 = VERTEX_POINT ( 'NONE', #28960 ) ;
#43707 = CARTESIAN_POINT ( 'NONE',  ( 6.633470331352866900, -0.1302952867699505302, 1.781688180685939926 ) ) ;
#43708 = CARTESIAN_POINT ( 'NONE',  ( 5.065906673361608270, 5.939254536123854677, -1.199719254218450271 ) ) ;
#43709 = FILL_AREA_STYLE_COLOUR ( '', #129172 ) ;
#43710 = CARTESIAN_POINT ( 'NONE',  ( 0.6678513782990652681, 1.809512280066556400, -0.08962025572057349954 ) ) ;
#43711 = CARTESIAN_POINT ( 'NONE',  ( 5.573810548549551491, 6.635772073796838200, -1.082531754730548412 ) ) ;
#43712 = CARTESIAN_POINT ( 'NONE',  ( 11.81254310278123754, 7.953092247000543402, -2.153480349962514140 ) ) ;
#43713 = ORIENTED_EDGE ( 'NONE', *, *, #83547, .T. ) ;
#43714 = ADVANCED_FACE ( 'NONE', ( #95045 ), #161095, .F. ) ;
#43715 = CARTESIAN_POINT ( 'NONE',  ( 9.856414487010592751, 10.60149777770828194, 0.7216878364870438212 ) ) ;
#43716 = CIRCLE ( 'NONE', #164751, 0.5000000000000016653 ) ;
#43718 = CARTESIAN_POINT ( 'NONE',  ( 6.889514614038635187, 11.18951748302043114, -0.7998128361456291469 ) ) ;
#43717 = CARTESIAN_POINT ( 'NONE',  ( 1.135121963537696566, -0.04462593873827064989, -1.961518378280776354 ) ) ;
#43719 = CARTESIAN_POINT ( 'NONE',  ( 5.062082326478217098, -1.060395474731326448, 1.595121111449711693 ) ) ;
#43720 = CARTESIAN_POINT ( 'NONE',  ( -11.49978884755372732, 13.74270821162817668, 3.429452816445256236 ) ) ;
#43721 = CARTESIAN_POINT ( 'NONE',  ( -5.631831469557842418, 7.372220891417233801, 1.235678285582973546 ) ) ;
#43723 = EDGE_LOOP ( 'NONE', ( #214133, #57195, #6772 ) ) ;
#43722 = CARTESIAN_POINT ( 'NONE',  ( 4.663641653420880218, 8.384739662392275861, -0.7216878364870207285 ) ) ;
#43724 = CARTESIAN_POINT ( 'NONE',  ( -8.758204044748012507, 11.24099069033793974, 1.443375672974064550 ) ) ;
#43725 = CARTESIAN_POINT ( 'NONE',  ( 1.463986924769441478, 2.129665692569195024, -0.3698555562515608020 ) ) ;
#43726 = CARTESIAN_POINT ( 'NONE',  ( -3.284818356260900796, 7.054314858938165678, 0.7998128361456352531 ) ) ;
#43727 = CARTESIAN_POINT ( 'NONE',  ( 7.241463443474815520, 8.581367117876336437, -1.082531754730548412 ) ) ;
#43728 = CARTESIAN_POINT ( 'NONE',  ( -2.266184231778562541, 5.795632037050281404, 1.040834085586084257E-14 ) ) ;
#43729 = CARTESIAN_POINT ( 'NONE',  ( 4.946237996787820279, 1.820793779319082706, 0.1331645236858983172 ) ) ;
#43730 = EDGE_CURVE ( 'NONE', #40788, #168810, #60670, .T. ) ;
#43732 = CARTESIAN_POINT ( 'NONE',  ( 8.384452190322788212, 12.99440559435832476, -8.518166066213405330 ) ) ;
#43731 =( BOUNDED_SURFACE ( )  B_SPLINE_SURFACE ( 3, 3, ( 
 ( #3106, #203444, #204513, #202379, #20441, #85453, #6318, #21488, #86523, #187217, #152588 ),
 ( #136359, #4175, #151538, #36695, #103851, #123393, #70244, #35627, #55098, #186142, #137425 ),
 ( #23646, #101705, #71313, #169899, #73467, #167777, #39923, #106031, #87598, #139568, #5237 ),
 ( #121247, #38846, #205595, #69177, #104929, #170971, #22570, #72392, #135297, #138492, #52951 ),
 ( #122325, #140652, #92954, #75615, #95085, #59357, #58297, #77739, #62550, #108182, #193620 ),
 ( #161133, #190412, #43144, #175265, #124453, #76670, #208791, #125514, #210924, #191476, #61491 ),
 ( #45261, #42068, #159001, #60421, #143860, #12721, #78794, #207734, #111381, #27928, #177384 ) ),
 .UNSPECIFIED., .T., .F., .T. ) 
 B_SPLINE_SURFACE_WITH_KNOTS ( ( 4, 3, 4 ),
 ( 4, 1, 1, 1, 1, 1, 1, 1, 4 ),
 ( 0.000000000000000000, 0.5000000000000000000, 1.000000000000000000 ),
 ( 0.000000000000000000, 0.2255509035172358623, 0.3975895543896152406, 0.5252637114030099807, 0.6177357421269481508, 0.6841390318922365710, 0.7334310489036851566, 0.7741974304450970346, 1.000000000000000000 ),
 .UNSPECIFIED. ) 
 GEOMETRIC_REPRESENTATION_ITEM ( )  RATIONAL_B_SPLINE_SURFACE ( (
 ( 1.000000000000000000, 1.000000000000000000, 1.000000000000000000, 1.000000000000000000, 1.000000000000000444, 0.9999999999999997780, 1.000000000000000000, 1.000000000000000000, 1.000000000000000000, 1.000000000000000000, 1.000000000000000000),
 ( 0.3333333333333333703, 0.3333333333333333703, 0.3333333333333332593, 0.3333333333333334814, 0.3333333333333334814, 0.3333333333333333148, 0.3333333333333333703, 0.3333333333333333703, 0.3333333333333333703, 0.3333333333333334259, 0.3333333333333333703),
 ( 0.3333333333333333703, 0.3333333333333333703, 0.3333333333333332593, 0.3333333333333334814, 0.3333333333333334814, 0.3333333333333333148, 0.3333333333333333703, 0.3333333333333333703, 0.3333333333333333703, 0.3333333333333334259, 0.3333333333333333703),
 ( 1.000000000000000000, 1.000000000000000000, 1.000000000000000000, 1.000000000000000000, 1.000000000000000444, 0.9999999999999997780, 1.000000000000000000, 1.000000000000000000, 1.000000000000000000, 1.000000000000000000, 1.000000000000000000),
 ( 0.3333333333333333703, 0.3333333333333333703, 0.3333333333333332593, 0.3333333333333334814, 0.3333333333333334814, 0.3333333333333333148, 0.3333333333333333703, 0.3333333333333333703, 0.3333333333333333703, 0.3333333333333334259, 0.3333333333333333703),
 ( 0.3333333333333333703, 0.3333333333333333703, 0.3333333333333332593, 0.3333333333333334814, 0.3333333333333334814, 0.3333333333333333148, 0.3333333333333333703, 0.3333333333333333703, 0.3333333333333333703, 0.3333333333333334259, 0.3333333333333333703),
 ( 1.000000000000000000, 1.000000000000000000, 1.000000000000000000, 1.000000000000000000, 1.000000000000000444, 0.9999999999999997780, 1.000000000000000000, 1.000000000000000000, 1.000000000000000000, 1.000000000000000000, 1.000000000000000000) ) ) 
 REPRESENTATION_ITEM ( '' )  SURFACE ( )  );
#43733 = CARTESIAN_POINT ( 'NONE',  ( 1.300003668391478406, -1.971530339922975550, -0.004173579811568225127 ) ) ;
#43734 = CARTESIAN_POINT ( 'NONE',  ( 3.269685606991072468, 0.4601866041431811327, -1.856093204100267124 ) ) ;
#43735 = ORIENTED_EDGE ( 'NONE', *, *, #36106, .T. ) ;
#43736 =( REPRESENTATION_RELATIONSHIP ('NONE','NONE', #84563, #47273 ) REPRESENTATION_RELATIONSHIP_WITH_TRANSFORMATION ( #55791 )SHAPE_REPRESENTATION_RELATIONSHIP( ) );
#43737 = DIRECTION ( 'NONE',  ( 0.6507913734559641616, -0.7592566023653004592, 0.000000000000000000 ) ) ;
#43738 = CARTESIAN_POINT ( 'NONE',  ( 4.281674416708352027, -1.885371899234816739, 0.5696992939150746782 ) ) ;
#43739 = ORIENTED_EDGE ( 'NONE', *, *, #143009, .T. ) ;
#43740 = CARTESIAN_POINT ( 'NONE',  ( 6.040568865451770186, -1.638250791085652303, 1.042688759833640066 ) ) ;
#43741 = ORIENTED_EDGE ( 'NONE', *, *, #43463, .T. ) ;
#43742 = CARTESIAN_POINT ( 'NONE',  ( -5.478376588373717659, 8.549133898814758936, -1.199719254218452047 ) ) ;
#43744 = CARTESIAN_POINT ( 'NONE',  ( 7.015831072854086692, -6.604036961759984337, -6.576431128233156009 ) ) ;
#43743 = CARTESIAN_POINT ( 'NONE',  ( -4.664887371553763096, 7.600063145858131364, -1.199719254218453823 ) ) ;
#43745 = CARTESIAN_POINT ( 'NONE',  ( 6.821160681006781523, 9.051383109298340557, 1.443375672974063439 ) ) ;
#43746 = CARTESIAN_POINT ( 'NONE',  ( 3.844317892072905973, 1.020479721125296280, -1.617037373464407457 ) ) ;
#43747 = DIRECTION ( 'NONE',  ( 0.000000000000000000, -1.000000000000000000, 0.000000000000000000 ) ) ;
#43748 = DIRECTION ( 'NONE',  ( 0.000000000000000000, 0.000000000000000000, 1.000000000000000000 ) ) ;
#43749 = CARTESIAN_POINT ( 'NONE',  ( 9.518502046417362195, 4.418053365869059057, -7.307953274077121364 ) ) ;
#43750 = CARTESIAN_POINT ( 'NONE',  ( 5.408844923620411471, -0.4912159631041897456, -1.952115566551455572 ) ) ;
#43752 = CARTESIAN_POINT ( 'NONE',  ( 5.770720322323381168, -0.3006437417610394736, -1.993894057904864514 ) ) ;
#43751 = CARTESIAN_POINT ( 'NONE',  ( 6.463509179248937642, 0.3066564278407272748, -1.799597105106438777 ) ) ;
#43753 = CARTESIAN_POINT ( 'NONE',  ( 6.727182134110193168, 4.701113012587437190, 2.373661997258198486 ) ) ;
#43754 = CARTESIAN_POINT ( 'NONE',  ( 1.416557266959647787, 0.8372786474034592530, 1.893679232998768391 ) ) ;
#43755 = CARTESIAN_POINT ( 'NONE',  ( -8.527715433315703919, 9.051348881730875817, 1.040834085586084257E-14 ) ) ;
#43756 = CIRCLE ( 'NONE', #78355, 11.95586206896534698 ) ;
#43757 = CARTESIAN_POINT ( 'NONE',  ( -6.320392545075788959, 6.875563024200552320, -0.7000339101758262794 ) ) ;
#43758 = LINE ( 'NONE', #191028, #164151 ) ;
#43759 = CARTESIAN_POINT ( 'NONE',  ( 6.315307248462690204, -0.2269180964024133385, 1.856785020699961875 ) ) ;
#43760 = CARTESIAN_POINT ( 'NONE',  ( 4.801558957534076022, 8.753569217098425170, 0.7998128361456462443 ) ) ;
#43761 = CARTESIAN_POINT ( 'NONE',  ( 5.722950238744209273, 6.809768379023969587, 1.082531754730549967 ) ) ;
#43762 = VECTOR ( 'NONE', #160000, 1000.000000000000000 ) ;
#43763 = FACE_OUTER_BOUND ( 'NONE', #138436, .T. ) ;
#43764 = CARTESIAN_POINT ( 'NONE',  ( -1.364683531250000748, 11.42187500034139802, 0.000000000000000000 ) ) ;
#43765 = CARTESIAN_POINT ( 'NONE',  ( -3.815730167242251003, 6.539103397502874948, -1.199719254218452047 ) ) ;
#43767 = CARTESIAN_POINT ( 'NONE',  ( -5.582925393777276035, 9.735439736040634173, 0.7998128361456291469 ) ) ;
#43766 = CARTESIAN_POINT ( 'NONE',  ( 6.956180625286545904, -6.372104534814153176, -6.956180625285512065 ) ) ;
#43768 = CARTESIAN_POINT ( 'NONE',  ( 4.060950141605116137, -0.9941625748171744048, 1.420652921118512602 ) ) ;
#43769 = CARTESIAN_POINT ( 'NONE',  ( -5.739179097286464248, 5.590130456455974617, -0.7998128361456221525 ) ) ;
#43770 = CARTESIAN_POINT ( 'NONE',  ( 2.131770371054972912, 1.982354287819853456, -0.5969549857752221023 ) ) ;
#43771 = CARTESIAN_POINT ( 'NONE',  ( 3.726253221435165575, 2.107214626963071602, 0.2054869192316331195 ) ) ;
#43772 = CARTESIAN_POINT ( 'NONE',  ( 7.670162217029129259, 9.971608557999250166, 1.599625672291281386 ) ) ;
#43773 = CARTESIAN_POINT ( 'NONE',  ( 0.09411116651286953461, -9.919020924439822195, 10.99959762541857877 ) ) ;
#43774 = CARTESIAN_POINT ( 'NONE',  ( 0.6726246190636753219, 1.362232206854155914, -1.422558973980556418 ) ) ;
#43775 = CARTESIAN_POINT ( 'NONE',  ( 5.624517712206933417, 6.335738387217328516, 1.153896037602806013 ) ) ;
#43776 = CARTESIAN_POINT ( 'NONE',  ( 3.958617665510264949, 5.641473247893851628, -1.443375672974051449 ) ) ;
#43778 = CARTESIAN_POINT ( 'NONE',  ( 0.1406777020166137260, 1.830675540527426648, 0.5531436448603862521 ) ) ;
#43777 = CARTESIAN_POINT ( 'NONE',  ( -3.475000000000000533, -1.079166666666665941, -2.006292185433948827 ) ) ;
#43779 = CARTESIAN_POINT ( 'NONE',  ( 4.013863964491473979, -1.177108192605724746, -1.966824220290509961 ) ) ;
#43780 = CARTESIAN_POINT ( 'NONE',  ( 0.7854531640391904102, 1.224056292049885419, 1.354719642434290439 ) ) ;
#43781 = CARTESIAN_POINT ( 'NONE',  ( 2.830216799141628492, -0.9462872844297947061, -1.661813493071498726 ) ) ;
#43782 = AXIS2_PLACEMENT_3D ( 'NONE', #138653, #55258, #24871 ) ;
#43783 = CARTESIAN_POINT ( 'NONE',  ( 5.017399365509065845, 8.011327138806002779, -1.199719254218450271 ) ) ;
#43784 = CARTESIAN_POINT ( 'NONE',  ( 6.358410854684775515, 8.441231968597481483, -1.443375672974058777 ) ) ;
#43785 = CARTESIAN_POINT ( 'NONE',  ( -8.188234707649510113, 11.64035869464474082, -1.199719254218446718 ) ) ;
#43786 = EDGE_CURVE ( 'NONE', #63320, #107948, #187262, .T. ) ;
#43787 = CARTESIAN_POINT ( 'NONE',  ( 1.529542846128278066, -0.2424046428922912721, 1.998471667700427057 ) ) ;
#43788 = CARTESIAN_POINT ( 'NONE',  ( 2.061309051315598051, 1.628117514333087934, 1.094105149622534467 ) ) ;
#43789 = CARTESIAN_POINT ( 'NONE',  ( -7.808606406466886973, 11.19745900993164511, 1.199719254218453823 ) ) ;
#43790 = CARTESIAN_POINT ( 'NONE',  ( -6.470265622219711688, 8.571729197388226140, -1.599625672291263179 ) ) ;
#43791 = DIRECTION ( 'NONE',  ( -0.000000000000000000, -1.000000000000000000, -0.000000000000000000 ) ) ;
#43793 = CARTESIAN_POINT ( 'NONE',  ( 3.221328931188462086, -1.705978018192667811, 0.4708956190180821344 ) ) ;
#43792 = CARTESIAN_POINT ( 'NONE',  ( 5.191392108680514816, -0.7531529969884572795, 1.950447244483977993 ) ) ;
#43794 = CARTESIAN_POINT ( 'NONE',  ( -0.6125000000000089262, 0.02083333401611819902, -1.060881119635969094 ) ) ;
#43795 = CARTESIAN_POINT ( 'NONE',  ( 5.999983301813878178, -0.8195729662384824143, -2.140910441102741313 ) ) ;
#43796 = CARTESIAN_POINT ( 'NONE',  ( 5.191228607790203675, -0.6215644750859107281, 1.625735776773645780 ) ) ;
#43797 = CARTESIAN_POINT ( 'NONE',  ( 6.414979237560321401, 10.63589287712906462, 1.040834085586084257E-14 ) ) ;
#43798 = SURFACE_SIDE_STYLE ('',( #147684 ) ) ;
#43799 = CARTESIAN_POINT ( 'NONE',  ( 6.011065113327825671, 1.732079373560748481, 0.08140909068810914251 ) ) ;
#43800 = CARTESIAN_POINT ( 'NONE',  ( 6.145025799957537060, -0.3124719705198654718, -2.148460482323500731 ) ) ;
#43801 = LINE ( 'NONE', #173802, #99959 ) ;
#43802 = CARTESIAN_POINT ( 'NONE',  ( 0.02287343425391458532, 0.3688939426326736104, 2.084831875159770753 ) ) ;
#43803 = CARTESIAN_POINT ( 'NONE',  ( 4.750000000000003553, 2.703060497845378561E-13, 2.052068128417943171 ) ) ;
#43804 = FACE_OUTER_BOUND ( 'NONE', #152053, .T. ) ;
#43805 = CARTESIAN_POINT ( 'NONE',  ( 3.680616551068579767, -1.856277683350136432, -0.5147254836462693550 ) ) ;
#43806 = CARTESIAN_POINT ( 'NONE',  ( -0.7500000000000179856, 11.07291666734946212, 1.299038105676658228 ) ) ;
#43807 = CARTESIAN_POINT ( 'NONE',  ( -0.1044638861024569515, -0.1585131741546479955, -2.186235582987208659 ) ) ;
#43808 = VERTEX_POINT ( 'NONE', #36402 ) ;
#43809 = CARTESIAN_POINT ( 'NONE',  ( 0.7499999999999902300, 4.816666666666684193, -1.299038105676658228 ) ) ;
#43810 = CARTESIAN_POINT ( 'NONE',  ( 4.299907273828439180, 8.168308919441841454, 1.040834085586084257E-14 ) ) ;
#43811 = CARTESIAN_POINT ( 'NONE',  ( 6.470265622219697477, 8.571729197388226140, -1.599625672291262513 ) ) ;
#43812 = CARTESIAN_POINT ( 'NONE',  ( 2.508681548337174494, -2.215532678404589007, -0.1606611847707327678 ) ) ;
#43813 = CARTESIAN_POINT ( 'NONE',  ( 4.363950690066983107, 4.004001632660354915, -0.1812806842866887536 ) ) ;
#43814 = CARTESIAN_POINT ( 'NONE',  ( 7.293923454472080792, 9.532663335016016148, 1.443375672974076540 ) ) ;
#43815 = CARTESIAN_POINT ( 'NONE',  ( -9.286972035236626510, 11.85788667924133399, -1.443375672974058777 ) ) ;
#43816 = CARTESIAN_POINT ( 'NONE',  ( 5.722950238744187956, 9.690876021928001904, 0.7216878364870317197 ) ) ;
#43817 = CARTESIAN_POINT ( 'NONE',  ( 1.055314813143366726, -1.277040974352643854, 1.560502084637045650 ) ) ;
#43819 = CARTESIAN_POINT ( 'NONE',  ( 5.547355216851989290, 1.820699215414087302, -0.9693467284541881224 ) ) ;
#43818 = CARTESIAN_POINT ( 'NONE',  ( 8.239604668803105270, 10.63595808506888396, -1.599625672291268286 ) ) ;
#43820 = CARTESIAN_POINT ( 'NONE',  ( -4.600294193738529103, 4.261431402316699035, -0.7998128361456221525 ) ) ;
#43821 = CARTESIAN_POINT ( 'NONE',  ( -1.364683531250012516, 1.530208333674756505, 0.7879004041258379498 ) ) ;
#43822 = CARTESIAN_POINT ( 'NONE',  ( 0.4558546072216109191, 0.6692488815305540628, 1.638537551351123112 ) ) ;
#43823 = CARTESIAN_POINT ( 'NONE',  ( 6.363864384548370445, -0.09514871459133207587, -1.731698918886691363 ) ) ;
#43824 = CARTESIAN_POINT ( 'NONE',  ( 5.882304624916216973, -0.2641129477329319242, -1.720170474299307806 ) ) ;
#43825 = EDGE_CURVE ( 'NONE', #192556, #13744, #200356, .T. ) ;
#43826 = CARTESIAN_POINT ( 'NONE',  ( 2.630776572171345418, 0.2838290345775448809, 2.274689434353324824 ) ) ;
#43827 = CARTESIAN_POINT ( 'NONE',  ( -1.402160292154681736E-14, -0.4281249996585808071, 1.575800808251672791 ) ) ;
#43828 = CARTESIAN_POINT ( 'NONE',  ( 1.745803608711377075, 0.5764907460206626366, 1.748616612666432868 ) ) ;
#43829 = CARTESIAN_POINT ( 'NONE',  ( 9.561524646135536543, 12.17819805862340310, -1.599625672291262513 ) ) ;
#43830 = SURFACE_STYLE_FILL_AREA ( #112084 ) ;
#43831 = CARTESIAN_POINT ( 'NONE',  ( 2.924607851032960504, 1.718362407962298333, 0.6167639819729958672 ) ) ;
#43832 = CARTESIAN_POINT ( 'NONE',  ( 3.270157880292836605, 1.821742160604752137, -0.8647241845514613834 ) ) ;
#43833 = CARTESIAN_POINT ( 'NONE',  ( -3.267151830768959098, 4.834763107362302748, -1.443375672974058777 ) ) ;
#43834 = FACE_OUTER_BOUND ( 'NONE', #120025, .T. ) ;
#43835 = CARTESIAN_POINT ( 'NONE',  ( 5.948290813881442318, 2.103388047956732620, 0.1067411848718266276 ) ) ;
#43836 = CARTESIAN_POINT ( 'NONE',  ( -5.605406444246153974, 8.627059054007450101, -1.199719254218440723 ) ) ;
#43837 = CARTESIAN_POINT ( 'NONE',  ( 7.320235437844907267, 14.95386332671184881, 9.102015036127445669 ) ) ;
#43838 = CARTESIAN_POINT ( 'NONE',  ( 2.945825538390862697, 1.462269270728074222, 1.465923284304726737 ) ) ;
#43839 = CARTESIAN_POINT ( 'NONE',  ( 4.650610384687404952, 5.384465856012134566, 1.199719254218462483 ) ) ;
#43840 = CARTESIAN_POINT ( 'NONE',  ( -1.360316468750019991, 0.4218750003414165062, -4.336808689942017736E-14 ) ) ;
#43841 = CARTESIAN_POINT ( 'NONE',  ( 4.969442291489525765, -1.791676405564743169, -1.133875526122554378 ) ) ;
#43843 = AXIS2_PLACEMENT_3D ( 'NONE', #129296, #195271, #146549 ) ;
#43842 = ITEM_DEFINED_TRANSFORMATION ( 'NONE', 'NONE', #138757,  #200407 ) ;
#43845 = ADVANCED_FACE ( 'NONE', ( #67807 ), #167531, .F. ) ;
#43844 = CARTESIAN_POINT ( 'NONE',  ( 1.348133503156129454, 1.924256495421622359, 0.09534579948072999245 ) ) ;
#43846 = ORIENTED_EDGE ( 'NONE', *, *, #194138, .F. ) ;
#43847 = CARTESIAN_POINT ( 'NONE',  ( -3.169574050544739841, 6.919863168935977527, -0.7998128361456481317 ) ) ;
#43848 = CARTESIAN_POINT ( 'NONE',  ( 9.596473800374404561, 10.09030761005864285, 0.000000000000000000 ) ) ;
#43849 = CARTESIAN_POINT ( 'NONE',  ( 4.692530563661249765, 8.488719734331187539, 0.000000000000000000 ) ) ;
#43850 = CARTESIAN_POINT ( 'NONE',  ( 0.8858701160440104472, 2.800000000000024247, -1.189311836856266735 ) ) ;
#43851 = CARTESIAN_POINT ( 'NONE',  ( -4.229253852459088137, 7.021547696922494808, 1.199719254218464037 ) ) ;
#43852 = CARTESIAN_POINT ( 'NONE',  ( 5.748313822965784858, 1.043546352714582071, -1.845953426139717246 ) ) ;
#43853 = CARTESIAN_POINT ( 'NONE',  ( 1.975741970143765736, 2.015461639870301358, -0.6107432106882881850 ) ) ;
#43854 = CARTESIAN_POINT ( 'NONE',  ( -4.145761110728687804, 8.058748072483927771, -0.7998128361456481317 ) ) ;
#43855 = CARTESIAN_POINT ( 'NONE',  ( 7.065770611016287006, 11.39514947949436774, 1.040834085586084257E-14 ) ) ;
#43856 = CARTESIAN_POINT ( 'NONE',  ( 5.981279135395962676, -0.04703572473597864706, 1.860536724379359574 ) ) ;
#43857 = CARTESIAN_POINT ( 'NONE',  ( 8.586391356156291010, 8.911878091804165791, 0.7998128361456481317 ) ) ;
#43858 = SURFACE_STYLE_USAGE ( .BOTH. , #190072 ) ;
#43859 = CARTESIAN_POINT ( 'NONE',  ( -3.461074353238556167, 7.259946855412102273, 0.000000000000000000 ) ) ;
#43860 = CARTESIAN_POINT ( 'NONE',  ( -3.195971524519394702, 4.751719416737803847, -1.599625672291262513 ) ) ;
#43861 = CARTESIAN_POINT ( 'NONE',  ( -1.844764736977754005, 2.494476015512113509, 2.491383360649019885 ) ) ;
#43863 = CARTESIAN_POINT ( 'NONE',  ( 2.506241959165692812, 1.961374882610424919, 0.05109738790698423877 ) ) ;
#43862 = CARTESIAN_POINT ( 'NONE',  ( 0.6124999999999793943, -0.3333333333333243775, -1.060881119635979530 ) ) ;
#43864 = CARTESIAN_POINT ( 'NONE',  ( 1.112450467520700537, -0.9725818059473789745, -1.930612204972524282 ) ) ;
#43866 = CARTESIAN_POINT ( 'NONE',  ( -5.937252720508472414, 6.122620518184580973, 0.7955437839095025332 ) ) ;
#43865 = CARTESIAN_POINT ( 'NONE',  ( -6.961185525973791144, 7.086080966583015339, 0.7998128361456341429 ) ) ;
#43867 = CARTESIAN_POINT ( 'NONE',  ( -1.364683531250012516, 2.030208333674750953, 0.7879004041258379498 ) ) ;
#43868 = CARTESIAN_POINT ( 'NONE',  ( 2.723678392350858957, -1.506833864184083493, -0.8575499777047421723 ) ) ;
#43869 = CARTESIAN_POINT ( 'NONE',  ( 2.343362483081043557, 1.739954169810492557, 0.04345107811378270263 ) ) ;
#43870 = CARTESIAN_POINT ( 'NONE',  ( 4.826339496784873617, 8.574553812983598533, -0.7216878364870257245 ) ) ;
#43871 = CARTESIAN_POINT ( 'NONE',  ( -12.04274103669372309, 7.374159847806027734, 3.963224530603232765 ) ) ;
#43872 = CARTESIAN_POINT ( 'NONE',  ( 1.845077155533506374, -1.080901620906085325, 1.701686244941137183 ) ) ;
#43873 = CARTESIAN_POINT ( 'NONE',  ( -0.08172171391244466288, -9.906619969460795261, -10.99969643042365419 ) ) ;
#43874 = CARTESIAN_POINT ( 'NONE',  ( -3.461074353238556167, 7.259946855412102273, 0.000000000000000000 ) ) ;
#43875 = EDGE_CURVE ( 'NONE', #40754, #206605, #91782, .T. ) ;
#43876 = CARTESIAN_POINT ( 'NONE',  ( 1.252734725572089536, -1.555569235904795011, 1.211063379650168415 ) ) ;
#43877 = PRESENTATION_LAYER_ASSIGNMENT (  '', '', ( #23105 ) ) ;
#43879 = CARTESIAN_POINT ( 'NONE',  ( -4.990809943606273613, 7.876343129965691858, -1.082531754730549967 ) ) ;
#43878 = CARTESIAN_POINT ( 'NONE',  ( 5.308822938259078583, -0.4706598425541131947, -1.853433239416848455 ) ) ;
#43880 = CARTESIAN_POINT ( 'NONE',  ( -4.733205024502264102, 7.575804057677677505, 1.082531754730549967 ) ) ;
#43881 = CARTESIAN_POINT ( 'NONE',  ( 4.864343252252968597, 8.897093904262280972, 0.000000000000000000 ) ) ;
#43882 = CARTESIAN_POINT ( 'NONE',  ( -6.149505192250180663, 9.332117270003974951, -1.199719254218452047 ) ) ;
#43883 = CARTESIAN_POINT ( 'NONE',  ( 1.242838512808578377, 1.947023393874779851, 0.5366068325038054754 ) ) ;
#43884 = CARTESIAN_POINT ( 'NONE',  ( 5.151735183068521629, 5.112705256442466428, 1.040834085586084257E-14 ) ) ;
#43885 = CARTESIAN_POINT ( 'NONE',  ( 6.001056180859140277, 1.891180833080384982, -1.322043635676501072 ) ) ;
#43886 = CARTESIAN_POINT ( 'NONE',  ( 5.810985101215744741, -1.547553103248515027, 1.205733875218002238 ) ) ;
#43887 = CARTESIAN_POINT ( 'NONE',  ( 3.344534541303633368, -1.931932779036081183, -0.3399374921491463142 ) ) ;
#43888 = CARTESIAN_POINT ( 'NONE',  ( 9.420217803396747414, 9.884675613584706255, 0.7998128361456462443 ) ) ;
#43889 = CARTESIAN_POINT ( 'NONE',  ( 0.5807041986926939625, -0.7231374404764076003, 1.882475062126743204 ) ) ;
#43890 = ORIENTED_EDGE ( 'NONE', *, *, #209881, .T. ) ;
#43891 = CARTESIAN_POINT ( 'NONE',  ( 0.9368845280443529600, -1.665339089426773000, 1.307453795268032071 ) ) ;
#43893 = CARTESIAN_POINT ( 'NONE',  ( -6.398558430645608475, 9.552403038140164782, -1.199719254218440723 ) ) ;
#43892 = CARTESIAN_POINT ( 'NONE',  ( -4.796887421136680985, 4.490790167614548523, 1.214306433183764966E-14 ) ) ;
#43894 = CARTESIAN_POINT ( 'NONE',  ( 1.763359053103892293, 0.9455654613358072114, 1.579637215005654349 ) ) ;
#43895 = ORIENTED_EDGE ( 'NONE', *, *, #98658, .F. ) ;
#43896 = CARTESIAN_POINT ( 'NONE',  ( 11.75926639340631041, 7.883781762499332046, -2.170924231206847743 ) ) ;
#43897 = CARTESIAN_POINT ( 'NONE',  ( 2.988655875014298857, -1.259908772670719657, 1.705623289672608678 ) ) ;
#43898 = CARTESIAN_POINT ( 'NONE',  ( 0.7499999999999902300, 4.097916667349481123, -1.299038105676658228 ) ) ;
#43899 = CARTESIAN_POINT ( 'NONE',  ( 8.749089199520284410, 9.101692242395490240, 0.7998128361456481317 ) ) ;
#43900 = CARTESIAN_POINT ( 'NONE',  ( 8.174640274396848483, 8.501778173076651512, 0.7998128361456291469 ) ) ;
#43901 = CARTESIAN_POINT ( 'NONE',  ( 3.673166697908346379, 0.05419028943656278852, -2.060251915681856616 ) ) ;
#43903 = CARTESIAN_POINT ( 'NONE',  ( 0.3097736896383457839, 1.270387085892955792, -1.333027339516623888 ) ) ;
#43902 = CARTESIAN_POINT ( 'NONE',  ( -6.530223543276495235, 10.77034456713125188, -0.7998128361456291469 ) ) ;
#43904 = CARTESIAN_POINT ( 'NONE',  ( 1.364683531249988535, 4.155208333674753618, -0.7879004041258239610 ) ) ;
#43905 = CARTESIAN_POINT ( 'NONE',  ( 1.378881877344245055, 3.612814789602863730, 0.5904953584335879135 ) ) ;
#43906 = AXIS2_PLACEMENT_3D ( 'NONE', #76714, #13834, #25829 ) ;
#43907 = CARTESIAN_POINT ( 'NONE',  ( -3.094265954482842140, 2.800000000000024691, -2.490342512183689294 ) ) ;
#43908 = CARTESIAN_POINT ( 'NONE',  ( 2.337552072221838362, -2.021662389422747452, 1.015643474128526291 ) ) ;
#43909 = CARTESIAN_POINT ( 'NONE',  ( -8.026063749610047537, 11.34719622697832264, -1.082531754730543971 ) ) ;
#43910 = CARTESIAN_POINT ( 'NONE',  ( 2.003910543607852812, -0.7718314612508870853, 1.639047433122240660 ) ) ;
#43911 = CARTESIAN_POINT ( 'NONE',  ( 3.643669983026840420, 1.900603903897592595, -0.2398275428802750520 ) ) ;
#43912 = CARTESIAN_POINT ( 'NONE',  ( 4.105968538015460467, 0.7004154448949986289, -1.948405661837959713 ) ) ;
#43913 = CARTESIAN_POINT ( 'NONE',  ( 1.364683531249986537, 2.467708333674753174, -0.7879004041258239610 ) ) ;
#43914 = AXIS2_PLACEMENT_3D ( 'NONE', #179708, #64871, #65909 ) ;
#43915 = CARTESIAN_POINT ( 'NONE',  ( 2.553542074257345362, 0.5272840835596946940, -1.899572117879143596 ) ) ;
#43916 = CARTESIAN_POINT ( 'NONE',  ( 6.727182134110236689, 0.003007720480393410133, 1.910970182385362870 ) ) ;
#43917 = CARTESIAN_POINT ( 'NONE',  ( 2.746779440450992649, -1.556306552617524597, 1.037596984913228937 ) ) ;
#43919 = CARTESIAN_POINT ( 'NONE',  ( 4.634937608369048334, 8.440560775401745985, -0.4060563726728562139 ) ) ;
#43918 = CARTESIAN_POINT ( 'NONE',  ( 2.157223245065964967, -1.782429894076944521, 1.465742965790328700 ) ) ;
#43920 = CARTESIAN_POINT ( 'NONE',  ( 2.312761410774709425, -1.440873624601293423, 1.177899742917737358 ) ) ;
#43921 = CARTESIAN_POINT ( 'NONE',  ( 1.364683531249990311, 3.384375000341416140, 1.214306433183764966E-14 ) ) ;
#43922 = CARTESIAN_POINT ( 'NONE',  ( 6.426245203579573406, 1.057156898221789598, 1.771034054399809987 ) ) ;
#43923 = CARTESIAN_POINT ( 'NONE',  ( -5.773074481320628948, 5.629675071162500544, 0.000000000000000000 ) ) ;
#43924 = CARTESIAN_POINT ( 'NONE',  ( 5.449487677688982679, 8.445153826357429949, -1.199719254218446718 ) ) ;
#43925 = CARTESIAN_POINT ( 'NONE',  ( -1.465205965978033209, 3.329490383941810183, 0.3306380942217598262 ) ) ;
#43926 = CARTESIAN_POINT ( 'NONE',  ( 0.9089716955857042313, 1.593442362523834754, -1.377222155420864347 ) ) ;
#43927 = CARTESIAN_POINT ( 'NONE',  ( 1.364683531249990311, 4.696875000341417916, 1.214306433183764966E-14 ) ) ;
#43928 = CARTESIAN_POINT ( 'NONE',  ( 6.415313282229532454, -0.2716245656670859820, 2.144420208805633887 ) ) ;
#43929 = CARTESIAN_POINT ( 'NONE',  ( -0.03488881496042146174, -1.619560933857542073, 1.206636643155176714 ) ) ;
#43930 = CARTESIAN_POINT ( 'NONE',  ( -1.602468905319636405E-14, -1.053124999658583638, -1.575800808251665908 ) ) ;
#43931 = CARTESIAN_POINT ( 'NONE',  ( -4.446711195602255806, 5.250546485366484717, -1.082531754730544860 ) ) ;
#43934 = CARTESIAN_POINT ( 'NONE',  ( 3.497640442645619796, 6.064035702186436616, -1.082531754730543083 ) ) ;
#43933 = CARTESIAN_POINT ( 'NONE',  ( 6.925078400183555694, 1.300159714275823664, 1.872400972051186496 ) ) ;
#43932 = CARTESIAN_POINT ( 'NONE',  ( 7.388267364804250725, 7.584343111885245570, -0.7998128361456341429 ) ) ;
#43935 = CARTESIAN_POINT ( 'NONE',  ( -5.327428015527048366, 5.180030537728460338, -0.7998128361456362523 ) ) ;
#43936 = CARTESIAN_POINT ( 'NONE',  ( 4.364470425680367249, -1.957169923074707274, -0.4852690807995581057 ) ) ;
#43938 = CARTESIAN_POINT ( 'NONE',  ( -6.333067150914850174, 8.481940657524365434, 1.443375672974064550 ) ) ;
#43937 = CARTESIAN_POINT ( 'NONE',  ( -9.327646496521984076, 11.90534021740758064, -1.443375672974059665 ) ) ;
#43940 = CARTESIAN_POINT ( 'NONE',  ( 0.6823417656249969321, 10.52604166700806587, -1.181850606188757036 ) ) ;
#43939 = CARTESIAN_POINT ( 'NONE',  ( 5.577088068215094729, -0.04877400797019536272, -2.161318155665878038 ) ) ;
#43941 = CARTESIAN_POINT ( 'NONE',  ( -11.84668730067608600, 13.39999999999998259, 1.399999999999998579 ) ) ;
#43942 = CARTESIAN_POINT ( 'NONE',  ( -8.123306592882240551, 12.62894145833798376, 0.000000000000000000 ) ) ;
#43944 = CARTESIAN_POINT ( 'NONE',  ( 6.609000000000036401, 0.002801690667396730238, 2.000160786441218086 ) ) ;
#43943 = CARTESIAN_POINT ( 'NONE',  ( -5.043269954159181445, 8.827639346586952485, 1.214306433183764966E-14 ) ) ;
#43945 = CARTESIAN_POINT ( 'NONE',  ( -1.364683531250014514, 0.3010416670080866552, -0.7879004041258359514 ) ) ;
#43946 = CARTESIAN_POINT ( 'NONE',  ( 0.008494835128459769791, -5.601932402265091149, 11.00038526257045390 ) ) ;
#43947 = CARTESIAN_POINT ( 'NONE',  ( -1.500000000000015099, 8.729166666666664298, -0.8660254037844309360 ) ) ;
#43948 = CARTESIAN_POINT ( 'NONE',  ( 1.224769985559545304, -0.04580521419573525821, 1.724442238450181186 ) ) ;
#43949 = CARTESIAN_POINT ( 'NONE',  ( 5.806634928402749196, 9.996434193103704402, -0.7998128361456481317 ) ) ;
#43950 = CARTESIAN_POINT ( 'NONE',  ( 5.180097208873055692, 8.201141289397330780, -1.199719254218450271 ) ) ;
#43951 = CARTESIAN_POINT ( 'NONE',  ( -1.402160292154681736E-14, -0.8656249996585829720, 1.575800808251672791 ) ) ;
#43952 = CARTESIAN_POINT ( 'NONE',  ( 0.5437790142346760058, 1.764394620056912055, 0.1386062191098563767 ) ) ;
#43953 = CARTESIAN_POINT ( 'NONE',  ( 2.279941584743001126, 1.973825526184776580, -0.3948664393432794184 ) ) ;
#43954 = FILL_AREA_STYLE_COLOUR ( '', #157784 ) ;
#43955 = CARTESIAN_POINT ( 'NONE',  ( 3.962124768131184638, 2.190450126196175074, -0.2673064950309556043 ) ) ;
#43956 = CARTESIAN_POINT ( 'NONE',  ( 5.524361701572801486, 1.063745579927848794, 1.892525341434271091 ) ) ;
#43957 = ORIENTED_EDGE ( 'NONE', *, *, #179963, .F. ) ;
#43958 = CARTESIAN_POINT ( 'NONE',  ( -1.402160292154681736E-14, -0.4124999999999747202, -1.732050807568870754 ) ) ;
#43959 = CARTESIAN_POINT ( 'NONE',  ( 8.066738210006679566, 10.43428054980638997, 1.443375672974076540 ) ) ;
#43961 = CARTESIAN_POINT ( 'NONE',  ( 2.566029989117986077, -1.034146858587611906, 1.730878619409223163 ) ) ;
#43960 = CARTESIAN_POINT ( 'NONE',  ( 3.141385665567609564, 0.05408136815227351790, 2.119969838212852675 ) ) ;
#43963 = ORIENTED_EDGE ( 'NONE', *, *, #23354, .F. ) ;
#43962 = CARTESIAN_POINT ( 'NONE',  ( 3.410248120744460376, -1.809760825414870267, -0.08362741940017533182 ) ) ;
#43964 = CARTESIAN_POINT ( 'NONE',  ( 5.176180785367283654, 9.260904359562321275, -0.7998128361456481317 ) ) ;
#43965 = ORIENTED_EDGE ( 'NONE', *, *, #3532, .F. ) ;
#43966 = EDGE_CURVE ( 'NONE', #9078, #24478, #204434, .T. ) ;
#43967 = CARTESIAN_POINT ( 'NONE',  ( 0.2857447052702493662, -0.8859512962964136706, 1.647562673099879138 ) ) ;
#43968 = CARTESIAN_POINT ( 'NONE',  ( 5.281064527722868718, 6.119995689553514140, 1.199719254218462483 ) ) ;
#43969 = CARTESIAN_POINT ( 'NONE',  ( 6.375623774462673587, 1.745513195383348926, -0.5351242734627087438 ) ) ;
#43971 = CARTESIAN_POINT ( 'NONE',  ( 1.376049117821566137, -1.906831126389372022, -0.1839060664316337634 ) ) ;
#43970 = CARTESIAN_POINT ( 'NONE',  ( -4.090809663021341969, 5.795697244990093644, 1.599625672291267398 ) ) ;
#43972 = CARTESIAN_POINT ( 'NONE',  ( -0.7500000000000179856, 8.572916667349467446, 1.299038105676658228 ) ) ;
#43973 = CARTESIAN_POINT ( 'NONE',  ( -1.402160292154681736E-14, 1.759375000341421469, -1.575800808251659024 ) ) ;
#43974 = DIRECTION ( 'NONE',  ( -0.000000000000000000, 1.000000000000000000, -0.000000000000000000 ) ) ;
#43975 = CARTESIAN_POINT ( 'NONE',  ( 5.295850518597075229, -0.7817450549502875656, 2.015575934489414411 ) ) ;
#43976 = CARTESIAN_POINT ( 'NONE',  ( -4.665414256878293031, 7.496714828783040296, -1.082531754730549967 ) ) ;
#43977 = CARTESIAN_POINT ( 'NONE',  ( -6.074935347375019390, 9.245119117649618801, 1.199719254218452047 ) ) ;
#43978 = CARTESIAN_POINT ( 'NONE',  ( 3.058948843759463188, 0.5191580478346515815, 2.055925682384197373 ) ) ;
#43980 = CARTESIAN_POINT ( 'NONE',  ( -10.12897898315521061, 6.154003805053667620, 5.673299828594959848 ) ) ;
#43979 = CARTESIAN_POINT ( 'NONE',  ( -0.02988540731099689068, 4.098597030192621560, -2.281328281275496916 ) ) ;
#43981 = CARTESIAN_POINT ( 'NONE',  ( 4.305907937463241630, -1.966273716216637046, 0.1420514027590073225 ) ) ;
#43982 = CARTESIAN_POINT ( 'NONE',  ( 6.521744167503259249, -0.4122283346772101509, 1.874327247564554266 ) ) ;
#43983 = EDGE_LOOP ( 'NONE', ( #61017, #13443, #126013, #22351 ) ) ;
#43984 = AXIS2_PLACEMENT_3D ( 'NONE', #70950, #154371, #22194 ) ;
#43985 = CARTESIAN_POINT ( 'NONE',  ( 5.296159404803077564, -0.9547103268642830320, -1.889991272064439176 ) ) ;
#43986 = SURFACE_STYLE_FILL_AREA ( #192327 ) ;
#43987 = CARTESIAN_POINT ( 'NONE',  ( 6.795365950078042339, -1.759944107108902367, 0.8842400836535941888 ) ) ;
#43988 = CARTESIAN_POINT ( 'NONE',  ( 2.290873232013816541, 1.501373485850267198, 1.231690586011934041 ) ) ;
#43989 = ORIENTED_EDGE ( 'NONE', *, *, #205891, .F. ) ;
#43990 = CARTESIAN_POINT ( 'NONE',  ( 6.313256805818848960, 7.394496357324014113, 1.199719254218452047 ) ) ;
#43991 = CARTESIAN_POINT ( 'NONE',  ( 6.875920180786008196, 8.050936961452347163, -1.199719254218452047 ) ) ;
#43993 = CARTESIAN_POINT ( 'NONE',  ( 5.198661835836162481, 8.152523677529138979, 1.199719254218462483 ) ) ;
#43992 = CARTESIAN_POINT ( 'NONE',  ( 3.978531085967525360, -0.2047937889433377179, -2.080580830362771305 ) ) ;
#43994 = CARTESIAN_POINT ( 'NONE',  ( 5.989670002187236442, 10.20997511251894529, -0.7998128361456481317 ) ) ;
#43996 = ORIENTED_EDGE ( 'NONE', *, *, #125545, .T. ) ;
#43995 = CARTESIAN_POINT ( 'NONE',  ( 0.3459856143687444208, 0.9327069207067508749, -1.552719410179828952 ) ) ;
#43997 = CARTESIAN_POINT ( 'NONE',  ( 5.039771180630152614, -1.558841386063321455, -1.562417271110942307 ) ) ;
#43998 = CARTESIAN_POINT ( 'NONE',  ( -0.5000000000000403011, 3.949999999999953548, 0.4499999999999556577 ) ) ;
#43999 = CARTESIAN_POINT ( 'NONE',  ( 3.258999418838660400, -1.672185875938383859, 1.440126295696932068 ) ) ;
#44000 = CARTESIAN_POINT ( 'NONE',  ( 4.858757509019037357, 5.629766575900002401, 2.420000000000000373 ) ) ;
#44001 = CARTESIAN_POINT ( 'NONE',  ( 2.086439996564274146, -1.175226666667992914, 1.508458442701497315 ) ) ;
#44002 = CARTESIAN_POINT ( 'NONE',  ( 9.423080456697809026, 10.95234760669099749, -1.199719254218446718 ) ) ;
#44003 = CARTESIAN_POINT ( 'NONE',  ( 4.756339170418532269, -2.069830778647030023, -0.05414847147890837487 ) ) ;
#44005 = CARTESIAN_POINT ( 'NONE',  ( 2.342841879718413622, 0.4729757327756216601, 2.109170662781891359 ) ) ;
#44004 = CARTESIAN_POINT ( 'NONE',  ( 9.617648866954018771, -9.063431457505044975, -0.6035590660249217088 ) ) ;
#44006 = CARTESIAN_POINT ( 'NONE',  ( 5.073855206572205567, -1.217758175834412260, 1.821886007100224969 ) ) ;
#44007 = ORIENTED_EDGE ( 'NONE', *, *, #156764, .F. ) ;
#44008 = CARTESIAN_POINT ( 'NONE',  ( -6.147915675425737803, 6.345191967827721768, 0.2080023349117297582 ) ) ;
#44009 = CARTESIAN_POINT ( 'NONE',  ( 3.475000000000000533, -1.954166666666666163, 2.006292185433948827 ) ) ;
#44010 = CARTESIAN_POINT ( 'NONE',  ( -0.1341411654175228285, 8.212692222353540572, 2.039118504324687553 ) ) ;
#44011 = CARTESIAN_POINT ( 'NONE',  ( 5.194709132691408549, 6.089524072008651423, 1.199719254218452935 ) ) ;
#44012 = DIRECTION ( 'NONE',  ( -0.6483454320283800199, 0.000000000000000000, 0.7613463080411787542 ) ) ;
#44013 = CARTESIAN_POINT ( 'NONE',  ( -3.492107083971660586, 6.231819477012331632, 1.199719254218452935 ) ) ;
#44014 = CARTESIAN_POINT ( 'NONE',  ( -7.863365906246048809, 12.11775129068834289, -0.7216878364870267237 ) ) ;
#44016 = CARTESIAN_POINT ( 'NONE',  ( 6.384963997392946844, 6.413822516572072807, 0.7998128361456352531 ) ) ;
#44015 = COLOUR_RGB ( '', 0.09019608, 0.27058824, 0.51372549) ;
#44017 = CARTESIAN_POINT ( 'NONE',  ( 6.227406488038683463, 0.1581931229415085571, -2.064300627111630870 ) ) ;
#44018 = CARTESIAN_POINT ( 'NONE',  ( 4.723225685987796574, -0.09301374627979085152, 1.924373785979951013 ) ) ;
#44019 = CARTESIAN_POINT ( 'NONE',  ( 6.310183273250552283, 1.218863855842572175, -1.731025912240143017 ) ) ;
#44020 = FACE_OUTER_BOUND ( 'NONE', #7979, .T. ) ;
#44021 = CARTESIAN_POINT ( 'NONE',  ( 5.015626762051672571, 7.938982758113895422, 1.199719254218462483 ) ) ;
#44022 = CARTESIAN_POINT ( 'NONE',  ( -4.218512253981381299, 3.978430757497701364, -0.5307291018261834914 ) ) ;
#44023 = CARTESIAN_POINT ( 'NONE',  ( 4.909022984592102290, -1.584153972474154459, 1.169931220002416339 ) ) ;
#44024 = CARTESIAN_POINT ( 'NONE',  ( 0.6213436022244859247, -2.079703760468250451, 0.6910661131078955632 ) ) ;
#44025 = CARTESIAN_POINT ( 'NONE',  ( 4.406759617291758246, 1.409692282476209924, -1.160130723419292131 ) ) ;
#44026 = CARTESIAN_POINT ( 'NONE',  ( 7.200788982633824276, 7.573544365927161515, 0.000000000000000000 ) ) ;
#44027 = CARTESIAN_POINT ( 'NONE',  ( 4.378920427089557421, 5.171457255435017331, -1.082531754730548412 ) ) ;
#44028 = CARTESIAN_POINT ( 'NONE',  ( -5.596483547390937119, 9.751257581923240991, 0.000000000000000000 ) ) ;
#44029 = CARTESIAN_POINT ( 'NONE',  ( 5.011674058906918638, 5.875983152593414971, 1.199719254218452047 ) ) ;
#44030 = ORIENTED_EDGE ( 'NONE', *, *, #188668, .F. ) ;
#44032 = CARTESIAN_POINT ( 'NONE',  ( 5.062748685862976217, 0.5883423404384033883, 1.925289297555386359 ) ) ;
#44031 = CARTESIAN_POINT ( 'NONE',  ( 3.192734241421916419, 1.453351889590439816, 1.130385295574042104 ) ) ;
#44033 = CARTESIAN_POINT ( 'NONE',  ( 0.7205771127097709838, -1.942975266472912299, -1.227557580038857399 ) ) ;
#44034 = CARTESIAN_POINT ( 'NONE',  ( 5.981297772519294398, -0.05168599705708888659, 1.961257141919122926 ) ) ;
#44035 = CARTESIAN_POINT ( 'NONE',  ( -5.368138756007025947, 8.350246751061767725, 1.199719254218452047 ) ) ;
#44036 = CARTESIAN_POINT ( 'NONE',  ( 10.67552548858665418, -7.034525073436789455, 9.912773128239630417E-13 ) ) ;
#44037 = CARTESIAN_POINT ( 'NONE',  ( -4.946027110887008860, 4.664786472323266153, -0.7998128361456221525 ) ) ;
#44038 = CARTESIAN_POINT ( 'NONE',  ( 0.9067890187421032699, 0.5993529260880943177, 1.981728858978973218 ) ) ;
#44039 = CARTESIAN_POINT ( 'NONE',  ( -4.553559489343377287, 6.405848385690952718, -1.599625672291271394 ) ) ;
#44041 = CARTESIAN_POINT ( 'NONE',  ( 0.3209005354254980680, -0.09642172165634513292, 1.868300368337752815 ) ) ;
#44040 = CARTESIAN_POINT ( 'NONE',  ( 1.804351596996961238, 1.546985077243122397, -1.406606537801007972 ) ) ;
#44042 = CARTESIAN_POINT ( 'NONE',  ( 0.5160254906862444813, 7.984099418343982180, -1.935262202534223208 ) ) ;
#44043 = ORIENTED_EDGE ( 'NONE', *, *, #188975, .F. ) ;
#44044 = DIRECTION ( 'NONE',  ( 1.000000000000000000, -0.000000000000000000, -0.000000000000000000 ) ) ;
#44045 = CARTESIAN_POINT ( 'NONE',  ( 1.557743604271996762, -1.230989698698783608, 1.230628217043183925 ) ) ;
#44046 = CARTESIAN_POINT ( 'NONE',  ( 5.660692828905515839, 6.562895374266609849, -1.199719254218445830 ) ) ;
#44048 = CARTESIAN_POINT ( 'NONE',  ( 1.515977770626730781, 8.685538819012467826, 2.532029653471363773 ) ) ;
#44047 = CARTESIAN_POINT ( 'NONE',  ( -11.48788097203293823, 13.83043054397690241, -3.469500700354831491 ) ) ;
#44049 = CARTESIAN_POINT ( 'NONE',  ( 3.158550911874979938, -1.305529951647845355, 1.127390448682374924 ) ) ;
#44050 = CARTESIAN_POINT ( 'NONE',  ( 2.630644284709309666, 0.2711686948545319886, 2.174668582101045633 ) ) ;
#44051 = CARTESIAN_POINT ( 'NONE',  ( 5.110101661328442901, -2.196521081226535443, 0.2136625748923453583 ) ) ;
#44052 = DIRECTION ( 'NONE',  ( 0.000000000000000000, 0.000000000000000000, 1.000000000000000000 ) ) ;
#44053 = TOROIDAL_SURFACE ( 'NONE', #40650, 0.8300000000000010703, 0.08000000000000000167 ) ;
#44054 = CARTESIAN_POINT ( 'NONE',  ( 2.870184708472456325, -2.148041568373111776, 0.3144570722862209955 ) ) ;
#44055 = CARTESIAN_POINT ( 'NONE',  ( 0.7854531640391904102, 1.224056292049885419, 1.354719642434290439 ) ) ;
#44056 = CARTESIAN_POINT ( 'NONE',  ( 3.520818605202329810, 0.3149718393082919232, 2.093694903831443188 ) ) ;
#44057 = CARTESIAN_POINT ( 'NONE',  ( 6.539320575229251808, 0.01001626003939220556, 1.796977979958065852 ) ) ;
#44058 = ORIENTED_EDGE ( 'NONE', *, *, #27074, .F. ) ;
#44060 = CARTESIAN_POINT ( 'NONE',  ( -0.6823417656250003738, 1.030208333674752286, -1.181850606188749264 ) ) ;
#44059 = CARTESIAN_POINT ( 'NONE',  ( 3.421668107411596882, -1.366637645153226055, -1.840301194555084230 ) ) ;
#44061 = CARTESIAN_POINT ( 'NONE',  ( 6.727182134110238465, -0.007837387828812580545, 2.289081727344749240 ) ) ;
#44062 = CARTESIAN_POINT ( 'NONE',  ( 4.379447312414087357, 5.068108938359919158, -1.199719254218452047 ) ) ;
#44063 = CIRCLE ( 'NONE', #175485, 1.250000000000000888 ) ;
#44064 = CARTESIAN_POINT ( 'NONE',  ( 5.830790380266278383, 1.493519825859883854, -1.644436761705171612 ) ) ;
#44065 = CARTESIAN_POINT ( 'NONE',  ( -6.073689629242158716, 9.069426419882418600, -1.082531754730538864 ) ) ;
#44066 = CARTESIAN_POINT ( 'NONE',  ( 3.212919216758630014, 6.692230152952963529, 0.000000000000000000 ) ) ;
#44067 = CARTESIAN_POINT ( 'NONE',  ( -4.894130264408858899, 8.653643041878236630, -0.7216878364870207285 ) ) ;
#44068 = CARTESIAN_POINT ( 'NONE',  ( 0.000000000000000000, -9.900000000000005684, 10.91970695577495931 ) ) ;
#44069 = ORIENTED_EDGE ( 'NONE', *, *, #135546, .T. ) ;
#44070 = CARTESIAN_POINT ( 'NONE',  ( 3.955704058034177351, -1.882473782773282700, -0.7231407674024927790 ) ) ;
#44072 = CARTESIAN_POINT ( 'NONE',  ( 1.815356060102671698, -1.766853000457936806, -1.063981086615989113 ) ) ;
#44071 = CARTESIAN_POINT ( 'NONE',  ( 4.638861114170084399, 8.563755066507100722, 0.7998128361456462443 ) ) ;
#44073 = CARTESIAN_POINT ( 'NONE',  ( -11.81911962874431055, 13.75710573484113830, 1.591749704452489533 ) ) ;
#44074 = CARTESIAN_POINT ( 'NONE',  ( 4.434925645001613681, 5.307073019657559065, -1.082531754730548412 ) ) ;
#44075 = CARTESIAN_POINT ( 'NONE',  ( -1.642778471875000035, -3.317708332855374476, -2.845375778867859751 ) ) ;
#44076 = CARTESIAN_POINT ( 'NONE',  ( -1.364683531250010295, 4.530208333674754506, 0.7879004041258379498 ) ) ;
#44077 = CARTESIAN_POINT ( 'NONE',  ( 5.490230790444213582, -0.5297859672059505032, -2.126319610106224278 ) ) ;
#44078 = CARTESIAN_POINT ( 'NONE',  ( 2.602185585689294367, -0.1948409242511044692, 2.006959980107574371 ) ) ;
#44079 = CARTESIAN_POINT ( 'NONE',  ( 1.909461114401575843, -0.8690924446688346183, -1.623246667998109682 ) ) ;
#44080 = VECTOR ( 'NONE', #137560, 1000.000000000000000 ) ;
#44081 = CARTESIAN_POINT ( 'NONE',  ( 6.337546739384100292, 9.481222731668410120, 1.199719254218460707 ) ) ;
#44082 = CARTESIAN_POINT ( 'NONE',  ( 6.581069972421211389, -0.09314021972051110543, -1.823315219958022482 ) ) ;
#44083 = CARTESIAN_POINT ( 'NONE',  ( -6.191269702934848240, 10.37489842006599616, 0.000000000000000000 ) ) ;
#44085 = CARTESIAN_POINT ( 'NONE',  ( -4.630991987519598396, 7.560518531151607213, 1.199719254218452935 ) ) ;
#44084 = CARTESIAN_POINT ( 'NONE',  ( 6.227429363453246935, -2.132905367568146637, 0.7551758973065140212 ) ) ;
#44086 = CARTESIAN_POINT ( 'NONE',  ( 1.594499780405156830, -2.096077427685174577, -0.2048490792218547185 ) ) ;
#44087 = CARTESIAN_POINT ( 'NONE',  ( -5.692444392891315097, 7.734547439830227411, -1.599625672291271394 ) ) ;
#44088 = CARTESIAN_POINT ( 'NONE',  ( 9.237182729612253951, 9.671134694169463586, 0.7998128361456462443 ) ) ;
#44089 = DIRECTION ( 'NONE',  ( 0.000000000000000000, 0.000000000000000000, 1.000000000000000000 ) ) ;
#44090 = DIRECTION ( 'NONE',  ( 0.6933894494960498589, 0.000000000000000000, -0.7205630238414714173 ) ) ;
#44092 = ADVANCED_FACE ( 'NONE', ( #70168 ), #4098, .T. ) ;
#44091 = CARTESIAN_POINT ( 'NONE',  ( -6.906989191158078079, 10.14557225873805812, -1.199719254218440723 ) ) ;
#44093 = CARTESIAN_POINT ( 'NONE',  ( -0.07538891330675576152, -7.154544010627095219, 9.499700864329900796 ) ) ;
#44094 = CARTESIAN_POINT ( 'NONE',  ( 7.171900071504736296, 9.390302721554109056, -1.443375672974058777 ) ) ;
#44095 = CARTESIAN_POINT ( 'NONE',  ( 4.067188154045468629, 7.737431308562400467, -0.5659913801023385149 ) ) ;
#44096 = CARTESIAN_POINT ( 'NONE',  ( -9.815740026613960723, 11.51441345488021106, -1.082531754730539753 ) ) ;
#44098 = CARTESIAN_POINT ( 'NONE',  ( 3.234858691920166951, 1.406421598713000432, -1.719528915531160385 ) ) ;
#44097 = CARTESIAN_POINT ( 'NONE',  ( 1.406653384705614629, -2.110883996484512970, -0.2024971186788473154 ) ) ;
#44099 = CARTESIAN_POINT ( 'NONE',  ( 0.4345545588612038657, 1.130843733186673639, -1.894998796914903139 ) ) ;
#44100 = CARTESIAN_POINT ( 'NONE',  ( -4.827585214917754719, 7.789877296449459365, -1.199719254218453823 ) ) ;
#44101 = CARTESIAN_POINT ( 'NONE',  ( 5.497994985541524215, 6.373081223675282736, -1.199719254218445830 ) ) ;
#44102 = CARTESIAN_POINT ( 'NONE',  ( 4.738696794244872557, -1.902450960283699199, -0.4786090228221794307 ) ) ;
#44103 = CARTESIAN_POINT ( 'NONE',  ( 8.432281472695482449, 11.92507992053172572, 1.199719254218450271 ) ) ;
#44104 = CARTESIAN_POINT ( 'NONE',  ( -5.672026259827416261, 6.146810915570031675, 0.7861540255039052294 ) ) ;
#44105 = CARTESIAN_POINT ( 'NONE',  ( -0.6823417656250003738, 0.7177083336747519526, -1.181850606188749264 ) ) ;
#44106 = CARTESIAN_POINT ( 'NONE',  ( -6.156811154381562012, 6.355570232966157640, 0.7216878364870257245 ) ) ;
#44108 = ORIENTED_EDGE ( 'NONE', *, *, #98529, .F. ) ;
#44107 = CARTESIAN_POINT ( 'NONE',  ( -6.182154858151506893, 9.195969186943299789, 1.082531754730548412 ) ) ;
#44109 = CARTESIAN_POINT ( 'NONE',  ( 3.779626292077961747, 0.2561244552635975058, -2.104982076983111572 ) ) ;
#44110 = CARTESIAN_POINT ( 'NONE',  ( -5.635349125135588721, 6.603604063193491136, 1.199719254218452935 ) ) ;
#44111 = CARTESIAN_POINT ( 'NONE',  ( 4.627887939457571598, -1.327398817707679868, -1.706084338546076662 ) ) ;
#44112 = CARTESIAN_POINT ( 'NONE',  ( 4.106863108761789505, -0.3106082297497716471, 1.814695527881895698 ) ) ;
#44113 = CARTESIAN_POINT ( 'NONE',  ( -4.274576072154308903, 7.290118009659216192, 0.9321895248279310486 ) ) ;
#44114 = CARTESIAN_POINT ( 'NONE',  ( 0.6823417656249882723, 0.1552083336747514530, 1.181850606188755259 ) ) ;
#44115 = CARTESIAN_POINT ( 'NONE',  ( 5.560439297528310121, -1.575983010118024774, -0.7385839837668640717 ) ) ;
#44116 = CARTESIAN_POINT ( 'NONE',  ( 11.48788097203293823, 9.769569456023095455, -3.469500700354831491 ) ) ;
#44117 = CARTESIAN_POINT ( 'NONE',  ( 3.226477370372302644, 5.747678784534228313, 1.082531754730546636 ) ) ;
#44118 = CARTESIAN_POINT ( 'NONE',  ( 9.278192185738603825, 11.44758586271118084, 7.613438169660605936 ) ) ;
#44119 = CARTESIAN_POINT ( 'NONE',  ( 3.168983506954273999, -1.996715753333128118, -0.8287754370841573515 ) ) ;
#44120 = CARTESIAN_POINT ( 'NONE',  ( 6.116564501996816894, 0.5879282371138266905, -1.928457050679150298 ) ) ;
#44121 = CARTESIAN_POINT ( 'NONE',  ( -8.365017589507372620, 9.821903944922480534, 1.082531754730558626 ) ) ;
#44122 = CARTESIAN_POINT ( 'NONE',  ( 2.553791647773369089, 0.5774160426356907960, -2.083079400968433248 ) ) ;
#44124 = EDGE_CURVE ( 'NONE', #79317, #34325, #62016, .T. ) ;
#44123 =( BOUNDED_CURVE ( )  B_SPLINE_CURVE ( 2, ( #116286, #68515, #200647, #117356, #202784 ),
 .UNSPECIFIED., .F., .T. ) 
 B_SPLINE_CURVE_WITH_KNOTS ( ( 3, 2, 3 ),
 ( 0.5190269744418570808, 0.5250000000000000222, 0.5270515662701394932 ),
 .UNSPECIFIED. ) 
 CURVE ( )  GEOMETRIC_REPRESENTATION_ITEM ( )  RATIONAL_B_SPLINE_CURVE ( ( 0.9456026235272760871, 0.9039719575195083179, 1.000000000000000000, 0.9670170684818317763, 0.9502741377139820589 ) ) 
 REPRESENTATION_ITEM ( '' )  );
#44125 = CARTESIAN_POINT ( 'NONE',  ( 4.165272970243100836, 0.2446167658484849627, -1.956081580383911778 ) ) ;
#44126 = CARTESIAN_POINT ( 'NONE',  ( 0.04676574305502099321, -1.756316032869180921, 1.310637071781264984 ) ) ;
#44127 = CARTESIAN_POINT ( 'NONE',  ( 4.827648274430585751, 0.9952931021880854212, -1.667489682845281207 ) ) ;
#44129 = ORIENTED_EDGE ( 'NONE', *, *, #186987, .T. ) ;
#44128 = CARTESIAN_POINT ( 'NONE',  ( -9.951321562306267410, 10.71222269888655987, 1.040834085586084257E-14 ) ) ;
#44130 = CARTESIAN_POINT ( 'NONE',  ( -5.986807348886189040, 9.142303119412650503, -1.199719254218452047 ) ) ;
#44131 = DIRECTION ( 'NONE',  ( 0.000000000000000000, 1.000000000000000000, 0.000000000000000000 ) ) ;
#44133 = ORIENTED_EDGE ( 'NONE', *, *, #64546, .F. ) ;
#44132 = CARTESIAN_POINT ( 'NONE',  ( -3.980200614063634568, 6.801261928786307642, 1.199719254218452935 ) ) ;
#44134 = CARTESIAN_POINT ( 'NONE',  ( -8.961576348508652146, 10.51788916375733685, -1.082531754730543083 ) ) ;
#44135 = CARTESIAN_POINT ( 'NONE',  ( 2.520803682403276902, 1.441976459853638204, -1.670562425240495363 ) ) ;
#44136 = CARTESIAN_POINT ( 'NONE',  ( -3.285556943750000070, -2.559374999522041172, 0.000000000000000000 ) ) ;
#44137 = CARTESIAN_POINT ( 'NONE',  ( 6.754749089495472703, -0.5201146403621333958, -1.891512521893109700 ) ) ;
#44138 = CARTESIAN_POINT ( 'NONE',  ( 1.364683531249988535, 5.467708333674750953, -0.7879004041258300672 ) ) ;
#44139 = CARTESIAN_POINT ( 'NONE',  ( 0.7499999999999902300, 4.847916667349482012, -1.299038105676658228 ) ) ;
#44140 = CARTESIAN_POINT ( 'NONE',  ( 5.125043568333415678, 6.701081866602433657, -1.409791652392645700 ) ) ;
#44142 = LINE ( 'NONE', #90765, #99540 ) ;
#44141 = CARTESIAN_POINT ( 'NONE',  ( -7.065207446497166366, 9.336104335703744539, 0.000000000000000000 ) ) ;
#44143 = CARTESIAN_POINT ( 'NONE',  ( 5.402248404572855378, 1.391679675130308880, -1.205515946264820615 ) ) ;
#44144 = ORIENTED_EDGE ( 'NONE', *, *, #30090, .T. ) ;
#44145 = CARTESIAN_POINT ( 'NONE',  ( -7.561650146977034455E-14, -0.5468749996585524631, 1.570758158831754070 ) ) ;
#44146 = CARTESIAN_POINT ( 'NONE',  ( -8.182509401047415309, 9.505014708432145909, 1.199719254218462483 ) ) ;
#44147 = DIRECTION ( 'NONE',  ( 1.000000000000000000, 0.000000000000000000, 0.000000000000000000 ) ) ;
#44148 = CARTESIAN_POINT ( 'NONE',  ( 5.959260761812961604, -1.790568634313693730, 1.135864312162476297 ) ) ;
#44149 = LINE ( 'NONE', #27881, #35747 ) ;
#44150 = CARTESIAN_POINT ( 'NONE',  ( 5.834086172582112262, 5.700855377634248100, 1.040834085586084257E-14 ) ) ;
#44151 = CARTESIAN_POINT ( 'NONE',  ( 6.204382384804184802, -0.7375479284208189545, -1.924474620761642996 ) ) ;
#44154 = CARTESIAN_POINT ( 'NONE',  ( 4.247483403459266782, 1.840758003770435414, -0.04960325993209198370 ) ) ;
#44153 = CARTESIAN_POINT ( 'NONE',  ( 2.470971460243949203, 1.660895280785526618, 0.8397924955986632023 ) ) ;
#44152 = CARTESIAN_POINT ( 'NONE',  ( -1.247849810309911600, 13.37576698399836594, 0.5524780460566154350 ) ) ;
#44155 = CARTESIAN_POINT ( 'NONE',  ( 6.286176778230493589, 10.48562334124426698, 0.7998128361456462443 ) ) ;
#44156 = CARTESIAN_POINT ( 'NONE',  ( 0.3423093779010028537, 2.999999999999988898, 0.3423093779009768189 ) ) ;
#44157 = CARTESIAN_POINT ( 'NONE',  ( -7.944151662964566540, 8.232874793072271657, 0.000000000000000000 ) ) ;
#44159 = ORIENTED_EDGE ( 'NONE', *, *, #189732, .F. ) ;
#44158 = DIRECTION ( 'NONE',  ( -0.6483454320283800199, 0.000000000000000000, 0.7613463080411786432 ) ) ;
#44160 = VECTOR ( 'NONE', #191070, 1000.000000000000000 ) ;
#44161 = CARTESIAN_POINT ( 'NONE',  ( 4.073040751519330094, -2.058760688187323495, -0.7953439701907027981 ) ) ;
#44162 = CARTESIAN_POINT ( 'NONE',  ( 5.905634875922824989, -0.5580066813290808225, 2.192401876011939699 ) ) ;
#44163 = CARTESIAN_POINT ( 'NONE',  ( -5.422898255786193111, 8.310169817517122581, -1.082531754730544860 ) ) ;
#44164 = CARTESIAN_POINT ( 'NONE',  ( 6.222923320161976690, 1.335851037236086558, -1.223852264422401692 ) ) ;
#44165 = CARTESIAN_POINT ( 'NONE',  ( -0.1179535434602772825, -2.016182236903838465, -0.04464881524945257807 ) ) ;
#44166 = DIRECTION ( 'NONE',  ( -5.551115123125765446E-17, 0.000000000000000000, 1.000000000000000000 ) ) ;
#44167 = EDGE_CURVE ( 'NONE', #166401, #73904, #42676, .T. ) ;
#44168 = CARTESIAN_POINT ( 'NONE',  ( 9.017865005868369366, 14.59732426908277070, -7.917871330580335432 ) ) ;
#44169 = CARTESIAN_POINT ( 'NONE',  ( 5.496708366351358066, -1.866603419165157041, -0.4147590543357379533 ) ) ;
#44170 = PLANE ( 'NONE',  #130096 ) ;
#44171 = CARTESIAN_POINT ( 'NONE',  ( 1.059204734455133412, 0.3686402435371800013, -1.833797362824276078 ) ) ;
#44172 = AXIS2_PLACEMENT_3D ( 'NONE', #774, #21305, #135109 ) ;
#44173 = CARTESIAN_POINT ( 'NONE',  ( 0.8488426437929346147, -1.825078332268307513, -0.8578388575243289793 ) ) ;
#44175 = CARTESIAN_POINT ( 'NONE',  ( 3.457739842999438817, 0.5116738510754537117, -2.042838612040797752 ) ) ;
#44174 = CARTESIAN_POINT ( 'NONE',  ( -8.143643823302737061, 12.65266822716189843, 0.000000000000000000 ) ) ;
#44176 = CARTESIAN_POINT ( 'NONE',  ( 8.398386088661320414, 11.88553530582519357, -1.199719254218446718 ) ) ;
#44178 = CARTESIAN_POINT ( 'NONE',  ( -7.771848369131641121, 10.09024240211882351, -1.599625672291263179 ) ) ;
#44177 = CARTESIAN_POINT ( 'NONE',  ( -1.500000000000001332, -0.8499999999999757749, 0.000000000000000000 ) ) ;
#44179 = CARTESIAN_POINT ( 'NONE',  ( 11.41126283316774348, 9.841253930915392800, 3.405403429622879230 ) ) ;
#44180 = CARTESIAN_POINT ( 'NONE',  ( 2.795180614130913010, -0.1526695769738794506, -2.014101982623817566 ) ) ;
#44181 = CARTESIAN_POINT ( 'NONE',  ( -1.364683531250012516, 3.530208333674758059, 0.7879004041258379498 ) ) ;
#44182 = CARTESIAN_POINT ( 'NONE',  ( 3.063252641683779753, 5.661212951017999373, 1.199719254218450271 ) ) ;
#44183 = CARTESIAN_POINT ( 'NONE',  ( 4.569695524216377258, 2.097929177840287540, -0.5203329012281321386 ) ) ;
#44184 = CARTESIAN_POINT ( 'NONE',  ( 7.204675194429079505E-15, -1.793749999044084831, -3.475000000000000089 ) ) ;
#44185 = CARTESIAN_POINT ( 'NONE',  ( -1.001543065824772872E-14, 4.962500000000019007, 1.732050807568877637 ) ) ;
#44187 = CARTESIAN_POINT ( 'NONE',  ( -9.497898427948538114, -9.431315562283163700, 0.2398643602166746491 ) ) ;
#44186 = CARTESIAN_POINT ( 'NONE',  ( 7.126746022638799971, 8.343567110280638133, 1.199719254218452047 ) ) ;
#44188 = CARTESIAN_POINT ( 'NONE',  ( 7.565086526301031178, 11.76975868075249387, 1.040834085586084257E-14 ) ) ;
#44190 = CARTESIAN_POINT ( 'NONE',  ( 7.861308842906358230, 15.31505636599913878, -9.009337879868121846 ) ) ;
#44189 = CARTESIAN_POINT ( 'NONE',  ( 0.5026746641029911089, 2.165404592850531440, 0.1593437185135812284 ) ) ;
#44192 = CARTESIAN_POINT ( 'NONE',  ( 1.065666191918061445, -1.167978014494171823, 1.423405568861766168 ) ) ;
#44191 = CARTESIAN_POINT ( 'NONE',  ( -6.914295153289458540, 7.169025221700239925, 0.7216878364870317197 ) ) ;
#44193 = CARTESIAN_POINT ( 'NONE',  ( 0.6823417656249899377, 2.092708333674753174, 1.181850606188767472 ) ) ;
#44194 = CARTESIAN_POINT ( 'NONE',  ( 2.648187065138879692, 0.7411268365287645432, 2.062558662443473523 ) ) ;
#44195 = CARTESIAN_POINT ( 'NONE',  ( 4.161989969715261140, 4.726297878971393196, -7.499999999999991118 ) ) ;
#44196 = CARTESIAN_POINT ( 'NONE',  ( 2.307839474932214419, -0.4956500345179111200, 2.207406129587013766 ) ) ;
#44197 = CARTESIAN_POINT ( 'NONE',  ( -7.314787569772770226, 8.492672571945082183, -1.199719254218452935 ) ) ;
#44198 = CARTESIAN_POINT ( 'NONE',  ( -0.6823417656250212460, 4.863541667008086655, 1.181850606188767472 ) ) ;
#44199 = CARTESIAN_POINT ( 'NONE',  ( 5.107728353013315292, 7.811434107096660640, 1.148430247377411728 ) ) ;
#44200 = CARTESIAN_POINT ( 'NONE',  ( -1.500000000000015099, 12.97916666666666963, -0.8660254037844309360 ) ) ;
#44201 = CARTESIAN_POINT ( 'NONE',  ( 6.373741612200171325, 7.569024981389272710, 1.082531754730549967 ) ) ;
#44202 = CARTESIAN_POINT ( 'NONE',  ( 4.024454502147566615, 1.679793015868607409, 0.5571282570626963082 ) ) ;
#44203 = CIRCLE ( 'NONE', #71834, 0.05000000000000109912 ) ;
#44204 =( BOUNDED_CURVE ( )  B_SPLINE_CURVE ( 3, ( #136753, #202780, #82648, #148732 ),
 .UNSPECIFIED., .F., .T. ) 
 B_SPLINE_CURVE_WITH_KNOTS ( ( 4, 4 ),
 ( 0.000000000000000000, 0.5000000000000001110 ),
 .UNSPECIFIED. ) 
 CURVE ( )  GEOMETRIC_REPRESENTATION_ITEM ( )  RATIONAL_B_SPLINE_CURVE ( ( 1.000000000000000000, 0.3333333333333332038, 0.3333333333333333703, 1.000000000000000222 ) ) 
 REPRESENTATION_ITEM ( '' )  );
#44205 = CARTESIAN_POINT ( 'NONE',  ( 8.398386088661320414, 11.88553530582519357, -1.199719254218446718 ) ) ;
#44206 = CARTESIAN_POINT ( 'NONE',  ( 1.307801118376609839, -0.5120802815330603996, 2.042612192628911139 ) ) ;
#44208 = CARTESIAN_POINT ( 'NONE',  ( -1.500000000000013101, 1.670833333333355153, 0.8660254037844403729 ) ) ;
#44207 = CARTESIAN_POINT ( 'NONE',  ( 1.364683531249996529, 9.963541667008065872, 0.7879004041258405033 ) ) ;
#44209 = CARTESIAN_POINT ( 'NONE',  ( -5.496904935697871863, 5.377753611261092637, 0.7998128361456281477 ) ) ;
#44210 = CARTESIAN_POINT ( 'NONE',  ( 5.993767587909683670, -2.000856116866961187, 0.2496242821527286382 ) ) ;
#44211 = ORIENTED_EDGE ( 'NONE', *, *, #116234, .T. ) ;
#44212 = AXIS2_PLACEMENT_3D ( 'NONE', #61780, #176600, #10871 ) ;
#44213 = ADVANCED_FACE ( 'NONE', ( #88597 ), #73261, .T. ) ;
#44214 = CARTESIAN_POINT ( 'NONE',  ( 9.154780037725547714, 11.70366268214508487, 1.599625672291279388 ) ) ;
#44215 = CARTESIAN_POINT ( 'NONE',  ( 4.100366707588389836, -0.5864361863821172527, -1.776433678864146382 ) ) ;
#44216 = CARTESIAN_POINT ( 'NONE',  ( 4.258688845354158481, -0.6446009455991275061, -1.967446834807617506 ) ) ;
#44217 = CARTESIAN_POINT ( 'NONE',  ( -5.872089928050201024, 8.904503111816948646, 1.082531754730550855 ) ) ;
#44218 = CARTESIAN_POINT ( 'NONE',  ( 0.000000000000000000, -4.000000000000003553, 0.000000000000000000 ) ) ;
#44219 = CARTESIAN_POINT ( 'NONE',  ( -1.522480120926886116, 8.691153603980712461, 2.524399069149781294 ) ) ;
#44220 = CARTESIAN_POINT ( 'NONE',  ( 5.969332771766739931, 10.18624834369502885, -0.7998128361456481317 ) ) ;
#44221 = CARTESIAN_POINT ( 'NONE',  ( -4.910230551782461816, 4.674830742458788713, -0.3039354299698590056 ) ) ;
#44222 = CARTESIAN_POINT ( 'NONE',  ( -0.6823417656250246877, -0.9489583329919115684, 1.181850606188755259 ) ) ;
#44223 = ADVANCED_FACE ( 'NONE', ( #67549 ), #204834, .T. ) ;
#44224 = CARTESIAN_POINT ( 'NONE',  ( 4.387127823891323608, 0.09410986116351567621, 1.959716250186482434 ) ) ;
#44225 = CARTESIAN_POINT ( 'NONE',  ( 1.036482258494644038, 1.943774389176852857, -0.5350038931242264706 ) ) ;
#44226 = CARTESIAN_POINT ( 'NONE',  ( -4.013798184412302739, 7.796799554311066416, 0.4460873486146191835 ) ) ;
#44228 = FILL_AREA_STYLE ('',( #192573 ) ) ;
#44227 = CARTESIAN_POINT ( 'NONE',  ( 8.782984583554449998, 9.141236857102018831, 1.040834085586084257E-14 ) ) ;
#44229 = CARTESIAN_POINT ( 'NONE',  ( 1.124039026005444475, 1.118881483734196935, -1.498852260102357947 ) ) ;
#44230 = CARTESIAN_POINT ( 'NONE',  ( -0.6823417656250212460, 3.801041667008085767, 1.181850606188767472 ) ) ;
#44231 = CARTESIAN_POINT ( 'NONE',  ( 2.988542084594744797, -1.195720007494217585, 1.619529446093708636 ) ) ;
#44233 = CARTESIAN_POINT ( 'NONE',  ( 3.374719764411674205, -0.4154235484931252942, -2.075916080105549177 ) ) ;
#44232 = CARTESIAN_POINT ( 'NONE',  ( -6.914295153289458540, 7.169025221700239925, 0.7216878364870317197 ) ) ;
#44234 = DIRECTION ( 'NONE',  ( 0.000000000000000000, 1.000000000000000000, 0.000000000000000000 ) ) ;
#44235 = CARTESIAN_POINT ( 'NONE',  ( 4.861816338261779613, -0.5554421346023461492, 1.994381909410049669 ) ) ;
#44236 = CARTESIAN_POINT ( 'NONE',  ( 3.061108821635398769, 6.793320401875094561, -0.7998128361456362523 ) ) ;
#44238 = CARTESIAN_POINT ( 'NONE',  ( 4.376584659113025744, 4.000436945253625254, 0.7998128361456341429 ) ) ;
#44237 = CARTESIAN_POINT ( 'NONE',  ( -0.09403702165171158589, -0.8981432076055823055, -1.886421477387869361 ) ) ;
#44240 = ORIENTED_EDGE ( 'NONE', *, *, #212216, .T. ) ;
#44239 = CARTESIAN_POINT ( 'NONE',  ( 5.086841682847768276, -0.2248377094848166835, -1.811598703993194670 ) ) ;
#44241 = CARTESIAN_POINT ( 'NONE',  ( 8.697719238366680372, 10.10609285197134533, 1.199719254218462483 ) ) ;
#44242 = CARTESIAN_POINT ( 'NONE',  ( 7.834474503270790535, -6.459788825448837812, -7.722692672890167032 ) ) ;
#44243 = CARTESIAN_POINT ( 'NONE',  ( 11.15162045555251957, 9.712998552558403276, 5.837063001226317382 ) ) ;
#44244 = CARTESIAN_POINT ( 'NONE',  ( 6.194375513154499302, -2.195555142843173879, -0.2223249613259313806 ) ) ;
#44245 = CARTESIAN_POINT ( 'NONE',  ( -8.012344526598182026E-15, 11.35937500034139980, -1.575800808251669460 ) ) ;
#44246 = CARTESIAN_POINT ( 'NONE',  ( 5.285773936917006921, 1.841837585529454202, -0.5139651673399318055 ) ) ;
#44247 = CARTESIAN_POINT ( 'NONE',  ( -7.648771216403934758, 12.07531685244661723, -0.7998128361456291469 ) ) ;
#44248 = CARTESIAN_POINT ( 'NONE',  ( 6.307567778855705853, 8.381915046796901692, -1.599625672291262513 ) ) ;
#44249 = CARTESIAN_POINT ( 'NONE',  ( -11.84668729410359411, 11.00620512324533529, -1.400000000000001688 ) ) ;
#44250 = ADVANCED_FACE ( 'NONE', ( #91330 ), #34676, .F. ) ;
#44251 =( NAMED_UNIT ( * ) PLANE_ANGLE_UNIT ( ) SI_UNIT ( $, .RADIAN. ) );
#44252 = CARTESIAN_POINT ( 'NONE',  ( 5.172599298813543633, 5.993452922492633839, -1.199719254218452047 ) ) ;
#44253 = ORIENTED_EDGE ( 'NONE', *, *, #45961, .F. ) ;
#44254 = TOROIDAL_SURFACE ( 'NONE', #151554, 2.400000000000000355, 0.1000000000000000056 ) ;
#44255 = CARTESIAN_POINT ( 'NONE',  ( 0.000000000000000000, 0.000000000000000000, 0.000000000000000000 ) ) ;
#44256 = CARTESIAN_POINT ( 'NONE',  ( -0.02299388927988389383, 2.039721852852835582, -2.328191723522631928 ) ) ;
#44257 = CARTESIAN_POINT ( 'NONE',  ( 7.679767667498067496, 7.924426798361372093, 0.000000000000000000 ) ) ;
#44258 = CARTESIAN_POINT ( 'NONE',  ( -6.121671443416687453, 7.010146470470823843, 0.9629068762325782016 ) ) ;
#44259 = CARTESIAN_POINT ( 'NONE',  ( -6.426201623197489887, 6.599582769926260362, 0.7216878364870317197 ) ) ;
#44260 = CARTESIAN_POINT ( 'NONE',  ( 3.334415713957098681, 5.977569868670206787, -1.199719254218446718 ) ) ;
#44261 = CARTESIAN_POINT ( 'NONE',  ( 2.922656654487673311, -1.361644196593906342, 1.423118114318456584 ) ) ;
#44262 = EDGE_CURVE ( 'NONE', #120674, #39859, #117417, .T. ) ;
#44263 = CARTESIAN_POINT ( 'NONE',  ( 3.884388800492278193, -0.6352171928143932611, -1.913798906059568594 ) ) ;
#44264 = CARTESIAN_POINT ( 'NONE',  ( -7.802881099864745984, 9.062115023719057305, -1.199719254218446718 ) ) ;
#44265 = CARTESIAN_POINT ( 'NONE',  ( 4.854701522145073334, 7.821512988214679218, -1.199719254218450271 ) ) ;
#44266 = CARTESIAN_POINT ( 'NONE',  ( 6.727182134110227807, 1.996671600852136352, 2.590479658440256738 ) ) ;
#44267 = B_SPLINE_CURVE_WITH_KNOTS ( 'NONE', 3,
 ( #167486, #49472, #165345, #202074, #37476, #66742, #36404, #131831, #16941, #21196 ),
 .UNSPECIFIED., .F., .F.,
 ( 4, 3, 3, 4 ),
 ( 7.376790794998995890E-17, 3.125231531348378344E-05, 6.250486059666306160E-05, 0.0001052831138300465999 ),
 .UNSPECIFIED. ) ;
#44268 = CARTESIAN_POINT ( 'NONE',  ( 3.451304434523004172, 0.5324976444292061073, -2.125649318046138880 ) ) ;
#44269 = SURFACE_STYLE_FILL_AREA ( #191549 ) ;
#44270 = CARTESIAN_POINT ( 'NONE',  ( 2.274328125206574569, -1.186679513062695257, 1.517402005686524280 ) ) ;
#44271 = CARTESIAN_POINT ( 'NONE',  ( -9.318531651294266638, 9.766041769465124034, -0.7998128361456291469 ) ) ;
#44272 = EDGE_CURVE ( 'NONE', #97798, #105253, #39965, .T. ) ;
#44273 = CARTESIAN_POINT ( 'NONE',  ( 0.1331565106231328843, 0.003911343561965873426, -1.946049565259087455 ) ) ;
#44274 = CARTESIAN_POINT ( 'NONE',  ( 3.255366281057017197, 6.812028071292901998, -0.7216878364870338292 ) ) ;
#44275 = CARTESIAN_POINT ( 'NONE',  ( 7.771848369131631351, 10.09024240211882351, -1.599625672291262513 ) ) ;
#44276 = CARTESIAN_POINT ( 'NONE',  ( 5.717788096661236885, 7.693838750903348789, 1.599625672291267398 ) ) ;
#44277 = CARTESIAN_POINT ( 'NONE',  ( 5.912764389335563919, 6.070849007079172743, -0.7216878364870458196 ) ) ;
#44278 = ORIENTED_EDGE ( 'NONE', *, *, #6091, .T. ) ;
#44280 = CARTESIAN_POINT ( 'NONE',  ( 2.842442125518374496, 1.116481279481882805, -1.674925767759533723 ) ) ;
#44279 = CARTESIAN_POINT ( 'NONE',  ( 6.532758020889952277, -1.641319963461195464, 0.8346263169811756200 ) ) ;
#44281 = CARTESIAN_POINT ( 'NONE',  ( 4.025041230705061146, 2.281562605710918845, -0.2770438755856743929 ) ) ;
#44283 = CARTESIAN_POINT ( 'NONE',  ( 1.621681814730125515, 1.834508062647151272, -0.3115270159769789604 ) ) ;
#44282 = CARTESIAN_POINT ( 'NONE',  ( -0.1288028175206544224, 1.298820314038674928, -2.522219681210400744 ) ) ;
#44284 = CARTESIAN_POINT ( 'NONE',  ( 3.285556943750000070, -1.334374999522040861, 0.000000000000000000 ) ) ;
#44285 = CARTESIAN_POINT ( 'NONE',  ( -4.970620135051034616, 8.062850052469723749, -1.111334424012894617 ) ) ;
#44286 = CARTESIAN_POINT ( 'NONE',  ( 6.486579876843341808, -1.171037552013409089, 1.512559164390047783 ) ) ;
#44287 = CARTESIAN_POINT ( 'NONE',  ( -8.518600588087975822, 8.832788862391110385, 1.040834085586084257E-14 ) ) ;
#44288 = CARTESIAN_POINT ( 'NONE',  ( -5.695833931516914639, 6.778132687258748845, 1.082531754730549078 ) ) ;
#44290 = CARTESIAN_POINT ( 'NONE',  ( 3.766346201128992988, -1.256895078192099335, 1.385637336983977397 ) ) ;
#44289 = CARTESIAN_POINT ( 'NONE',  ( 4.493745196466782943, -2.090321524099489903, -0.04957026750533782833 ) ) ;
#44291 = CARTESIAN_POINT ( 'NONE',  ( 4.989037340148863464, 8.764367963574922982, -0.7216878364870257245 ) ) ;
#44292 = ORIENTED_EDGE ( 'NONE', *, *, #183608, .T. ) ;
#44293 = CARTESIAN_POINT ( 'NONE',  ( -1.443289932012703552E-16, 2.099999999999997868, 2.600000000000008082 ) ) ;
#44294 = CARTESIAN_POINT ( 'NONE',  ( 1.000000000000003553, 6.400000000000022560, 1.214306433183764966E-14 ) ) ;
#44295 = CARTESIAN_POINT ( 'NONE',  ( 6.182236774357948050, -0.9162642880373177423, 1.461205601097197659 ) ) ;
#44296 = CARTESIAN_POINT ( 'NONE',  ( -6.573005544526917099, 6.562927978236513304, -0.7998128361456291469 ) ) ;
#44297 = CARTESIAN_POINT ( 'NONE',  ( 1.511953044659793077, -1.632839461445406481, 0.5843666143663208690 ) ) ;
#44298 = CARTESIAN_POINT ( 'NONE',  ( -0.4480869943418438472, 14.55305228462710687, 11.95586206503659277 ) ) ;
#44299 = DIRECTION ( 'NONE',  ( -1.000000000000000000, 0.000000000000000000, 0.000000000000000000 ) ) ;
#44300 = PRESENTATION_LAYER_ASSIGNMENT (  '', '', ( #137691 ) ) ;
#44301 = CARTESIAN_POINT ( 'NONE',  ( 5.331008558256671748, -2.041869270619638854, -0.7380826535893101337 ) ) ;
#44302 = CARTESIAN_POINT ( 'NONE',  ( 4.336427269025699971, 1.790907886515300085, 0.3537760332646966432 ) ) ;
#44303 = CARTESIAN_POINT ( 'NONE',  ( 2.237090426018002454, -0.09115598566783281176, -1.959741687340324168 ) ) ;
#44304 = CARTESIAN_POINT ( 'NONE',  ( 0.6325982246286944166, 0.6188553777890459795, 2.024753282845246805 ) ) ;
#44305 = LINE ( 'NONE', #190524, #68209 ) ;
#44306 = CARTESIAN_POINT ( 'NONE',  ( 7.588813295347141441, 9.876701482703580837, -1.599625672291262513 ) ) ;
#44307 = CARTESIAN_POINT ( 'NONE',  ( 2.403126630736720948, -0.3650820022202577175, -2.088671427859823293 ) ) ;
#44308 = CARTESIAN_POINT ( 'NONE',  ( -3.795919822146293754, 4.491289883001181593, -1.082531754730549967 ) ) ;
#44309 = SPHERICAL_SURFACE ( 'NONE', #142847, 0.08000000000000000167 ) ;
#44310 = CARTESIAN_POINT ( 'NONE',  ( -5.251027302601237956, 6.428042375187708934, -1.158707231040608576 ) ) ;
#44311 = AXIS2_PLACEMENT_3D ( 'NONE', #29922, #96005, #75465 ) ;
#44312 = CARTESIAN_POINT ( 'NONE',  ( 0.4970418144054839504, 0.3504251219754518365, 2.040211723117946629 ) ) ;
#44314 = CARTESIAN_POINT ( 'NONE',  ( -1.402160292154681736E-14, 14.09375000068279959, 1.732050807568881190 ) ) ;
#44313 = CARTESIAN_POINT ( 'NONE',  ( -10.19206596916605001, 3.593463588655721797, 6.350353714858171017 ) ) ;
#44316 = ORIENTED_EDGE ( 'NONE', *, *, #153335, .F. ) ;
#44315 = CARTESIAN_POINT ( 'NONE',  ( 3.018465837578692579, -2.218647833171137673, 0.1111532960578337226 ) ) ;
#44317 = CARTESIAN_POINT ( 'NONE',  ( 0.6515572338587878320, 1.139979866233470807, 1.996073129511093169 ) ) ;
#44319 = CARTESIAN_POINT ( 'NONE',  ( 5.805554948619430000, -1.622591123950654746, -1.273203187973567241 ) ) ;
#44318 = CARTESIAN_POINT ( 'NONE',  ( 4.369805582306193870, 3.992528022312320957, 1.214306433183764966E-14 ) ) ;
#44321 = CARTESIAN_POINT ( 'NONE',  ( -1.737500000000000266, -2.508333333333334636, -3.009438278150923907 ) ) ;
#44320 = CARTESIAN_POINT ( 'NONE',  ( 3.770049233051776749, 6.556085317605844232, 1.199719254218451159 ) ) ;
#44322 = CARTESIAN_POINT ( 'NONE',  ( 0.2333540202161402677, 0.7093705336200817335, -2.128223931541360248 ) ) ;
#44323 = CARTESIAN_POINT ( 'NONE',  ( 5.425302022954732628, -1.172690680311109901, -1.419496581506813904 ) ) ;
#44324 = DIRECTION ( 'NONE',  ( 0.000000000000000000, 1.000000000000000000, 0.000000000000000000 ) ) ;
#44325 = CARTESIAN_POINT ( 'NONE',  ( 3.167801447087334576, 6.847518788243868393, -0.7998128361456291469 ) ) ;
#44326 = CARTESIAN_POINT ( 'NONE',  ( -0.1106727585416019261, 4.087503477334416324, -2.558207815289376796 ) ) ;
#44327 = CARTESIAN_POINT ( 'NONE',  ( 2.449869591326372387, 1.724352457016034457, 0.04528501180301596624 ) ) ;
#44328 = CARTESIAN_POINT ( 'NONE',  ( 1.446500318503376903, -1.422605717829699579, 1.429450658469958446 ) ) ;
#44329 = CARTESIAN_POINT ( 'NONE',  ( 3.059543388688467314, -1.367113599135186819, 1.847867383329027335 ) ) ;
#44330 = CARTESIAN_POINT ( 'NONE',  ( 2.900009951539525677, -0.7123764238676842941, 2.147366075387107553 ) ) ;
#44331 = CARTESIAN_POINT ( 'NONE',  ( 5.479168138989118475, -0.05037515785718051087, -2.105640702651077945 ) ) ;
#44332 = CARTESIAN_POINT ( 'NONE',  ( -6.455090533882201775, 8.624301270986276080, -1.443375672974066548 ) ) ;
#44333 = CARTESIAN_POINT ( 'NONE',  ( 3.391635040236582022, -0.7200671834438672203, 1.616821809559340517 ) ) ;
#44335 = CARTESIAN_POINT ( 'NONE',  ( 6.040627043210095692, -1.938779113641406759, 1.222911669862235096 ) ) ;
#44334 = CARTESIAN_POINT ( 'NONE',  ( 5.031484404002889654, 6.003058238492422483, 1.082531754730549078 ) ) ;
#44336 = CARTESIAN_POINT ( 'NONE',  ( 4.540845788227630742, -1.424921066559198257, -1.165926479108070346 ) ) ;
#44338 = EDGE_CURVE ( 'NONE', #18903, #80718, #28440, .T. ) ;
#44337 = CARTESIAN_POINT ( 'NONE',  ( -6.112028321662274166, 6.025121218227761588, 0.7998128361456341429 ) ) ;
#44339 = CARTESIAN_POINT ( 'NONE',  ( 4.921246571636183731, 7.724909519342112674, -1.082531754730549078 ) ) ;
#44340 = CARTESIAN_POINT ( 'NONE',  ( -1.201851678989727383E-14, 3.712500000000020339, 1.732050807568877637 ) ) ;
#44341 = CARTESIAN_POINT ( 'NONE',  ( 4.927760762764835434, 1.128268568998530563, -1.878541326455762661 ) ) ;
#44342 = CARTESIAN_POINT ( 'NONE',  ( -3.262708522383007903, 6.958243709422141876, 1.040834085586084257E-14 ) ) ;
#44343 = CARTESIAN_POINT ( 'NONE',  ( -1.420000000000056550, 7.240846818246208905, -4.154462424328208670 ) ) ;
#44344 = CARTESIAN_POINT ( 'NONE',  ( 5.248515149483167441, -2.054309126314420642, -0.2569322651706855143 ) ) ;
#44345 = CARTESIAN_POINT ( 'NONE',  ( 0.1105650446291406575, 1.931126588553159884, 0.5807481968119408977 ) ) ;
#44346 = CARTESIAN_POINT ( 'NONE',  ( -0.6823417656249969321, 4.467708333674755394, -1.181850606188749264 ) ) ;
#44347 = CARTESIAN_POINT ( 'NONE',  ( 3.211465258343335627, -0.3752234067680487728, 1.889445157240315254 ) ) ;
#44348 = CARTESIAN_POINT ( 'NONE',  ( -1.364683531250014514, 9.588541667008064096, -0.7879004041258335089 ) ) ;
#44349 = CARTESIAN_POINT ( 'NONE',  ( -4.148431816101615155, 3.942184661647709198, 0.7216878364870317197 ) ) ;
#44350 = CARTESIAN_POINT ( 'NONE',  ( 0.4576791451081770323, -1.901157720872756141, 1.148870853762502753 ) ) ;
#44351 = EDGE_LOOP ( 'NONE', ( #161068, #92613, #74337, #163655 ) ) ;
#44353 = DIRECTION ( 'NONE',  ( -1.000000000000000000, 0.000000000000000000, 3.491481338843133355E-15 ) ) ;
#44352 = CARTESIAN_POINT ( 'NONE',  ( -4.990809943606294929, 4.995235487061662205, -0.7216878364870338292 ) ) ;
#44354 = CARTESIAN_POINT ( 'NONE',  ( 3.032219910950674890, 6.689340329417765574, 0.7998128361456321445 ) ) ;
#44355 = CARTESIAN_POINT ( 'NONE',  ( 3.929058411375439874, 6.499999999999999112, 0.7500000000000006661 ) ) ;
#44356 = UNCERTAINTY_MEASURE_WITH_UNIT (LENGTH_MEASURE( 1.000000000000000082E-05 ), #30136, 'distance_accuracy_value', 'NONE');
#44357 = CYLINDRICAL_SURFACE ( 'NONE', #130625, 0.4000000000000001332 ) ;
#44358 = PLANE ( 'NONE',  #151465 ) ;
#44360 = CARTESIAN_POINT ( 'NONE',  ( 1.258172656280614365, -1.962046632281065461, -0.003472340283867945618 ) ) ;
#44359 = CIRCLE ( 'NONE', #127469, 4.000000000000000000 ) ;
#44361 = CARTESIAN_POINT ( 'NONE',  ( -1.402160292154681736E-14, 0.7593750003414168059, -1.575800808251659024 ) ) ;
#44362 = CARTESIAN_POINT ( 'NONE',  ( 6.526263005029544928, 1.249015235541932167, -1.764162671312206498 ) ) ;
#44363 = CARTESIAN_POINT ( 'NONE',  ( 5.547302793442128177, 1.730978599593002043, -0.9233319674036490898 ) ) ;
#44364 = CARTESIAN_POINT ( 'NONE',  ( -9.982881178363895103, 10.54111621771303753, 1.040834085586084257E-14 ) ) ;
#44365 = CARTESIAN_POINT ( 'NONE',  ( -4.080641047588902559, 7.704572288921609058, -0.7216878364870257245 ) ) ;
#44366 = CARTESIAN_POINT ( 'NONE',  ( 6.192270064542984898, -2.150811787302907785, -0.2168040374768212541 ) ) ;
#44368 = ORIENTED_EDGE ( 'NONE', *, *, #171086, .F. ) ;
#44367 = CARTESIAN_POINT ( 'NONE',  ( -0.008494835128554827433, -5.601932402265138222, -11.00038526257045390 ) ) ;
#44369 = CARTESIAN_POINT ( 'NONE',  ( -0.6823417656249969321, 4.717708333674755394, -1.181850606188749264 ) ) ;
#44370 = CARTESIAN_POINT ( 'NONE',  ( 6.626250064558294461, 1.136881752820615432, -1.610320780329032253 ) ) ;
#44371 = CARTESIAN_POINT ( 'NONE',  ( 6.151638658550825589, -0.2577636348817541334, -1.714396880517143451 ) ) ;
#44373 = CARTESIAN_POINT ( 'NONE',  ( 2.542740116143254792, -1.820367712357463974, 1.220030464664762393 ) ) ;
#44372 = CARTESIAN_POINT ( 'NONE',  ( 1.360316468749969809, 0.7447916670080856338, 0.7853790794158741484 ) ) ;
#44374 = CARTESIAN_POINT ( 'NONE',  ( 4.454349891636342207, 2.307156057683857675, -0.05211387993751984832 ) ) ;
#44375 = CARTESIAN_POINT ( 'NONE',  ( 5.800091581907264704, -2.060967560761736372, -0.004405934171711199318 ) ) ;
#44376 = CARTESIAN_POINT ( 'NONE',  ( 0.7966981359470609592, 1.587242811699969725, 1.118599961973030021 ) ) ;
#44377 = CARTESIAN_POINT ( 'NONE',  ( -6.534666851662457532, 6.726125536468730459, 1.040834085586084257E-14 ) ) ;
#44378 = DIRECTION ( 'NONE',  ( 0.000000000000000000, 0.000000000000000000, -1.000000000000000000 ) ) ;
#44379 = CARTESIAN_POINT ( 'NONE',  ( 4.623349522974431025, 1.846400237221163865, 1.042759738753673338 ) ) ;
#44380 = SURFACE_SIDE_STYLE ('',( #192726 ) ) ;
#44381 = CARTESIAN_POINT ( 'NONE',  ( 2.022111496571117772, -1.799922141918413487, 0.9091460122201827643 ) ) ;
#44382 = CARTESIAN_POINT ( 'NONE',  ( -7.022760381754429737, 7.295567988242705582, 1.040834085586084257E-14 ) ) ;
#44383 = CARTESIAN_POINT ( 'NONE',  ( 5.737410212107617369, -1.997324651315037780, 0.9386623957203032997 ) ) ;
#44384 = CARTESIAN_POINT ( 'NONE',  ( 4.787437623848783907, 6.678706240755900581, -1.249999999999999334 ) ) ;
#44386 =( BOUNDED_CURVE ( )  B_SPLINE_CURVE ( 2, ( #128057, #45663, #113919, #110710, #147419, #94419, #160458 ),
 .UNSPECIFIED., .F., .F. ) 
 B_SPLINE_CURVE_WITH_KNOTS ( ( 3, 2, 2, 3 ),
 ( 0.1999999999999999556, 0.2041666666666666630, 0.2083333333333333981, 0.2125000000000001055 ),
 .UNSPECIFIED. ) 
 CURVE ( )  GEOMETRIC_REPRESENTATION_ITEM ( )  RATIONAL_B_SPLINE_CURVE ( ( 1.000000000000001776, 0.8660254037844369313, 1.000000000000000000, 0.8660254037844387076, 1.000000000000000000, 0.8660254037844351549, 1.000000000000003553 ) ) 
 REPRESENTATION_ITEM ( '' )  );
#44385 = CARTESIAN_POINT ( 'NONE',  ( -2.703472480837374903, -3.106478463707009308, -2.089468915991812725 ) ) ;
#44387 = CARTESIAN_POINT ( 'NONE',  ( 0.1174333910212103232, -1.791171220025630895, 0.3524246893974944395 ) ) ;
#44388 = FACE_OUTER_BOUND ( 'NONE', #193933, .T. ) ;
#44390 = CARTESIAN_POINT ( 'NONE',  ( 5.341549334104194635, 6.294524313618772737, 1.082531754730558626 ) ) ;
#44389 = CARTESIAN_POINT ( 'NONE',  ( -4.986341270546564175, 8.046800470007955397, 1.126807992560383331 ) ) ;
#44391 = CARTESIAN_POINT ( 'NONE',  ( -9.348561386651960348, 4.000000000000000888, 7.001914024036569373 ) ) ;
#44392 = ORIENTED_EDGE ( 'NONE', *, *, #38423, .F. ) ;
#44393 = CARTESIAN_POINT ( 'NONE',  ( 5.137599278355773791, -1.455842209265911569, -1.458961989641535117 ) ) ;
#44394 = CARTESIAN_POINT ( 'NONE',  ( 6.966220764712121927, 6.002124920821316323, 2.420000000000000373 ) ) ;
#44395 = FACE_OUTER_BOUND ( 'NONE', #51476, .T. ) ;
#44396 = CARTESIAN_POINT ( 'NONE',  ( -3.079673448598517549, 6.744702790006905424, 1.040834085586084257E-14 ) ) ;
#44397 = CARTESIAN_POINT ( 'NONE',  ( -5.015590482412729756, 4.816220082428420923, 0.000000000000000000 ) ) ;
#44398 = CARTESIAN_POINT ( 'NONE',  ( 4.776038667982859032, 1.997392889608617716, -0.2983725866285909523 ) ) ;
#44400 = EDGE_LOOP ( 'NONE', ( #102833, #3199, #16383, #206716 ) ) ;
#44399 = CARTESIAN_POINT ( 'NONE',  ( 0.7499999999999885647, 0.8166666666666877461, -1.299038105676652899 ) ) ;
#44401 = AXIS2_PLACEMENT_3D ( 'NONE', #210910, #46312, #128699 ) ;
#44403 = CARTESIAN_POINT ( 'NONE',  ( 8.242994207428692377, 12.56065097540143327, -0.7216878364870328300 ) ) ;
#44402 = CARTESIAN_POINT ( 'NONE',  ( -5.815521545619021460, 5.749472989502435460, -0.7998128361456362523 ) ) ;
#44404 = CARTESIAN_POINT ( 'NONE',  ( 7.969495366734495434, 8.192166104145387706, 1.040834085586084257E-14 ) ) ;
#44405 = CARTESIAN_POINT ( 'NONE',  ( 4.610263661134276880, -0.8792652907330700263, -1.864042625929088759 ) ) ;
#44406 = CARTESIAN_POINT ( 'NONE',  ( 3.164685561777963230, 1.281361203394768111, 1.556908733426412450 ) ) ;
#44407 = ORIENTED_EDGE ( 'NONE', *, *, #58668, .F. ) ;
#44408 = CARTESIAN_POINT ( 'NONE',  ( 6.727182134110178069, 2.947419669445831669, 2.641212418657997496 ) ) ;
#44409 = CARTESIAN_POINT ( 'NONE',  ( 4.059776932288224671, 6.823824623389866950, 1.199719254218462483 ) ) ;
#44410 = CARTESIAN_POINT ( 'NONE',  ( 3.221888912838869690, 0.9023448338944944913, -1.803416113280359445 ) ) ;
#44412 = ORIENTED_EDGE ( 'NONE', *, *, #48185, .T. ) ;
#44411 = CARTESIAN_POINT ( 'NONE',  ( -0.5473748313345772054, 7.493086169160624976, -1.923660786605011497 ) ) ;
#44413 = CARTESIAN_POINT ( 'NONE',  ( 2.899767358622063806, 0.2439914025648345919, 2.001204936777578602 ) ) ;
#44414 = CARTESIAN_POINT ( 'NONE',  ( 2.167674216824653222, -1.133089441918342599, 1.451089449600144521 ) ) ;
#44415 = CARTESIAN_POINT ( 'NONE',  ( 1.471738413253330879, 0.1659702479998256264, -2.301786031945464828 ) ) ;
#44416 = CARTESIAN_POINT ( 'NONE',  ( 3.725458348705031231, 7.568394850123006279, -1.734723475976807094E-15 ) ) ;
#44417 = CARTESIAN_POINT ( 'NONE',  ( 2.794378387653595475, -2.155598273342887339, -0.1620501260681943834 ) ) ;
#44418 = CARTESIAN_POINT ( 'NONE',  ( 7.587759525142423911, 12.00413654597487501, 0.7998128361456462443 ) ) ;
#44419 = STYLED_ITEM ( 'NONE', ( #175518 ), #34286 ) ;
#44420 = CARTESIAN_POINT ( 'NONE',  ( -4.740547266272593596, 8.682388910626682943, -0.7998128361456281477 ) ) ;
#44421 = EDGE_CURVE ( 'NONE', #161718, #204270, #68492, .T. ) ;
#44422 = ORIENTED_EDGE ( 'NONE', *, *, #138594, .T. ) ;
#44423 = LINE ( 'NONE', #56392, #49293 ) ;
#44424 = CARTESIAN_POINT ( 'NONE',  ( 1.674454752297813265, -1.775319108138155633, -0.5897529795871117031 ) ) ;
#44425 = CARTESIAN_POINT ( 'NONE',  ( 5.700065208342940615, -1.971640594297157989, -0.0006100080248323812597 ) ) ;
#44427 = CARTESIAN_POINT ( 'NONE',  ( 7.849807752188022292, 11.14156422998596696, -1.082531754730543083 ) ) ;
#44426 = CARTESIAN_POINT ( 'NONE',  ( 1.364683531249988535, 3.405208333674749621, -0.7879004041258239610 ) ) ;
#44429 = CARTESIAN_POINT ( 'NONE',  ( 0.1005910224048736229, -2.206496634663042133, -0.04943112074598519229 ) ) ;
#44428 = CARTESIAN_POINT ( 'NONE',  ( -7.739006755302186846, 7.923262724141010516, 0.7998128361456462443 ) ) ;
#44430 = FACE_OUTER_BOUND ( 'NONE', #52390, .T. ) ;
#44431 = CARTESIAN_POINT ( 'NONE',  ( 4.981731378017507872, 7.899438143407371271, -1.199719254218452047 ) ) ;
#44432 = CARTESIAN_POINT ( 'NONE',  ( -6.112028321662274166, 6.025121218227761588, 0.7998128361456341429 ) ) ;
#44433 = CARTESIAN_POINT ( 'NONE',  ( -0.3046331935817688241, -6.606549254264993287, -9.611339018008544954 ) ) ;
#44434 = CARTESIAN_POINT ( 'NONE',  ( 5.190288350601474754, -1.956472792631309909, -0.2422539641438857527 ) ) ;
#44435 = CARTESIAN_POINT ( 'NONE',  ( 6.486581104273712484, -1.239329707167437622, 1.595369898402546838 ) ) ;
#44436 = CARTESIAN_POINT ( 'NONE',  ( 1.499999999999987121, 1.035416667349484232, 0.8660254037844524744 ) ) ;
#44437 = CARTESIAN_POINT ( 'NONE',  ( 4.354349988907435964, 2.307223249097400064, -0.05412331456603951957 ) ) ;
#44438 = CARTESIAN_POINT ( 'NONE',  ( 1.955997896808071568, -0.6987562721488985717, 1.940702610317937671 ) ) ;
#44439 = CARTESIAN_POINT ( 'NONE',  ( 7.998947442382716488, 9.394822106610419610, -1.082531754730543083 ) ) ;
#44440 = CARTESIAN_POINT ( 'NONE',  ( 5.448397627845284141, 7.449826213943242514, 1.599625672291268286 ) ) ;
#44441 = CARTESIAN_POINT ( 'NONE',  ( 5.598591087800349086, 5.496387455380669529, -0.7998128361456481317 ) ) ;
#44442 = CARTESIAN_POINT ( 'NONE',  ( -1.402160292154681736E-14, 2.259375000341416140, -1.575800808251660134 ) ) ;
#44443 = CARTESIAN_POINT ( 'NONE',  ( -0.7589079839483203749, 14.55289787277384583, 11.96588861122574521 ) ) ;
#44444 = CARTESIAN_POINT ( 'NONE',  ( 6.453317929980448397, 6.631218461173066459, 1.040834085586084257E-14 ) ) ;
#44445 = CARTESIAN_POINT ( 'NONE',  ( 5.125502745298136098, 0.2179265861129157655, -2.160231653469760982 ) ) ;
#44446 = CYLINDRICAL_SURFACE ( 'NONE', #58221, 1.250000000000000000 ) ;
#44448 = CARTESIAN_POINT ( 'NONE',  ( 4.458453498679889826, -1.646799808365447149, -0.8236825204945982248 ) ) ;
#44447 = CARTESIAN_POINT ( 'NONE',  ( -2.982430605326321427, 6.423326772948587227, -0.7216878364870267237 ) ) ;
#44450 = CARTESIAN_POINT ( 'NONE',  ( 0.000000000000000000, 2.999999999999999112, -10.25000000000000000 ) ) ;
#44449 = DIRECTION ( 'NONE',  ( 8.881784197001252323E-15, 0.000000000000000000, -1.000000000000000000 ) ) ;
#44451 = CARTESIAN_POINT ( 'NONE',  ( 5.952700804540857149, -1.878875186057769486, -1.127905468421293689 ) ) ;
#44452 = CARTESIAN_POINT ( 'NONE',  ( 1.224999999999947020, 0.1666666673495328932, 0.7072540797572737237 ) ) ;
#44453 = CARTESIAN_POINT ( 'NONE',  ( 6.192268726830573833, -2.250890937568471362, -0.2291988078206678991 ) ) ;
#44454 = ADVANCED_FACE ( 'NONE', ( #82506 ), #81458, .T. ) ;
#44455 = CARTESIAN_POINT ( 'NONE',  ( -4.038103646828244742, 7.764432012698684105, 0.5462726908427618655 ) ) ;
#44456 = DIRECTION ( 'NONE',  ( 0.000000000000000000, 0.000000000000000000, 1.000000000000000000 ) ) ;
#44457 = CARTESIAN_POINT ( 'NONE',  ( 4.749341595749815070, 8.305088035112140332, 0.7662636247844747395 ) ) ;
#44458 = CARTESIAN_POINT ( 'NONE',  ( -4.380693030546956912, 6.204170850428461392, 1.443375672974065660 ) ) ;
#44459 = CARTESIAN_POINT ( 'NONE',  ( 4.014622883422321209, 5.777089012116397804, -1.443375672974068769 ) ) ;
#44460 = CARTESIAN_POINT ( 'NONE',  ( 1.129378208368720271, -1.118813933885588474, -1.371354111526525754 ) ) ;
#44462 = CARTESIAN_POINT ( 'NONE',  ( 4.986981296356192139, -1.896340117422308236, -0.6759883393069978652 ) ) ;
#44461 = AXIS2_PLACEMENT_3D ( 'NONE', #23750, #74649, #89854 ) ;
#44463 = CARTESIAN_POINT ( 'NONE',  ( 6.388916700537700777, 8.476822122092563916, 1.599625672291281386 ) ) ;
#44464 = CARTESIAN_POINT ( 'NONE',  ( 4.454198790814194453, 2.105553956100237656, -0.04914431425445846269 ) ) ;
#44465 = CARTESIAN_POINT ( 'NONE',  ( 2.565921762024740982, -0.9824477935329900546, 1.644319621262643638 ) ) ;
#44466 = CARTESIAN_POINT ( 'NONE',  ( 2.846322183865124700, 5.408127416896231665, -1.199719254218446718 ) ) ;
#44467 = CARTESIAN_POINT ( 'NONE',  ( 3.033609518001907368, 1.871031307821906964, -0.6153852250644732402 ) ) ;
#44468 = CARTESIAN_POINT ( 'NONE',  ( 5.326427914677607234, -0.9117507067677769195, -1.802394291917883473 ) ) ;
#44469 = CARTESIAN_POINT ( 'NONE',  ( 1.270139834521961886, -1.189467451172643964, 1.443775233441677130 ) ) ;
#44472 = ORIENTED_EDGE ( 'NONE', *, *, #76253, .T. ) ;
#44471 = CARTESIAN_POINT ( 'NONE',  ( 1.195406425308798148, 1.765864799226088744, -0.7346160280939582066 ) ) ;
#44470 = CARTESIAN_POINT ( 'NONE',  ( 5.285687151129126349, 1.162661966624499277, 1.274325963116212934 ) ) ;
#44474 = CARTESIAN_POINT ( 'NONE',  ( 5.016153647376212277, 5.914896012436124728, 1.082531754730558626 ) ) ;
#44473 = CARTESIAN_POINT ( 'NONE',  ( 0.8388348947251201837, 2.174866457552121268, 0.3736606161612308630 ) ) ;
#44475 = CARTESIAN_POINT ( 'NONE',  ( -1.364683531250012516, 2.301041667008087988, -0.7879004041258289570 ) ) ;
#44476 = CARTESIAN_POINT ( 'NONE',  ( 7.588813295347141441, 9.876701482703580837, -1.599625672291262513 ) ) ;
#44477 = CARTESIAN_POINT ( 'NONE',  ( 6.614126560844452385, -0.8839695271746010885, -1.648598838400926692 ) ) ;
#44478 = DIRECTION ( 'NONE',  ( 7.993605777301127091E-15, 0.000000000000000000, 1.000000000000000000 ) ) ;
#44479 = DIRECTION ( 'NONE',  ( 3.330669073875479482E-16, -3.330669073875479482E-16, -1.000000000000000000 ) ) ;
#44480 = CARTESIAN_POINT ( 'NONE',  ( -1.333477130264982158, 8.249568609204956715, 9.911050286642574036 ) ) ;
#44481 = AXIS2_PLACEMENT_3D ( 'NONE', #153401, #39647, #168575 ) ;
#44482 = ORIENTED_EDGE ( 'NONE', *, *, #67908, .F. ) ;
#44483 = CARTESIAN_POINT ( 'NONE',  ( 1.574760213118006735, 1.391939136705011348, -1.532762857463897843 ) ) ;
#44484 = CARTESIAN_POINT ( 'NONE',  ( 0.7499999999999902300, 3.483333333333352044, 1.299038105676669330 ) ) ;
#44485 = CARTESIAN_POINT ( 'NONE',  ( 5.799137018343234473, 7.788745826199009237, -1.599625672291262513 ) ) ;
#44486 = CARTESIAN_POINT ( 'NONE',  ( -6.852756576703439961, 10.08230087520760954, 1.199719254218453823 ) ) ;
#44487 = CARTESIAN_POINT ( 'NONE',  ( 3.878514461961128479, 6.682628084666728085, -1.199719254218448494 ) ) ;
#44488 = CARTESIAN_POINT ( 'NONE',  ( -0.09308815784560355022, -0.4424663830696302091, -1.977475021732390204 ) ) ;
#44489 = CARTESIAN_POINT ( 'NONE',  ( 0.000000000000000000, 0.000000000000000000, 0.000000000000000000 ) ) ;
#44490 = CARTESIAN_POINT ( 'NONE',  ( -1.364683531249997417, 3.009375000341422801, 1.214306433183764966E-14 ) ) ;
#44491 = EDGE_CURVE ( 'NONE', #194227, #3320, #125205, .T. ) ;
#44493 = CARTESIAN_POINT ( 'NONE',  ( 3.440018289565364817, 5.036440642624797626, 1.599625672291267398 ) ) ;
#44492 = CARTESIAN_POINT ( 'NONE',  ( 1.220146605508150803E-14, 11.68749999999999822, -1.499999999999998446 ) ) ;
#44494 = CARTESIAN_POINT ( 'NONE',  ( 4.710314442360476583, -1.556670644073439913, -1.281164596596932936 ) ) ;
#44495 = CARTESIAN_POINT ( 'NONE',  ( 4.505048170306029220, -0.08773398713153966744, 1.913818227509517023 ) ) ;
#44496 = SURFACE_SIDE_STYLE ('',( #59654 ) ) ;
#44497 = CARTESIAN_POINT ( 'NONE',  ( 2.419692422129790632, -1.264489869534379141, -1.789777738334753732 ) ) ;
#44498 = CARTESIAN_POINT ( 'NONE',  ( 0.1335669894368864130, 4.084991946249068029, -2.708374394877795410 ) ) ;
#44499 = CARTESIAN_POINT ( 'NONE',  ( 0.7499999999999885647, 0.5979166673494851203, -1.299038105676652899 ) ) ;
#44500 = CARTESIAN_POINT ( 'NONE',  ( 5.748296788003684377, 0.9886478197097836595, -1.753632158501418514 ) ) ;
#44501 = CARTESIAN_POINT ( 'NONE',  ( -5.181187258716735577, 9.196468901811520880, 0.7998128361456481317 ) ) ;
#44503 = CARTESIAN_POINT ( 'NONE',  ( 6.398082464950202386, -0.9982666083749867081, -1.867140504451180183 ) ) ;
#44502 = CARTESIAN_POINT ( 'NONE',  ( -4.175548123328963079, 4.934189567714277302, 1.082531754730560403 ) ) ;
#44504 = CARTESIAN_POINT ( 'NONE',  ( 0.6823417656249969321, 9.338541667008065872, -1.181850606188757036 ) ) ;
#44506 = CARTESIAN_POINT ( 'NONE',  ( -6.526270840131767059, 8.707344961610770540, -1.599625672291271394 ) ) ;
#44505 = CARTESIAN_POINT ( 'NONE',  ( 3.175413592762990067, 1.328342846777453845, 1.614508523670985740 ) ) ;
#44508 = ORIENTED_EDGE ( 'NONE', *, *, #118916, .F. ) ;
#44507 = CARTESIAN_POINT ( 'NONE',  ( 2.080655396751258213, -0.08067463971387846267, -1.723007254337567407 ) ) ;
#44509 = CARTESIAN_POINT ( 'NONE',  ( 6.117454236943913770, 1.763945953808215394, 1.176740244630887222 ) ) ;
#44510 = CARTESIAN_POINT ( 'NONE',  ( 6.322179702674084467, 6.270297829408224111, 1.040834085586084257E-14 ) ) ;
#44511 = CARTESIAN_POINT ( 'NONE',  ( -1.420000000000001039, 6.280000000000042881, -2.873333333333329520 ) ) ;
#44512 = CARTESIAN_POINT ( 'NONE',  ( 7.470306724221089212, -6.701288531903148993, 8.074422843255659288 ) ) ;
#44513 = CARTESIAN_POINT ( 'NONE',  ( 0.000000000000000000, -9.746166700180788567, 9.579665964948883783 ) ) ;
#44514 = CARTESIAN_POINT ( 'NONE',  ( 4.984594031318565932, 8.967110136513669616, 0.7998128361456462443 ) ) ;
#44515 = ORIENTED_EDGE ( 'NONE', *, *, #24434, .F. ) ;
#44516 = DIRECTION ( 'NONE',  ( -1.776356839400250465E-15, 0.000000000000000000, 1.000000000000000000 ) ) ;
#44517 = CARTESIAN_POINT ( 'NONE',  ( 3.211360534488953977, 1.429591190403207035, 1.112411576641762379 ) ) ;
#44518 = CARTESIAN_POINT ( 'NONE',  ( -6.663996196316808174, 7.733415969579778171, -1.199719254218446718 ) ) ;
#44519 = CARTESIAN_POINT ( 'NONE',  ( 3.704402285031850539, 5.344888637335695414, -1.599625672291262513 ) ) ;
#44520 = ORIENTED_EDGE ( 'NONE', *, *, #110772, .F. ) ;
#44521 = CARTESIAN_POINT ( 'NONE',  ( 5.682802662783380754, 6.658966523782627434, 1.199719254218452935 ) ) ;
#44522 = CARTESIAN_POINT ( 'NONE',  ( 3.017991377792153429, -1.809312282836759378, 0.09115427604276456208 ) ) ;
#44523 = CARTESIAN_POINT ( 'NONE',  ( 6.639320575229294086, 0.5800432152290584398, 2.049144803211971233 ) ) ;
#44524 = DIRECTION ( 'NONE',  ( 0.6507913734559640506, -0.7592566023653004592, 0.000000000000000000 ) ) ;
#44525 = CARTESIAN_POINT ( 'NONE',  ( 4.574835874639041400, 6.943354005153362429, 1.191215277921169324 ) ) ;
#44526 = CARTESIAN_POINT ( 'NONE',  ( 3.613571450151699782, 0.4543224947703514149, -1.804596983994880333 ) ) ;
#44527 = CARTESIAN_POINT ( 'NONE',  ( 1.177184062793021679, 1.451467631357589383, 1.250241458713635456 ) ) ;
#44528 = CARTESIAN_POINT ( 'NONE',  ( 0.9733497034139363402, 1.760643049788807257, -0.4823509818385819936 ) ) ;
#44529 = CARTESIAN_POINT ( 'NONE',  ( 4.848511436970775357, 8.075560130489554567, 0.9049096096846224180 ) ) ;
#44530 = DIRECTION ( 'NONE',  ( 0.000000000000000000, 1.000000000000000000, 0.000000000000000000 ) ) ;
#44531 = CARTESIAN_POINT ( 'NONE',  ( 5.825676364550436581, 7.207913871576331566, 1.168708750232345883 ) ) ;
#44532 = CARTESIAN_POINT ( 'NONE',  ( -11.52888687719600647, 9.805768748949601488, 3.331331986263579736 ) ) ;
#44533 = CARTESIAN_POINT ( 'NONE',  ( -2.467220768007014176, 5.822248629409386922, 0.7216878364870317197 ) ) ;
#44534 = CARTESIAN_POINT ( 'NONE',  ( 7.619319141200063150, 9.912291636198670375, 1.443375672974076540 ) ) ;
#44535 = CARTESIAN_POINT ( 'NONE',  ( 5.682459527512692787, 1.176241607570350567, -1.579419126353029279 ) ) ;
#44536 = ADVANCED_FACE ( 'NONE', ( #63071 ), #78948, .T. ) ;
#44537 = CARTESIAN_POINT ( 'NONE',  ( 2.518767860054324625, 0.2516336668320385828, 2.000731427934741902 ) ) ;
#44538 = CARTESIAN_POINT ( 'NONE',  ( -4.660252114795309097, 6.460046772059735432, -1.599625672291256295 ) ) ;
#44539 = CARTESIAN_POINT ( 'NONE',  ( -0.3384797366876900471, 6.551676121695759747, 3.195407356336833260 ) ) ;
#44540 = CARTESIAN_POINT ( 'NONE',  ( 0.1114262914704557683, -2.049844763593706265, 0.4100319678014376912 ) ) ;
#44541 = CARTESIAN_POINT ( 'NONE',  ( 8.769426429940780920, 9.125419011219408461, 0.7998128361456462443 ) ) ;
#44542 = CARTESIAN_POINT ( 'NONE',  ( 4.928697230495170167, 1.843396615675118699, 0.5593075106890015302 ) ) ;
#44543 = CARTESIAN_POINT ( 'NONE',  ( -5.636439174979254396, 7.598931675607687453, -1.599625672291256295 ) ) ;
#44544 = ADVANCED_FACE ( 'NONE', ( #94531 ), #160570, .T. ) ;
#44545 = CARTESIAN_POINT ( 'NONE',  ( 1.008509592878764183, 1.385430265305506170, -1.188947219173806413 ) ) ;
#44546 = CARTESIAN_POINT ( 'NONE',  ( 2.332911791115964473, 2.140974936812658935, 0.5348262304398290201 ) ) ;
#44547 = CARTESIAN_POINT ( 'NONE',  ( -6.225321503573748139, 6.939195112795077947, 0.8439093341676749960 ) ) ;
#44548 = CARTESIAN_POINT ( 'NONE',  ( -0.07025823700084612988, -1.875094440630159065, 0.3749275819610526916 ) ) ;
#44549 = CARTESIAN_POINT ( 'NONE',  ( 0.6956774629466413451, -1.390297546174504850, -1.395334862655448260 ) ) ;
#44550 = CARTESIAN_POINT ( 'NONE',  ( 3.157691648149099972, 0.8757969000599256093, 1.733462199761313993 ) ) ;
#44551 = CARTESIAN_POINT ( 'NONE',  ( 0.9661724576192336489, 1.646585359754201061, 1.163093122096101162 ) ) ;
#44553 = CARTESIAN_POINT ( 'NONE',  ( 5.893359673372067675, -1.683065101977880840, 0.7942114673132483205 ) ) ;
#44552 = CARTESIAN_POINT ( 'NONE',  ( -5.550083779947821760, 7.568460058062819407, -1.599625672291271394 ) ) ;
#44554 = CARTESIAN_POINT ( 'NONE',  ( 5.408776937209000657, 5.274937613024121674, 0.7998128361456352531 ) ) ;
#44555 = CARTESIAN_POINT ( 'NONE',  ( 1.416786528094145625, 7.999640415717673037, -11.00953083556808210 ) ) ;
#44556 = CARTESIAN_POINT ( 'NONE',  ( 10.24726517383036928, 10.84956421242393887, 0.000000000000000000 ) ) ;
#44557 = CARTESIAN_POINT ( 'NONE',  ( -4.229253852459088137, 7.021547696922494808, 1.199719254218464037 ) ) ;
#44558 = CARTESIAN_POINT ( 'NONE',  ( -7.910256278930404505, 8.193330178365746619, -0.7998128361456362523 ) ) ;
#44559 = CARTESIAN_POINT ( 'NONE',  ( 1.699035084177059174, 1.824418957995146195, 1.213967346723361596 ) ) ;
#44560 = CARTESIAN_POINT ( 'NONE',  ( 3.958617665510264949, 5.641473247893851628, -1.443375672974051449 ) ) ;
#44561 = AXIS2_PLACEMENT_3D ( 'NONE', #205254, #89415, #73123 ) ;
#44562 = CARTESIAN_POINT ( 'NONE',  ( 7.364013710877980401, 8.620379413226322285, -1.199719254218452047 ) ) ;
#44563 = DIRECTION ( 'NONE',  ( 0.000000000000000000, 0.000000000000000000, -1.000000000000000000 ) ) ;
#44564 = CARTESIAN_POINT ( 'NONE',  ( 2.912524513316586461, 1.322148455168963510, -1.259233298254287536 ) ) ;
#44565 = CARTESIAN_POINT ( 'NONE',  ( -1.408489644590935175, 7.311701683603598845, 4.382268911471428829 ) ) ;
#44567 = EDGE_CURVE ( 'NONE', #209056, #102449, #116968, .T. ) ;
#44566 = CARTESIAN_POINT ( 'NONE',  ( -2.754277761870538299, 6.365074488824250309, 1.040834085586084257E-14 ) ) ;
#44568 = CARTESIAN_POINT ( 'NONE',  ( -5.978723031652583231, 7.198045494411626777, -1.221819409761595088 ) ) ;
#44569 = CARTESIAN_POINT ( 'NONE',  ( 0.1253635393240644380, 7.629137130509072051, -2.744100600304347104 ) ) ;
#44570 = CARTESIAN_POINT ( 'NONE',  ( 9.999301985278609806, 11.62460605670194447, 1.199719254218452047 ) ) ;
#44571 = CARTESIAN_POINT ( 'NONE',  ( 1.260239703848411441, 0.7801416839768731126, 1.761649912542123664 ) ) ;
#44572 = CARTESIAN_POINT ( 'NONE',  ( 5.471523917629521172, -0.2915489554583711729, 1.939870717765689534 ) ) ;
#44573 = AXIS2_PLACEMENT_3D ( 'NONE', #140911, #8729, #156061 ) ;
#44574 = CARTESIAN_POINT ( 'NONE',  ( 1.499999999999997113, 14.64583333333333393, -0.8660254037844378194 ) ) ;
#44575 = CARTESIAN_POINT ( 'NONE',  ( -7.874588291438845644, 8.081441182967111558, -0.7998128361456291469 ) ) ;
#44576 = CARTESIAN_POINT ( 'NONE',  ( 4.822949958159288286, 6.649860922651058992, -1.599625672291256295 ) ) ;
#44577 = CARTESIAN_POINT ( 'NONE',  ( 5.021103811603734535, -2.081066139062941023, 0.6872292908843835590 ) ) ;
#44578 = CARTESIAN_POINT ( 'NONE',  ( 5.196852952739812181, 4.957416621151552683, -0.7998128361456221525 ) ) ;
#44579 = CARTESIAN_POINT ( 'NONE',  ( 4.346580092118113470, -2.046995731385771400, -0.3088174131898810959 ) ) ;
#44581 = CARTESIAN_POINT ( 'NONE',  ( -1.364683531250012516, 0.8427083336747532849, 0.7879004041258379498 ) ) ;
#44580 = PLANE ( 'NONE',  #23568 ) ;
#44582 = ORIENTED_EDGE ( 'NONE', *, *, #34126, .F. ) ;
#44583 = CARTESIAN_POINT ( 'NONE',  ( 4.026267332373588914, -1.999701941076356349, 1.133592428816285080 ) ) ;
#44585 = VERTEX_POINT ( 'NONE', #118281 ) ;
#44584 = CARTESIAN_POINT ( 'NONE',  ( 7.971831135155394321, 8.402817200543854170, -0.7216878364870267237 ) ) ;
#44587 = CARTESIAN_POINT ( 'NONE',  ( 1.001543065824772753E-15, -1.071874999522043792, 3.793834371823811669 ) ) ;
#44586 = CARTESIAN_POINT ( 'NONE',  ( 4.204437034013637664, 6.958908068774287692, -1.082531754730548412 ) ) ;
#44588 = CARTESIAN_POINT ( 'NONE',  ( -9.797178276310326339, 4.534233751442683591, -6.931118765264285386 ) ) ;
#44589 = CARTESIAN_POINT ( 'NONE',  ( 3.626839189636944738, -1.793926730891879151, 0.7440942006126953778 ) ) ;
#44590 = ORIENTED_EDGE ( 'NONE', *, *, #7040, .T. ) ;
#44591 = CARTESIAN_POINT ( 'NONE',  ( 9.422553571373278203, 11.05569592376608945, -1.082531754730543083 ) ) ;
#44592 = CARTESIAN_POINT ( 'NONE',  ( 5.396708386617175890, -1.867154475869851504, -0.4128305108781898936 ) ) ;
#44593 = CARTESIAN_POINT ( 'NONE',  ( 6.598688221398479214, -0.4661808427693337475, -1.660524940999157373 ) ) ;
#44594 = CARTESIAN_POINT ( 'NONE',  ( 4.610564714392807240, 1.931124171932835809, 0.5807562064495259690 ) ) ;
#44595 = DIRECTION ( 'NONE',  ( 0.000000000000000000, 1.000000000000000000, 0.000000000000000000 ) ) ;
#44596 = CARTESIAN_POINT ( 'NONE',  ( 1.313402753022639091, 1.947697196196996217, 1.037691534346518729 ) ) ;
#44598 = CARTESIAN_POINT ( 'NONE',  ( -3.526529353330355221, 6.168015774643768268, -1.082531754730546636 ) ) ;
#44597 = CARTESIAN_POINT ( 'NONE',  ( -9.480175724453545172, 12.08329098332774265, 1.599625672291281386 ) ) ;
#44600 = CARTESIAN_POINT ( 'NONE',  ( 6.503183016764070068, 1.472852356768614479, 0.9808112332466749628 ) ) ;
#44599 = CARTESIAN_POINT ( 'NONE',  ( 1.306708042577527262, 1.844576602789575137, 0.9840055123579400931 ) ) ;
#44601 = CARTESIAN_POINT ( 'NONE',  ( 6.047500043413473136, -1.423963828944514010, 1.427935028000301809 ) ) ;
#44603 = CARTESIAN_POINT ( 'NONE',  ( 2.994356955963250133, -0.6658908676899841783, -2.193406925754942893 ) ) ;
#44602 = CARTESIAN_POINT ( 'NONE',  ( 6.086684617892325733, 6.065829907154645539, -0.7998128361456481317 ) ) ;
#44604 = CARTESIAN_POINT ( 'NONE',  ( 0.6381061630796550643, -1.494939029692418320, 0.8907679528266756463 ) ) ;
#44605 = CARTESIAN_POINT ( 'NONE',  ( 2.566775492539817627, 0.7186216927172992541, 1.995234744298620910 ) ) ;
#44606 = DIRECTION ( 'NONE',  ( 1.224646799147360603E-16, 1.000000000000000000, -8.546850786086437571E-32 ) ) ;
#44607 = CARTESIAN_POINT ( 'NONE',  ( 1.528208422804043121, 1.709223377337875549, -0.2899604983128030722 ) ) ;
#44608 = CARTESIAN_POINT ( 'NONE',  ( -0.6801582343750438575, 0.7135416670080579893, 1.178068619123810334 ) ) ;
#44609 = DIRECTION ( 'NONE',  ( 0.000000000000000000, -1.000000000000000000, 0.000000000000000000 ) ) ;
#44610 = CARTESIAN_POINT ( 'NONE',  ( 1.170657403521972562, -0.9760459728485239017, -1.939464792355448663 ) ) ;
#44611 = CARTESIAN_POINT ( 'NONE',  ( 3.854704076794239764, -1.883312302057647880, -0.7212934815618715634 ) ) ;
#44612 = CARTESIAN_POINT ( 'NONE',  ( 5.250000000000002665, 2.988487650205320908E-13, 2.052068128417942283 ) ) ;
#44613 = CIRCLE ( 'NONE', #165652, 0.08000000000000020983 ) ;
#44614 = CARTESIAN_POINT ( 'NONE',  ( -1.500000000000013101, 1.660416667349487119, -0.8660254037844313801 ) ) ;
#44615 = CARTESIAN_POINT ( 'NONE',  ( 6.393193437440540805, 1.674708767708126045, -0.9521171982297592651 ) ) ;
#44616 = CARTESIAN_POINT ( 'NONE',  ( -0.6823417656250039265, 12.56770833367473017, -1.181850606188755259 ) ) ;
#44617 = CARTESIAN_POINT ( 'NONE',  ( 3.252379014334851437, 0.9957207747773239026, -1.985791214296761087 ) ) ;
#44618 = ORIENTED_EDGE ( 'NONE', *, *, #73601, .F. ) ;
#44619 = CARTESIAN_POINT ( 'NONE',  ( 6.451695228974854146, -8.176248043968833201, 7.005920419302530178 ) ) ;
#44620 = CARTESIAN_POINT ( 'NONE',  ( -0.7500000000000249800, -0.5583333333333134751, 1.299038105676659116 ) ) ;
#44621 = CARTESIAN_POINT ( 'NONE',  ( 8.372323551638698902, 9.726464550788689323, 1.199719254218462483 ) ) ;
#44622 = CARTESIAN_POINT ( 'NONE',  ( -1.364683531250014514, -1.219791666325248602, 0.7879004041258379498 ) ) ;
#44623 = CARTESIAN_POINT ( 'NONE',  ( 0.2043192855987647494, 1.601443664334546213, 0.9084302959305108338 ) ) ;
#44624 = CARTESIAN_POINT ( 'NONE',  ( 4.158614545834369736, -0.6132839004606009947, -1.863630207987923226 ) ) ;
#44626 = CARTESIAN_POINT ( 'NONE',  ( -5.368665641331555882, 8.246898433986675769, 1.082531754730548412 ) ) ;
#44625 = CARTESIAN_POINT ( 'NONE',  ( 2.184835310096557404, 5.700724961754617404, 1.040834085586084257E-14 ) ) ;
#44627 = CARTESIAN_POINT ( 'NONE',  ( -1.500267808745624709, 4.350826524122706651, 0.06648599600051158243 ) ) ;
#44628 = CARTESIAN_POINT ( 'NONE',  ( 6.309908665641647652, -2.246456703917932618, 0.2676860584361096529 ) ) ;
#44629 = CONICAL_SURFACE ( 'NONE', #61457, 10.92874649719719571, 0.04746665426984499059 ) ;
#44630 = CARTESIAN_POINT ( 'NONE',  ( 2.014201374223419272, 2.057289675485386216, -0.1496214851241447485 ) ) ;
#44631 = CARTESIAN_POINT ( 'NONE',  ( -7.019370843573183194, 9.212351955633947043, 1.599625672291283607 ) ) ;
#44632 = B_SPLINE_CURVE_WITH_KNOTS ( 'NONE', 3,
 ( #14588, #34049, #212791, #167265, #64429, #68661, #100122, #130573, #17773, #84934, #196563, #48205, #151023, #31935, #149952, #1521 ),
 .UNSPECIFIED., .F., .F.,
 ( 4, 2, 2, 2, 2, 2, 2, 4 ),
 ( -5.999999999939666895E-08, 0.002684213935019686640, 0.004026350902529528264, 0.005368487870039371189, 0.006710624837549212379, 0.008052761805059056172, 0.009394898772568899964, 0.01073703574007874202 ),
 .UNSPECIFIED. ) ;
#44633 = VERTEX_POINT ( 'NONE', #100892 ) ;
#44634 = CARTESIAN_POINT ( 'NONE',  ( -0.7500000000000215383, 1.472916667349486008, 1.299038105676659116 ) ) ;
#44635 = CARTESIAN_POINT ( 'NONE',  ( 3.567518508692040236, 1.825626599287116791, -0.4067673385957787380 ) ) ;
#44636 = CARTESIAN_POINT ( 'NONE',  ( 2.760114697247218807, 1.645750434341390900, -0.5467383172713826678 ) ) ;
#44637 = CARTESIAN_POINT ( 'NONE',  ( 0.01182134700736507844, -2.246462713633586183, 0.4557613021327082681 ) ) ;
#44638 = CARTESIAN_POINT ( 'NONE',  ( 1.360703683432495259, 0.8952624662355921359, 2.017188127302282030 ) ) ;
#44639 = CARTESIAN_POINT ( 'NONE',  ( 3.854492016355787420, 0.7758605394001509836, 2.017853709245204463 ) ) ;
#44640 = CARTESIAN_POINT ( 'NONE',  ( 4.523342001410900259, -1.195735706813789045, -1.530077746507539027 ) ) ;
#44641 = CARTESIAN_POINT ( 'NONE',  ( 6.714126539417144102, -0.8821443205445091973, -1.649434700640100226 ) ) ;
#44642 = CARTESIAN_POINT ( 'NONE',  ( 0.06249170576382599707, -1.450827213159947338, -1.451031289061120777 ) ) ;
#44643 = DIRECTION ( 'NONE',  ( 0.000000000000000000, 0.000000000000000000, -1.000000000000000000 ) ) ;
#44644 = SURFACE_STYLE_FILL_AREA ( #59805 ) ;
#44645 = CARTESIAN_POINT ( 'NONE',  ( 1.360316468749973584, 2.786458333674735499, -0.7853790794159101196 ) ) ;
#44646 = CARTESIAN_POINT ( 'NONE',  ( 5.818982467333652764, 0.9914020171761170896, -1.755767668913270407 ) ) ;
#44647 = CARTESIAN_POINT ( 'NONE',  ( -8.748035429315585532, 11.22912730566677553, -1.599625672291263179 ) ) ;
#44648 = CARTESIAN_POINT ( 'NONE',  ( 5.282873410819217241, 9.315102745931094219, -0.7998128361456281477 ) ) ;
#44649 = CARTESIAN_POINT ( 'NONE',  ( 2.680963214763174118, -0.4786715097226356130, -0.1016399112248461689 ) ) ;
#44650 = CARTESIAN_POINT ( 'NONE',  ( 3.264084022359412529, 0.8216391472936382945, 1.630427331384458833 ) ) ;
#44651 = CARTESIAN_POINT ( 'NONE',  ( 2.678998284833411070, -2.111460168698295004, -0.6414983429729387288 ) ) ;
#44652 = ORIENTED_EDGE ( 'NONE', *, *, #31028, .F. ) ;
#44653 = CARTESIAN_POINT ( 'NONE',  ( -4.950135482320926705, 6.868520377498098739, -1.443375672974066548 ) ) ;
#44654 = CARTESIAN_POINT ( 'NONE',  ( -3.285556943750000514, -1.626041666188708046, -1.896917185911906500 ) ) ;
#44655 = CARTESIAN_POINT ( 'NONE',  ( -6.808165692356648258, 11.09461040772476714, 0.7998128361456481317 ) ) ;
#44656 = CARTESIAN_POINT ( 'NONE',  ( 1.107682413490064022, 1.532168600112630230, 1.316196929287305473 ) ) ;
#44657 = CARTESIAN_POINT ( 'NONE',  ( 0.9969211937387794098, -2.069638562867767373, -0.4609060192823294932 ) ) ;
#44659 = EDGE_CURVE ( 'NONE', #134155, #204270, #161923, .T. ) ;
#44658 = CARTESIAN_POINT ( 'NONE',  ( -1.000000000000017097, 9.200000000000018829, 0.4000000000000144551 ) ) ;
#44660 = CARTESIAN_POINT ( 'NONE',  ( -4.613517410400161722, 8.604463755433990002, -0.7998128361456362523 ) ) ;
#44661 = CARTESIAN_POINT ( 'NONE',  ( 1.498636204049142773, 0.3563576638296832577, 1.826325547775342173 ) ) ;
#44662 = CARTESIAN_POINT ( 'NONE',  ( 3.734381245560244089, 6.444196322207211836, 1.199719254218462483 ) ) ;
#44663 = AXIS2_PLACEMENT_3D ( 'NONE', #136275, #100554, #165553 ) ;
#44664 = CARTESIAN_POINT ( 'NONE',  ( 0.3214396764580421118, -0.1044536432763705502, 2.159311484102262479 ) ) ;
#44665 = CARTESIAN_POINT ( 'NONE',  ( 5.801407773674092105, 1.352156682446106206, -1.496049708713815374 ) ) ;
#44666 = VERTEX_POINT ( 'NONE', #36959 ) ;
#44667 = ORIENTED_EDGE ( 'NONE', *, *, #34950, .T. ) ;
#44668 = CARTESIAN_POINT ( 'NONE',  ( -9.972185678051314284, 11.59297036493672017, 1.199719254218462483 ) ) ;
#44669 = CARTESIAN_POINT ( 'NONE',  ( 4.301258635363705451, 1.467727663998198429, 1.085573330547324744 ) ) ;
#44672 = VERTEX_POINT ( 'NONE', #135547 ) ;
#44671 = CARTESIAN_POINT ( 'NONE',  ( -5.067137445304809695, 6.740953878067043270, -1.444057985504534125 ) ) ;
#44670 = CARTESIAN_POINT ( 'NONE',  ( -4.899292406491858820, 6.809203455697518947, -1.599625672291271394 ) ) ;
#44673 = CARTESIAN_POINT ( 'NONE',  ( 5.568688238291347403, 7.519645578322940338, 1.337618216391135428 ) ) ;
#44674 = CARTESIAN_POINT ( 'NONE',  ( 6.081407632663145435, 1.356090666932512789, -1.492028312255622824 ) ) ;
#44675 = CARTESIAN_POINT ( 'NONE',  ( 5.999929499617846496, -0.6670042279848520383, -1.716255146773135287 ) ) ;
#44676 = CARTESIAN_POINT ( 'NONE',  ( -0.02299388927987088688, 7.629137130509112907, -2.510989390717012881 ) ) ;
#44677 = CARTESIAN_POINT ( 'NONE',  ( 4.705897867575262516, -0.6186405800616563422, 2.223174812903663256 ) ) ;
#44678 = CARTESIAN_POINT ( 'NONE',  ( 4.532168488718122390, 8.509556680138327778, 0.7998128361456271485 ) ) ;
#44679 = CARTESIAN_POINT ( 'NONE',  ( 5.606754022945427351, 1.640879930231559758, -1.407263238018638507 ) ) ;
#44680 = CARTESIAN_POINT ( 'NONE',  ( 6.765682348419287173, 7.852049813699357728, 1.199719254218462483 ) ) ;
#44681 = CARTESIAN_POINT ( 'NONE',  ( 2.560020840168964806, -1.337455066581024976, 1.408356088163305042 ) ) ;
#44682 = EDGE_CURVE ( 'NONE', #83007, #34393, #29608, .T. ) ;
#44684 = ADVANCED_FACE ( 'NONE', ( #103039 ), #183212, .T. ) ;
#44683 = AXIS2_PLACEMENT_3D ( 'NONE', #53748, #150196, #119881 ) ;
#44685 = CARTESIAN_POINT ( 'NONE',  ( 4.903846967696810388, 0.3865712588492843937, 2.265520236764162920 ) ) ;
#44686 = DIRECTION ( 'NONE',  ( -5.578564026256490882E-16, -1.000000000000000000, -9.066213480720158442E-32 ) ) ;
#44687 = CARTESIAN_POINT ( 'NONE',  ( -6.454563648557663846, 9.688018802362710957, -1.199719254218452047 ) ) ;
#44688 = CARTESIAN_POINT ( 'NONE',  ( 4.328871119428026049, 0.09166491666120352155, 1.868520897946590598 ) ) ;
#44689 = ORIENTED_EDGE ( 'NONE', *, *, #187563, .F. ) ;
#44692 = CARTESIAN_POINT ( 'NONE',  ( -5.808742468812186033, 5.741564066561132940, 0.000000000000000000 ) ) ;
#44691 = CARTESIAN_POINT ( 'NONE',  ( -0.7500000000000006661, 0.8895833340161543035, -1.299038105676652011 ) ) ;
#44690 = CARTESIAN_POINT ( 'NONE',  ( 2.285291272251275707, 0.09004542135446562401, -1.910373438827176251 ) ) ;
#44693 = CARTESIAN_POINT ( 'NONE',  ( 4.090592613104036879, -2.182713160620152859, -0.3248913242878055385 ) ) ;
#44694 = CARTESIAN_POINT ( 'NONE',  ( -1.506334365903787775, 8.679455619938881483, -2.541882285198141300 ) ) ;
#44695 = CARTESIAN_POINT ( 'NONE',  ( -0.2108831679771167866, 1.375689764684871808, -2.152500126786048185 ) ) ;
#44696 = CARTESIAN_POINT ( 'NONE',  ( 5.139949632912227173, 8.050339434155988627, -1.082531754730548412 ) ) ;
#44697 = CARTESIAN_POINT ( 'NONE',  ( -5.099275172071237705, 8.963255110809500437, 0.000000000000000000 ) ) ;
#44698 = CARTESIAN_POINT ( 'NONE',  ( 1.616417101162690440, 1.326873100732330890, -1.458104111731808983 ) ) ;
#44699 = CARTESIAN_POINT ( 'NONE',  ( 1.290513193724596164, -1.035378025537621927, 2.062353807931560645 ) ) ;
#44700 = CARTESIAN_POINT ( 'NONE',  ( 2.805073129645048624, -1.632656238785214597, 1.087510969322850629 ) ) ;
#44701 = CARTESIAN_POINT ( 'NONE',  ( -6.042630808230841359E-15, -2.012500000000000178, 3.474999999999999645 ) ) ;
#44702 = CARTESIAN_POINT ( 'NONE',  ( 6.666849506214659549, 1.532398756413049457, -1.380780335402414849 ) ) ;
#44703 = CARTESIAN_POINT ( 'NONE',  ( 3.212919216758630014, 6.692230152952963529, 0.000000000000000000 ) ) ;
#44704 = CARTESIAN_POINT ( 'NONE',  ( 3.749232653202066778, 0.2420323627391370025, -2.001857840249580800 ) ) ;
#44705 = CARTESIAN_POINT ( 'NONE',  ( 5.876533236880477240, 5.820653295974182129, 0.7998128361456352531 ) ) ;
#44706 = EDGE_LOOP ( 'NONE', ( #20272, #655 ) ) ;
#44707 = CARTESIAN_POINT ( 'NONE',  ( -8.947491310014823895, 12.52615806407091803, 1.199719254218462483 ) ) ;
#44708 = LINE ( 'NONE', #195206, #42045 ) ;
#44709 = CARTESIAN_POINT ( 'NONE',  ( 9.561524646135536543, 12.17819805862340310, -1.599625672291262513 ) ) ;
#44710 = CARTESIAN_POINT ( 'NONE',  ( 1.710090495726908966, 0.6328077935687204114, -2.076762233347277053 ) ) ;
#44711 = DIRECTION ( 'NONE',  ( 0.000000000000000000, 1.000000000000000000, 0.000000000000000000 ) ) ;
#44712 = CARTESIAN_POINT ( 'NONE',  ( 10.96384816988413924, 2.972657967447023708, -3.969100948793135686 ) ) ;
#44713 = CARTESIAN_POINT ( 'NONE',  ( -9.796852598875474882, 4.534176102514267725, -6.931574287351667252 ) ) ;
#44714 = CARTESIAN_POINT ( 'NONE',  ( 2.635844295777586943, 0.8854499327175249235, -1.647724587607077629 ) ) ;
#44715 = CARTESIAN_POINT ( 'NONE',  ( 6.714160596891073141, -1.012370167489636819, -1.909856561116265450 ) ) ;
#44717 = CARTESIAN_POINT ( 'NONE',  ( 6.827182134110196365, 4.700652535171166768, 2.373648650996477372 ) ) ;
#44716 = FACE_OUTER_BOUND ( 'NONE', #142960, .T. ) ;
#44718 = CARTESIAN_POINT ( 'NONE',  ( 1.364683531249986537, -0.09479166632524321789, -0.7879004041258309554 ) ) ;
#44719 = CARTESIAN_POINT ( 'NONE',  ( -1.455305287003866965, 3.352261184402082428, -0.3947446046151094623 ) ) ;
#44720 = CARTESIAN_POINT ( 'NONE',  ( 1.734869227892420707, 1.784761669998648381, 0.6870963898520030533 ) ) ;
#44721 = CARTESIAN_POINT ( 'NONE',  ( 4.539784583036060361, 0.7555593814247036910, -1.600612801534553542 ) ) ;
#44722 = CARTESIAN_POINT ( 'NONE',  ( 2.385291144485178982, 0.09204604084523880514, -1.910175020619097275 ) ) ;
#44723 = CARTESIAN_POINT ( 'NONE',  ( -5.066996723205291708, 6.934582148538044777, 1.599625672291267398 ) ) ;
#44725 = CARTESIAN_POINT ( 'NONE',  ( 6.257445408045815505, 1.831477697454777953, -0.5614084181123339956 ) ) ;
#44724 = CARTESIAN_POINT ( 'NONE',  ( -1.620863580070950549, -1.399999999999998579, 1.903365770102946941 ) ) ;
#44726 = AXIS2_PLACEMENT_3D ( 'NONE', #173488, #77012, #43486 ) ;
#44727 = CARTESIAN_POINT ( 'NONE',  ( 0.7499999999999885647, 0.2333333333333562076, 1.299038105676657340 ) ) ;
#44728 = CARTESIAN_POINT ( 'NONE',  ( 1.170471352854907776, -0.9292243337341490328, -1.850172451097586990 ) ) ;
#44729 = CARTESIAN_POINT ( 'NONE',  ( 1.364683531249986537, -0.5739583329919174526, 0.7879004041258500513 ) ) ;
#44730 = CARTESIAN_POINT ( 'NONE',  ( 5.146153885717090759, 7.883215235610427918, -1.279915058160858710 ) ) ;
#44731 = CARTESIAN_POINT ( 'NONE',  ( 5.190257414508706368, -1.856628772771324210, -0.2281712211116558864 ) ) ;
#44732 = CARTESIAN_POINT ( 'NONE',  ( 1.189776066567624691, -0.8228614858879386151, 1.629801898503015156 ) ) ;
#44734 = CARTESIAN_POINT ( 'NONE',  ( 4.629651883607522223, 8.329987488807731211, -0.3686744245932921937 ) ) ;
#44733 = CARTESIAN_POINT ( 'NONE',  ( 4.828867971087246858, 2.111205472107956282, 0.6427781511747706622 ) ) ;
#44735 = CIRCLE ( 'NONE', #176141, 1.000000000000000000 ) ;
#44736 = CARTESIAN_POINT ( 'NONE',  ( 0.6823417656249917140, 5.405208333674749177, 1.181850606188765695 ) ) ;
#44737 = CARTESIAN_POINT ( 'NONE',  ( 2.717292478832333380, -1.793364790446878798, -1.018969015592002592 ) ) ;
#44738 = CARTESIAN_POINT ( 'NONE',  ( -8.799405390469187793, 10.22472669609091689, -1.199719254218446718 ) ) ;
#44739 =( LENGTH_UNIT ( ) NAMED_UNIT ( * ) SI_UNIT ( .MILLI., .METRE. ) );
#44740 = CARTESIAN_POINT ( 'NONE',  ( 1.409302795777320982, 3.485449738227918370, -0.5172811130322817474 ) ) ;
#44741 = CYLINDRICAL_SURFACE ( 'NONE', #37492, 8.049999999999993605 ) ;
#44742 = CARTESIAN_POINT ( 'NONE',  ( 5.169401708560450004, 9.252995436621013425, 0.000000000000000000 ) ) ;
#44743 = EDGE_LOOP ( 'NONE', ( #174783, #12672, #21165, #182775, #136680 ) ) ;
#44744 = CARTESIAN_POINT ( 'NONE',  ( 5.301260566756325510, -1.777534899005998481, 1.061244097098137606 ) ) ;
#44745 = CARTESIAN_POINT ( 'NONE',  ( -0.6823417656250246877, 0.3635416670080895973, 1.181850606188755259 ) ) ;
#44746 = CARTESIAN_POINT ( 'NONE',  ( 2.776834730583700228, -2.067601613962879448, -0.6303956341740593050 ) ) ;
#44747 = CARTESIAN_POINT ( 'NONE',  ( -4.752344554418619360, 8.202642464201909789, 0.7248784622895955154 ) ) ;
#44748 = CARTESIAN_POINT ( 'NONE',  ( 3.000653711923051414, -1.990157830909113024, -0.3430147326864175783 ) ) ;
#44749 = CARTESIAN_POINT ( 'NONE',  ( 6.720655732516639169, 2.430015300743305406, 2.455394564723146100 ) ) ;
#44750 = VERTEX_POINT ( 'NONE', #87854 ) ;
#44751 = EDGE_CURVE ( 'NONE', #213971, #29321, #112148, .T. ) ;
#44754 = CARTESIAN_POINT ( 'NONE',  ( 7.049876689426101350, 9.247942109129029475, -1.443375672974057666 ) ) ;
#44753 = CARTESIAN_POINT ( 'NONE',  ( 3.475000000000000533, -1.895833333333332815, -2.006292185433951047 ) ) ;
#44752 = CARTESIAN_POINT ( 'NONE',  ( 10.10343170205820407, 2.974000657017351390, 5.833219012922953972 ) ) ;
#44755 = CARTESIAN_POINT ( 'NONE',  ( -5.275531169048922386, 5.327410250078064458, -0.7216878364870338292 ) ) ;
#44756 = CARTESIAN_POINT ( 'NONE',  ( 1.130092623156966347, 2.014433208573155110, 0.09411304420373775570 ) ) ;
#44758 = CARTESIAN_POINT ( 'NONE',  ( 5.970311429539967740, -2.080533979117826782, -0.6889730390344513955 ) ) ;
#44757 = CARTESIAN_POINT ( 'NONE',  ( -4.608882153641705059, 7.464447381635583412, -1.199719254218452047 ) ) ;
#44759 = CARTESIAN_POINT ( 'NONE',  ( -1.500000000000011324, 4.910416667349486453, -0.8660254037844313801 ) ) ;
#44760 = CARTESIAN_POINT ( 'NONE',  ( 4.465046277278037934, -1.532637281380120564, 1.143568071694904598 ) ) ;
#44761 = CARTESIAN_POINT ( 'NONE',  ( -4.939248034080176097, 4.656877549381960080, 1.214306433183764966E-14 ) ) ;
#44762 = CARTESIAN_POINT ( 'NONE',  ( 6.941411460072420603, 7.200660912947041581, 1.040834085586084257E-14 ) ) ;
#44764 = CARTESIAN_POINT ( 'NONE',  ( 3.462517696756307384, -1.944077823024586538, -0.5350690621670484148 ) ) ;
#44763 = CARTESIAN_POINT ( 'NONE',  ( -8.148087131688679818, 12.44992605370473804, -0.7216878364870267237 ) ) ;
#44765 = CARTESIAN_POINT ( 'NONE',  ( -1.364683531250010295, 13.44270833367473017, 0.7879004041258445001 ) ) ;
#44766 = CARTESIAN_POINT ( 'NONE',  ( -4.462568837553487100, 5.235360394347691404, -1.199719254218453823 ) ) ;
#44767 = CARTESIAN_POINT ( 'NONE',  ( 5.631808906544129911, -1.097478420741523575, -1.330571920265137376 ) ) ;
#44768 = CARTESIAN_POINT ( 'NONE',  ( 5.688527969385528849, 8.794310509995222347, -1.199719254218452047 ) ) ;
#44769 = CARTESIAN_POINT ( 'NONE',  ( 2.198393463710220264, 5.716542807637226886, 0.7998128361456462443 ) ) ;
#44770 = CARTESIAN_POINT ( 'NONE',  ( 3.559516622919870350E-16, 1.551257596039481879, -2.000000000000006217 ) ) ;
#44771 = EDGE_CURVE ( 'NONE', #50158, #121448, #3465, .T. ) ;
#44772 = CARTESIAN_POINT ( 'NONE',  ( 11.94105721237523277, 10.19999999999999929, -1.187919463087249827 ) ) ;
#44773 = CARTESIAN_POINT ( 'NONE',  ( 0.6728209460903147310, 1.430239379376567976, -1.496996390900617424 ) ) ;
#44774 = PRESENTATION_LAYER_ASSIGNMENT (  '', '', ( #138146 ) ) ;
#44775 = CARTESIAN_POINT ( 'NONE',  ( -1.500000000000055511, 7.240846818246208905, -4.154462424328210446 ) ) ;
#44776 = VERTEX_POINT ( 'NONE', #200509 ) ;
#44777 = CARTESIAN_POINT ( 'NONE',  ( 5.795527448272657089, 1.671165027121311430, -0.6995385440057879656 ) ) ;
#44778 = CARTESIAN_POINT ( 'NONE',  ( 3.770049233051776749, 6.556085317605844232, 1.199719254218451159 ) ) ;
#44779 = PLANE ( 'NONE',  #97705 ) ;
#44780 = CARTESIAN_POINT ( 'NONE',  ( 0.5272532902790193488, -0.2650996996472804734, 1.791917353721095285 ) ) ;
#44781 = CARTESIAN_POINT ( 'NONE',  ( 4.651856102820254968, 7.480896982382013505, -1.082531754730548412 ) ) ;
#44782 = CARTESIAN_POINT ( 'NONE',  ( 10.26921470707188178, 10.85134567802567673, -6.214135076749980335 ) ) ;
#44783 = CARTESIAN_POINT ( 'NONE',  ( 3.099763004921416876, -2.188912590334081809, 0.1079765428157742069 ) ) ;
#44784 = ORIENTED_EDGE ( 'NONE', *, *, #45494, .F. ) ;
#44786 = CARTESIAN_POINT ( 'NONE',  ( 7.727257484784855635, 11.10255193463598111, -1.199719254218446718 ) ) ;
#44785 = CARTESIAN_POINT ( 'NONE',  ( 0.4495626703563436743, 1.451167377975391304, 1.320406988977901985 ) ) ;
#44787 = CARTESIAN_POINT ( 'NONE',  ( 4.605048111083247520, -0.08973289204975383460, 1.913620015931324581 ) ) ;
#44788 = CARTESIAN_POINT ( 'NONE',  ( -1.500000000000021982, 7.388542872122518368, 4.154462424328226433 ) ) ;
#44789 = CARTESIAN_POINT ( 'NONE',  ( -6.478676351974181458, 6.772485410396933858, 0.2589597434300341394 ) ) ;
#44790 = CARTESIAN_POINT ( 'NONE',  ( 6.727182134110200273, -0.004969159814478123736, 2.189081792362323586 ) ) ;
#44791 = CARTESIAN_POINT ( 'NONE',  ( 0.6823417656249882723, -0.3239583329919110133, -1.181850606188749264 ) ) ;
#44793 = VERTEX_POINT ( 'NONE', #168036 ) ;
#44792 = CARTESIAN_POINT ( 'NONE',  ( 4.853455804012212660, 7.645820290447483458, 1.082531754730558626 ) ) ;
#44794 = ADVANCED_FACE ( 'NONE', ( #85710 ), #19485, .T. ) ;
#44795 = CARTESIAN_POINT ( 'NONE',  ( -7.687109909268394325, 11.91211929421440097, 0.000000000000000000 ) ) ;
#44796 = CARTESIAN_POINT ( 'NONE',  ( 2.061604318190731533, 0.3698614785779800185, -2.129673623264888960 ) ) ;
#44797 = CARTESIAN_POINT ( 'NONE',  ( -3.959863383643135393, 6.777535159962392086, 1.199719254218452935 ) ) ;
#44798 = CARTESIAN_POINT ( 'NONE',  ( 4.913904330310220558, 4.697586238308844919, 0.000000000000000000 ) ) ;
#44799 = CARTESIAN_POINT ( 'NONE',  ( 1.764397251013736234, -1.293498944356825664, 1.288518760371157201 ) ) ;
#44800 = CARTESIAN_POINT ( 'NONE',  ( -0.2046613956954954905, -0.1581703332043625232, -2.086340352340488646 ) ) ;
#44801 = EDGE_CURVE ( 'NONE', #182295, #71404, #137655, .T. ) ;
#44802 = CARTESIAN_POINT ( 'NONE',  ( 5.016531207907320322, 1.258010867292450152, -1.323153095230594989 ) ) ;
#44803 = CARTESIAN_POINT ( 'NONE',  ( 10.91109197447695855, 8.117831379166393191, -4.410072780793198532 ) ) ;
#44804 = CARTESIAN_POINT ( 'NONE',  ( 3.111475685156277038, 1.510342251817019532, 1.173009309769344588 ) ) ;
#44805 = ORIENTED_EDGE ( 'NONE', *, *, #76744, .T. ) ;
#44806 = CARTESIAN_POINT ( 'NONE',  ( 3.631270037613967716, 0.05078019485712419873, -1.969077574667767783 ) ) ;
#44807 = ORIENTED_EDGE ( 'NONE', *, *, #208519, .T. ) ;
#44808 = CARTESIAN_POINT ( 'NONE',  ( 5.442900063589676485, -1.533566843616997133, -1.191469007954217618 ) ) ;
#44809 = ORIENTED_EDGE ( 'NONE', *, *, #52849, .F. ) ;
#44810 = CARTESIAN_POINT ( 'NONE',  ( -4.938913097128142304, 8.984092056616635347, -0.7998128361456362523 ) ) ;
#44812 = FACE_OUTER_BOUND ( 'NONE', #194151, .T. ) ;
#44811 = CARTESIAN_POINT ( 'NONE',  ( -4.014095998097799267, 6.840806543492835345, -1.199719254218450271 ) ) ;
#44813 = CARTESIAN_POINT ( 'NONE',  ( 7.499068361690118145, 7.921536974826172361, -0.7216878364870317197 ) ) ;
#44814 = CARTESIAN_POINT ( 'NONE',  ( 4.037688526304391345, -1.829018870347882242, 0.5580751363460645376 ) ) ;
#44815 = CARTESIAN_POINT ( 'NONE',  ( 4.492266506575326446, 7.256230230409263626, -1.267781117195718288 ) ) ;
#44816 = CARTESIAN_POINT ( 'NONE',  ( 0.000000000000000000, 13.49999999999999822, 0.000000000000000000 ) ) ;
#44817 = CARTESIAN_POINT ( 'NONE',  ( 4.927462483923885195, 4.713404084191450849, -0.7998128361456481317 ) ) ;
#44818 = CARTESIAN_POINT ( 'NONE',  ( 5.285796247307868789, 1.939527786139252585, -0.5389555323440149426 ) ) ;
#44820 =( BOUNDED_SURFACE ( )  B_SPLINE_SURFACE ( 3, 2, ( 
 ( #98483, #113738, #148310 ),
 ( #177614, #29225, #164548 ),
 ( #95317, #212209, #12949 ),
 ( #179743, #31361, #163492 ),
 ( #14006, #15074, #79027 ),
 ( #145143, #211149, #81165 ) ),
 .UNSPECIFIED., .F., .F., .T. ) 
 B_SPLINE_SURFACE_WITH_KNOTS ( ( 4, 2, 4 ),
 ( 3, 3 ),
 ( 0.000000000000000000, 0.002122857551078453833, 0.004245715102156907665 ),
 ( 0.000000000000000000, 1.000000000000000000 ),
 .UNSPECIFIED. ) 
 GEOMETRIC_REPRESENTATION_ITEM ( )  RATIONAL_B_SPLINE_SURFACE ( (
 ( 1.000000000000000000, 0.7806433624857551656, 1.000000000000000000),
 ( 1.000000000000000000, 0.7860453980259762830, 1.000000000000000000),
 ( 1.000000000000000000, 0.7924770197564222629, 1.000000000000000000),
 ( 1.000000000000000000, 0.8094762427233136437, 1.000000000000000000),
 ( 1.000000000000000000, 0.8200718518785207189, 1.000000000000000000),
 ( 1.000000000000000000, 0.8343063410434355953, 1.000000000000000000) ) ) 
 REPRESENTATION_ITEM ( '' )  SURFACE ( )  );
#44819 = CARTESIAN_POINT ( 'NONE',  ( 0.2333540202161603905, 0.003568502611739342648, -2.045944795905803471 ) ) ;
#44821 = CARTESIAN_POINT ( 'NONE',  ( 5.619710272201024814, -1.780234218580947436, 0.4041525643716862848 ) ) ;
#44822 = CARTESIAN_POINT ( 'NONE',  ( 1.064989848632340363, 1.568927673159369762, -1.351003706900590018 ) ) ;
#44823 = CARTESIAN_POINT ( 'NONE',  ( -7.375272376154093479, 9.627570410311676596, -1.443375672974059665 ) ) ;
#44824 = CARTESIAN_POINT ( 'NONE',  ( -6.114219544286552122, 7.015314154546907766, -0.9703045268592332961 ) ) ;
#44825 = CARTESIAN_POINT ( 'NONE',  ( 11.01135777277262306, 12.69999999999998153, 1.399999999999998579 ) ) ;
#44826 = CARTESIAN_POINT ( 'NONE',  ( 6.543822781336226413, 0.7137633992815132222, -1.729328153040734506 ) ) ;
#44827 = CARTESIAN_POINT ( 'NONE',  ( 5.438792177376376991, 9.497007973581119700, 1.040834085586084257E-14 ) ) ;
#44828 = CARTESIAN_POINT ( 'NONE',  ( -5.112968612895188336, 4.859551557999480131, -0.5494739808295947547 ) ) ;
#44829 = DIRECTION ( 'NONE',  ( 1.014813233446432150E-15, 1.000000000000000000, -4.583713267641621330E-32 ) ) ;
#44830 = CARTESIAN_POINT ( 'NONE',  ( 1.364683531250000303, 12.06770833367473195, -0.7879004041258355073 ) ) ;
#44831 = CARTESIAN_POINT ( 'NONE',  ( -3.438964519360665051, 7.163875705896082913, -0.7998128361456281477 ) ) ;
#44832 = CARTESIAN_POINT ( 'NONE',  ( -4.055297343818976330, 5.824542549245813383, 1.443375672974065660 ) ) ;
#44833 = AXIS2_PLACEMENT_3D ( 'NONE', #81003, #147091, #32255 ) ;
#44834 = CARTESIAN_POINT ( 'NONE',  ( 4.096141260758720648, -0.2909454306243773325, 1.709365352543093186 ) ) ;
#44835 = CARTESIAN_POINT ( 'NONE',  ( -4.446184310277715213, 7.274633231044262516, -1.199719254218452047 ) ) ;
#44836 = CARTESIAN_POINT ( 'NONE',  ( 0.7782871991188352601, -1.104406889285912907, -1.750870654829151274 ) ) ;
#44837 = CARTESIAN_POINT ( 'NONE',  ( 2.900141384978659698, -1.046112932010187624, -1.840686247649555796 ) ) ;
#44838 = CARTESIAN_POINT ( 'NONE',  ( 5.030238685870051185, 5.827365540725222282, -1.199719254218452047 ) ) ;
#44839 = CARTESIAN_POINT ( 'NONE',  ( 7.564559641420864899, 10.91273778404466199, -1.199719254218446718 ) ) ;
#44840 = CARTESIAN_POINT ( 'NONE',  ( 0.4405300623744661803, 6.460114622649768990, 3.246819496866228505 ) ) ;
#44841 = CARTESIAN_POINT ( 'NONE',  ( 6.860220180191213935, -2.069926439015772335, 0.04462916171246725239 ) ) ;
#44842 = CARTESIAN_POINT ( 'NONE',  ( 4.121712324234096059, 7.667736414601909800, 0.7403736254629582625 ) ) ;
#44843 = CARTESIAN_POINT ( 'NONE',  ( 5.680503174445848735, 5.729601246382692636, 1.040834085586084257E-14 ) ) ;
#44845 = CARTESIAN_POINT ( 'NONE',  ( 4.161989969270892153, 6.839110149915929249, 1.082531754730558626 ) ) ;
#44844 = CARTESIAN_POINT ( 'NONE',  ( 3.475000000000000533, -2.595833333333334103, -2.006292185433951047 ) ) ;
#44846 = CARTESIAN_POINT ( 'NONE',  ( 3.222906779550426926, 0.05642716604136116532, 2.291727194984194860 ) ) ;
#44847 = CARTESIAN_POINT ( 'NONE',  ( 0.6623940301842005107, -1.324425631624454036, 1.256838194884236204 ) ) ;
#44848 = CARTESIAN_POINT ( 'NONE',  ( 3.480628297764537304, -1.280852673386581264, 1.420289963180096260 ) ) ;
#44849 = CARTESIAN_POINT ( 'NONE',  ( 5.071631979963703962, 8.074598522336444262, 1.199719254218451159 ) ) ;
#44850 = CARTESIAN_POINT ( 'NONE',  ( 5.788968402910795064, 9.697620870130524651, 0.7216878364870438212 ) ) ;
#44851 = CARTESIAN_POINT ( 'NONE',  ( -7.808606406466886973, 11.19745900993164511, 1.199719254218453823 ) ) ;
#44852 = CARTESIAN_POINT ( 'NONE',  ( 1.845949328209312901, -1.318067166357287379, -1.521789114188701664 ) ) ;
#44853 = CARTESIAN_POINT ( 'NONE',  ( 2.201936455694650796, 0.7555380192853027310, -1.810630540845730385 ) ) ;
#44854 = CARTESIAN_POINT ( 'NONE',  ( -8.188234707649510113, 11.64035869464474082, -1.199719254218446718 ) ) ;
#44855 = B_SPLINE_CURVE_WITH_KNOTS ( 'NONE', 3,
 ( #87215, #106724, #104546, #170591, #74180, #137045 ),
 .UNSPECIFIED., .F., .F.,
 ( 4, 2, 4 ),
 ( 0.000000000000000000, 0.5000000000000000000, 1.000000000000000000 ),
 .UNSPECIFIED. ) ;
#44856 = CARTESIAN_POINT ( 'NONE',  ( -4.889686956022917919, 8.856385215335397021, 1.214306433183764966E-14 ) ) ;
#44857 = CARTESIAN_POINT ( 'NONE',  ( -11.48806469435255373, 9.769102271275510674, -3.468902948106704631 ) ) ;
#44859 = CARTESIAN_POINT ( 'NONE',  ( 3.186155166506371650, -1.743393047566743181, -0.3038327287053984027 ) ) ;
#44858 = CARTESIAN_POINT ( 'NONE',  ( 5.437476023981094642, 0.8479630442611612029, -1.911130889300112878 ) ) ;
#44860 = CARTESIAN_POINT ( 'NONE',  ( 0.7124089920923117880, 14.00000000000000533, 12.66466791154580207 ) ) ;
#44862 = CARTESIAN_POINT ( 'NONE',  ( 5.912145817070847187, 1.543564834742835234, -1.694840376948128391 ) ) ;
#44861 = DIRECTION ( 'NONE',  ( 0.000000000000000000, 0.000000000000000000, 1.000000000000000000 ) ) ;
#44863 = CARTESIAN_POINT ( 'NONE',  ( 4.769343782054527026, 1.005586498893149772, 1.420189556619367410 ) ) ;
#44864 = CARTESIAN_POINT ( 'NONE',  ( 7.730120138085914583, 12.17022392774227768, 0.7998128361456462443 ) ) ;
#44865 = CARTESIAN_POINT ( 'NONE',  ( -0.1104750535120234134, 0.7027814200676918421, -2.185477693842474256 ) ) ;
#44866 = CARTESIAN_POINT ( 'NONE',  ( 4.921093860428086941, 0.6645110682935355673, 1.601655696547391594 ) ) ;
#44867 = CARTESIAN_POINT ( 'NONE',  ( 4.738842072872849087, -2.104903140973454434, -0.5318641579697135358 ) ) ;
#44868 = CARTESIAN_POINT ( 'NONE',  ( 5.183294799126148433, 4.941598775268944976, 1.040834085586084257E-14 ) ) ;
#44869 = ADVANCED_FACE ( 'NONE', ( #40173 ), #6573, .F. ) ;
#44870 = CARTESIAN_POINT ( 'NONE',  ( 6.368375356916068597, -1.978549699825098429, -0.3886382054163611821 ) ) ;
#44871 = CARTESIAN_POINT ( 'NONE',  ( 4.593750000000003553, -1.895863743164180493, -0.7852924748297412938 ) ) ;
#44872 = CARTESIAN_POINT ( 'NONE',  ( 1.499999999999989120, 5.577083334016153415, -0.8660254037844323793 ) ) ;
#44873 = CARTESIAN_POINT ( 'NONE',  ( 2.942313797947668785, 1.911627860423757097, 0.2376154225440275658 ) ) ;
#44874 = CARTESIAN_POINT ( 'NONE',  ( 0.7500000000000006661, 10.94791666734946212, -1.299038105676657340 ) ) ;
#44875 = CARTESIAN_POINT ( 'NONE',  ( 0.3467151180503316166, 1.136585144892443777, -1.908366640695156047 ) ) ;
#44876 = ORIENTED_EDGE ( 'NONE', *, *, #194169, .T. ) ;
#44877 = CARTESIAN_POINT ( 'NONE',  ( -0.1409997244346088419, 5.722143553014046979, -2.594341442600463843 ) ) ;
#44878 = CARTESIAN_POINT ( 'NONE',  ( -0.7500000000000006661, 2.608333333333358262, -1.299038105676652011 ) ) ;
#44879 = CARTESIAN_POINT ( 'NONE',  ( 5.880485940025228508, 7.883652901494672349, 1.599625672291267398 ) ) ;
#44880 = CARTESIAN_POINT ( 'NONE',  ( 2.649351634902767483, 0.2746262237617850821, 2.204210978092531192 ) ) ;
#44882 = CARTESIAN_POINT ( 'NONE',  ( -4.370663978927098015, 5.060324124126027279, 1.009771797811723326 ) ) ;
#44881 = AXIS2_PLACEMENT_3D ( 'NONE', #134829, #36218, #114367 ) ;
#44883 = CARTESIAN_POINT ( 'NONE',  ( 6.914295153289432783, 10.05013286460426691, -1.082531754730537976 ) ) ;
#44884 = CARTESIAN_POINT ( 'NONE',  ( 0.1467296397388196671, 8.209138825498294878, 2.038183423090501378 ) ) ;
#44885 = CARTESIAN_POINT ( 'NONE',  ( 7.024532985656128936, 9.288650798055913427, 1.443375672974065660 ) ) ;
#44886 = CARTESIAN_POINT ( 'NONE',  ( 0.1588275700346117869, 1.163271727376416376, 1.646837250247008777 ) ) ;
#44888 = CARTESIAN_POINT ( 'NONE',  ( 5.582507124453381486, 1.231422846540839666, -1.654610746699414214 ) ) ;
#44887 = CARTESIAN_POINT ( 'NONE',  ( 7.242026607993941489, 11.60078147596829901, 0.7998128361456462443 ) ) ;
#44889 = DIRECTION ( 'NONE',  ( 0.7592566023653005702, -0.6507913734559639396, 0.000000000000000000 ) ) ;
#44890 = CARTESIAN_POINT ( 'NONE',  ( -3.684065054611367351, 5.321161868511784299, -1.599625672291256295 ) ) ;
#44891 = DIRECTION ( 'NONE',  ( 0.000000000000000000, 0.000000000000000000, -1.000000000000000000 ) ) ;
#44892 = CARTESIAN_POINT ( 'NONE',  ( -0.6823417656250003738, 0.4677083336747517306, -1.181850606188749264 ) ) ;
#44893 = CARTESIAN_POINT ( 'NONE',  ( 0.3679306741783492929, -1.162814898748459225, 1.334192561405376676 ) ) ;
#44894 = CARTESIAN_POINT ( 'NONE',  ( 5.537694164425770005, -1.361542515911953855, 1.073868356900798959 ) ) ;
#44895 = CARTESIAN_POINT ( 'NONE',  ( 6.058121337783492599, -1.224224903413055010, 1.237393016278231617 ) ) ;
#44896 = CARTESIAN_POINT ( 'NONE',  ( 2.507732108623667688, -2.266951094411073786, 0.3397945559272512739 ) ) ;
#44897 = CARTESIAN_POINT ( 'NONE',  ( -1.364683531250000748, -0.2406249996585799189, 0.000000000000000000 ) ) ;
#44898 = CARTESIAN_POINT ( 'NONE',  ( 2.642321604431462578, -1.530645349967133972, 1.022873098850234141 ) ) ;
#44899 = CARTESIAN_POINT ( 'NONE',  ( 7.736899214892750010, 12.17813285068358020, 1.040834085586084257E-14 ) ) ;
#44900 = CARTESIAN_POINT ( 'NONE',  ( 2.379681254797087586, 1.121034037677430595, 1.440765146680768272 ) ) ;
#44901 = CARTESIAN_POINT ( 'NONE',  ( 2.250625165576759290, 1.976955744075848065, -0.3961026872240576702 ) ) ;
#44902 = CARTESIAN_POINT ( 'NONE',  ( -4.243338890952911058, 5.013278796608906518, -1.082531754730543971 ) ) ;
#44903 = CARTESIAN_POINT ( 'NONE',  ( 9.056676007273772200, 14.47807714179512573, -7.134106128614786435 ) ) ;
#44904 = CARTESIAN_POINT ( 'NONE',  ( 4.295997052264050708, -0.8081792604435251715, 1.944918383092561376 ) ) ;
#44905 = CARTESIAN_POINT ( 'NONE',  ( -6.470265622219711688, 8.571729197388226140, -1.599625672291263179 ) ) ;
#44906 = CARTESIAN_POINT ( 'NONE',  ( 8.655308441557755472, 13.90277502934238463, 7.849885418944005266 ) ) ;
#44907 = CARTESIAN_POINT ( 'NONE',  ( 1.996617168637443429, 2.047528291220417351, 0.3059219562495316125 ) ) ;
#44908 = CARTESIAN_POINT ( 'NONE',  ( 3.018661757337009810, 6.673522483535157868, 0.000000000000000000 ) ) ;
#44909 = CARTESIAN_POINT ( 'NONE',  ( 1.360316468749945606, 0.06770833367471427999, -0.7853790794159161148 ) ) ;
#44910 = CARTESIAN_POINT ( 'NONE',  ( 5.110073233524446756, -0.7627883623938614965, 1.978724553277847464 ) ) ;
#44911 = CARTESIAN_POINT ( 'NONE',  ( 6.393173274427864428, 1.585754722747900969, -0.9045919592586546543 ) ) ;
#44912 = ORIENTED_EDGE ( 'NONE', *, *, #191183, .F. ) ;
#44913 = CARTESIAN_POINT ( 'NONE',  ( -4.197131071882288289, 7.054347462908075350, -1.199719254218455378 ) ) ;
#44914 = CARTESIAN_POINT ( 'NONE',  ( 8.048736748007069508, 12.54194330598362406, -0.7998128361456352531 ) ) ;
#44915 = CARTESIAN_POINT ( 'NONE',  ( 5.736508391913541338, 6.825586224388162648, -1.082531754730548412 ) ) ;
#44916 = CARTESIAN_POINT ( 'NONE',  ( -3.474999999999998312, -0.9770833323774182899, 2.006292185433951047 ) ) ;
#44917 = CARTESIAN_POINT ( 'NONE',  ( -6.579784621333750749, 6.570836901177822931, 0.7998128361456341429 ) ) ;
#44918 = CARTESIAN_POINT ( 'NONE',  ( 6.082307721193076944, 1.091511717630256673, 1.817998432235830908 ) ) ;
#44919 = CARTESIAN_POINT ( 'NONE',  ( 1.237491679122425969, -1.904027454836676014, 0.9001316648933003206 ) ) ;
#44920 = CARTESIAN_POINT ( 'NONE',  ( -3.630551273409382329, 7.457669928944732796, 0.7998128361456352531 ) ) ;
#44921 = CARTESIAN_POINT ( 'NONE',  ( 9.576136569953906275, 10.06658084123472641, 0.000000000000000000 ) ) ;
#44922 = CARTESIAN_POINT ( 'NONE',  ( 5.787920722453932854, -1.179413039982403433, -1.439513333959110852 ) ) ;
#44923 = CARTESIAN_POINT ( 'NONE',  ( 9.426996880203592610, 9.892584536526015881, -0.7998128361456281477 ) ) ;
#44924 = DIRECTION ( 'NONE',  ( 1.000000000000000000, 0.000000000000000000, -1.665334536937734811E-16 ) ) ;
#44925 = CARTESIAN_POINT ( 'NONE',  ( -6.102578539926875933, 10.13377570664109051, 0.7216878364870267237 ) ) ;
#44926 = CARTESIAN_POINT ( 'NONE',  ( -9.110716038703348119, 12.61262389758715408, 1.082531754730560403 ) ) ;
#44927 = CARTESIAN_POINT ( 'NONE',  ( -9.857181934075960328, 5.275265258315555705, 6.218892358987248237 ) ) ;
#44928 = CARTESIAN_POINT ( 'NONE',  ( 1.154700538379228147, -4.295408888568413630, -1.734723475976807094E-15 ) ) ;
#44930 = CARTESIAN_POINT ( 'NONE',  ( 2.523818479427087702, 1.924573107942130656, -0.3798230296482503210 ) ) ;
#44929 = CARTESIAN_POINT ( 'NONE',  ( -7.555971681517696936, 7.709721804725773175, 0.7998128361456462443 ) ) ;
#44931 = CARTESIAN_POINT ( 'NONE',  ( 1.217891636700708435, -2.108894920778502602, 0.4742063263511315796 ) ) ;
#44933 = CARTESIAN_POINT ( 'NONE',  ( -6.138286310890375574, 5.995785266799176227, -0.01092221066891288506 ) ) ;
#44932 = CARTESIAN_POINT ( 'NONE',  ( -5.285699784481336927, 7.260012063351913625, 1.599625672291263179 ) ) ;
#44934 = CARTESIAN_POINT ( 'NONE',  ( 1.364683531249988757, 1.634375000341421691, 0.000000000000000000 ) ) ;
#44935 = CARTESIAN_POINT ( 'NONE',  ( 2.776348759439921654, -1.715481723685903903, 0.2504971047874882117 ) ) ;
#44936 = CARTESIAN_POINT ( 'NONE',  ( 2.747703163511563407, 0.5864964929944632699, 1.638654499222062189 ) ) ;
#44937 = CARTESIAN_POINT ( 'NONE',  ( 7.782016984564060103, 9.141736572488651902, 1.082531754730558626 ) ) ;
#44938 = CARTESIAN_POINT ( 'NONE',  ( -10.92046113480654768, 4.688422163420479016, 4.459782501114215592 ) ) ;
#44939 = EDGE_CURVE ( 'NONE', #192862, #74902, #86366, .T. ) ;
#44940 = CARTESIAN_POINT ( 'NONE',  ( 1.950545848857932807, 1.388271641964162084, 1.462223312268404074 ) ) ;
#44941 = FACE_BOUND ( 'NONE', #97390, .T. ) ;
#44942 = CARTESIAN_POINT ( 'NONE',  ( -5.334207092333882017, 5.187939460669764635, 0.7998128361456281477 ) ) ;
#44943 = CARTESIAN_POINT ( 'NONE',  ( 0.8132764231247009423, -0.2916495841569742842, 1.949667021961091429 ) ) ;
#44945 = CARTESIAN_POINT ( 'NONE',  ( -4.475600106286965918, 8.235634200727838916, 0.7216878364870338292 ) ) ;
#44944 = CARTESIAN_POINT ( 'NONE',  ( 6.258066496116281741, 0.7254575739856858885, -1.769658340881982816 ) ) ;
#44946 = CARTESIAN_POINT ( 'NONE',  ( -4.950135482320914271, 8.789258806100786359, -0.7216878364870338292 ) ) ;
#44947 = CARTESIAN_POINT ( 'NONE',  ( 5.203297092594585393, 9.292540051327542017, 0.7998128361456341429 ) ) ;
#44948 = CARTESIAN_POINT ( 'NONE',  ( -6.119526231721793330, 8.232809585132461194, 1.599625672291263179 ) ) ;
#44949 = CARTESIAN_POINT ( 'NONE',  ( 1.506516584307997730, -2.010164795747824140, -0.1955670033209846170 ) ) ;
#44950 = LINE ( 'NONE', #112135, #125283 ) ;
#44951 = CARTESIAN_POINT ( 'NONE',  ( 4.419161195688524835, 2.107920515157933661, 0.9393535314214102039 ) ) ;
#44952 = CARTESIAN_POINT ( 'NONE',  ( 6.373494408814909917, -0.2414686440028299685, 1.946897059556201848 ) ) ;
#44953 = ADVANCED_FACE ( 'NONE', ( #74805 ), #58548, .T. ) ;
#44954 = CARTESIAN_POINT ( 'NONE',  ( 3.414850490325722632, -1.488543670003231068, 1.277929504599809585 ) ) ;
#44955 = CARTESIAN_POINT ( 'NONE',  ( 7.099665995050449041, 11.43469409420089455, 0.7998128361456462443 ) ) ;
#44956 = FACE_OUTER_BOUND ( 'NONE', #175712, .T. ) ;
#44957 = VERTEX_POINT ( 'NONE', #5494 ) ;
#44958 = CARTESIAN_POINT ( 'NONE',  ( 1.200578840252497947, 1.417437365323451104, -1.573097661806458936 ) ) ;
#44960 = CARTESIAN_POINT ( 'NONE',  ( -6.021792782764022078, 10.17717534653336209, -0.7998128361456291469 ) ) ;
#44959 = CARTESIAN_POINT ( 'NONE',  ( -4.946027110887008860, 4.664786472323266153, -0.7998128361456221525 ) ) ;
#44961 = CARTESIAN_POINT ( 'NONE',  ( 1.482094074889642288, -0.2687121449159133313, -1.821302815977184686 ) ) ;
#44962 = ORIENTED_EDGE ( 'NONE', *, *, #48897, .T. ) ;
#44963 = CARTESIAN_POINT ( 'NONE',  ( 10.85711101555931180, 9.595049302670672020, -5.123733482772419023 ) ) ;
#44964 = CARTESIAN_POINT ( 'NONE',  ( 3.375340920106313813, -1.871962376360849056, -0.9962781187466958066 ) ) ;
#44965 = CARTESIAN_POINT ( 'NONE',  ( -1.499999999999997780, 4.181250000682819490, 1.214306433183764966E-14 ) ) ;
#44966 = CARTESIAN_POINT ( 'NONE',  ( 7.884230021546724920, 9.157022099014721306, 1.199719254218462483 ) ) ;
#44967 = CARTESIAN_POINT ( 'NONE',  ( -1.225000000000042277, 0.5208333333333544646, 0.7072540797572777205 ) ) ;
#44968 = ORIENTED_EDGE ( 'NONE', *, *, #26377, .F. ) ;
#44969 = CARTESIAN_POINT ( 'NONE',  ( 3.708323652925065161, -0.8317495340520587588, -1.885651027073296904 ) ) ;
#44970 = VECTOR ( 'NONE', #69169, 1000.000000000000000 ) ;
#44972 = CARTESIAN_POINT ( 'NONE',  ( -0.04178991631376138827, -1.644041690304678616, -0.8291446804715857377 ) ) ;
#44971 = CARTESIAN_POINT ( 'NONE',  ( -7.395082721250053837, 10.71501471051202614, -1.199719254218446718 ) ) ;
#44973 = CARTESIAN_POINT ( 'NONE',  ( 0.6823417656249899377, 2.842708333674753618, 1.181850606188765695 ) ) ;
#44974 = CARTESIAN_POINT ( 'NONE',  ( 1.464817136648363327, 4.229140356987229232, 0.3332976056707502299 ) ) ;
#44975 = LINE ( 'NONE', #195475, #33824 ) ;
#44976 = CARTESIAN_POINT ( 'NONE',  ( 2.636292518416444075, 1.068738387235500298, -1.994089298797457666 ) ) ;
#44977 = CARTESIAN_POINT ( 'NONE',  ( -9.083599731475995753, 11.62061899152058686, 1.443375672974064550 ) ) ;
#44978 = CARTESIAN_POINT ( 'NONE',  ( 2.830093135299842189, -0.8964878685940536052, -1.574152086365911529 ) ) ;
#44979 = CARTESIAN_POINT ( 'NONE',  ( 2.852642732684606663, -1.771934378248109399, -0.7286688389312511172 ) ) ;
#44980 = CARTESIAN_POINT ( 'NONE',  ( 4.229010956685672618, -1.930657356216297860, -0.7480826485904977785 ) ) ;
#44981 = CARTESIAN_POINT ( 'NONE',  ( 0.6823417656249899377, 2.655208333674753618, 1.181850606188767472 ) ) ;
#44982 = CARTESIAN_POINT ( 'NONE',  ( 2.096496217048297694, -0.5238668508756593178, -1.900535169118612755 ) ) ;
#44983 = CARTESIAN_POINT ( 'NONE',  ( 6.252564000042572623, 0.6067452241035797833, 1.828529084590237774 ) ) ;
#44984 = CARTESIAN_POINT ( 'NONE',  ( 2.904993682805886213, 1.579364189935757778, 1.002181356900035070 ) ) ;
#44986 = CARTESIAN_POINT ( 'NONE',  ( 4.626831674679969808, 8.450518883791096059, -0.3637425496919588497 ) ) ;
#44985 = CARTESIAN_POINT ( 'NONE',  ( 2.350585845863040646, 2.307203942772034111, 0.05475910514858049749 ) ) ;
#44987 = CARTESIAN_POINT ( 'NONE',  ( 2.892830138475974255, 0.2247066616481566970, 1.847348555264594960 ) ) ;
#44988 = CARTESIAN_POINT ( 'NONE',  ( -0.6823417656250212460, 2.301041667008084435, 1.181850606188767472 ) ) ;
#44989 = CARTESIAN_POINT ( 'NONE',  ( 6.109847269609326226, 0.6021898890512421554, -1.972802226155190297 ) ) ;
#44990 = CARTESIAN_POINT ( 'NONE',  ( -4.843287188579803448, 6.673587691474970107, -1.599625672291256295 ) ) ;
#44991 = CARTESIAN_POINT ( 'NONE',  ( 5.764187864104357573, 9.876636274763768597, 1.040834085586084257E-14 ) ) ;
#44992 = CARTESIAN_POINT ( 'NONE',  ( -1.364708430267705497, 4.015407764754321818, 0.6235921627254642496 ) ) ;
#44993 = CARTESIAN_POINT ( 'NONE',  ( 6.352575683687115671, 0.6571560004794211318, 2.000881423421707161 ) ) ;
#44994 = CARTESIAN_POINT ( 'NONE',  ( 1.364683531249988535, 4.467708333674754506, -0.7879004041258300672 ) ) ;
#44995 = CARTESIAN_POINT ( 'NONE',  ( 5.571600594950134600, 2.084881007647599205, -0.5705972643132786182 ) ) ;
#44996 = CARTESIAN_POINT ( 'NONE',  ( 6.340491327343366734, 1.161156619345372842, -1.652315300818160582 ) ) ;
#44997 = CARTESIAN_POINT ( 'NONE',  ( -1.364683531250014514, 0.03020833367475737191, 0.7879004041258379498 ) ) ;
#44998 = CARTESIAN_POINT ( 'NONE',  ( -3.606105671554953318, 7.150947683548662503, 0.7216878364870317197 ) ) ;
#44999 = ADVANCED_FACE ( 'NONE', ( #56419 ), #41663, .F. ) ;
#45002 = CARTESIAN_POINT ( 'NONE',  ( 4.636525346193557162, 7.392734756325715750, -1.082531754730549078 ) ) ;
#45001 = CARTESIAN_POINT ( 'NONE',  ( -3.285556943750000070, -0.1093749995220438809, 0.000000000000000000 ) ) ;
#45000 = CARTESIAN_POINT ( 'NONE',  ( 5.200434439293556643, 8.224868058221247225, -1.199719254218452047 ) ) ;
#45003 =( BOUNDED_CURVE ( )  B_SPLINE_CURVE ( 2, ( #154596, #152454, #67959, #203307, #84246, #134103, #122178, #38707, #51763 ),
 .UNSPECIFIED., .F., .T. ) 
 B_SPLINE_CURVE_WITH_KNOTS ( ( 3, 2, 2, 2, 3 ),
 ( 0.4375000000000000000, 0.4404761904761904656, 0.4464285714285714524, 0.4523809523809523836, 0.4553571428571427937 ),
 .UNSPECIFIED. ) 
 CURVE ( )  GEOMETRIC_REPRESENTATION_ITEM ( )  RATIONAL_B_SPLINE_CURVE ( ( 0.9330127018922194093, 0.9330127018922194093, 1.000000000000000000, 0.8660254037844387076, 1.000000000000000000, 0.8660254037844387076, 1.000000000000000000, 0.9330127018922206306, 0.9330127018922194093 ) ) 
 REPRESENTATION_ITEM ( '' )  );
#45004 = CARTESIAN_POINT ( 'NONE',  ( -2.428612866367529932E-14, 2.999999999999999112, 2.420000000000000373 ) ) ;
#45005 = CARTESIAN_POINT ( 'NONE',  ( 4.786342355033275986, -0.6839347017603314427, -1.897111394664739326 ) ) ;
#45006 = CARTESIAN_POINT ( 'NONE',  ( -6.744291347794091784, 9.955758108146730123, -1.199719254218440723 ) ) ;
#45008 = CARTESIAN_POINT ( 'NONE',  ( -7.580417283372126391, 8.016444050121833698, 0.7216878364870317197 ) ) ;
#45007 = CARTESIAN_POINT ( 'NONE',  ( -8.595506201384022660, 11.05117653974661529, 1.443375672974064550 ) ) ;
#45009 = FACE_OUTER_BOUND ( 'NONE', #131287, .T. ) ;
#45011 = CARTESIAN_POINT ( 'NONE',  ( -1.364683531250010740, 9.130208333674731946, 0.7879004041258445001 ) ) ;
#45010 = CARTESIAN_POINT ( 'NONE',  ( 5.752838164830007983, -1.706859214253673152, 1.326403591387192771 ) ) ;
#45012 = CARTESIAN_POINT ( 'NONE',  ( -11.81905481421901705, 13.75735655617264896, 1.592167362352176818 ) ) ;
#45013 = CARTESIAN_POINT ( 'NONE',  ( -8.462260433223891098, 13.02438760540324481, -0.7998128361456281477 ) ) ;
#45015 = CARTESIAN_POINT ( 'NONE',  ( 0.06975588353394339414, -0.9023057962903738849, 1.689756990376343859 ) ) ;
#45014 = CARTESIAN_POINT ( 'NONE',  ( -5.680503174001480637, 9.571078103069643461, 0.7216878364870458196 ) ) ;
#45016 = CARTESIAN_POINT ( 'NONE',  ( 1.364683531249986537, -0.7822916663252464931, -0.7879004041258309554 ) ) ;
#45017 = DIRECTION ( 'NONE',  ( 0.000000000000000000, 1.000000000000000000, -3.330669073875479482E-16 ) ) ;
#45018 = CARTESIAN_POINT ( 'NONE',  ( 2.261930500750704454, 0.7363377991795038158, 1.559957641100855330 ) ) ;
#45019 = CARTESIAN_POINT ( 'NONE',  ( 4.598150373690133463, 5.393538853173795111, -1.199719254218452047 ) ) ;
#45020 = CARTESIAN_POINT ( 'NONE',  ( 6.313256805818848960, 7.394496357324014113, 1.199719254218452047 ) ) ;
#45021 = CARTESIAN_POINT ( 'NONE',  ( -11.90610347052960627, 8.844549510192225128, 1.527030362374957262 ) ) ;
#45022 = CARTESIAN_POINT ( 'NONE',  ( 0.9304724923206836307, 0.1222484634449630542, 1.765570801851876537 ) ) ;
#45023 = CARTESIAN_POINT ( 'NONE',  ( 2.121741512283023656, -0.4388329339449773547, 1.964535544105987075 ) ) ;
#45024 = CARTESIAN_POINT ( 'NONE',  ( -4.829398645541163937, 4.822074999085563363, -0.2304323518458932241 ) ) ;
#45025 = CARTESIAN_POINT ( 'NONE',  ( 4.436686946050734548, 2.163524548302516060, 0.4339203326570104102 ) ) ;
#45026 = CARTESIAN_POINT ( 'NONE',  ( 5.875877563635198975, -2.119900239643329964, 0.4680052475878637708 ) ) ;
#45027 = ORIENTED_EDGE ( 'NONE', *, *, #204793, .T. ) ;
#45028 = CARTESIAN_POINT ( 'NONE',  ( 3.410758162289653672, 6.136912401716668519, -1.199719254218453823 ) ) ;
#45029 = CARTESIAN_POINT ( 'NONE',  ( 8.554831740098659765, 10.04335378727902395, 1.082531754730558626 ) ) ;
#45031 = CARTESIAN_POINT ( 'NONE',  ( 2.759388848745081280, 1.913798524274639812, -0.6352183541234107667 ) ) ;
#45030 = CARTESIAN_POINT ( 'NONE',  ( 3.703867829435038228, 1.536975034498413439, 1.461131120854219700 ) ) ;
#45033 = VERTEX_POINT ( 'NONE', #143041 ) ;
#45032 = CARTESIAN_POINT ( 'NONE',  ( 2.865264419611464941, -1.483432276133073380, -1.039550242524535539 ) ) ;
#45034 = CARTESIAN_POINT ( 'NONE',  ( 6.873057527484919937, 6.983264968346048818, 0.7998128361456352531 ) ) ;
#45035 = ORIENTED_EDGE ( 'NONE', *, *, #149161, .T. ) ;
#45036 = PRESENTATION_LAYER_ASSIGNMENT (  '', '', ( #180002 ) ) ;
#45037 = CARTESIAN_POINT ( 'NONE',  ( 0.1275333129481092398, -1.147091320445620566, -1.478225367208672481 ) ) ;
#45038 = CARTESIAN_POINT ( 'NONE',  ( 6.962275575817444384, 8.081408578997208991, -1.199719254218446718 ) ) ;
#45039 = CARTESIAN_POINT ( 'NONE',  ( 5.865807274569020180, 1.797851641234180509, -0.3166982042408575948 ) ) ;
#45041 = CARTESIAN_POINT ( 'NONE',  ( 1.604551054648394537, 1.788909703809701712, 0.6859268596576766353 ) ) ;
#45040 = CARTESIAN_POINT ( 'NONE',  ( -2.754277761870538299, 6.365074488824250309, 1.040834085586084257E-14 ) ) ;
#45042 = CARTESIAN_POINT ( 'NONE',  ( 0.3869736770896747835, 1.794419290072776896, -11.79366332131311523 ) ) ;
#45043 = CARTESIAN_POINT ( 'NONE',  ( 11.07790593930098311, 11.29999999999999893, 0.6999999999999992895 ) ) ;
#45044 = CARTESIAN_POINT ( 'NONE',  ( -0.6823417656250003738, 2.030208333674753174, -1.181850606188749264 ) ) ;
#45045 = DIRECTION ( 'NONE',  ( 0.6507913734559640506, -0.7592566023653004592, 0.000000000000000000 ) ) ;
#45046 = CARTESIAN_POINT ( 'NONE',  ( -6.984421689334302741, 11.30024240419870374, 0.000000000000000000 ) ) ;
#45047 = EDGE_CURVE ( 'NONE', #148930, #60029, #132816, .T. ) ;
#45048 = CARTESIAN_POINT ( 'NONE',  ( 5.735289742212391850, -1.956171686333206816, 0.9202595734885756773 ) ) ;
#45049 = CARTESIAN_POINT ( 'NONE',  ( -5.831415467653581430, 5.975941931783510519, 0.7216878364870257245 ) ) ;
#45050 = CARTESIAN_POINT ( 'NONE',  ( -5.915100157312088491, 10.12297696016459092, -0.7998128361456362523 ) ) ;
#45051 = CARTESIAN_POINT ( 'NONE',  ( 3.568700945156903614, 0.7666329941097769218, 1.977337035738421900 ) ) ;
#45053 = CARTESIAN_POINT ( 'NONE',  ( -12.40260256363088942, 6.580881934270854217, 3.466095386915876819 ) ) ;
#45052 = FACE_OUTER_BOUND ( 'NONE', #205990, .T. ) ;
#45054 = CARTESIAN_POINT ( 'NONE',  ( 4.639890180388304586, 0.8457560770286243201, -1.780867954887039417 ) ) ;
#45055 = CARTESIAN_POINT ( 'NONE',  ( -0.1931356145602729502, -0.4479747710816587292, -1.970277229543435427 ) ) ;
#45056 = VERTEX_POINT ( 'NONE', #210108 ) ;
#45057 = CARTESIAN_POINT ( 'NONE',  ( 5.366459209908462036, -2.066393128712967098, -0.4610789482254721294 ) ) ;
#45059 = EDGE_CURVE ( 'NONE', #39684, #124676, #89257, .T. ) ;
#45058 = CARTESIAN_POINT ( 'NONE',  ( 5.275531169048896629, 7.248148678680751189, -1.443375672974078316 ) ) ;
#45060 = CARTESIAN_POINT ( 'NONE',  ( 0.7310241076574041097, -1.948878508384953356, -0.6990896207654460071 ) ) ;
#45061 = CARTESIAN_POINT ( 'NONE',  ( 2.132666086734685162, -1.734545437858775463, 0.8733739462151270949 ) ) ;
#45062 = EDGE_LOOP ( 'NONE', ( #48259, #139017, #66044, #104952 ) ) ;
#45063 = CARTESIAN_POINT ( 'NONE',  ( -2.972980823146582186, 6.690504403638126263, 0.000000000000000000 ) ) ;
#45064 = CARTESIAN_POINT ( 'NONE',  ( 5.013482942003290255, 9.071090208970993274, -0.7998128361456481317 ) ) ;
#45066 = CARTESIAN_POINT ( 'NONE',  ( 6.144869935491714230, 8.192100896205568361, -1.599625672291262513 ) ) ;
#45065 = CARTESIAN_POINT ( 'NONE',  ( 3.117214558520535306, -2.014654392230078805, 0.5582205872023697779 ) ) ;
#45067 = CARTESIAN_POINT ( 'NONE',  ( 5.031484404002891431, 5.042689024191078673, 0.7216878364870328300 ) ) ;
#45069 = VERTEX_POINT ( 'NONE', #84118 ) ;
#45068 = CARTESIAN_POINT ( 'NONE',  ( 0.09988412287174981696, -0.8557525428138833545, 1.596560661436140283 ) ) ;
#45070 = CARTESIAN_POINT ( 'NONE',  ( 6.094375512030342001, -2.195847865938059140, -0.2203403561373064590 ) ) ;
#45071 = CARTESIAN_POINT ( 'NONE',  ( -0.4694063952341876456, -6.700000000000002842, -10.98997987423603107 ) ) ;
#45072 = CARTESIAN_POINT ( 'NONE',  ( 2.819571115601596123, -0.2173934082839618365, 2.196046946737562511 ) ) ;
#45073 = CARTESIAN_POINT ( 'NONE',  ( 8.229962938695207342, 9.560377169021284871, 1.199719254218462483 ) ) ;
#45074 = DIRECTION ( 'NONE',  ( 0.000000000000000000, 0.000000000000000000, -1.000000000000000000 ) ) ;
#45075 = CARTESIAN_POINT ( 'NONE',  ( 1.857924044808876296, 0.7306008629870773818, -1.767408594711167735 ) ) ;
#45076 = CIRCLE ( 'NONE', #128178, 12.00000000000000355 ) ;
#45077 = CARTESIAN_POINT ( 'NONE',  ( 8.048736748007069508, 12.54194330598362406, -0.7998128361456352531 ) ) ;
#45078 = CARTESIAN_POINT ( 'NONE',  ( 5.406714943436663035, 0.5975561702324573288, 1.982271326387271770 ) ) ;
#45080 = CARTESIAN_POINT ( 'NONE',  ( 2.729541802387557059, -2.017400560480298033, 0.7770373237434913261 ) ) ;
#45079 = CARTESIAN_POINT ( 'NONE',  ( -2.819205876637805641, 5.376491725131008259, -1.199719254218446718 ) ) ;
#45081 = CARTESIAN_POINT ( 'NONE',  ( 4.739868811304373430, 2.185674081084403753, 0.1610935195608814985 ) ) ;
#45082 = ORIENTED_EDGE ( 'NONE', *, *, #188457, .F. ) ;
#45083 = CARTESIAN_POINT ( 'NONE',  ( 8.550388431712704573, 13.12720360364021133, 0.000000000000000000 ) ) ;
#45084 = CARTESIAN_POINT ( 'NONE',  ( 4.059580577656426215, 7.665954309842628156, -0.5688408669104396687 ) ) ;
#45085 = CARTESIAN_POINT ( 'NONE',  ( -0.2184521437216538908, 7.205153265248401162, 1.990034439536109145 ) ) ;
#45086 = CARTESIAN_POINT ( 'NONE',  ( 5.200434439293556643, 8.224868058221247225, -1.199719254218452047 ) ) ;
#45087 = CARTESIAN_POINT ( 'NONE',  ( 3.285556943750000070, -3.171874999522043215, 0.000000000000000000 ) ) ;
#45088 = CARTESIAN_POINT ( 'NONE',  ( -3.006876207180748217, 6.730049018344652190, -0.7998128361456481317 ) ) ;
#45089 = CARTESIAN_POINT ( 'NONE',  ( 0.7740648250077889481, 1.777010169924503558, -0.9530137779002674225 ) ) ;
#45090 = ADVANCED_FACE ( 'NONE', ( #46579, #112698 ), #10841, .T. ) ;
#45091 = CARTESIAN_POINT ( 'NONE',  ( -8.351459436338030784, 11.72682452816096976, -1.082531754730543971 ) ) ;
#45092 = CARTESIAN_POINT ( 'NONE',  ( 6.561219994370630637, 6.619454513046008515, 0.000000000000000000 ) ) ;
#45093 = CARTESIAN_POINT ( 'NONE',  ( 4.873920291170623642, -2.031351322358550870, 0.3986081187722507746 ) ) ;
#45094 = CARTESIAN_POINT ( 'NONE',  ( 3.773980605468800320, 1.071039916736727937, 1.601146377209327731 ) ) ;
#45095 = CARTESIAN_POINT ( 'NONE',  ( -0.08826282632121498772, -1.242921985031696153, -1.588411632956095110 ) ) ;
#45096 = CARTESIAN_POINT ( 'NONE',  ( -9.110189153378817295, 12.71597221466224603, 1.199719254218462483 ) ) ;
#45097 = CARTESIAN_POINT ( 'NONE',  ( 5.823390672269506574, 6.752709524857930745, -1.199719254218446718 ) ) ;
#45098 = CARTESIAN_POINT ( 'NONE',  ( 9.681502974757703939, 4.134313097118708313, 7.090028219590145397 ) ) ;
#45099 = CARTESIAN_POINT ( 'NONE',  ( 3.625798818847306038, 1.922417080405220968, -0.4270903664440502956 ) ) ;
#45100 = CARTESIAN_POINT ( 'NONE',  ( 0.5159075615763093481, -1.175655012515547160, -1.849222068403690411 ) ) ;
#45101 = CARTESIAN_POINT ( 'NONE',  ( 3.668406916800326378, -1.225078373119498965, 1.353803248016254956 ) ) ;
#45102 = CARTESIAN_POINT ( 'NONE',  ( 7.349928672384119288, 8.707909884937221179, 1.082531754730549967 ) ) ;
#45103 = CARTESIAN_POINT ( 'NONE',  ( 2.535011535630975477, 5.901337858304024131, 0.7216878364870438212 ) ) ;
#45104 = CARTESIAN_POINT ( 'NONE',  ( -5.582925393777276035, 9.735439736040634173, 0.7998128361456291469 ) ) ;
#45105 = CARTESIAN_POINT ( 'NONE',  ( 4.960304097753311936, 6.880383762169266504, 1.599625672291268286 ) ) ;
#45106 = VERTEX_POINT ( 'NONE', #176569 ) ;
#45108 = CARTESIAN_POINT ( 'NONE',  ( 5.642843092333371224, 1.941422931094261450, 0.5326616679640855390 ) ) ;
#45107 = CARTESIAN_POINT ( 'NONE',  ( 1.311775528174640604, 1.236260529797410301, -1.364685630449238740 ) ) ;
#45109 = CARTESIAN_POINT ( 'NONE',  ( 0.7557052203445973060, -2.281327611594321958, -0.2792575881873406440 ) ) ;
#45110 = CARTESIAN_POINT ( 'NONE',  ( 5.278158119090741174, -1.046208158741080529, -1.659298866772864534 ) ) ;
#45111 = CARTESIAN_POINT ( 'NONE',  ( -5.357443255694392725, 9.402100898285455699, 0.000000000000000000 ) ) ;
#45112 = DIRECTION ( 'NONE',  ( -3.330669073875478989E-16, 3.330669073875478989E-16, 1.000000000000000000 ) ) ;
#45113 = CARTESIAN_POINT ( 'NONE',  ( -3.490334480514268645, 6.159475096320226939, -1.199719254218452935 ) ) ;
#45114 = CARTESIAN_POINT ( 'NONE',  ( -10.30923643716948490, 0.9706168436483916251, -5.952040432139263260 ) ) ;
#45115 = CARTESIAN_POINT ( 'NONE',  ( -6.147696309153835692, 6.137010213626392208, 0.7998128361456281477 ) ) ;
#45117 = CARTESIAN_POINT ( 'NONE',  ( 6.473528777534793832, 1.692185636751794897, -0.5185713626470798143 ) ) ;
#45116 = CARTESIAN_POINT ( 'NONE',  ( 0.9430502156211654219, -1.650385480578796749, -1.283440319295367615 ) ) ;
#45118 = CARTESIAN_POINT ( 'NONE',  ( -1.284279953904156280, 2.921639714193936754, 0.7750000000000117906 ) ) ;
#45119 = CARTESIAN_POINT ( 'NONE',  ( -0.2104748580754409182, 6.947232144882289795, -2.698723162346649662 ) ) ;
#45120 = CARTESIAN_POINT ( 'NONE',  ( 1.522608870468153741, -1.638875412371978646, 0.5861679430564836757 ) ) ;
#45121 = CARTESIAN_POINT ( 'NONE',  ( 4.625302960556422427, 8.547937220624488575, 1.040834085586084257E-14 ) ) ;
#45123 = DIRECTION ( 'NONE',  ( 0.000000000000000000, 8.546850786086437571E-32, 1.000000000000000000 ) ) ;
#45122 = CARTESIAN_POINT ( 'NONE',  ( 3.999999999995414152E-05, 14.55305236562591098, 11.95586206891494996 ) ) ;
#45124 = CARTESIAN_POINT ( 'NONE',  ( 1.769703478646069028, 0.8846387809394311574, 1.480598516496567152 ) ) ;
#45125 = CARTESIAN_POINT ( 'NONE',  ( 1.540847765565691585, -1.849059859674206496, 1.176127931831471907 ) ) ;
#45126 = CARTESIAN_POINT ( 'NONE',  ( 4.336686996305870068, 2.164023489887345164, 0.4319772483800735086 ) ) ;
#45127 = DIRECTION ( 'NONE',  ( 0.000000000000000000, 1.000000000000000000, -8.673617379884026597E-16 ) ) ;
#45128 = CARTESIAN_POINT ( 'NONE',  ( 2.254941745292405653, -0.5755891407489240885, -2.093346358694737841 ) ) ;
#45129 = CARTESIAN_POINT ( 'NONE',  ( 0.8205984872286451459, 1.685833220154912881, 0.7012733028506010768 ) ) ;
#45130 = CARTESIAN_POINT ( 'NONE',  ( 3.169268314845040901, 1.912196763353574358, -0.9095376832224701946 ) ) ;
#45131 = CARTESIAN_POINT ( 'NONE',  ( 6.539320575229256249, 6.039323383297771741, 2.391644441267444687 ) ) ;
#45132 = ORIENTED_EDGE ( 'NONE', *, *, #208519, .F. ) ;
#45134 = CARTESIAN_POINT ( 'NONE',  ( -1.402160292154681736E-14, 0.009375000341421267647, -1.575800808251665908 ) ) ;
#45133 = CARTESIAN_POINT ( 'NONE',  ( 4.195090427499806651, 1.841111018879896477, 1.365591311898015192 ) ) ;
#45135 = SURFACE_STYLE_FILL_AREA ( #194550 ) ;
#45136 = CARTESIAN_POINT ( 'NONE',  ( 4.729096653068339151, 4.411700938201493116, -0.7998128361456211532 ) ) ;
#45137 = CARTESIAN_POINT ( 'NONE',  ( 6.094412736144367848, -1.190704872505081946, 1.875028197947399278 ) ) ;
#45138 = CARTESIAN_POINT ( 'NONE',  ( -6.887178846062123938, 8.097758744236356776, -1.082531754730544860 ) ) ;
#45139 = CARTESIAN_POINT ( 'NONE',  ( 4.039966587192250103, 7.657118751792200584, 0.7216878364870298324 ) ) ;
#45140 = CARTESIAN_POINT ( 'NONE',  ( -6.358410854684777291, 10.36197039720016022, -0.7216878364870267237 ) ) ;
#45141 = CARTESIAN_POINT ( 'NONE',  ( 3.919715808126649659, 7.587102519540811940, 0.000000000000000000 ) ) ;
#45142 = ORIENTED_EDGE ( 'NONE', *, *, #5562, .T. ) ;
#45143 = CARTESIAN_POINT ( 'NONE',  ( 4.254529844270301453, 1.955172953530256219, -0.4926405443339901269 ) ) ;
#45145 = CARTESIAN_POINT ( 'NONE',  ( 2.483324480268500611, -0.004404232681418790429, 2.062741127353195925 ) ) ;
#45144 = CARTESIAN_POINT ( 'NONE',  ( 7.122110765880372618, 7.203550736482235095, 0.7998128361456341429 ) ) ;
#45146 = CARTESIAN_POINT ( 'NONE',  ( -2.788906526875773208E-15, 12.43750000000000000, -1.499999999999998446 ) ) ;
#45147 = CARTESIAN_POINT ( 'NONE',  ( 4.706088717274895750, 6.583799151611112954, 1.443375672974065660 ) ) ;
#45148 = CARTESIAN_POINT ( 'NONE',  ( -1.642778471875000035, -2.267708332855375541, -2.845375778867859751 ) ) ;
#45149 = CARTESIAN_POINT ( 'NONE',  ( -1.001543065824772872E-14, 4.571875000341418804, 1.575800808251672791 ) ) ;
#45150 = CARTESIAN_POINT ( 'NONE',  ( 4.998067021457727854, -0.7363416341295281331, -2.064161796032103258 ) ) ;
#45151 = CARTESIAN_POINT ( 'NONE',  ( 2.865861461037176205, -0.1511401116795624278, -2.010826411938296143 ) ) ;
#45152 = CARTESIAN_POINT ( 'NONE',  ( 1.716098596715152746, 1.718394358364897068, 0.6617865747741287219 ) ) ;
#45153 = CARTESIAN_POINT ( 'NONE',  ( 7.416473721875251890, 8.611306416064660851, 1.199719254218462483 ) ) ;
#45154 = CARTESIAN_POINT ( 'NONE',  ( 6.668987789458199700, -1.670617902683011025, -0.7365018021969899076 ) ) ;
#45155 = CARTESIAN_POINT ( 'NONE',  ( 6.381482430641396419, -0.5404875331735843336, -1.942542459342583294 ) ) ;
#45156 = CARTESIAN_POINT ( 'NONE',  ( -6.177711549321182716, 10.35908057418338402, 0.7998128361456481317 ) ) ;
#45158 = CARTESIAN_POINT ( 'NONE',  ( -4.142898457427624415, 6.991076079377632091, 1.199719254218452935 ) ) ;
#45157 = CARTESIAN_POINT ( 'NONE',  ( 5.295900185863533061, -0.8195587353489269811, 2.109036902066116603 ) ) ;
#45159 = CARTESIAN_POINT ( 'NONE',  ( 1.260533433194007236, 0.8550034467163977192, 1.924895685913818655 ) ) ;
#45160 = CARTESIAN_POINT ( 'NONE',  ( -7.910256278930404505, 8.193330178365746619, -0.7998128361456362523 ) ) ;
#45161 = CARTESIAN_POINT ( 'NONE',  ( 7.293396569147545527, 10.59638086639245280, 1.199719254218460707 ) ) ;
#45162 = CARTESIAN_POINT ( 'NONE',  ( 6.577113915960825175, 8.766661883411348555, -1.443375672974078761 ) ) ;
#45163 = DIRECTION ( 'NONE',  ( -0.008473495442210265960, -2.748389711249667622E-16, -0.9999640992930650674 ) ) ;
#45164 = CARTESIAN_POINT ( 'NONE',  ( -8.362681821530818738, 8.650883634741092010, -0.7998128361456291469 ) ) ;
#45165 = UNCERTAINTY_MEASURE_WITH_UNIT (LENGTH_MEASURE( 1.000000000000000082E-05 ), #210151, 'distance_accuracy_value', 'NONE');
#45166 = CARTESIAN_POINT ( 'NONE',  ( -3.795153912786186634, 7.352191159395610853, -0.7064407198300488577 ) ) ;
#45167 = CARTESIAN_POINT ( 'NONE',  ( 7.090551149822735155, 9.295395646258437949, 1.443375672974076540 ) ) ;
#45168 = CARTESIAN_POINT ( 'NONE',  ( 4.061730550730160871, 7.744580798899280971, -0.5443347154160914636 ) ) ;
#45169 = CARTESIAN_POINT ( 'NONE',  ( -9.219181267612684749, 10.81842823604534765, 1.082531754730558626 ) ) ;
#45171 = CARTESIAN_POINT ( 'NONE',  ( 3.199698422319953384, 2.006668028495290024, -0.9531968752462171013 ) ) ;
#45170 = CARTESIAN_POINT ( 'NONE',  ( 1.898838059644195386, -2.080654286433290867, -0.4088066060855889972 ) ) ;
#45172 = CARTESIAN_POINT ( 'NONE',  ( -5.608757509019812737, 5.629195651549657065, 0.4603112365162060904 ) ) ;
#45173 = CARTESIAN_POINT ( 'NONE',  ( -5.641074431737709283, 8.738948049406083385, -1.199719254218452047 ) ) ;
#45174 = CARTESIAN_POINT ( 'NONE',  ( 6.962275575817444384, 8.081408578997208991, -1.199719254218446718 ) ) ;
#45175 = CARTESIAN_POINT ( 'NONE',  ( 4.756279191188107269, -1.961398630904508833, -0.05015466537350299348 ) ) ;
#45176 = CARTESIAN_POINT ( 'NONE',  ( 10.24048609702354717, 10.84165528948263457, -0.7998128361456281477 ) ) ;
#45177 = CARTESIAN_POINT ( 'NONE',  ( -4.698067037153471404, 6.865000302791745668, 1.228424997642649563 ) ) ;
#45178 = CARTESIAN_POINT ( 'NONE',  ( 4.681643115420508039, 4.356338477612361260, 0.7998128361456341429 ) ) ;
#45179 = CARTESIAN_POINT ( 'NONE',  ( -3.851925040058333582, 7.508013290127760087, -0.7216878364870458196 ) ) ;
#45181 = VERTEX_POINT ( 'NONE', #153393 ) ;
#45180 = CARTESIAN_POINT ( 'NONE',  ( -6.643132081016132062, 8.773406732650713025, 1.443375672974078761 ) ) ;
#45182 = CARTESIAN_POINT ( 'NONE',  ( 3.568700945156903614, 0.7666329941097769218, 1.977337035738421900 ) ) ;
#45183 = CARTESIAN_POINT ( 'NONE',  ( -6.120580001926503755, 6.105374521861167914, -0.7998128361456362523 ) ) ;
#45184 = CARTESIAN_POINT ( 'NONE',  ( 4.873979933848565871, 1.241796773192262116, 1.769252301715443565 ) ) ;
#45185 = CARTESIAN_POINT ( 'NONE',  ( 4.440845869443198701, -1.426288408191313639, -1.164454570719307469 ) ) ;
#45186 = CARTESIAN_POINT ( 'NONE',  ( -4.820845164874406841, 6.759277571458118139, 1.248045366310134741 ) ) ;
#45187 = CARTESIAN_POINT ( 'NONE',  ( 1.364683531249988757, -0.05312499965857975237, 0.000000000000000000 ) ) ;
#45188 = CARTESIAN_POINT ( 'NONE',  ( 6.052664191884576717, -1.496297717267160765, -0.8884939375988825105 ) ) ;
#45189 = FACE_OUTER_BOUND ( 'NONE', #202558, .T. ) ;
#45190 = CARTESIAN_POINT ( 'NONE',  ( 4.880572111239557920, 4.796348339308675435, -0.7216878364870197293 ) ) ;
#45192 = ADVANCED_FACE ( 'NONE', ( #2840 ), #130296, .T. ) ;
#45191 = STYLED_ITEM ( 'NONE', ( #57089 ), #162819 ) ;
#45193 = CARTESIAN_POINT ( 'NONE',  ( 3.327187652246216931, 0.05129554954072869377, 2.161254785723889515 ) ) ;
#45194 = CARTESIAN_POINT ( 'NONE',  ( 6.134138708105167481, 0.1511139231759016377, -2.010518800921741622 ) ) ;
#45195 = CARTESIAN_POINT ( 'NONE',  ( -7.795575137733361970, 12.03866206075687018, 0.7216878364870458196 ) ) ;
#45196 = CARTESIAN_POINT ( 'NONE',  ( 2.061604318190731533, 0.3698614785779800185, -2.129673623264888960 ) ) ;
#45197 = CARTESIAN_POINT ( 'NONE',  ( 3.356668533229437923, -1.495150621271496671, 1.284956859879735402 ) ) ;
#45198 = CARTESIAN_POINT ( 'NONE',  ( 2.887907956677421506, -2.014008092954455265, 0.1037802451031161477 ) ) ;
#45199 = CARTESIAN_POINT ( 'NONE',  ( 0.1522426329377546128, 0.8445714516599597266, 2.022489037641273857 ) ) ;
#45200 = CARTESIAN_POINT ( 'NONE',  ( 4.880387366230515944, -0.2415804104359954019, -1.926931144411721641 ) ) ;
#45202 = EDGE_LOOP ( 'NONE', ( #102903, #4276, #100395, #67535, #51300 ) ) ;
#45201 = CARTESIAN_POINT ( 'NONE',  ( -9.964879715919934711, 10.72804054476916313, 0.7216878364870438212 ) ) ;
#45203 = CARTESIAN_POINT ( 'NONE',  ( -6.967964602780620353, 7.093989889524320525, 0.000000000000000000 ) ) ;
#45204 = CARTESIAN_POINT ( 'NONE',  ( 11.78331023100045272, 9.799999999999982947, 1.799999999999999600 ) ) ;
#45206 = VERTEX_POINT ( 'NONE', #18704 ) ;
#45205 = CARTESIAN_POINT ( 'NONE',  ( -5.655686355556086120, 6.627330832017406692, 1.199719254218452935 ) ) ;
#45207 = CARTESIAN_POINT ( 'NONE',  ( -8.812436658758329600, 9.383523644747281622, 1.040834085586084257E-14 ) ) ;
#45208 = CARTESIAN_POINT ( 'NONE',  ( 1.729795059504362076, -2.077734391967264838, 0.7439406459070623256 ) ) ;
#45209 = CARTESIAN_POINT ( 'NONE',  ( -1.642778471875000035, -1.217708332855376607, -2.845375778867859751 ) ) ;
#45210 = CARTESIAN_POINT ( 'NONE',  ( 5.981297772519294398, -0.05168599705708888659, 1.961257141919122926 ) ) ;
#45211 = CARTESIAN_POINT ( 'NONE',  ( 1.364683531249992088, 5.696875000341418804, 1.214306433183764966E-14 ) ) ;
#45212 = CARTESIAN_POINT ( 'NONE',  ( -1.500000000000013101, 4.160416667349482900, -0.8660254037844313801 ) ) ;
#45213 = CARTESIAN_POINT ( 'NONE',  ( 5.250185332887272516, 6.604911474350376288, -1.376424501724478944 ) ) ;
#45214 = DIRECTION ( 'NONE',  ( -0.000000000000000000, -1.000000000000000000, -0.000000000000000000 ) ) ;
#45215 = CARTESIAN_POINT ( 'NONE',  ( 4.945164379994194448, 0.5744887182440976403, -1.749284230371531024 ) ) ;
#45216 = VERTEX_POINT ( 'NONE', #70642 ) ;
#45217 = CARTESIAN_POINT ( 'NONE',  ( 1.224999999999971001, 2.708333334016145066, -0.7072540797573036997 ) ) ;
#45218 = CARTESIAN_POINT ( 'NONE',  ( -6.184490626128011925, 10.36698949712469364, -0.7998128361456291469 ) ) ;
#45219 = CARTESIAN_POINT ( 'NONE',  ( 7.767011945534265216, -7.169578370797519362, -7.110792111438882124 ) ) ;
#45220 = CARTESIAN_POINT ( 'NONE',  ( 5.853796514643677007, -1.537196951383312804, -1.461068456062891041 ) ) ;
#45221 = DIRECTION ( 'NONE',  ( 1.000000000000000000, 0.000000000000000000, 0.000000000000000000 ) ) ;
#45222 = CARTESIAN_POINT ( 'NONE',  ( 3.472859903394816872, 7.203420320602605287, -0.7998128361456291469 ) ) ;
#45223 = CARTESIAN_POINT ( 'NONE',  ( 6.186805567823734364, -0.2977626877682394424, -2.039013576910824632 ) ) ;
#45226 = CARTESIAN_POINT ( 'NONE',  ( 3.245484093776138668, 1.841430844176932480, -0.003062914905635482320 ) ) ;
#45225 = CARTESIAN_POINT ( 'NONE',  ( 1.855673809551155795, -0.6311025070286357952, 1.750906552266822569 ) ) ;
#45224 = DIRECTION ( 'NONE',  ( -0.8164965809277378028, 2.168827410163043206E-15, -0.5773502691896092998 ) ) ;
#45227 = CARTESIAN_POINT ( 'NONE',  ( 5.621827251160867789, 9.710548892996357040, 1.040834085586084257E-14 ) ) ;
#45228 = CARTESIAN_POINT ( 'NONE',  ( -5.064290697676250730, 7.960144884870772763, -1.236948567437242907 ) ) ;
#45229 = CARTESIAN_POINT ( 'NONE',  ( -7.282664789195997912, 8.525472337930658284, 1.199719254218452047 ) ) ;
#45231 = ORIENTED_EDGE ( 'NONE', *, *, #39272, .T. ) ;
#45230 = CARTESIAN_POINT ( 'NONE',  ( -6.484567079770452658, -6.583980363594976737, -7.100579091573040458 ) ) ;
#45232 = CARTESIAN_POINT ( 'NONE',  ( 3.299657469156279888, 1.739734091921738557, 1.357710657151039779 ) ) ;
#45233 = CARTESIAN_POINT ( 'NONE',  ( 5.571622904855764169, 2.182566619097675797, -0.5956038432519733528 ) ) ;
#45234 = CARTESIAN_POINT ( 'NONE',  ( -5.734735788900501952, 9.634349487118505806, 0.000000000000000000 ) ) ;
#45235 = CARTESIAN_POINT ( 'NONE',  ( 5.906502150075481516, -1.803732336900876421, -0.1683732622318224459 ) ) ;
#45236 = CARTESIAN_POINT ( 'NONE',  ( 6.298046708350548251, -0.9096110389208410529, -1.686033347247811731 ) ) ;
#45237 = CARTESIAN_POINT ( 'NONE',  ( 5.664887262500884368, -1.691755685069219695, -0.7986314380193232365 ) ) ;
#45238 = CARTESIAN_POINT ( 'NONE',  ( 5.672493831469004100, 0.7790509395085333244, 1.746586765831580124 ) ) ;
#45239 = CARTESIAN_POINT ( 'NONE',  ( -5.889704870869313602, 5.973669892210054400, 0.3102931194572235429 ) ) ;
#45240 = CARTESIAN_POINT ( 'NONE',  ( 0.6021629784135495989, -0.6261829430146518272, -1.762877433595814614 ) ) ;
#45241 = CARTESIAN_POINT ( 'NONE',  ( 1.253139057289072822, 0.1435168058863903473, -2.011451928166609893 ) ) ;
#45243 = CARTESIAN_POINT ( 'NONE',  ( 4.424511703531566198, 1.296206220603330461, -1.659847191385990239 ) ) ;
#45242 = CARTESIAN_POINT ( 'NONE',  ( -7.669108446824431269, 12.09904362127053545, -0.7998128361456291469 ) ) ;
#45244 = CARTESIAN_POINT ( 'NONE',  ( 8.235688245297327015, 11.69572115523387268, -1.199719254218446718 ) ) ;
#45246 = CARTESIAN_POINT ( 'NONE',  ( -9.677822722056413696, 10.18521468535430685, 1.040834085586084257E-14 ) ) ;
#45245 = CARTESIAN_POINT ( 'NONE',  ( -1.500000000000015099, -0.8291666666666407393, 0.8660254037844403729 ) ) ;
#45247 = CARTESIAN_POINT ( 'NONE',  ( -1.743066579297358008E-15, 2.250000000682787160, -1.225000000000020739 ) ) ;
#45248 = CARTESIAN_POINT ( 'NONE',  ( 3.357680014348028763, -1.532128950806666445, -1.316242992507418386 ) ) ;
#45249 = CARTESIAN_POINT ( 'NONE',  ( 0.6823417656249899377, 3.926041667008085767, -1.181850606188754593 ) ) ;
#45250 = CARTESIAN_POINT ( 'NONE',  ( 8.568389894156670294, 12.94027927658408217, -0.7216878364870257245 ) ) ;
#45251 = CARTESIAN_POINT ( 'NONE',  ( 3.444745247808535638, 0.5215555581963465803, 2.097624034931542703 ) ) ;
#45252 = CARTESIAN_POINT ( 'NONE',  ( 6.620655732516659064, 6.039214117936750448, 2.421170424969817603 ) ) ;
#45253 = CARTESIAN_POINT ( 'NONE',  ( 1.499999999999989120, 5.795833333333350268, -0.8660254037844323793 ) ) ;
#45254 = CARTESIAN_POINT ( 'NONE',  ( 7.180978637093494044, 8.406838493811077839, -1.199719254218452047 ) ) ;
#45255 = CARTESIAN_POINT ( 'NONE',  ( 8.310784975052673218, 10.71900177569337487, -1.443375672974063439 ) ) ;
#45257 = CARTESIAN_POINT ( 'NONE',  ( 8.908442372161164968, 14.67457862154163628, -8.041203192133428601 ) ) ;
#45256 = CARTESIAN_POINT ( 'NONE',  ( 0.3444781036854955847, -1.022991162849467228, 1.915094836987745630 ) ) ;
#45258 = CARTESIAN_POINT ( 'NONE',  ( -7.388830529767770550, 7.722649827591604677, 1.040834085586084257E-14 ) ) ;
#45259 = CARTESIAN_POINT ( 'NONE',  ( 0.6823417656249882723, 2.426041667008084435, -1.181850606188749264 ) ) ;
#45260 = CARTESIAN_POINT ( 'NONE',  ( 2.402122600552298870, -0.8417629408748151798, -2.023652355447076001 ) ) ;
#45261 = CARTESIAN_POINT ( 'NONE',  ( 6.883263157960369583, 7.629137130509070275, 2.653810918356712900 ) ) ;
#45262 = CARTESIAN_POINT ( 'NONE',  ( 3.063607368349754889, 0.3334396122402134011, -2.237705976790417939 ) ) ;
#45263 = CARTESIAN_POINT ( 'NONE',  ( -7.640183256500752584, 8.872300873127729304, -1.199719254218446718 ) ) ;
#45264 = CARTESIAN_POINT ( 'NONE',  ( -4.595850884908229794, 4.464173575255435011, 0.7216878364870317197 ) ) ;
#45265 = CARTESIAN_POINT ( 'NONE',  ( 0.6823417656249917140, 4.655208333674755394, 1.181850606188765695 ) ) ;
#45266 = CARTESIAN_POINT ( 'NONE',  ( 5.264264421420239870, 7.666326994050936428, 1.218248458220503094 ) ) ;
#45267 = CARTESIAN_POINT ( 'NONE',  ( 0.7500000000000006661, 11.83333333333333393, 1.299038105676657340 ) ) ;
#45268 = CARTESIAN_POINT ( 'NONE',  ( 7.078765600110826561, 8.391552967285011988, -1.082531754730548412 ) ) ;
#45269 = CARTESIAN_POINT ( 'NONE',  ( 4.569463179464338332, 1.716784003608927467, -0.4291735618162701438 ) ) ;
#45270 = CARTESIAN_POINT ( 'NONE',  ( 9.908311333488716954, 10.45411806535867782, 0.7998128361456462443 ) ) ;
#45271 = CARTESIAN_POINT ( 'NONE',  ( 0.8332068151313138937, 0.1548093300561304564, 2.100314307419436588 ) ) ;
#45272 = CARTESIAN_POINT ( 'NONE',  ( -0.6823417656250003738, 8.651041667008065872, 1.181850606188754593 ) ) ;
#45273 = CARTESIAN_POINT ( 'NONE',  ( -6.147696309153835692, 6.137010213626392208, 0.7998128361456281477 ) ) ;
#45274 = CARTESIAN_POINT ( 'NONE',  ( 6.081657687927014777, -0.6766999560612970699, 1.899624756701682626 ) ) ;
#45275 = EDGE_LOOP ( 'NONE', ( #51667, #65421 ) ) ;
#45276 = CARTESIAN_POINT ( 'NONE',  ( 10.57266086055835075, 11.22919251360659310, 0.000000000000000000 ) ) ;
#45277 = CARTESIAN_POINT ( 'NONE',  ( 4.240975883383619305, -1.627667033997456381, 0.9218181776217827528 ) ) ;
#45278 = CARTESIAN_POINT ( 'NONE',  ( 2.870052101067874339, -2.048368873657464118, 0.2992715783270774588 ) ) ;
#45279 = CIRCLE ( 'NONE', #207754, 0.09999999999999982514 ) ;
#45280 = CARTESIAN_POINT ( 'NONE',  ( -5.221298554594238084, 8.145246509451649075, 1.082531754730549967 ) ) ;
#45281 = CARTESIAN_POINT ( 'NONE',  ( 8.052653171512838881, 11.48218023581863001, -1.199719254218446718 ) ) ;
#45282 = CARTESIAN_POINT ( 'NONE',  ( -1.525408907393426716, 8.692885148323941991, 2.521481920632497431 ) ) ;
#45283 = CARTESIAN_POINT ( 'NONE',  ( -4.000724900121314320, 7.680942274213022003, 0.03569885272684778649 ) ) ;
#45284 = EDGE_CURVE ( 'NONE', #100589, #144319, #135687, .T. ) ;
#45285 = CARTESIAN_POINT ( 'NONE',  ( 6.666866396406604167, -1.974176978123330040, -0.8811043787171415342 ) ) ;
#45286 = CARTESIAN_POINT ( 'NONE',  ( 1.364683531249992088, 5.446875000341417916, 1.214306433183764966E-14 ) ) ;
#45287 = CARTESIAN_POINT ( 'NONE',  ( 4.053139552913617827, 1.658577106941661272, -1.047563642765911185 ) ) ;
#45288 = CARTESIAN_POINT ( 'NONE',  ( 0.8782795706883707032, -0.2985837142155840507, 1.993765709762222782 ) ) ;
#45289 = DIRECTION ( 'NONE',  ( 1.224646799147353454E-16, 0.000000000000000000, -1.000000000000000000 ) ) ;
#45291 = CARTESIAN_POINT ( 'NONE',  ( 4.161361007603033180, 7.399433999391101580, -0.7812420967184935394 ) ) ;
#45290 = CARTESIAN_POINT ( 'NONE',  ( 8.796542737168120851, 9.157054702984622097, -0.7998128361456211532 ) ) ;
#45292 = CARTESIAN_POINT ( 'NONE',  ( 0.6494046996203367561, 0.5928216254872006319, -1.774177939146783345 ) ) ;
#45293 = CARTESIAN_POINT ( 'NONE',  ( 0.6823417656249899377, 3.426041667008085323, -1.181850606188754593 ) ) ;
#45294 = CARTESIAN_POINT ( 'NONE',  ( 3.269792347016476697, 0.4849277011088357070, -1.953833955329455696 ) ) ;
#45296 = CARTESIAN_POINT ( 'NONE',  ( 2.425544100157220662, -1.571072031863307572, -1.419494070558358967 ) ) ;
#45295 = CARTESIAN_POINT ( 'NONE',  ( -5.748293942514180799, 7.729428904398431222, -1.443375672974052559 ) ) ;
#45298 = EDGE_CURVE ( 'NONE', #35846, #106915, #44204, .T. ) ;
#45297 = CARTESIAN_POINT ( 'NONE',  ( 7.320715180198387628, 14.46587040911547639, -9.511302536372342686 ) ) ;
#45299 = CARTESIAN_POINT ( 'NONE',  ( 3.437997351728830697, 1.311287738946330439, 1.602184970737066116 ) ) ;
#45300 = CARTESIAN_POINT ( 'NONE',  ( 5.657495238652423097, 9.822437888394988548, 0.000000000000000000 ) ) ;
#45302 = CARTESIAN_POINT ( 'NONE',  ( 2.758194185376297902, 5.305311418659259814, 1.199719254218452047 ) ) ;
#45301 = CARTESIAN_POINT ( 'NONE',  ( 6.474567623737461197, -0.1010770918629246007, -2.088323083193554641 ) ) ;
#45304 = ORIENTED_EDGE ( 'NONE', *, *, #116636, .T. ) ;
#45303 = CARTESIAN_POINT ( 'NONE',  ( 5.508770632382115728, 1.381118045931900573, -1.193960910464037850 ) ) ;
#45305 = CARTESIAN_POINT ( 'NONE',  ( 8.914649696185335870, 10.35917838609310593, -1.199719254218446718 ) ) ;
#45306 = DIRECTION ( 'NONE',  ( -0.6507913734559658270, 0.7592566023652989049, 0.000000000000000000 ) ) ;
#45307 = CARTESIAN_POINT ( 'NONE',  ( 11.10187507031741028, 9.547320325560693988, -4.066230808108215022 ) ) ;
#45308 =( GEOMETRIC_REPRESENTATION_CONTEXT ( 3 ) GLOBAL_UNCERTAINTY_ASSIGNED_CONTEXT ( ( #65671 ) ) GLOBAL_UNIT_ASSIGNED_CONTEXT ( ( #151307, #17002, #106874 ) ) REPRESENTATION_CONTEXT ( 'NONE', 'WORKASPACE' ) );
#45309 = CARTESIAN_POINT ( 'NONE',  ( 5.965903178300209220, 2.175115270774199416, -0.3715683035191637562 ) ) ;
#45310 = CARTESIAN_POINT ( 'NONE',  ( -8.012344526598182026E-15, 11.60937500034139980, -1.575800808251669460 ) ) ;
#45311 = CARTESIAN_POINT ( 'NONE',  ( 4.582611755193141789, -1.246403352314252810, 1.450376384258989182 ) ) ;
#45312 = CARTESIAN_POINT ( 'NONE',  ( -9.481229494658258261, 9.955855920056455588, -0.7998128361456291469 ) ) ;
#45313 = CARTESIAN_POINT ( 'NONE',  ( 7.630541526392844887, 7.796719957080126662, 0.7998128361456341429 ) ) ;
#45314 = CARTESIAN_POINT ( 'NONE',  ( 1.360316468749941832, 2.276041667008116942, 0.7853790794158921340 ) ) ;
#45315 = CARTESIAN_POINT ( 'NONE',  ( 4.487385655998885170, 5.298000022495898520, 1.082531754730560403 ) ) ;
#45316 = FACE_OUTER_BOUND ( 'NONE', #104982, .T. ) ;
#45317 = CARTESIAN_POINT ( 'NONE',  ( 3.472859903394816872, 7.203420320602605287, -0.7998128361456291469 ) ) ;
#45318 = VERTEX_POINT ( 'NONE', #182275 ) ;
#45319 = CIRCLE ( 'NONE', #152609, 0.08000000000000050127 ) ;
#45320 = CARTESIAN_POINT ( 'NONE',  ( -6.291865805193673111, 9.498204651771386509, -1.199719254218452047 ) ) ;
#45321 = CARTESIAN_POINT ( 'NONE',  ( 4.260029445439534435, 7.236136616047147641, 2.499999999999999556 ) ) ;
#45322 = CARTESIAN_POINT ( 'NONE',  ( 5.722423353419669567, 8.833855124701747386, 1.199719254218451159 ) ) ;
#45323 = DIRECTION ( 'NONE',  ( -0.8583236685137344280, -0.5131086435338277907, 3.252606517456507780E-15 ) ) ;
#45324 = CARTESIAN_POINT ( 'NONE',  ( -5.349061533644712263, 7.606979636585072591, 1.237473162191610188 ) ) ;
#45325 = EDGE_CURVE ( 'NONE', #17304, #154836, #143198, .T. ) ;
#45326 = CARTESIAN_POINT ( 'NONE',  ( -7.076992996653451939, 7.358839372291564374, 0.7216878364870317197 ) ) ;
#45327 = CARTESIAN_POINT ( 'NONE',  ( 3.846762897975340767, 5.510976019103107859, -1.599625672291256295 ) ) ;
#45328 = CARTESIAN_POINT ( 'NONE',  ( 2.483201282919132336, -0.004963586128624993335, 1.969629312250702036 ) ) ;
#45329 = CARTESIAN_POINT ( 'NONE',  ( 3.743767684670766371, 2.000855813463810140, -0.2496267151909299931 ) ) ;
#45330 = CARTESIAN_POINT ( 'NONE',  ( -8.044065211609668253, 8.279164256499745633, 0.7998128361456602331 ) ) ;
#45331 = CARTESIAN_POINT ( 'NONE',  ( 4.583538449871731757, 7.505156070562471804, 1.199719254218451159 ) ) ;
#45332 = CARTESIAN_POINT ( 'NONE',  ( 6.727182134110168299, 1.217656702865956397, 2.400974650093392171 ) ) ;
#45333 = CARTESIAN_POINT ( 'NONE',  ( 3.890727776643727598, 1.851661642969665067, -1.171806376371389957 ) ) ;
#45334 = CARTESIAN_POINT ( 'NONE',  ( -5.567429050782688904, 5.875295893689919779, -0.7230728617713001460 ) ) ;
#45335 = CARTESIAN_POINT ( 'NONE',  ( 2.168856224914788466, -1.760356022852540114, -0.7827933968581005653 ) ) ;
#45336 = CARTESIAN_POINT ( 'NONE',  ( -10.15913717534155047, 10.74674821418697057, 0.7998128361456462443 ) ) ;
#45337 = CARTESIAN_POINT ( 'NONE',  ( -0.1296875068448125057, 2.889142263448498227, -2.315371602238533555 ) ) ;
#45338 = CARTESIAN_POINT ( 'NONE',  ( 0.1333542156527295908, 5.722835866173135777, -2.639957043922738666 ) ) ;
#45339 = CARTESIAN_POINT ( 'NONE',  ( 3.092668437693027794, 6.622213920701574885, -0.7216878364870338292 ) ) ;
#45340 = CARTESIAN_POINT ( 'NONE',  ( 6.286176778230493589, 10.48562334124426698, 0.7998128361456462443 ) ) ;
#45341 = CARTESIAN_POINT ( 'NONE',  ( 4.611744806942754238, 8.532119374741881757, -0.7998128361456231517 ) ) ;
#45342 = CARTESIAN_POINT ( 'NONE',  ( -2.060660350336243063, 8.500464906087067618, -2.499999999999995559 ) ) ;
#45343 = CARTESIAN_POINT ( 'NONE',  ( 4.082413651490639062, 7.776916670132135501, 0.000000000000000000 ) ) ;
#45344 = VERTEX_POINT ( 'NONE', #20827 ) ;
#45346 = CARTESIAN_POINT ( 'NONE',  ( 1.945949197151348509, -1.316483196816301549, -1.523026451717986784 ) ) ;
#45345 = CARTESIAN_POINT ( 'NONE',  ( 4.757273854911123756, 1.820453720981948242, -0.2752165127944474210 ) ) ;
#45347 = CARTESIAN_POINT ( 'NONE',  ( 3.866856096493505923, -0.6709599815711597692, 2.198256080205548635 ) ) ;
#45349 = CARTESIAN_POINT ( 'NONE',  ( 2.395144146474707636, -1.664902989962243174, 0.8314883405181148213 ) ) ;
#45348 = CARTESIAN_POINT ( 'NONE',  ( -0.1291982275798261026, 4.084732128465967449, -2.628654587324832814 ) ) ;
#45350 = CARTESIAN_POINT ( 'NONE',  ( 1.642778471875000035, -1.976041666188709689, -2.845375778867859751 ) ) ;
#45351 = CARTESIAN_POINT ( 'NONE',  ( -2.820451594992841482, 6.512553637458760036, 0.000000000000000000 ) ) ;
#45352 = CARTESIAN_POINT ( 'NONE',  ( 5.291234991620994421, -0.05314252713351996088, -1.911838368980276925 ) ) ;
#45353 = CARTESIAN_POINT ( 'NONE',  ( -7.426115451983156923, 9.686887332112256388, -1.599625672291263179 ) ) ;
#45354 = CARTESIAN_POINT ( 'NONE',  ( -5.804299160426237059, 7.865044668620976509, -1.443375672974066548 ) ) ;
#45356 = CARTESIAN_POINT ( 'NONE',  ( 3.080767038946086611, -0.1360980058115155988, -1.865751385159146070 ) ) ;
#45355 = CARTESIAN_POINT ( 'NONE',  ( 4.441018442196864591, -1.617167385086373033, -1.325159661343593420 ) ) ;
#45357 = CARTESIAN_POINT ( 'NONE',  ( 6.073689629242148058, 8.109057205581079231, -1.443375672974057666 ) ) ;
#45358 = ORIENTED_EDGE ( 'NONE', *, *, #29782, .T. ) ;
#45359 = FACE_OUTER_BOUND ( 'NONE', #153428, .T. ) ;
#45360 = DIRECTION ( 'NONE',  ( -0.000000000000000000, 1.000000000000000000, 9.023263958591317418E-17 ) ) ;
#45361 = CARTESIAN_POINT ( 'NONE',  ( 4.986778444009251743, -0.2158907008250054438, -1.711239743519934242 ) ) ;
#45362 = CARTESIAN_POINT ( 'NONE',  ( -6.738566041191992539, 7.820414121934134322, 1.199719254218450271 ) ) ;
#45363 = CARTESIAN_POINT ( 'NONE',  ( 1.722904486866124962, 1.715286564835089456, 0.2538950934896730405 ) ) ;
#45364 = DIRECTION ( 'NONE',  ( -1.000000000000000000, 0.000000000000000000, 0.000000000000000000 ) ) ;
#45365 = CARTESIAN_POINT ( 'NONE',  ( 1.878188943807060696, 3.299815425349224451, 0.3999999999999645506 ) ) ;
#45366 = AXIS2_PLACEMENT_3D ( 'NONE', #63584, #9501, #47360 ) ;
#45367 = FACE_OUTER_BOUND ( 'NONE', #92904, .T. ) ;
#45368 = CARTESIAN_POINT ( 'NONE',  ( 5.840740439281987051, -2.116473627201011620, -0.4831736825232531007 ) ) ;
#45369 = CARTESIAN_POINT ( 'NONE',  ( 4.318856058802469811, 1.670182456744148336, 0.7377305746401884301 ) ) ;
#45370 = CARTESIAN_POINT ( 'NONE',  ( 1.744895479173363517, -0.2825750800353257208, -1.941159045430330465 ) ) ;
#45371 = CARTESIAN_POINT ( 'NONE',  ( 0.03496603831146075092, -1.697522432243668389, 1.265142316669096934 ) ) ;
#45372 = TOROIDAL_SURFACE ( 'NONE', #38395, 11.18000000000000149, 0.08000000000000000167 ) ;
#45373 = CARTESIAN_POINT ( 'NONE',  ( 10.62873463776380056, 13.79999999999999893, -3.200000000000001510 ) ) ;
#45374 = CARTESIAN_POINT ( 'NONE',  ( 2.456316247939566821, 8.205176026796580757, 2.499999999999998668 ) ) ;
#45375 = CARTESIAN_POINT ( 'NONE',  ( 7.426115451983150706, 9.686887332112256388, -1.599625672291262513 ) ) ;
#45376 = CARTESIAN_POINT ( 'NONE',  ( 2.350376503035214615, 0.9972050307137376723, -1.871358364749615033 ) ) ;
#45377 = CARTESIAN_POINT ( 'NONE',  ( -4.826339496784927796, 5.693446170079573321, 1.082531754730560403 ) ) ;
#45378 = CARTESIAN_POINT ( 'NONE',  ( 3.696970665278032975, 7.535159219458173574, -0.4808056554564468787 ) ) ;
#45379 = CARTESIAN_POINT ( 'NONE',  ( -4.957065645985164970, 6.648394846229956023, -1.245809975726259067 ) ) ;
#45380 =( BOUNDED_CURVE ( )  B_SPLINE_CURVE ( 2, ( #100799, #18475, #147442, #68280, #16333, #82415, #148504 ),
 .UNSPECIFIED., .F., .T. ) 
 B_SPLINE_CURVE_WITH_KNOTS ( ( 3, 2, 2, 3 ),
 ( 0.05357142857142838110, 0.05952380952380941642, 0.06547619047619046562, 0.07142857142857149400 ),
 .UNSPECIFIED. ) 
 CURVE ( )  GEOMETRIC_REPRESENTATION_ITEM ( )  RATIONAL_B_SPLINE_CURVE ( ( 1.000000000000004219, 0.8660254037844345998, 1.000000000000000000, 0.8660254037844387076, 1.000000000000000000, 0.8660254037844371533, 1.000000000000001554 ) ) 
 REPRESENTATION_ITEM ( '' )  );
#45381 = CARTESIAN_POINT ( 'NONE',  ( 1.217730340897508645, 0.4076058164220326407, -2.029561569317724690 ) ) ;
#45383 = CARTESIAN_POINT ( 'NONE',  ( -1.402160292154681736E-14, 13.34375000068279427, 1.732050807568881190 ) ) ;
#45382 = CARTESIAN_POINT ( 'NONE',  ( -10.89183506716020666, 4.909321371462001871, 5.036854565707462150 ) ) ;
#45385 = ORIENTED_EDGE ( 'NONE', *, *, #23022, .T. ) ;
#45384 = CARTESIAN_POINT ( 'NONE',  ( 3.457896741714714395, -1.683011943829109791, -1.449823692882054482 ) ) ;
#45386 = CARTESIAN_POINT ( 'NONE',  ( 0.7920821852162404086, 1.736045259359697335, -1.506783991232300446 ) ) ;
#45388 = CARTESIAN_POINT ( 'NONE',  ( 5.383662037909134668, -1.960299721042932930, 0.6417261926762083402 ) ) ;
#45387 = CARTESIAN_POINT ( 'NONE',  ( 10.56143847536557878, 11.42402576412244386, 0.000000000000000000 ) ) ;
#45390 = CARTESIAN_POINT ( 'NONE',  ( -1.737500000000000266, -1.108333333333332726, -3.009438278150923907 ) ) ;
#45389 = CARTESIAN_POINT ( 'NONE',  ( 4.044074958626150185, 7.940114228364351767, 0.7998128361456271485 ) ) ;
#45391 = CARTESIAN_POINT ( 'NONE',  ( 0.2331563151865730654, 0.7315591717663977311, -2.029986209603263259 ) ) ;
#45392 = CARTESIAN_POINT ( 'NONE',  ( 5.565905774130330386, -1.163279849954502287, 1.427249551226833502 ) ) ;
#45393 = CARTESIAN_POINT ( 'NONE',  ( 2.517010073631369860, 6.088262185878572375, -0.7998128361456281477 ) ) ;
#45394 = CARTESIAN_POINT ( 'NONE',  ( 2.924480221818404946, 1.623360404532696810, 0.5830473908832736196 ) ) ;
#45395 = CARTESIAN_POINT ( 'NONE',  ( 0.8136858238772455287, -1.282993010278702606, -1.555696519147983459 ) ) ;
#45396 = CARTESIAN_POINT ( 'NONE',  ( 2.620138118368781743, 0.2850873451692262361, 2.280912332010568644 ) ) ;
#45397 = CARTESIAN_POINT ( 'NONE',  ( 0.6823417656249899377, 3.488541667008085323, -1.181850606188754593 ) ) ;
#45398 =( BOUNDED_SURFACE ( )  B_SPLINE_SURFACE ( 1, 2, ( 
 ( #189606, #73725, #75858, #139822, #107362, #24966, #157129, #8718, #74802, #140903, #206915, #58545, #92142, #9786, #61745, #177642, #125763, #196019, #112695, #176566, #14031, #191725, #96405, #63873, #160312, #10838, #11916, #210105, #113766, #79051, #29250, #110564, #144111, #59607, #161392, #130028, #97461, #95342, #193865, #28175, #43381, #12976, #30320, #109502, #143038, #178705, #179769, #80117, #162455, #175509, #127912, #47655, #209033, #77989, #31386, #141967, #62798, #163517, #212240, #45514, #146222, #44447, #145168, #211173, #128960, #194939, #46576, #15104, #27099, #207979, #93207, #111629, #94271, #60668, #159237, #76912, #126832, #192789, #164574, #198124, #48704, #99575, #67038, #972, #135292, #119085, #69173, #50821, #166710, #181867, #18300, #98512, #81193, #149390, #165640, #82244, #33503, #201307, #148335, #132114, #16158, #84386, #185065, #35623, #51897, #115882, #133175, #199175, #36690, #214335, #17228, #19369, #197066, #65965, #114818, #116947, #49755, #101701, #182946, #85449, #167771, #213303, #118020, #102776, #147270, #52947, #180816, #150473, #83303, #68103, #168832, #151534, #184009, #34562, #64928, #134239, #100633, #3102, #2033, #131078, #32443, #200246, #138487, #23642, #123388, #104925, #204509, #155799, #56158, #188278, #39918, #54024, #4170, #21484, #156874, #86519, #140647, #120162, #122321, #169895, #170966, #203440, #74548, #73463, #107104, #106027, #5233, #7383, #124449, #89750, #87593, #139564, #20436, #186138, #37773, #24708, #103847, #70240, #206660, #153665, #205591, #136355, #57228, #189353, #40993, #58293, #42064, #173127, #71308, #152584, #137421, #121243, #90810, #172049, #8461, #190408, #108178, #202375, #55094, #187213, #22566, #38842, #88671, #154731, #6314, #72388, #208786, #59353, #177381, #28995, #192537, #44191, #110311, #61488, #30060, #210921, #95082, #77736, #47397, #75610, #176319, #209849, #174204, #25777, #161130, #27924, #94019, #111377, #109253, #91889, #160058, #127653, #157944, #13788, #144914, #60417, #46323, #9536, #128710, #96150, #11662, #43140, #143857, #193617, #145971, #12717, #45258, #142780, #78791, #141721, #62547, #162201, #129778, #194680, #112439, #126577, #207730, #178452, #79862, #125509, #175261, #211983, #63623, #195759, #191472, #26846, #92950, #158996, #10590, #76666, #35370, #113510, #34305, #2850, #183761, #115621, #1787, #15910, #198920, #132915, #182686, #116687, #66774, #84129, #14846, #50566, #166451, #83053, #81993, #114573, #148081, #213050, #201052, #68919, #196817, #147027, #150215, #18042, #214086, #179519, #31137, #100380, #51646, #167518, #48459, #180565, #65714, #197869, #199997, #67844, #19115, #97212, #135039, #131862, #101445, #85194, #32187, #133990, #16972, #117770, #163264, #49501, #151278, #80936, #64678, #130825, #98263, #164321, #181617, #33246, #99328, #165379, #149129, #710, #120989, #122057, #170712, #140387, #168577, #54838, #88410, #52694, #118825, #55900, #186956, #38588, #204248, #202111, #184811, #104665, #154478, #36440, #106840, #23380, #87336, #139303, #102515, #7124, #189101, #71052, #136095, #137168, #22297, #24442, #188021, #6056, #21232, #72127, #20178, #138234, #40734, #8207, #39649, #105758, #153403, #86265, #171784, #155545, #152336, #53771, #89490, #90554, #205332, #73197, #3913, #56970, #172871, #119904, #203192, #156617, #69983, #123143, #74292, #185878, #37514, #103590, #169647, #4974, #11399, #61234, #209588, #159796, #177120, #107926, #143596, #45007, #176065, #108986, #207475, #175005, #91632, #79612, #95897, #75354, #25524, #28737, #111117, #92692, #206406, #124195, #77477, #144659, #46070, #141467, #59094, #26591, #76407, #78542, #94822, #112191, #190158, #161950, #158738, #194429, #178196, #125254, #160873, #110052, #210674, #41813, #10333, #12467, #13542, #127389, #62302, #193362, #191215, #173950, #42878, #128461, #142516, #29812, #208525, #60161, #157684, #58031, #9282, #126316, #192276, #43937, #93757, #27662, #182428, #47141, #131617, #67591, #212797, #15660, #133736, #145731, #66522, #35111, #1527, #147829, #34055, #48211, #16720, #165129, #454, #148881, #99076 ),
 ( #198670, #31941, #211731, #63369, #82805, #83867, #199743, #14595, #80691, #114323, #81747, #17779, #50317, #51389, #129525, #101182, #98025, #117510, #183503, #146782, #116435, #49260, #149958, #195505, #180321, #100128, #167271, #132665, #18856, #166190, #130579, #113258, #196569, #179263, #64435, #30886, #164080, #213848, #96964, #163012, #65466, #197616, #115381, #181375, #32999, #155285, #121798, #154217, #202936, #172611, #200798, #87076, #120727, #84940, #151029, #88150, #153146, #4721, #22039, #19927, #2598, #70796, #186700, #68667, #139048, #55642, #119645, #171523, #134791, #39396, #6866, #103331, #168332, #169394, #136909, #56716, #5789, #38329, #53510, #54579, #52449, #104405, #72945, #40479, #170454, #71866, #185628, #118575, #137975, #187766, #184561, #86013, #105491, #122885, #23116, #89233, #152087, #205074, #188843, #106583, #36182, #102258, #203994, #3657, #69735, #20979, #135839, #201864, #37261, #110864, #143340, #190959, #93506, #157433, #142266, #76161, #59909, #126063, #208277, #109806, #74035, #192026, #43689, #92449, #9026, #41554, #75101, #206153, #94573, #176870, #189909, #57780, #175815, #27408, #141211, #24187, #156360, #159547, #209334, #193108, #107667, #173695, #207222, #125002, #77221, #11144, #44757, #7945, #28482, #58846, #127136, #90291, #91373, #60982, #140126, #123941, #42624, #25271, #108734, #174762, #26335, #158488, #10087, #202557, #53135, #54209, #89926, #86702, #123567, #170077, #71496, #102957, #6496, #72571, #21664, #87770, #153846, #105108, #73650, #40094, #138671, #121423, #90991, #119266, #5417, #39025, #3291, #69359, #204691, #137607, #203623, #154912, #152771, #135467, #55274, #171148, #201489, #57402, #188463, #37958, #155977, #185251, #172233, #139749, #187393, #4352, #22739, #88857, #189530, #56341, #122502, #186323, #106207, #36875, #23821, #205774, #173307, #7564, #41178, #104031, #169016, #107285, #24886, #20614, #70420, #120347, #136538, #101272, #168416, #53598, #33090, #183590, #82893, #83955, #116523, #201943, #200884, #20013, #51474, #132753, #134877, #37345, #151117, #148968, #2684, #147919, #99164, #165217, #152173, #16808, #197707, #119733, #181460, #118664, #131702, #68755, #52530, #86099, #185711, #169480, #184647, #541, #213935, #66607, #34144, #3742, #117598, #18944, #167357, #85029, #65556, #36267, #102345, #150045, #21064, #49349, #69817, #115468, #135924, #182514, #50405, #198756, #166282, #133820, #67676, #103419, #100214, #17871, #35198, #1616, #199833, #172698, #104497, #87161, #155367, #171613, #88238, #39480, #207316, #154308, #138064, #170540, #24276, #125095, #41646, #57867, #121884, #139131, #6952, #191053, #22125, #187854, #25361, #203022, #5880, #120812, #205159, #71954, #107760, #122970, #91461, #173786, #4803, #124030, #108826, #153232, #58938, #54664, #90382, #204077, #74126, #42718, #157523, #189996, #188930, #174851, #140221, #73033, #9118, #89320, #75193, #141305, #105579, #56801, #156451, #70883, #23206, #40568, #8035, #106675, #206241, #136995, #186789, #38416, #55729, #60004, #78386, #11243, #198246, #62149, #33628, #116009, #158580, #66095, #50952, #92540, #149519, #208372, #32566, #93601, #16287, #133300, #49885, #132238, #128308, #67166, #82373, #160711, #165772, #28581, #181996, #17355, #44851, #144506, #98642, #99701, #110957, #210513, #164700, #194270, #45916, #112035, #126157, #159646, #83437, #178037, #1105, #199306, #192120, #148463, #175910, #176964, #209430, #117076, #31, #26430, #10179, #77321, #76254, #142363, #43785, #27501, #109898, #143434, #61075, #127234, #193204, #94669, #12305, #22684, #2159, #153785, #166838, #103976, #186264, #203567, #154854, #204634, #87713, #68236, #34687, #134370, #69299, #187339, #86644, #54152, #202501, #120290, #100756, #37899, #5354, #185192, #56285, #18434, #71436, #84510, #137548, #3234, #85572, #150597, #201433, #168957, #102898, #88796, #6438, #171090, #152711, #170018, #135411, #21606, #200374, #183075, #36817, #53073, #184132, #119207, #72515, #35755, #19497, #52022, #55219, #138611, #121364, #38968, #20561, #4294, #70365, #118147, #101830, #105054, #167898 ) ),
 .UNSPECIFIED., .F., .F., .F. ) 
 B_SPLINE_SURFACE_WITH_KNOTS ( ( 2, 2 ),
 ( 3, 2, 2, 2, 2, 2, 2, 2, 2, 2, 2, 2, 2, 2, 2, 2, 2, 2, 2, 2, 2, 2, 2, 2, 2, 2, 2, 2, 2, 2, 2, 2, 2, 2, 2, 2, 2, 2, 2, 2, 2, 2, 2, 2, 2, 2, 2, 2, 2, 2, 2, 2, 2, 2, 2, 2, 2, 2, 2, 2, 2, 2, 2, 2, 2, 2, 2, 2, 2, 2, 2, 2, 2, 2, 2, 2, 2, 2, 2, 2, 2, 2, 2, 2, 2, 2, 2, 2, 2, 2, 2, 2, 2, 2, 2, 2, 2, 2, 2, 2, 2, 2, 2, 2, 2, 2, 2, 2, 2, 2, 2, 2, 2, 2, 2, 2, 2, 2, 2, 2, 2, 2, 2, 2, 2, 2, 2, 2, 2, 2, 2, 2, 2, 2, 2, 2, 2, 2, 2, 2, 2, 2, 2, 2, 2, 2, 2, 2, 2, 2, 2, 2, 2, 2, 2, 2, 2, 2, 2, 2, 2, 2, 2, 2, 2, 2, 2, 2, 2, 2, 2, 2, 2, 2, 2, 2, 2, 2, 2, 2, 2, 2, 2, 2, 2, 2, 2, 2, 2, 2, 2, 2, 2, 2, 2, 2, 2, 2, 2, 2, 2, 2, 2, 2, 2, 2, 2, 2, 2, 2, 2, 2, 2, 2, 2, 2, 2, 2, 2, 2, 2, 2, 2, 2, 2, 2, 2, 2, 2, 2, 2, 2, 2, 2, 2, 2, 2, 2, 2, 2, 3 ),
 ( 0.000000000000000000, 1.000000000000000000 ),
 ( 0.000000000000000000, 0.004166666666666666609, 0.008333333333333333218, 0.01250000000000000069, 0.01666666666666666644, 0.02083333333333333218, 0.02500000000000000139, 0.02916666666666666713, 0.03333333333333333287, 0.03749999999999999861, 0.04166666666666666435, 0.04583333333333333010, 0.05000000000000000278, 0.05416666666666666852, 0.05833333333333333426, 0.06250000000000000000, 0.06666666666666666574, 0.07083333333333333148, 0.07499999999999999722, 0.07916666666666666297, 0.08333333333333332871, 0.08749999999999999445, 0.09166666666666666019, 0.09583333333333333981, 0.1000000000000000056, 0.1041666666666666713, 0.1083333333333333370, 0.1125000000000000028, 0.1166666666666666685, 0.1208333333333333343, 0.1250000000000000000, 0.1291666666666666796, 0.1333333333333333315, 0.1375000000000000111, 0.1416666666666666630, 0.1458333333333333426, 0.1499999999999999944, 0.1541666666666666741, 0.1583333333333333259, 0.1625000000000000056, 0.1666666666666666574, 0.1708333333333333370, 0.1749999999999999889, 0.1791666666666666685, 0.1833333333333333204, 0.1875000000000000000, 0.1916666666666666796, 0.1958333333333333315, 0.2000000000000000111, 0.2041666666666666630, 0.2083333333333333426, 0.2124999999999999944, 0.2166666666666666741, 0.2208333333333333259, 0.2250000000000000056, 0.2291666666666666574, 0.2333333333333333370, 0.2374999999999999889, 0.2416666666666666685, 0.2458333333333333204, 0.2500000000000000000, 0.2541666666666666519, 0.2583333333333333592, 0.2625000000000000111, 0.2666666666666666630, 0.2708333333333333148, 0.2750000000000000222, 0.2791666666666666741, 0.2833333333333333259, 0.2874999999999999778, 0.2916666666666666852, 0.2958333333333333370, 0.2999999999999999889, 0.3041666666666666408, 0.3083333333333333481, 0.3125000000000000000, 0.3166666666666666519, 0.3208333333333333592, 0.3250000000000000111, 0.3291666666666666630, 0.3333333333333333148, 0.3375000000000000222, 0.3416666666666666741, 0.3458333333333333259, 0.3499999999999999778, 0.3541666666666666852, 0.3583333333333333370, 0.3624999999999999889, 0.3666666666666666408, 0.3708333333333333481, 0.3750000000000000000, 0.3791666666666666519, 0.3833333333333333592, 0.3875000000000000111, 0.3916666666666666630, 0.3958333333333333148, 0.4000000000000000222, 0.4041666666666666741, 0.4083333333333333259, 0.4124999999999999778, 0.4166666666666666852, 0.4208333333333333370, 0.4249999999999999889, 0.4291666666666666408, 0.4333333333333333481, 0.4375000000000000000, 0.4416666666666666519, 0.4458333333333333592, 0.4500000000000000111, 0.4541666666666666630, 0.4583333333333333148, 0.4625000000000000222, 0.4666666666666666741, 0.4708333333333333259, 0.4749999999999999778, 0.4791666666666666852, 0.4833333333333333370, 0.4874999999999999889, 0.4916666666666666408, 0.4958333333333333481, 0.5000000000000000000, 0.5041666666666666519, 0.5083333333333333037, 0.5124999999999999556, 0.5166666666666667185, 0.5208333333333333703, 0.5250000000000000222, 0.5291666666666666741, 0.5333333333333333259, 0.5374999999999999778, 0.5416666666666666297, 0.5458333333333332815, 0.5500000000000000444, 0.5541666666666666963, 0.5583333333333333481, 0.5625000000000000000, 0.5666666666666666519, 0.5708333333333333037, 0.5749999999999999556, 0.5791666666666667185, 0.5833333333333333703, 0.5875000000000000222, 0.5916666666666666741, 0.5958333333333333259, 0.5999999999999999778, 0.6041666666666666297, 0.6083333333333332815, 0.6125000000000000444, 0.6166666666666666963, 0.6208333333333333481, 0.6250000000000000000, 0.6291666666666666519, 0.6333333333333333037, 0.6374999999999999556, 0.6416666666666667185, 0.6458333333333333703, 0.6500000000000000222, 0.6541666666666666741, 0.6583333333333333259, 0.6624999999999999778, 0.6666666666666666297, 0.6708333333333332815, 0.6750000000000000444, 0.6791666666666666963, 0.6833333333333333481, 0.6875000000000000000, 0.6916666666666666519, 0.6958333333333333037, 0.6999999999999999556, 0.7041666666666667185, 0.7083333333333333703, 0.7125000000000000222, 0.7166666666666666741, 0.7208333333333333259, 0.7249999999999999778, 0.7291666666666666297, 0.7333333333333332815, 0.7375000000000000444, 0.7416666666666666963, 0.7458333333333333481, 0.7500000000000000000, 0.7541666666666666519, 0.7583333333333333037, 0.7624999999999999556, 0.7666666666666667185, 0.7708333333333333703, 0.7750000000000000222, 0.7791666666666666741, 0.7833333333333333259, 0.7874999999999999778, 0.7916666666666666297, 0.7958333333333332815, 0.8000000000000000444, 0.8041666666666666963, 0.8083333333333333481, 0.8125000000000000000, 0.8166666666666666519, 0.8208333333333333037, 0.8249999999999999556, 0.8291666666666667185, 0.8333333333333333703, 0.8375000000000000222, 0.8416666666666666741, 0.8458333333333333259, 0.8499999999999999778, 0.8541666666666666297, 0.8583333333333332815, 0.8625000000000000444, 0.8666666666666666963, 0.8708333333333333481, 0.8750000000000000000, 0.8791666666666666519, 0.8833333333333333037, 0.8874999999999999556, 0.8916666666666667185, 0.8958333333333333703, 0.9000000000000000222, 0.9041666666666666741, 0.9083333333333333259, 0.9124999999999999778, 0.9166666666666666297, 0.9208333333333332815, 0.9250000000000000444, 0.9291666666666666963, 0.9333333333333333481, 0.9375000000000000000, 0.9416666666666666519, 0.9458333333333333037, 0.9499999999999999556, 0.9541666666666667185, 0.9583333333333333703, 0.9625000000000000222, 0.9666666666666666741, 0.9708333333333333259, 0.9749999999999999778, 0.9791666666666666297, 0.9833333333333332815, 0.9875000000000000444, 0.9916666666666666963, 0.9958333333333333481, 1.000000000000000000 ),
 .UNSPECIFIED. ) 
 GEOMETRIC_REPRESENTATION_ITEM ( )  RATIONAL_B_SPLINE_SURFACE ( (
 ( 1.000000000000000000, 0.8660254037844387076, 1.000000000000000000, 0.8660254037844387076, 1.000000000000000000, 0.8660254037844387076, 1.000000000000000000, 0.8660254037844387076, 1.000000000000000000, 0.8660254037844387076, 1.000000000000000000, 0.8660254037844387076, 1.000000000000000000, 0.8660254037844387076, 1.000000000000000000, 0.8660254037844387076, 1.000000000000000000, 0.8660254037844387076, 1.000000000000000000, 0.8660254037844387076, 1.000000000000000000, 0.8660254037844387076, 1.000000000000000000, 0.8660254037844387076, 1.000000000000000000, 0.8660254037844387076, 1.000000000000000000, 0.8660254037844387076, 1.000000000000000000, 0.8660254037844387076, 1.000000000000000000, 0.8660254037844387076, 1.000000000000000000, 0.8660254037844387076, 1.000000000000000000, 0.8660254037844387076, 1.000000000000000000, 0.8660254037844387076, 1.000000000000000000, 0.8660254037844387076, 1.000000000000000000, 0.8660254037844387076, 1.000000000000000000, 0.8660254037844387076, 1.000000000000000000, 0.8660254037844387076, 1.000000000000000000, 0.8660254037844387076, 1.000000000000000000, 0.8660254037844387076, 1.000000000000000000, 0.8660254037844387076, 1.000000000000000000, 0.8660254037844387076, 1.000000000000000000, 0.8660254037844387076, 1.000000000000000000, 0.8660254037844387076, 1.000000000000000000, 0.8660254037844387076, 1.000000000000000000, 0.8660254037844387076, 1.000000000000000000, 0.8660254037844387076, 1.000000000000000000, 0.8660254037844387076, 1.000000000000000000, 0.8660254037844387076, 1.000000000000000000, 0.8660254037844387076, 1.000000000000000000, 0.8660254037844387076, 1.000000000000000000, 0.8660254037844387076, 1.000000000000000000, 0.8660254037844387076, 1.000000000000000000, 0.8660254037844387076, 1.000000000000000000, 0.8660254037844387076, 1.000000000000000000, 0.8660254037844387076, 1.000000000000000000, 0.8660254037844387076, 1.000000000000000000, 0.8660254037844387076, 1.000000000000000000, 0.8660254037844387076, 1.000000000000000000, 0.8660254037844387076, 1.000000000000000000, 0.8660254037844387076, 1.000000000000000000, 0.8660254037844387076, 1.000000000000000000, 0.8660254037844387076, 1.000000000000000000, 0.8660254037844387076, 1.000000000000000000, 0.8660254037844387076, 1.000000000000000000, 0.8660254037844387076, 1.000000000000000000, 0.8660254037844387076, 1.000000000000000000, 0.8660254037844387076, 1.000000000000000000, 0.8660254037844387076, 1.000000000000000000, 0.8660254037844387076, 1.000000000000000000, 0.8660254037844387076, 1.000000000000000000, 0.8660254037844387076, 1.000000000000000000, 0.8660254037844387076, 1.000000000000000000, 0.8660254037844387076, 1.000000000000000000, 0.8660254037844387076, 1.000000000000000000, 0.8660254037844387076, 1.000000000000000000, 0.8660254037844387076, 1.000000000000000000, 0.8660254037844387076, 1.000000000000000000, 0.8660254037844387076, 1.000000000000000000, 0.8660254037844387076, 1.000000000000000000, 0.8660254037844387076, 1.000000000000000000, 0.8660254037844387076, 1.000000000000000000, 0.8660254037844387076, 1.000000000000000000, 0.8660254037844387076, 1.000000000000000000, 0.8660254037844387076, 1.000000000000000000, 0.8660254037844387076, 1.000000000000000000, 0.8660254037844387076, 1.000000000000000000, 0.8660254037844387076, 1.000000000000000000, 0.8660254037844387076, 1.000000000000000000, 0.8660254037844387076, 1.000000000000000000, 0.8660254037844387076, 1.000000000000000000, 0.8660254037844387076, 1.000000000000000000, 0.8660254037844387076, 1.000000000000000000, 0.8660254037844387076, 1.000000000000000000, 0.8660254037844387076, 1.000000000000000000, 0.8660254037844387076, 1.000000000000000000, 0.8660254037844387076, 1.000000000000000000, 0.8660254037844387076, 1.000000000000000000, 0.8660254037844387076, 1.000000000000000000, 0.8660254037844387076, 1.000000000000000000, 0.8660254037844387076, 1.000000000000000000, 0.8660254037844387076, 1.000000000000000000, 0.8660254037844387076, 1.000000000000000000, 0.8660254037844387076, 1.000000000000000000, 0.8660254037844387076, 1.000000000000000000, 0.8660254037844387076, 1.000000000000000000, 0.8660254037844387076, 1.000000000000000000, 0.8660254037844387076, 1.000000000000000000, 0.8660254037844387076, 1.000000000000000000, 0.8660254037844387076, 1.000000000000000000, 0.8660254037844387076, 1.000000000000000000, 0.8660254037844387076, 1.000000000000000000, 0.8660254037844387076, 1.000000000000000000, 0.8660254037844387076, 1.000000000000000000, 0.8660254037844387076, 1.000000000000000000, 0.8660254037844387076, 1.000000000000000000, 0.8660254037844387076, 1.000000000000000000, 0.8660254037844387076, 1.000000000000000000, 0.8660254037844387076, 1.000000000000000000, 0.8660254037844387076, 1.000000000000000000, 0.8660254037844387076, 1.000000000000000000, 0.8660254037844387076, 1.000000000000000000, 0.8660254037844387076, 1.000000000000000000, 0.8660254037844387076, 1.000000000000000000, 0.8660254037844387076, 1.000000000000000000, 0.8660254037844387076, 1.000000000000000000, 0.8660254037844387076, 1.000000000000000000, 0.8660254037844387076, 1.000000000000000000, 0.8660254037844387076, 1.000000000000000000, 0.8660254037844387076, 1.000000000000000000, 0.8660254037844387076, 1.000000000000000000, 0.8660254037844387076, 1.000000000000000000, 0.8660254037844387076, 1.000000000000000000, 0.8660254037844387076, 1.000000000000000000, 0.8660254037844387076, 1.000000000000000000, 0.8660254037844387076, 1.000000000000000000, 0.8660254037844387076, 1.000000000000000000, 0.8660254037844387076, 1.000000000000000000, 0.8660254037844387076, 1.000000000000000000, 0.8660254037844387076, 1.000000000000000000, 0.8660254037844387076, 1.000000000000000000, 0.8660254037844387076, 1.000000000000000000, 0.8660254037844387076, 1.000000000000000000, 0.8660254037844387076, 1.000000000000000000, 0.8660254037844387076, 1.000000000000000000, 0.8660254037844387076, 1.000000000000000000, 0.8660254037844387076, 1.000000000000000000, 0.8660254037844387076, 1.000000000000000000, 0.8660254037844387076, 1.000000000000000000, 0.8660254037844387076, 1.000000000000000000, 0.8660254037844387076, 1.000000000000000000, 0.8660254037844387076, 1.000000000000000000, 0.8660254037844387076, 1.000000000000000000, 0.8660254037844387076, 1.000000000000000000, 0.8660254037844387076, 1.000000000000000000, 0.8660254037844387076, 1.000000000000000000, 0.8660254037844387076, 1.000000000000000000, 0.8660254037844387076, 1.000000000000000000, 0.8660254037844387076, 1.000000000000000000, 0.8660254037844387076, 1.000000000000000000, 0.8660254037844387076, 1.000000000000000000, 0.8660254037844387076, 1.000000000000000000, 0.8660254037844387076, 1.000000000000000000, 0.8660254037844387076, 1.000000000000000000, 0.8660254037844387076, 1.000000000000000000, 0.8660254037844387076, 1.000000000000000000, 0.8660254037844387076, 1.000000000000000000, 0.8660254037844387076, 1.000000000000000000, 0.8660254037844387076, 1.000000000000000000, 0.8660254037844387076, 1.000000000000000000, 0.8660254037844387076, 1.000000000000000000, 0.8660254037844387076, 1.000000000000000000, 0.8660254037844387076, 1.000000000000000000, 0.8660254037844387076, 1.000000000000000000, 0.8660254037844387076, 1.000000000000000000, 0.8660254037844387076, 1.000000000000000000, 0.8660254037844387076, 1.000000000000000000, 0.8660254037844387076, 1.000000000000000000, 0.8660254037844387076, 1.000000000000000000, 0.8660254037844387076, 1.000000000000000000, 0.8660254037844387076, 1.000000000000000000, 0.8660254037844387076, 1.000000000000000000, 0.8660254037844387076, 1.000000000000000000, 0.8660254037844387076, 1.000000000000000000, 0.8660254037844387076, 1.000000000000000000, 0.8660254037844387076, 1.000000000000000000, 0.8660254037844387076, 1.000000000000000000, 0.8660254037844387076, 1.000000000000000000, 0.8660254037844387076, 1.000000000000000000, 0.8660254037844387076, 1.000000000000000000, 0.8660254037844387076, 1.000000000000000000, 0.8660254037844387076, 1.000000000000000000, 0.8660254037844387076, 1.000000000000000000, 0.8660254037844387076, 1.000000000000000000, 0.8660254037844387076, 1.000000000000000000, 0.8660254037844387076, 1.000000000000000000, 0.8660254037844387076, 1.000000000000000000, 0.8660254037844387076, 1.000000000000000000, 0.8660254037844387076, 1.000000000000000000, 0.8660254037844387076, 1.000000000000000000, 0.8660254037844387076, 1.000000000000000000, 0.8660254037844387076, 1.000000000000000000, 0.8660254037844387076, 1.000000000000000000, 0.8660254037844387076, 1.000000000000000000, 0.8660254037844387076, 1.000000000000000000, 0.8660254037844387076, 1.000000000000000000, 0.8660254037844387076, 1.000000000000000000, 0.8660254037844387076, 1.000000000000000000, 0.8660254037844387076, 1.000000000000000000, 0.8660254037844387076, 1.000000000000000000, 0.8660254037844387076, 1.000000000000000000, 0.8660254037844387076, 1.000000000000000000, 0.8660254037844387076, 1.000000000000000000, 0.8660254037844387076, 1.000000000000000000, 0.8660254037844387076, 1.000000000000000000, 0.8660254037844387076, 1.000000000000000000, 0.8660254037844387076, 1.000000000000000000, 0.8660254037844387076, 1.000000000000000000, 0.8660254037844387076, 1.000000000000000000, 0.8660254037844387076, 1.000000000000000000, 0.8660254037844387076, 1.000000000000000000, 0.8660254037844387076, 1.000000000000000000, 0.8660254037844387076, 1.000000000000000000, 0.8660254037844387076, 1.000000000000000000, 0.8660254037844387076, 1.000000000000000000, 0.8660254037844387076, 1.000000000000000000, 0.8660254037844387076, 1.000000000000000000, 0.8660254037844387076, 1.000000000000000000, 0.8660254037844387076, 1.000000000000000000, 0.8660254037844387076, 1.000000000000000000, 0.8660254037844387076, 1.000000000000000000, 0.8660254037844387076, 1.000000000000000000, 0.8660254037844387076, 1.000000000000000000, 0.8660254037844387076, 1.000000000000000000, 0.8660254037844387076, 1.000000000000000000, 0.8660254037844387076, 1.000000000000000000, 0.8660254037844387076, 1.000000000000000000, 0.8660254037844387076, 1.000000000000000000, 0.8660254037844387076, 1.000000000000000000, 0.8660254037844387076, 1.000000000000000000, 0.8660254037844387076, 1.000000000000000000, 0.8660254037844387076, 1.000000000000000000, 0.8660254037844387076, 1.000000000000000000, 0.8660254037844387076, 1.000000000000000000, 0.8660254037844387076, 1.000000000000000000, 0.8660254037844387076, 1.000000000000000000, 0.8660254037844387076, 1.000000000000000000, 0.8660254037844387076, 1.000000000000000000, 0.8660254037844387076, 1.000000000000000000, 0.8660254037844387076, 1.000000000000000000, 0.8660254037844387076, 1.000000000000000000, 0.8660254037844387076, 1.000000000000000000, 0.8660254037844387076, 1.000000000000000000, 0.8660254037844387076, 1.000000000000000000, 0.8660254037844387076, 1.000000000000000000),
 ( 1.000000000000000000, 0.8660254037844387076, 1.000000000000000000, 0.8660254037844387076, 1.000000000000000000, 0.8660254037844387076, 1.000000000000000000, 0.8660254037844387076, 1.000000000000000000, 0.8660254037844387076, 1.000000000000000000, 0.8660254037844387076, 1.000000000000000000, 0.8660254037844387076, 1.000000000000000000, 0.8660254037844387076, 1.000000000000000000, 0.8660254037844387076, 1.000000000000000000, 0.8660254037844387076, 1.000000000000000000, 0.8660254037844387076, 1.000000000000000000, 0.8660254037844387076, 1.000000000000000000, 0.8660254037844387076, 1.000000000000000000, 0.8660254037844387076, 1.000000000000000000, 0.8660254037844387076, 1.000000000000000000, 0.8660254037844387076, 1.000000000000000000, 0.8660254037844387076, 1.000000000000000000, 0.8660254037844387076, 1.000000000000000000, 0.8660254037844387076, 1.000000000000000000, 0.8660254037844387076, 1.000000000000000000, 0.8660254037844387076, 1.000000000000000000, 0.8660254037844387076, 1.000000000000000000, 0.8660254037844387076, 1.000000000000000000, 0.8660254037844387076, 1.000000000000000000, 0.8660254037844387076, 1.000000000000000000, 0.8660254037844387076, 1.000000000000000000, 0.8660254037844387076, 1.000000000000000000, 0.8660254037844387076, 1.000000000000000000, 0.8660254037844387076, 1.000000000000000000, 0.8660254037844387076, 1.000000000000000000, 0.8660254037844387076, 1.000000000000000000, 0.8660254037844387076, 1.000000000000000000, 0.8660254037844387076, 1.000000000000000000, 0.8660254037844387076, 1.000000000000000000, 0.8660254037844387076, 1.000000000000000000, 0.8660254037844387076, 1.000000000000000000, 0.8660254037844387076, 1.000000000000000000, 0.8660254037844387076, 1.000000000000000000, 0.8660254037844387076, 1.000000000000000000, 0.8660254037844387076, 1.000000000000000000, 0.8660254037844387076, 1.000000000000000000, 0.8660254037844387076, 1.000000000000000000, 0.8660254037844387076, 1.000000000000000000, 0.8660254037844387076, 1.000000000000000000, 0.8660254037844387076, 1.000000000000000000, 0.8660254037844387076, 1.000000000000000000, 0.8660254037844387076, 1.000000000000000000, 0.8660254037844387076, 1.000000000000000000, 0.8660254037844387076, 1.000000000000000000, 0.8660254037844387076, 1.000000000000000000, 0.8660254037844387076, 1.000000000000000000, 0.8660254037844387076, 1.000000000000000000, 0.8660254037844387076, 1.000000000000000000, 0.8660254037844387076, 1.000000000000000000, 0.8660254037844387076, 1.000000000000000000, 0.8660254037844387076, 1.000000000000000000, 0.8660254037844387076, 1.000000000000000000, 0.8660254037844387076, 1.000000000000000000, 0.8660254037844387076, 1.000000000000000000, 0.8660254037844387076, 1.000000000000000000, 0.8660254037844387076, 1.000000000000000000, 0.8660254037844387076, 1.000000000000000000, 0.8660254037844387076, 1.000000000000000000, 0.8660254037844387076, 1.000000000000000000, 0.8660254037844387076, 1.000000000000000000, 0.8660254037844387076, 1.000000000000000000, 0.8660254037844387076, 1.000000000000000000, 0.8660254037844387076, 1.000000000000000000, 0.8660254037844387076, 1.000000000000000000, 0.8660254037844387076, 1.000000000000000000, 0.8660254037844387076, 1.000000000000000000, 0.8660254037844387076, 1.000000000000000000, 0.8660254037844387076, 1.000000000000000000, 0.8660254037844387076, 1.000000000000000000, 0.8660254037844387076, 1.000000000000000000, 0.8660254037844387076, 1.000000000000000000, 0.8660254037844387076, 1.000000000000000000, 0.8660254037844387076, 1.000000000000000000, 0.8660254037844387076, 1.000000000000000000, 0.8660254037844387076, 1.000000000000000000, 0.8660254037844387076, 1.000000000000000000, 0.8660254037844387076, 1.000000000000000000, 0.8660254037844387076, 1.000000000000000000, 0.8660254037844387076, 1.000000000000000000, 0.8660254037844387076, 1.000000000000000000, 0.8660254037844387076, 1.000000000000000000, 0.8660254037844387076, 1.000000000000000000, 0.8660254037844387076, 1.000000000000000000, 0.8660254037844387076, 1.000000000000000000, 0.8660254037844387076, 1.000000000000000000, 0.8660254037844387076, 1.000000000000000000, 0.8660254037844387076, 1.000000000000000000, 0.8660254037844387076, 1.000000000000000000, 0.8660254037844387076, 1.000000000000000000, 0.8660254037844387076, 1.000000000000000000, 0.8660254037844387076, 1.000000000000000000, 0.8660254037844387076, 1.000000000000000000, 0.8660254037844387076, 1.000000000000000000, 0.8660254037844387076, 1.000000000000000000, 0.8660254037844387076, 1.000000000000000000, 0.8660254037844387076, 1.000000000000000000, 0.8660254037844387076, 1.000000000000000000, 0.8660254037844387076, 1.000000000000000000, 0.8660254037844387076, 1.000000000000000000, 0.8660254037844387076, 1.000000000000000000, 0.8660254037844387076, 1.000000000000000000, 0.8660254037844387076, 1.000000000000000000, 0.8660254037844387076, 1.000000000000000000, 0.8660254037844387076, 1.000000000000000000, 0.8660254037844387076, 1.000000000000000000, 0.8660254037844387076, 1.000000000000000000, 0.8660254037844387076, 1.000000000000000000, 0.8660254037844387076, 1.000000000000000000, 0.8660254037844387076, 1.000000000000000000, 0.8660254037844387076, 1.000000000000000000, 0.8660254037844387076, 1.000000000000000000, 0.8660254037844387076, 1.000000000000000000, 0.8660254037844387076, 1.000000000000000000, 0.8660254037844387076, 1.000000000000000000, 0.8660254037844387076, 1.000000000000000000, 0.8660254037844387076, 1.000000000000000000, 0.8660254037844387076, 1.000000000000000000, 0.8660254037844387076, 1.000000000000000000, 0.8660254037844387076, 1.000000000000000000, 0.8660254037844387076, 1.000000000000000000, 0.8660254037844387076, 1.000000000000000000, 0.8660254037844387076, 1.000000000000000000, 0.8660254037844387076, 1.000000000000000000, 0.8660254037844387076, 1.000000000000000000, 0.8660254037844387076, 1.000000000000000000, 0.8660254037844387076, 1.000000000000000000, 0.8660254037844387076, 1.000000000000000000, 0.8660254037844387076, 1.000000000000000000, 0.8660254037844387076, 1.000000000000000000, 0.8660254037844387076, 1.000000000000000000, 0.8660254037844387076, 1.000000000000000000, 0.8660254037844387076, 1.000000000000000000, 0.8660254037844387076, 1.000000000000000000, 0.8660254037844387076, 1.000000000000000000, 0.8660254037844387076, 1.000000000000000000, 0.8660254037844387076, 1.000000000000000000, 0.8660254037844387076, 1.000000000000000000, 0.8660254037844387076, 1.000000000000000000, 0.8660254037844387076, 1.000000000000000000, 0.8660254037844387076, 1.000000000000000000, 0.8660254037844387076, 1.000000000000000000, 0.8660254037844387076, 1.000000000000000000, 0.8660254037844387076, 1.000000000000000000, 0.8660254037844387076, 1.000000000000000000, 0.8660254037844387076, 1.000000000000000000, 0.8660254037844387076, 1.000000000000000000, 0.8660254037844387076, 1.000000000000000000, 0.8660254037844387076, 1.000000000000000000, 0.8660254037844387076, 1.000000000000000000, 0.8660254037844387076, 1.000000000000000000, 0.8660254037844387076, 1.000000000000000000, 0.8660254037844387076, 1.000000000000000000, 0.8660254037844387076, 1.000000000000000000, 0.8660254037844387076, 1.000000000000000000, 0.8660254037844387076, 1.000000000000000000, 0.8660254037844387076, 1.000000000000000000, 0.8660254037844387076, 1.000000000000000000, 0.8660254037844387076, 1.000000000000000000, 0.8660254037844387076, 1.000000000000000000, 0.8660254037844387076, 1.000000000000000000, 0.8660254037844387076, 1.000000000000000000, 0.8660254037844387076, 1.000000000000000000, 0.8660254037844387076, 1.000000000000000000, 0.8660254037844387076, 1.000000000000000000, 0.8660254037844387076, 1.000000000000000000, 0.8660254037844387076, 1.000000000000000000, 0.8660254037844387076, 1.000000000000000000, 0.8660254037844387076, 1.000000000000000000, 0.8660254037844387076, 1.000000000000000000, 0.8660254037844387076, 1.000000000000000000, 0.8660254037844387076, 1.000000000000000000, 0.8660254037844387076, 1.000000000000000000, 0.8660254037844387076, 1.000000000000000000, 0.8660254037844387076, 1.000000000000000000, 0.8660254037844387076, 1.000000000000000000, 0.8660254037844387076, 1.000000000000000000, 0.8660254037844387076, 1.000000000000000000, 0.8660254037844387076, 1.000000000000000000, 0.8660254037844387076, 1.000000000000000000, 0.8660254037844387076, 1.000000000000000000, 0.8660254037844387076, 1.000000000000000000, 0.8660254037844387076, 1.000000000000000000, 0.8660254037844387076, 1.000000000000000000, 0.8660254037844387076, 1.000000000000000000, 0.8660254037844387076, 1.000000000000000000, 0.8660254037844387076, 1.000000000000000000, 0.8660254037844387076, 1.000000000000000000, 0.8660254037844387076, 1.000000000000000000, 0.8660254037844387076, 1.000000000000000000, 0.8660254037844387076, 1.000000000000000000, 0.8660254037844387076, 1.000000000000000000, 0.8660254037844387076, 1.000000000000000000, 0.8660254037844387076, 1.000000000000000000, 0.8660254037844387076, 1.000000000000000000, 0.8660254037844387076, 1.000000000000000000, 0.8660254037844387076, 1.000000000000000000, 0.8660254037844387076, 1.000000000000000000, 0.8660254037844387076, 1.000000000000000000, 0.8660254037844387076, 1.000000000000000000, 0.8660254037844387076, 1.000000000000000000, 0.8660254037844387076, 1.000000000000000000, 0.8660254037844387076, 1.000000000000000000, 0.8660254037844387076, 1.000000000000000000, 0.8660254037844387076, 1.000000000000000000, 0.8660254037844387076, 1.000000000000000000, 0.8660254037844387076, 1.000000000000000000, 0.8660254037844387076, 1.000000000000000000, 0.8660254037844387076, 1.000000000000000000, 0.8660254037844387076, 1.000000000000000000, 0.8660254037844387076, 1.000000000000000000, 0.8660254037844387076, 1.000000000000000000, 0.8660254037844387076, 1.000000000000000000, 0.8660254037844387076, 1.000000000000000000, 0.8660254037844387076, 1.000000000000000000, 0.8660254037844387076, 1.000000000000000000, 0.8660254037844387076, 1.000000000000000000, 0.8660254037844387076, 1.000000000000000000, 0.8660254037844387076, 1.000000000000000000, 0.8660254037844387076, 1.000000000000000000, 0.8660254037844387076, 1.000000000000000000, 0.8660254037844387076, 1.000000000000000000, 0.8660254037844387076, 1.000000000000000000, 0.8660254037844387076, 1.000000000000000000, 0.8660254037844387076, 1.000000000000000000, 0.8660254037844387076, 1.000000000000000000, 0.8660254037844387076, 1.000000000000000000, 0.8660254037844387076, 1.000000000000000000, 0.8660254037844387076, 1.000000000000000000, 0.8660254037844387076, 1.000000000000000000, 0.8660254037844387076, 1.000000000000000000, 0.8660254037844387076, 1.000000000000000000, 0.8660254037844387076, 1.000000000000000000, 0.8660254037844387076, 1.000000000000000000, 0.8660254037844387076, 1.000000000000000000, 0.8660254037844387076, 1.000000000000000000) ) ) 
 REPRESENTATION_ITEM ( '' )  SURFACE ( )  );
#45399 = CARTESIAN_POINT ( 'NONE',  ( 2.741812758617673040, -1.674694146245614412, -1.521292302590461665 ) ) ;
#45400 = CARTESIAN_POINT ( 'NONE',  ( 5.690091061058023314, -0.9480630415420692181, 1.880679904143019776 ) ) ;
#45401 = CARTESIAN_POINT ( 'NONE',  ( -7.932929277771797238, 8.427708043588125975, 0.000000000000000000 ) ) ;
#45402 = CARTESIAN_POINT ( 'NONE',  ( 3.110363945789674123, 1.284354398739546266, -1.217803596734900573 ) ) ;
#45403 = CARTESIAN_POINT ( 'NONE',  ( 5.015626762051672571, 7.938982758113895422, 1.199719254218462483 ) ) ;
#45405 = CARTESIAN_POINT ( 'NONE',  ( 0.1820931442207155415, -1.074843934555272273, 2.024655709774853207 ) ) ;
#45404 = CARTESIAN_POINT ( 'NONE',  ( 3.838366886000300404, 6.531826229425389485, -1.082531754730548412 ) ) ;
#45406 = CARTESIAN_POINT ( 'NONE',  ( 4.365079047384805122, 1.785254547683400306, -0.4496667978745386152 ) ) ;
#45407 = CARTESIAN_POINT ( 'NONE',  ( -3.601662362724658895, 7.353689856487406473, -0.7998128361456281477 ) ) ;
#45408 = CARTESIAN_POINT ( 'NONE',  ( 5.463572716182829581, 6.436884926043849653, 1.082531754730560403 ) ) ;
#45409 = CARTESIAN_POINT ( 'NONE',  ( 1.499999999999989120, 3.004166666666689522, 0.8660254037844524744 ) ) ;
#45410 = CARTESIAN_POINT ( 'NONE',  ( 5.138714532536901913, -1.880766731008373993, 1.124575086929799239 ) ) ;
#45411 = CARTESIAN_POINT ( 'NONE',  ( -2.937312835655025101, 6.578615408239493867, 1.040834085586084257E-14 ) ) ;
#45412 = CARTESIAN_POINT ( 'NONE',  ( 0.006800380015300722461, 7.009756401597622144, -1.999988438675401881 ) ) ;
#45413 =( BOUNDED_CURVE ( )  B_SPLINE_CURVE ( 2, ( #30040, #13768, #96126, #127632, #160038, #61466, #128690 ),
 .UNSPECIFIED., .F., .T. ) 
 B_SPLINE_CURVE_WITH_KNOTS ( ( 3, 2, 2, 3 ),
 ( 0.2125000000000001055, 0.2166666666666668128, 0.2208333333333334925, 0.2250000000000001998 ),
 .UNSPECIFIED. ) 
 CURVE ( )  GEOMETRIC_REPRESENTATION_ITEM ( )  RATIONAL_B_SPLINE_CURVE ( ( 0.9999999999999964473, 0.8660254037844422603, 1.000000000000000000, 0.8660254037844387076, 1.000000000000000000, 0.8660254037844324904, 1.000000000000006217 ) ) 
 REPRESENTATION_ITEM ( '' )  );
#45414 = CARTESIAN_POINT ( 'NONE',  ( -3.420250508247430155, -0.02876672507465954931, -0.2938434605158617985 ) ) ;
#45415 = CARTESIAN_POINT ( 'NONE',  ( 0.6823417656249917140, 4.342708333674755394, 1.181850606188765695 ) ) ;
#45416 = CARTESIAN_POINT ( 'NONE',  ( 3.369672229528171581, 1.879407295867494554, -0.4226879870903621494 ) ) ;
#45417 = CARTESIAN_POINT ( 'NONE',  ( -0.6823417656250039265, 9.317708333674733723, -1.181850606188755259 ) ) ;
#45418 = CARTESIAN_POINT ( 'NONE',  ( -4.284013352238265959, 5.060732334775157604, -1.082531754730544860 ) ) ;
#45419 = CARTESIAN_POINT ( 'NONE',  ( 0.4928134435002875513, -1.227493105415909946, 1.851297100075269153 ) ) ;
#45420 = VERTEX_POINT ( 'NONE', #118422 ) ;
#45422 = CARTESIAN_POINT ( 'NONE',  ( 5.558836782162523527, 7.518240855878357110, -1.384758111419038817 ) ) ;
#45421 = CARTESIAN_POINT ( 'NONE',  ( -4.421367491832313590, 6.251624388594711590, 1.443375672974065660 ) ) ;
#45423 = CARTESIAN_POINT ( 'NONE',  ( 5.515469562660962666, 5.329135999392899947, 0.7998128361456341429 ) ) ;
#45424 = CARTESIAN_POINT ( 'NONE',  ( 7.765925996254661179, -5.615420858948578342, -7.710915694720370084 ) ) ;
#45425 = CARTESIAN_POINT ( 'NONE',  ( -2.540684401258873848, 0.3622604021566178667, -0.2586409171621191216 ) ) ;
#45426 = CARTESIAN_POINT ( 'NONE',  ( 11.41381675112453387, 13.39999999999998259, 3.704697986577180746 ) ) ;
#45427 = CARTESIAN_POINT ( 'NONE',  ( 2.647703282711162398, 0.5884205719196273776, 1.638072370343154116 ) ) ;
#45428 = CARTESIAN_POINT ( 'NONE',  ( -4.824649217201493201, 7.689440087634505261, -1.092232977752989331 ) ) ;
#45429 = CARTESIAN_POINT ( 'NONE',  ( 0.7132427667453158371, -1.655377960257615966, -1.052639099659122390 ) ) ;
#45430 = CARTESIAN_POINT ( 'NONE',  ( -1.364683531250014514, 1.051041667008090208, -0.7879004041258289570 ) ) ;
#45431 = EDGE_CURVE ( 'NONE', #43808, #127442, #37262, .T. ) ;
#45432 = CARTESIAN_POINT ( 'NONE',  ( 5.998930166150279852, 1.769978137569449883, -1.240765152474863520 ) ) ;
#45433 = CARTESIAN_POINT ( 'NONE',  ( -9.215791728987058562, 11.77484298861683598, -1.599625672291263179 ) ) ;
#45434 = AXIS2_PLACEMENT_3D ( 'NONE', #43378, #72648, #8714 ) ;
#45435 = CARTESIAN_POINT ( 'NONE',  ( -6.222829318548141586, 6.362315081168691044, 0.7216878364870317197 ) ) ;
#45436 = CARTESIAN_POINT ( 'NONE',  ( 5.243122039519461097, -1.856066598825537373, 1.107904190987746063 ) ) ;
#45438 = ORIENTED_EDGE ( 'NONE', *, *, #163321, .T. ) ;
#45437 = CARTESIAN_POINT ( 'NONE',  ( -0.2104748580754201015, 7.629137130509078268, -2.703678718140526627 ) ) ;
#45439 = CARTESIAN_POINT ( 'NONE',  ( 1.364683531249990311, 4.634375000341417916, 1.214306433183764966E-14 ) ) ;
#45440 = CARTESIAN_POINT ( 'NONE',  ( 6.907508285686359883, -0.4377196890756588910, 1.929438547640258017 ) ) ;
#45441 = CARTESIAN_POINT ( 'NONE',  ( 5.764916378462246804, -1.734034293797588999, 0.002837784182162239165 ) ) ;
#45443 = CARTESIAN_POINT ( 'NONE',  ( 3.070069520051089906, -1.303570237086741024, 1.761582097007891923 ) ) ;
#45442 = CARTESIAN_POINT ( 'NONE',  ( -0.6801582343750125492, 1.098958333674737720, -1.178068619123855409 ) ) ;
#45444 = CARTESIAN_POINT ( 'NONE',  ( 3.013035845080668906, 1.672340031372629321, -1.590277441748239040 ) ) ;
#45445 = CARTESIAN_POINT ( 'NONE',  ( 6.274695623702050362, -1.955332461540583600, -0.6509123137334557052 ) ) ;
#45446 = CARTESIAN_POINT ( 'NONE',  ( 0.8142755762143333298, 1.794035260217427874, 0.7438321904150380082 ) ) ;
#45447 = CARTESIAN_POINT ( 'NONE',  ( -6.738039155867462604, 7.923762439009225389, 1.082531754730549967 ) ) ;
#45448 = DIRECTION ( 'NONE',  ( -1.000000000000000000, 7.771561172376096769E-16, 4.440892098500627148E-16 ) ) ;
#45449 = CARTESIAN_POINT ( 'NONE',  ( 4.236665939827915395, 1.302216991916404387, -1.673619383358643908 ) ) ;
#45450 = CARTESIAN_POINT ( 'NONE',  ( -1.409462824231155764E-15, 1.016282880930355459, 12.28865868783309701 ) ) ;
#45451 = CARTESIAN_POINT ( 'NONE',  ( 2.338517726396415863, 0.5350873343827439177, -1.944071628254496087 ) ) ;
#45452 = CARTESIAN_POINT ( 'NONE',  ( -5.382223794500843539, 7.302347065049529462, -1.443375672974051449 ) ) ;
#45453 = CARTESIAN_POINT ( 'NONE',  ( 5.526482418920476647, 1.318621124876094397, -1.769340128416618363 ) ) ;
#45454 = CARTESIAN_POINT ( 'NONE',  ( -3.285556943750000514, -0.9260416661887070910, -1.896917185911906500 ) ) ;
#45455 = CARTESIAN_POINT ( 'NONE',  ( -3.159337285218927427, -3.068491660968841295, 1.397772451703464425 ) ) ;
#45456 = DIRECTION ( 'NONE',  ( 1.224646799147353454E-16, 0.000000000000000000, -1.000000000000000000 ) ) ;
#45457 = CARTESIAN_POINT ( 'NONE',  ( -5.752402313948099533, 9.933162809573264695, -0.7998128361456362523 ) ) ;
#45459 = CARTESIAN_POINT ( 'NONE',  ( 6.825078400183572036, 7.051914997414900022, 2.742498282622223726 ) ) ;
#45458 = CARTESIAN_POINT ( 'NONE',  ( -5.227029541856937023, 7.814379162078399332, 1.287352361829100733 ) ) ;
#45460 = ORIENTED_EDGE ( 'NONE', *, *, #54713, .T. ) ;
#45461 = CARTESIAN_POINT ( 'NONE',  ( 4.979397702276197712, 1.923710689106904015, -0.7398180773239333430 ) ) ;
#45462 = CARTESIAN_POINT ( 'NONE',  ( -6.075462232255183892, 10.10214001435745246, 0.000000000000000000 ) ) ;
#45463 = CARTESIAN_POINT ( 'NONE',  ( 6.983263157960366563, -0.003091553303710344557, 1.945923119799706669 ) ) ;
#45464 = CARTESIAN_POINT ( 'NONE',  ( -5.066996723205291708, 6.934582148538044777, 1.599625672291267398 ) ) ;
#45465 = CARTESIAN_POINT ( 'NONE',  ( -2.830620210203090181, 6.524417021870718258, 0.000000000000000000 ) ) ;
#45466 = CARTESIAN_POINT ( 'NONE',  ( 4.143226661672769318, 0.1011831993794048007, 2.017277399227022094 ) ) ;
#45467 = CARTESIAN_POINT ( 'NONE',  ( -1.500000000000013101, 1.420833333333354043, 0.8660254037844403729 ) ) ;
#45469 = CARTESIAN_POINT ( 'NONE',  ( 9.924205255523292024, 10.68058700763975466, -0.7216878364870257245 ) ) ;
#45468 = CARTESIAN_POINT ( 'NONE',  ( -3.657667580636712934, 7.489305620709952649, -0.7998128361456481317 ) ) ;
#45470 = CARTESIAN_POINT ( 'NONE',  ( 6.551614543901692400, 8.666636272683888365, 1.599625672291281386 ) ) ;
#45471 = AXIS2_PLACEMENT_3D ( 'NONE', #110262, #45214, #145927 ) ;
#45472 = CARTESIAN_POINT ( 'NONE',  ( 2.729428266803469061, -1.923432490405907247, 0.7405405203823824944 ) ) ;
#45473 = CARTESIAN_POINT ( 'NONE',  ( 2.654922836763852878, 1.081066371885472277, 1.701947380796410059 ) ) ;
#45474 = VERTEX_POINT ( 'NONE', #150875 ) ;
#45475 = DIRECTION ( 'NONE',  ( 1.276756478318932585E-15, -1.000000000000000000, 1.665334536937738262E-16 ) ) ;
#45476 = CARTESIAN_POINT ( 'NONE',  ( 3.493197133815315603, 7.227147089426516402, -0.7998128361456291469 ) ) ;
#45477 =( BOUNDED_CURVE ( )  B_SPLINE_CURVE ( 2, ( #21648, #153831, #5401, #58190, #80846, #181523, #145880 ),
 .UNSPECIFIED., .F., .T. ) 
 B_SPLINE_CURVE_WITH_KNOTS ( ( 3, 2, 2, 3 ),
 ( 0.1500000000000002165, 0.1541666666666669516, 0.1583333333333336590, 0.1625000000000003941 ),
 .UNSPECIFIED. ) 
 CURVE ( )  GEOMETRIC_REPRESENTATION_ITEM ( )  RATIONAL_B_SPLINE_CURVE ( ( 0.9999999999999928946, 0.8660254037844458130, 1.000000000000000000, 0.8660254037844387076, 1.000000000000000000, 0.8660254037844261621, 1.000000000000012434 ) ) 
 REPRESENTATION_ITEM ( '' )  );
#45479 = EDGE_LOOP ( 'NONE', ( #135503, #8590, #20684, #186234, #52814, #79126, #97021, #55974 ) ) ;
#45478 = CARTESIAN_POINT ( 'NONE',  ( -0.006768871532359400575, 8.210909518262125673, -2.038649385027044403 ) ) ;
#45480 = CARTESIAN_POINT ( 'NONE',  ( 2.618517346670693247, 0.5404096030681636575, -1.942243668081746311 ) ) ;
#45481 = CARTESIAN_POINT ( 'NONE',  ( 1.886409237429786279, 1.602333580200336671, -0.9066872629178088783 ) ) ;
#45482 = EDGE_CURVE ( 'NONE', #69052, #207943, #201712, .T. ) ;
#45483 = CARTESIAN_POINT ( 'NONE',  ( 0.4347317753056179623, 1.181035649988096958, -1.982462206444644437 ) ) ;
#45484 = CARTESIAN_POINT ( 'NONE',  ( 4.050854035433010480, 7.948023151305657841, 0.000000000000000000 ) ) ;
#45485 = CARTESIAN_POINT ( 'NONE',  ( 2.425270691926324051, -0.002641788883844811090, 2.161773191836775521 ) ) ;
#45486 = CARTESIAN_POINT ( 'NONE',  ( -5.280010757518168063, 8.247430752824802980, -1.199719254218446718 ) ) ;
#45487 = VECTOR ( 'NONE', #117022, 1000.000000000000000 ) ;
#45488 = ORIENTED_EDGE ( 'NONE', *, *, #30522, .F. ) ;
#45489 = CARTESIAN_POINT ( 'NONE',  ( -11.86145016429273014, 10.90000000000000036, -1.100000000000002087 ) ) ;
#45490 = CARTESIAN_POINT ( 'NONE',  ( 0.9185735243398345240, 1.726912363944958617, 0.7195956246372691156 ) ) ;
#45491 = CARTESIAN_POINT ( 'NONE',  ( 5.190288350601474754, -1.956472792631309909, -0.2422539641438857527 ) ) ;
#45494 = EDGE_CURVE ( 'NONE', #134733, #81519, #33406, .T. ) ;
#45493 = CARTESIAN_POINT ( 'NONE',  ( 8.609064354553323639, 10.10662517080946543, -1.082531754730543083 ) ) ;
#45492 = CARTESIAN_POINT ( 'NONE',  ( -1.364683531250012516, 3.030208333674755394, 0.7879004041258379498 ) ) ;
#45496 = CARTESIAN_POINT ( 'NONE',  ( 0.6806489137391663613, -1.222764829241920648, 1.836970590647703627 ) ) ;
#45495 = CARTESIAN_POINT ( 'NONE',  ( -6.632963465583701534, 8.761543347979550589, -1.599625672291263179 ) ) ;
#45497 = CARTESIAN_POINT ( 'NONE',  ( 6.127406499145813257, 0.1562011534181114436, -2.064545280851529885 ) ) ;
#45498 = CARTESIAN_POINT ( 'NONE',  ( 5.982172092127724383, 8.002286745614243912, -1.599625672291262513 ) ) ;
#45499 = CARTESIAN_POINT ( 'NONE',  ( -7.061099074618889304, 7.132370430010492868, -0.7998128361456291469 ) ) ;
#45500 = CARTESIAN_POINT ( 'NONE',  ( 6.539320575229294441, -0.001643797937642132567, 2.203502507913539521 ) ) ;
#45501 = CARTESIAN_POINT ( 'NONE',  ( 4.469576204829595945, 1.912561584401346604, -0.4778803491252373026 ) ) ;
#45502 = CARTESIAN_POINT ( 'NONE',  ( 6.521752737896459706, -0.4354215942184087584, 1.979412122172687694 ) ) ;
#45503 = CARTESIAN_POINT ( 'NONE',  ( -1.201851678989727383E-14, 0.9937500006828198229, 1.732050807568877637 ) ) ;
#45504 = CARTESIAN_POINT ( 'NONE',  ( 4.864078691051298975, 2.283152030527708209, -0.3349727840419229330 ) ) ;
#45505 = CARTESIAN_POINT ( 'NONE',  ( 1.446217529737943153, -0.9311174319141333200, 1.840543939966767351 ) ) ;
#45506 = CARTESIAN_POINT ( 'NONE',  ( 8.107412671292042461, 9.521364873671299023, 1.082531754730558626 ) ) ;
#45507 = CARTESIAN_POINT ( 'NONE',  ( 4.583538449871731757, 7.505156070562471804, 1.199719254218451159 ) ) ;
#45508 = CARTESIAN_POINT ( 'NONE',  ( 3.074666975249065626, 6.809138247757705820, 0.000000000000000000 ) ) ;
#45509 = CARTESIAN_POINT ( 'NONE',  ( -0.6823417656250003738, 2.030208333674753174, -1.181850606188749264 ) ) ;
#45510 = CARTESIAN_POINT ( 'NONE',  ( 0.1453861984699222620, 14.53092100591740810, 11.99911925323659290 ) ) ;
#45511 = CARTESIAN_POINT ( 'NONE',  ( 4.975479186090839612, 8.748550117173898855, 0.7216878364870438212 ) ) ;
#45512 = CARTESIAN_POINT ( 'NONE',  ( 4.387298408599741961, 0.1025060220480543544, 2.168864852262440301 ) ) ;
#45513 = DIRECTION ( 'NONE',  ( 0.6507913734559641616, -0.7592566023653004592, 0.000000000000000000 ) ) ;
#45515 = CARTESIAN_POINT ( 'NONE',  ( 3.772867777003403589, 1.732451475078290448, -0.6238847238279123797 ) ) ;
#45514 = CARTESIAN_POINT ( 'NONE',  ( -2.955314298098991266, 6.391691081183366485, 0.7216878364870317197 ) ) ;
#45517 = CARTESIAN_POINT ( 'NONE',  ( 6.620655732516666170, 7.629137130509104026, 2.326260288887294969 ) ) ;
#45516 = CARTESIAN_POINT ( 'NONE',  ( 0.000000000000000000, -6.532648833121171172, 0.000000000000000000 ) ) ;
#45518 = CARTESIAN_POINT ( 'NONE',  ( 5.495707582769355781, -2.191739722525353429, -0.0009102486706394352645 ) ) ;
#45519 = CARTESIAN_POINT ( 'NONE',  ( -1.499999999999993339, 10.64264068711930733, 1.232676135170975238E-14 ) ) ;
#45520 = CARTESIAN_POINT ( 'NONE',  ( 5.454102184832422928, 2.260192964246518166, -0.1051519175162188013 ) ) ;
#45521 = ORIENTED_EDGE ( 'NONE', *, *, #191199, .F. ) ;
#45522 = CARTESIAN_POINT ( 'NONE',  ( -3.975508435578610555, 7.849559089036333148, -0.01386331990411299175 ) ) ;
#45523 = CARTESIAN_POINT ( 'NONE',  ( 4.812217717264355876, 8.234349973070900219, 0.8868998539744571419 ) ) ;
#45524 = CARTESIAN_POINT ( 'NONE',  ( -4.773879485343255347, 8.583626809626847987, 0.000000000000000000 ) ) ;
#45525 = CARTESIAN_POINT ( 'NONE',  ( -0.07302493934789386354, 1.405922845961228962, 11.99988463978226250 ) ) ;
#45526 = CARTESIAN_POINT ( 'NONE',  ( 1.041466456679561059, 0.7221788661597589032, -1.615996624379830493 ) ) ;
#45527 = AXIS2_PLACEMENT_3D ( 'NONE', #15045, #115831, #81138 ) ;
#45528 = CARTESIAN_POINT ( 'NONE',  ( 4.828775420069912450, 1.386532772215205878, -1.459704157296830784 ) ) ;
#45529 = CARTESIAN_POINT ( 'NONE',  ( 6.657217119509961201, 7.725507046638470321, -1.199719254218446718 ) ) ;
#45530 = CARTESIAN_POINT ( 'NONE',  ( 4.594815077023072902, -0.4589311638903668111, -2.055181093106945855 ) ) ;
#45531 = CARTESIAN_POINT ( 'NONE',  ( 2.144012975658988740, 0.8210224433658172005, 1.730898686554068311 ) ) ;
#45532 = AXIS2_PLACEMENT_3D ( 'NONE', #37031, #200583, #169174 ) ;
#45533 = CARTESIAN_POINT ( 'NONE',  ( 4.681643115420508039, 4.356338477612361260, 0.7998128361456341429 ) ) ;
#45534 = CARTESIAN_POINT ( 'NONE',  ( 2.769919614283973264, -1.948520106842245525, 0.2860871629452500509 ) ) ;
#45535 = CARTESIAN_POINT ( 'NONE',  ( 5.115492516475182327, 1.653579564094692866, 1.159561630411933830 ) ) ;
#45536 = CARTESIAN_POINT ( 'NONE',  ( 1.727212824277712944, -1.762453432929488528, 0.6273722324065673650 ) ) ;
#45539 = ORIENTED_EDGE ( 'NONE', *, *, #25456, .T. ) ;
#45538 = CARTESIAN_POINT ( 'NONE',  ( 0.9668906521006037647, -1.505869814250645478, 1.178657042999963878 ) ) ;
#45537 = CARTESIAN_POINT ( 'NONE',  ( 5.637229722410256549, -1.556708995667484441, 0.7431856355405024317 ) ) ;
#45541 = CARTESIAN_POINT ( 'NONE',  ( 3.362058906508953449, 6.866226457661676719, -0.7216878364870267237 ) ) ;
#45540 = CARTESIAN_POINT ( 'NONE',  ( 0.9442952520863318044, 0.8911936224933308948, -2.019119535841918278 ) ) ;
#45542 = CARTESIAN_POINT ( 'NONE',  ( 0.6823417656249882723, 1.738541667008083991, -1.181850606188749264 ) ) ;
#45543 = CARTESIAN_POINT ( 'NONE',  ( 8.914649696185335870, 10.35917838609310593, -1.199719254218446718 ) ) ;
#45544 = CARTESIAN_POINT ( 'NONE',  ( 11.52888687719590344, 12.30576874894964057, -3.331331986263459388 ) ) ;
#45545 = CARTESIAN_POINT ( 'NONE',  ( -2.900957617708239678, -3.232243495192087757, 1.542507481629953103 ) ) ;
#45546 = LINE ( 'NONE', #62832, #6598 ) ;
#45547 = ORIENTED_EDGE ( 'NONE', *, *, #70130, .F. ) ;
#45548 = CARTESIAN_POINT ( 'NONE',  ( -1.249999999999966471, 8.500000000000000000, 9.921567416492214520 ) ) ;
#45549 = CARTESIAN_POINT ( 'NONE',  ( 0.8892259839063383353, 0.1505779921940515187, 2.064926437897919964 ) ) ;
#45550 = CARTESIAN_POINT ( 'NONE',  ( -1.201851678989727383E-14, 2.462500000000023004, 1.732050807568877637 ) ) ;
#45551 = CARTESIAN_POINT ( 'NONE',  ( 4.476163270806094552, 8.373940915915776273, 0.7998128361456462443 ) ) ;
#45552 = CARTESIAN_POINT ( 'NONE',  ( -5.540478329478883524, 9.615641817700700145, 0.000000000000000000 ) ) ;
#45553 = CARTESIAN_POINT ( 'NONE',  ( 5.041653019435334393, 6.975290837464928728, -1.599625672291269396 ) ) ;
#45554 = CARTESIAN_POINT ( 'NONE',  ( -0.005205762187880831615, -1.959593580757122089, -0.4885912094437401820 ) ) ;
#45555 = DIRECTION ( 'NONE',  ( 0.04529798058948776573, 0.000000000000000000, 0.9989735196462988798 ) ) ;
#45556 = CARTESIAN_POINT ( 'NONE',  ( -1.364683531250012516, 2.280208333674751842, 0.7879004041258379498 ) ) ;
#45557 = ORIENTED_EDGE ( 'NONE', *, *, #78727, .T. ) ;
#45559 = CARTESIAN_POINT ( 'NONE',  ( 2.198393463710220264, 5.716542807637226886, 0.7998128361456462443 ) ) ;
#45558 = CARTESIAN_POINT ( 'NONE',  ( 6.830524215763060347, -1.208013408316032322, 1.546442907991877558 ) ) ;
#45560 = CARTESIAN_POINT ( 'NONE',  ( 4.341172599035714619, -1.163090190446917083, 1.646587424817484324 ) ) ;
#45561 = CARTESIAN_POINT ( 'NONE',  ( 4.241352010100610137, 0.4139369872660918492, -1.870304626840668893 ) ) ;
#45562 = CARTESIAN_POINT ( 'NONE',  ( 3.193114300108112147, 1.729001323093733111, 1.346577201094656395 ) ) ;
#45563 = CARTESIAN_POINT ( 'NONE',  ( 1.499999999999987121, 1.035416667349484232, 0.8660254037844524744 ) ) ;
#45564 = CARTESIAN_POINT ( 'NONE',  ( 4.904545999335794271, -1.998481532559828189, -0.2423253454618880809 ) ) ;
#45565 = CARTESIAN_POINT ( 'NONE',  ( -7.206322340863467346, 8.366129804884193888, 1.199719254218450271 ) ) ;
#45567 = CARTESIAN_POINT ( 'NONE',  ( 5.554358401905552967, -1.342484540487314026, 1.637217851860258699 ) ) ;
#45566 = CARTESIAN_POINT ( 'NONE',  ( -2.765500147507697459, 5.209872024525476597, 1.082531754730560403 ) ) ;
#45569 = EDGE_CURVE ( 'NONE', #90194, #205352, #80974, .T. ) ;
#45568 = CARTESIAN_POINT ( 'NONE',  ( 0.6823417656249969321, 9.088541667008065872, -1.181850606188757036 ) ) ;
#45571 = CARTESIAN_POINT ( 'NONE',  ( -6.770317605177755382, 8.992066187497757213, 1.599625672291269396 ) ) ;
#45570 = CARTESIAN_POINT ( 'NONE',  ( 3.931257944464498166, -1.443263031577642463, -1.512909484191153897 ) ) ;
#45573 = ORIENTED_EDGE ( 'NONE', *, *, #34126, .T. ) ;
#45572 = CARTESIAN_POINT ( 'NONE',  ( 2.256509660847346943, -1.335373073873729943, 1.091610183656815503 ) ) ;
#45574 = CARTESIAN_POINT ( 'NONE',  ( 4.799148092389167175, -0.2621723519393297508, -2.104289960152181393 ) ) ;
#45575 = CARTESIAN_POINT ( 'NONE',  ( 6.474182045725470402, 7.511966127223233869, -1.199719254218446718 ) ) ;
#45576 = CARTESIAN_POINT ( 'NONE',  ( -5.608757509019735465, 5.634241678024821454, 0.4696088000558009679 ) ) ;
#45577 = CARTESIAN_POINT ( 'NONE',  ( 7.455003611050232237, -6.808400134080644150, 7.905503641038496454 ) ) ;
#45578 = DIRECTION ( 'NONE',  ( 0.000000000000000000, 1.000000000000000000, 0.000000000000000000 ) ) ;
#45579 = CARTESIAN_POINT ( 'NONE',  ( 5.133733721068893807, 9.141106441222381918, 1.040834085586084257E-14 ) ) ;
#45580 = ORIENTED_EDGE ( 'NONE', *, *, #131308, .F. ) ;
#45581 = CARTESIAN_POINT ( 'NONE',  ( -11.92619526248524409, 13.52744613914173932, -1.328859120100604585 ) ) ;
#45583 = CARTESIAN_POINT ( 'NONE',  ( 1.822642882514250218, 1.341887823972046201, -1.217030898042359643 ) ) ;
#45582 = CARTESIAN_POINT ( 'NONE',  ( 5.020262018810099924, 9.078999131912302900, 0.7998128361456331437 ) ) ;
#45584 = CARTESIAN_POINT ( 'NONE',  ( -5.880485940025243607, 7.883652901494672349, 1.599625672291269396 ) ) ;
#45585 = VERTEX_POINT ( 'NONE', #32329 ) ;
#45586 = CARTESIAN_POINT ( 'NONE',  ( 4.054051625686104998, 4.688480637177271149, -1.199719254218446718 ) ) ;
#45587 = VERTEX_POINT ( 'NONE', #34453 ) ;
#45588 = CARTESIAN_POINT ( 'NONE',  ( 6.547661840756936691, 6.603636667163397256, 0.7998128361456352531 ) ) ;
#45589 = CARTESIAN_POINT ( 'NONE',  ( 2.578518618993036693, -1.248033014721174228, 1.313194663545588003 ) ) ;
#45590 = CARTESIAN_POINT ( 'NONE',  ( 6.639320575229274546, 6.037277963978410433, 2.591643891269063360 ) ) ;
#45591 = CARTESIAN_POINT ( 'NONE',  ( 4.352817808933668431, 7.164511876539561896, 1.041257065902738477 ) ) ;
#45592 = ORIENTED_EDGE ( 'NONE', *, *, #136104, .T. ) ;
#45593 = CARTESIAN_POINT ( 'NONE',  ( 3.789374314311170000, -1.720299746930791684, 0.7104884466354021155 ) ) ;
#45594 = EDGE_CURVE ( 'NONE', #135468, #84217, #148224, .T. ) ;
#45595 = CARTESIAN_POINT ( 'NONE',  ( 2.056118223505171372, -1.176884799952466087, 1.511379468370318113 ) ) ;
#45596 = CARTESIAN_POINT ( 'NONE',  ( 0.3053143536290473525, -0.4923201697357786344, 1.757875871163572024 ) ) ;
#45597 = CARTESIAN_POINT ( 'NONE',  ( 0.4019237886466778820, 11.57366454968462932, 1.500000000000001554 ) ) ;
#45598 = DIRECTION ( 'NONE',  ( 1.276756478318932585E-15, -1.000000000000000000, 1.665334536937738262E-16 ) ) ;
#45599 = CARTESIAN_POINT ( 'NONE',  ( 4.646267551848549004, 8.309382712783076386, 0.4446711254955729165 ) ) ;
#45600 = CARTESIAN_POINT ( 'NONE',  ( -4.284013352238274841, 4.100363120473813794, -0.7216878364870207285 ) ) ;
#45601 = CARTESIAN_POINT ( 'NONE',  ( 6.941411460516762943, 11.04213777067082702, -0.7216878364870267237 ) ) ;
#45602 = CARTESIAN_POINT ( 'NONE',  ( 5.893399327195629311, -1.782088370946652622, 0.8386133760364660183 ) ) ;
#45603 = CARTESIAN_POINT ( 'NONE',  ( -4.042302355168801320, 7.867769847672247074, 0.7998128361456341429 ) ) ;
#45604 = CARTESIAN_POINT ( 'NONE',  ( -11.96212011828583677, 9.771875549500631308, -0.9569185076418453839 ) ) ;
#45605 = CARTESIAN_POINT ( 'NONE',  ( 6.685463922536254877, -0.9407050535897142352, 1.977304495687677521 ) ) ;
#45606 =( NAMED_UNIT ( * ) PLANE_ANGLE_UNIT ( ) SI_UNIT ( $, .RADIAN. ) );
#45607 = CARTESIAN_POINT ( 'NONE',  ( 4.858382476810707118, 0.7369543258428765675, 1.780043821814878413 ) ) ;
#45608 = CARTESIAN_POINT ( 'NONE',  ( -8.016948904382338981, 8.247528564734524892, -0.7998128361456291469 ) ) ;
#45609 = EDGE_CURVE ( 'NONE', #166283, #120928, #198014, .T. ) ;
#45610 = CARTESIAN_POINT ( 'NONE',  ( 1.729251940891060713, -1.720190037149814444, 0.6116943438041824166 ) ) ;
#45611 = CARTESIAN_POINT ( 'NONE',  ( 2.086817400036289794, -2.164668306305051804, -0.4287355390964405211 ) ) ;
#45612 = FILL_AREA_STYLE ('',( #196116 ) ) ;
#45613 = CARTESIAN_POINT ( 'NONE',  ( 0.4219365929402639215, -1.902980170924161385, 0.1897552588234762416 ) ) ;
#45614 = CARTESIAN_POINT ( 'NONE',  ( 0.3616804892651844239, -0.5289564462071428830, 1.897103703902315530 ) ) ;
#45615 = CARTESIAN_POINT ( 'NONE',  ( 2.524863302051027159, -1.811236869417539141, 0.7011504990855742525 ) ) ;
#45616 = VERTEX_POINT ( 'NONE', #98398 ) ;
#45617 = CARTESIAN_POINT ( 'NONE',  ( 0.6849224457974397717, -1.076149790962807495, -1.704679027301945649 ) ) ;
#45619 = CARTESIAN_POINT ( 'NONE',  ( 5.418752549068918789, -1.349321427123598038, 1.281850857350794959 ) ) ;
#45618 = CARTESIAN_POINT ( 'NONE',  ( -6.656127069666307072, 6.730179434224282886, 0.7998128361456341429 ) ) ;
#45620 = CARTESIAN_POINT ( 'NONE',  ( 5.387385936583818591, 7.378645907471495846, -1.599625672291283607 ) ) ;
#45621 = CARTESIAN_POINT ( 'NONE',  ( -11.33772467203841394, 13.50732847981850426, -3.600000000000000977 ) ) ;
#45622 = CARTESIAN_POINT ( 'NONE',  ( 1.403499169901393673, 7.376709478541975784, -4.304123474986169207 ) ) ;
#45623 = CARTESIAN_POINT ( 'NONE',  ( -5.687809136132860210, 6.594531066031826150, -1.199719254218446718 ) ) ;
#45624 = CARTESIAN_POINT ( 'NONE',  ( -6.291865805193673111, 9.498204651771386509, -1.199719254218452047 ) ) ;
#45625 = CARTESIAN_POINT ( 'NONE',  ( 0.9959476074029065540, -2.191739723303194332, 0.005169097091584088505 ) ) ;
#45626 = CARTESIAN_POINT ( 'NONE',  ( 4.365362273920252889, 4.195270195769483124, 0.7216878364870317197 ) ) ;
#45627 = CARTESIAN_POINT ( 'NONE',  ( 11.00039779440667154, -6.304807775344823284, -0.01400375819716699437 ) ) ;
#45628 = DIRECTION ( 'NONE',  ( -0.000000000000000000, -1.000000000000000000, -0.000000000000000000 ) ) ;
#45629 = CARTESIAN_POINT ( 'NONE',  ( 3.228933428962964758, 0.04559371896543929631, 1.825288036790246204 ) ) ;
#45630 = CARTESIAN_POINT ( 'NONE',  ( -4.295235737431041478, 3.905529869957963029, -0.7998128361456221525 ) ) ;
#45631 = CARTESIAN_POINT ( 'NONE',  ( -4.790108344329849110, 4.482881244673243337, 0.7998128361456341429 ) ) ;
#45632 = CARTESIAN_POINT ( 'NONE',  ( -6.026230196168996578, 7.163122537909742071, -1.192248477780058380 ) ) ;
#45633 = CARTESIAN_POINT ( 'NONE',  ( -1.968007779264361323, 0.3930682408332470956, 0.6607764497958683592 ) ) ;
#45634 = CARTESIAN_POINT ( 'NONE',  ( 9.134442807305049428, 11.67993591332117376, 1.599625672291281386 ) ) ;
#45635 = CARTESIAN_POINT ( 'NONE',  ( 1.031717895469780988, -1.221320771479022627, -1.489887157414800267 ) ) ;
#45636 = CARTESIAN_POINT ( 'NONE',  ( 5.049637047142223167, 1.450995767963231264, 1.320413740667214508 ) ) ;
#45637 =( GEOMETRIC_REPRESENTATION_CONTEXT ( 3 ) GLOBAL_UNCERTAINTY_ASSIGNED_CONTEXT ( ( #109206 ) ) GLOBAL_UNIT_ASSIGNED_CONTEXT ( ( #79686, #212872, #130649 ) ) REPRESENTATION_CONTEXT ( 'NONE', 'WORKASPACE' ) );
#45638 = CARTESIAN_POINT ( 'NONE',  ( -7.365103760721662951, 9.615707025640515937, 1.599625672291295375 ) ) ;
#45639 = CARTESIAN_POINT ( 'NONE',  ( 5.986088515633498197, 6.942523675449257858, -1.199719254218446718 ) ) ;
#45640 = EDGE_CURVE ( 'NONE', #15455, #172181, #65613, .T. ) ;
#45641 = CARTESIAN_POINT ( 'NONE',  ( 5.091441847573507928, -0.7891374179831472935, 2.044738775321436997 ) ) ;
#45642 = CARTESIAN_POINT ( 'NONE',  ( 4.630273154266905777, 5.360739087188218122, 1.199719254218464037 ) ) ;
#45643 = CARTESIAN_POINT ( 'NONE',  ( 4.118080132427735407, 2.055207691244304691, -0.2483996215696740451 ) ) ;
#45645 = CARTESIAN_POINT ( 'NONE',  ( -1.364683531250000748, 1.821875000341421913, 0.000000000000000000 ) ) ;
#45644 = DIRECTION ( 'NONE',  ( 0.000000000000000000, 1.000000000000000000, -8.546850786086437571E-32 ) ) ;
#45646 = ORIENTED_EDGE ( 'NONE', *, *, #24424, .F. ) ;
#45647 = CARTESIAN_POINT ( 'NONE',  ( 3.885566394551481562, -0.7213347477983514944, -2.182621754721993490 ) ) ;
#45649 = VERTEX_POINT ( 'NONE', #20329 ) ;
#45648 = CARTESIAN_POINT ( 'NONE',  ( 7.836249599018724865, 9.205007956019091608, -1.082531754730537976 ) ) ;
#45651 = CARTESIAN_POINT ( 'NONE',  ( 3.285556943749998737, -0.9552083328553737651, -1.896917185911906500 ) ) ;
#45650 = CARTESIAN_POINT ( 'NONE',  ( 5.506019780925567986, 8.477421273504887722, -1.082531754730548412 ) ) ;
#45652 = CARTESIAN_POINT ( 'NONE',  ( 6.620655732516649294, 4.698502813744664941, 2.488957606609870421 ) ) ;
#45653 = CARTESIAN_POINT ( 'NONE',  ( 0.000000000000000000, -5.199999999999996625, 0.000000000000000000 ) ) ;
#45654 = CARTESIAN_POINT ( 'NONE',  ( 4.259667731375265554, 0.9167342216760937523, 1.711951518900257430 ) ) ;
#45655 = ORIENTED_EDGE ( 'NONE', *, *, #78683, .F. ) ;
#45656 = CARTESIAN_POINT ( 'NONE',  ( 8.690413276235306128, 13.08263988900915109, -0.7216878364870267237 ) ) ;
#45657 = EDGE_LOOP ( 'NONE', ( #48655, #61812, #209455 ) ) ;
#45658 = CARTESIAN_POINT ( 'NONE',  ( 4.799029005866479736, -0.2398712174674077491, -1.897248949554980024 ) ) ;
#45659 = FACE_OUTER_BOUND ( 'NONE', #30980, .T. ) ;
#45660 = CARTESIAN_POINT ( 'NONE',  ( 6.405283072077849305, 1.437190941405818156, 0.9532465752533066938 ) ) ;
#45661 = CARTESIAN_POINT ( 'NONE',  ( 4.311732611912100666, -1.244383703160652610, -1.586670621409623116 ) ) ;
#45662 =( BOUNDED_CURVE ( )  B_SPLINE_CURVE ( 3, ( #165969, #177966, #211503, #63140 ),
 .UNSPECIFIED., .F., .T. ) 
 B_SPLINE_CURVE_WITH_KNOTS ( ( 4, 4 ),
 ( 0.5000000000000006661, 1.000000000000000000 ),
 .UNSPECIFIED. ) 
 CURVE ( )  GEOMETRIC_REPRESENTATION_ITEM ( )  RATIONAL_B_SPLINE_CURVE ( ( 0.9999999999999991118, 0.3333333333333333703, 0.3333333333333342585, 1.000000000000000000 ) ) 
 REPRESENTATION_ITEM ( '' )  );
#45663 = CARTESIAN_POINT ( 'NONE',  ( 5.368665641331539007, 5.365790791082648781, -0.7216878364870152884 ) ) ;
#45664 = CARTESIAN_POINT ( 'NONE',  ( 1.682535984017709874, -1.178549783888741320, 1.865657194899547733 ) ) ;
#45666 = CARTESIAN_POINT ( 'NONE',  ( -11.96215121607992415, 12.27166446219175988, 0.9565349792967585696 ) ) ;
#45665 = CARTESIAN_POINT ( 'NONE',  ( -10.34217224912604571, 10.96028913360221502, 0.7998128361456462443 ) ) ;
#45668 = CARTESIAN_POINT ( 'NONE',  ( 6.819637456808122167, -1.715783256332433115, 0.4333192982870024967 ) ) ;
#45667 = CARTESIAN_POINT ( 'NONE',  ( 1.552797837233742095, -1.793874147449931344, -1.073420256486889324 ) ) ;
#45669 = CARTESIAN_POINT ( 'NONE',  ( 5.590470263882489910, -0.4872053753022275169, 1.956560708789633285 ) ) ;
#45671 = CARTESIAN_POINT ( 'NONE',  ( 3.012002838297692886, -1.130384021687063534, -1.994099915080405294 ) ) ;
#45670 = CARTESIAN_POINT ( 'NONE',  ( 4.817943484809818600, 6.714296380401858499, 1.599625672291269396 ) ) ;
#45672 = B_SPLINE_CURVE_WITH_KNOTS ( 'NONE', 3,
 ( #140320, #139228, #172800, #204174, #203123, #73126 ),
 .UNSPECIFIED., .F., .F.,
 ( 4, 2, 4 ),
 ( 0.000000000000000000, 0.0003144386176887254184, 0.0006288772353774508368 ),
 .UNSPECIFIED. ) ;
#45673 = CARTESIAN_POINT ( 'NONE',  ( 1.112787002727889885, -1.698604791339110465, 0.3779700589620417217 ) ) ;
#45674 = DIRECTION ( 'NONE',  ( 0.000000000000000000, 1.000000000000000000, 0.000000000000000000 ) ) ;
#45675 = CARTESIAN_POINT ( 'NONE',  ( 0.7195771044254402060, -1.460395948178545344, -0.9342476737749583204 ) ) ;
#45676 = CARTESIAN_POINT ( 'NONE',  ( 1.360316468749987573, 0.2760416670081234369, 0.7853790794158701516 ) ) ;
#45677 = CARTESIAN_POINT ( 'NONE',  ( -0.4214947629262029150, 3.038568440852209562, 0.4183962726263074638 ) ) ;
#45678 = CARTESIAN_POINT ( 'NONE',  ( 1.662788154211870983, -0.7805772603099859763, -2.026187018951190133 ) ) ;
#45679 = CARTESIAN_POINT ( 'NONE',  ( 2.307827663788959871, -1.164988201124015577, -1.645758576239789051 ) ) ;
#45680 = CARTESIAN_POINT ( 'NONE',  ( 4.531250000000003553, -0.7852924748302230196, -1.895863743163982429 ) ) ;
#45681 = AXIS2_PLACEMENT_3D ( 'NONE', #172221, #6484, #173294 ) ;
#45682 = CARTESIAN_POINT ( 'NONE',  ( -1.500000000000013101, 1.410416667349486008, -0.8660254037844313801 ) ) ;
#45683 = CARTESIAN_POINT ( 'NONE',  ( 6.322878010905701451, 1.798576545740763644, 0.6907619847127777213 ) ) ;
#45684 = CARTESIAN_POINT ( 'NONE',  ( 0.6823417656249969321, 13.02604166700806232, -1.181850606188757036 ) ) ;
#45685 = CARTESIAN_POINT ( 'NONE',  ( 3.164521688127000854, 2.221583673635919354, -0.003682443279265367429 ) ) ;
#45686 = VERTEX_POINT ( 'NONE', #53917 ) ;
#45688 = AXIS2_PLACEMENT_3D ( 'NONE', #172420, #27216, #155103 ) ;
#45687 = DIRECTION ( 'NONE',  ( 0.000000000000000000, 1.000000000000000000, 0.000000000000000000 ) ) ;
#45689 =( LENGTH_UNIT ( ) NAMED_UNIT ( * ) SI_UNIT ( .MILLI., .METRE. ) );
#45690 = CARTESIAN_POINT ( 'NONE',  ( 7.456094412511537151, 10.78619501698377370, 1.199719254218460707 ) ) ;
#45691 = ADVANCED_FACE ( 'NONE', ( #203333 ), #54986, .F. ) ;
#45692 = CYLINDRICAL_SURFACE ( 'NONE', #142485, 0.3999999999999997446 ) ;
#45693 = CARTESIAN_POINT ( 'NONE',  ( 5.917484386527373630, -0.9743193633129590969, -1.441955756940280997 ) ) ;
#45694 = CARTESIAN_POINT ( 'NONE',  ( 3.525789274851616639, 1.914599547803575330, -0.4273510147508317036 ) ) ;
#45696 = CARTESIAN_POINT ( 'NONE',  ( -6.399085315970151733, 7.528316292462387871, -1.082531754730544860 ) ) ;
#45695 = CARTESIAN_POINT ( 'NONE',  ( 2.333974999846879061, 5.874721266463329705, -0.7998128361456291469 ) ) ;
#45697 = CARTESIAN_POINT ( 'NONE',  ( -1.286956418854592332, 4.047654341997461991, 0.4592741676706398324 ) ) ;
#45698 = CARTESIAN_POINT ( 'NONE',  ( 5.044316441076016844, 2.255832582719615065, 0.1735265121041371095 ) ) ;
#45699 = CARTESIAN_POINT ( 'NONE',  ( 2.137244103193221889, -0.09901990427806567352, -2.060404765751827405 ) ) ;
#45700 = CARTESIAN_POINT ( 'NONE',  ( -5.343885102080728977, 9.386283052402845328, 0.7998128361456481317 ) ) ;
#45701 = ORIENTED_EDGE ( 'NONE', *, *, #83796, .T. ) ;
#45702 = CARTESIAN_POINT ( 'NONE',  ( 0.7499999999999885647, 1.847916667349486231, -1.299038105676652899 ) ) ;
#45703 = CARTESIAN_POINT ( 'NONE',  ( 3.585083614955933307, 1.692364770286663322, -0.7970176776704935850 ) ) ;
#45704 = CARTESIAN_POINT ( 'NONE',  ( 2.478840559695635548, -1.729657056378102853, -0.1252908626025364403 ) ) ;
#45705 = CARTESIAN_POINT ( 'NONE',  ( 6.269083535738129598, 2.097726667780253074, -0.6343229546324488100 ) ) ;
#45706 = CARTESIAN_POINT ( 'NONE',  ( 6.159233218726320125, -1.974841252017808468, -1.193533401095113300 ) ) ;
#45707 = CARTESIAN_POINT ( 'NONE',  ( 3.836934241894359054, 0.3148432204054998351, 2.138525872868973998 ) ) ;
#45708 = CARTESIAN_POINT ( 'NONE',  ( 4.277243253991915850, 1.269349932698702110, 1.469746654517690487 ) ) ;
#45709 = CARTESIAN_POINT ( 'NONE',  ( -4.297571505407598025, 5.076550180139354218, 1.082531754730558626 ) ) ;
#45710 = ADVANCED_FACE ( 'NONE', ( #142400 ), #113573, .T. ) ;
#45712 = ORIENTED_EDGE ( 'NONE', *, *, #81748, .T. ) ;
#45711 = CARTESIAN_POINT ( 'NONE',  ( 6.520764494017629254, 1.745421825204738431, 0.6730592012400560264 ) ) ;
#45713 = CARTESIAN_POINT ( 'NONE',  ( 4.124567353486244592, 7.428622122647839277, 0.6979301818166357974 ) ) ;
#45714 = CARTESIAN_POINT ( 'NONE',  ( 0.000000000000000000, 11.29999999999998117, 0.000000000000000000 ) ) ;
#45715 = CARTESIAN_POINT ( 'NONE',  ( 0.01804983835817890528, -0.5593552815991027494, 2.045460531183339814 ) ) ;
#45716 = CARTESIAN_POINT ( 'NONE',  ( -0.6801582343750282034, 2.432291667008048996, 1.178068619123807004 ) ) ;
#45717 = CARTESIAN_POINT ( 'NONE',  ( 5.695935454815424848, 1.779625283580280382, 0.9480427965274510482 ) ) ;
#45718 = CARTESIAN_POINT ( 'NONE',  ( -4.419594887930571758, 4.258541578781506409, 1.214306433183764966E-14 ) ) ;
#45719 = CARTESIAN_POINT ( 'NONE',  ( 6.584456157731144899, 10.83361595066169514, -0.7998128361456291469 ) ) ;
#45720 = CARTESIAN_POINT ( 'NONE',  ( 5.695833931072550094, 5.817763472438987726, 0.000000000000000000 ) ) ;
#45721 = CARTESIAN_POINT ( 'NONE',  ( 3.703562413045482060, -0.5285312144065814621, 1.747510042522756990 ) ) ;
#45722 = CARTESIAN_POINT ( 'NONE',  ( 2.011028756337205348, 1.635159560789069655, -1.482119803565529859 ) ) ;
#45723 = ORIENTED_EDGE ( 'NONE', *, *, #38054, .T. ) ;
#45724 = CARTESIAN_POINT ( 'NONE',  ( -4.136646265500958819, 7.840188053144158786, -0.7216878364870458196 ) ) ;
#45725 = CARTESIAN_POINT ( 'NONE',  ( 0.000000000000000000, 8.999999999999998224, 0.000000000000000000 ) ) ;
#45726 = CARTESIAN_POINT ( 'NONE',  ( -7.670162217029145246, 9.971608557999250166, 1.599625672291295375 ) ) ;
#45727 = CARTESIAN_POINT ( 'NONE',  ( 0.4748752182902976071, -1.459934291025711373, 1.395986992609834276 ) ) ;
#45728 = CARTESIAN_POINT ( 'NONE',  ( 1.629697543846151619, -0.2563088357964183883, 2.104862515383609800 ) ) ;
#45729 = ORIENTED_EDGE ( 'NONE', *, *, #119819, .F. ) ;
#45730 = CARTESIAN_POINT ( 'NONE',  ( -5.448397627845328550, 7.449826213943242514, 1.599625672291263179 ) ) ;
#45731 = CARTESIAN_POINT ( 'NONE',  ( 2.131498006616658891, 1.782543213153169548, -0.5345681993311669489 ) ) ;
#45732 = CIRCLE ( 'NONE', #142530, 0.09999999999999971412 ) ;
#45733 = CARTESIAN_POINT ( 'NONE',  ( 5.138703914779377158, 5.953908307786102583, 1.199719254218462483 ) ) ;
#45734 = CARTESIAN_POINT ( 'NONE',  ( 5.911025222378588850, 1.816451602635826612, 0.9735456368637726010 ) ) ;
#45735 = CARTESIAN_POINT ( 'NONE',  ( 6.152970239395502361, 1.038990588714868490, 1.728003889287746286 ) ) ;
#45736 = ORIENTED_EDGE ( 'NONE', *, *, #213110, .T. ) ;
#45737 = CARTESIAN_POINT ( 'NONE',  ( -8.839026081105473054, 12.39961529701003684, -1.199719254218446718 ) ) ;
#45738 = CARTESIAN_POINT ( 'NONE',  ( 3.439906511156048285, 0.8199118703316324863, -1.631291955839441865 ) ) ;
#45741 = ORIENTED_EDGE ( 'NONE', *, *, #136759, .T. ) ;
#45740 = CARTESIAN_POINT ( 'NONE',  ( -5.856132087369688044, 6.175168335346238990, -0.9273813317931516309 ) ) ;
#45739 = CARTESIAN_POINT ( 'NONE',  ( -3.657667580636712934, 7.489305620709952649, -0.7998128361456481317 ) ) ;
#45742 = CARTESIAN_POINT ( 'NONE',  ( 6.536750166778501736, 6.811520125210166476, 0.4662371894542677864 ) ) ;
#45743 = CARTESIAN_POINT ( 'NONE',  ( 6.556017512941495262, 1.755498886817616677, -0.9912500394320120645 ) ) ;
#45744 = CARTESIAN_POINT ( 'NONE',  ( 5.349485151062911115, 1.838858031828109363, -0.09410559872920226665 ) ) ;
#45745 = CARTESIAN_POINT ( 'NONE',  ( 0.07680821025391955381, 1.395885924038504644, -2.068540888291516833 ) ) ;
#45746 = CARTESIAN_POINT ( 'NONE',  ( 4.178580530314169650, -1.330465218273884087, 1.885386248989364466 ) ) ;
#45747 = CARTESIAN_POINT ( 'NONE',  ( 5.071631979963703962, 8.074598522336444262, 1.199719254218451159 ) ) ;
#45748 = CARTESIAN_POINT ( 'NONE',  ( 5.975883356200852425, 1.282301362320131588, 1.740048508431484953 ) ) ;
#45749 = CARTESIAN_POINT ( 'NONE',  ( 1.487729058832359952, -1.932848847819462756, -0.1887428500492206451 ) ) ;
#45750 = ORIENTED_EDGE ( 'NONE', *, *, #188907, .F. ) ;
#45751 = CARTESIAN_POINT ( 'NONE',  ( 5.097139630348237027, 1.187786601409031695, -1.967583100176452549 ) ) ;
#45752 = DIRECTION ( 'NONE',  ( 0.000000000000000000, 0.000000000000000000, -1.000000000000000000 ) ) ;
#45753 = CARTESIAN_POINT ( 'NONE',  ( -5.164730172163054966, 4.990216387137135889, -0.7998128361456362523 ) ) ;
#45754 = CARTESIAN_POINT ( 'NONE',  ( 4.311305935566238645, -0.3199438451688824125, 1.842931056080451935 ) ) ;
#45755 = ORIENTED_EDGE ( 'NONE', *, *, #101405, .F. ) ;
#45759 = EDGE_CURVE ( 'NONE', #97721, #208480, #209469, .T. ) ;
#45758 = CARTESIAN_POINT ( 'NONE',  ( -4.437261413422502798, 8.398831758960053406, 0.000000000000000000 ) ) ;
#45757 = CARTESIAN_POINT ( 'NONE',  ( -0.7500000000000249800, 0.2229166673494847872, 1.299038105676659116 ) ) ;
#45756 = CARTESIAN_POINT ( 'NONE',  ( 1.968876373762207255, -1.476028252698018628, 1.215921256797661609 ) ) ;
#45760 = CARTESIAN_POINT ( 'NONE',  ( 4.178501018151202118, -1.271701901513167421, 1.803451139310302986 ) ) ;
#45761 = CARTESIAN_POINT ( 'NONE',  ( 6.883263157960393563, 4.695771316066229772, 2.508818740863460572 ) ) ;
#45762 = CARTESIAN_POINT ( 'NONE',  ( 2.354312230267378236, 5.898448035287240820, -0.7998128361456281477 ) ) ;
#45763 = CARTESIAN_POINT ( 'NONE',  ( 5.017926250389229459, 8.868348035513836436, 0.000000000000000000 ) ) ;
#45764 = CARTESIAN_POINT ( 'NONE',  ( -9.459838494033043332, 12.05956421450382088, 1.599625672291281386 ) ) ;
#45765 = CARTESIAN_POINT ( 'NONE',  ( -5.709392084686210289, 8.714688961225625974, 1.082531754730550855 ) ) ;
#45766 = CARTESIAN_POINT ( 'NONE',  ( 1.915242260480106706, -0.2453889982298693984, 1.955985308386765542 ) ) ;
#45767 = ADVANCED_FACE ( 'NONE', ( #86415 ), #152482, .T. ) ;
#45768 = CARTESIAN_POINT ( 'NONE',  ( 1.396046310939329738, 1.748920304266964543, 1.505474166573782968 ) ) ;
#45769 = CARTESIAN_POINT ( 'NONE',  ( 2.277722772326017608, -1.903703133612335119, 0.4737097981617058862 ) ) ;
#45770 = CARTESIAN_POINT ( 'NONE',  ( -1.387358672534699799, 7.315968950353656020, 4.254625267138158584 ) ) ;
#45771 = CARTESIAN_POINT ( 'NONE',  ( 4.786014635464308498, -1.264713950826271027, -1.629283840103493253 ) ) ;
#45772 = CARTESIAN_POINT ( 'NONE',  ( 5.070386261830877928, 5.978167395966564435, -1.082531754730548412 ) ) ;
#45773 = CARTESIAN_POINT ( 'NONE',  ( 4.179656494762836516, 8.098292687190454586, -0.7998128361456362523 ) ) ;
#45774 = EDGE_LOOP ( 'NONE', ( #183929, #146447, #139733, #150545 ) ) ;
#45775 = CARTESIAN_POINT ( 'NONE',  ( -8.462260433223891098, 13.02438760540324481, -0.7998128361456281477 ) ) ;
#45776 = CARTESIAN_POINT ( 'NONE',  ( -3.285556943750000070, -0.1093749995220438809, 0.000000000000000000 ) ) ;
#45777 = CARTESIAN_POINT ( 'NONE',  ( 8.224992744984721327, 12.74757530245756243, 1.040834085586084257E-14 ) ) ;
#45778 = CARTESIAN_POINT ( 'NONE',  ( 1.006951398661716901, 0.6282198290366995952, 2.078224816918782025 ) ) ;
#45779 = CARTESIAN_POINT ( 'NONE',  ( 6.378184920586140727, 6.405913593630768510, 0.000000000000000000 ) ) ;
#45780 = B_SPLINE_CURVE_WITH_KNOTS ( 'NONE', 3,
 ( #214398, #150533, #198183, #3163, #68168, #134300, #120223, #200307, #181931, #66027, #184067, #118081, #35687, #185125, #101763, #36750 ),
 .UNSPECIFIED., .F., .F.,
 ( 4, 3, 3, 3, 3, 4 ),
 ( 0.000000000000000000, 4.381999914579121551E-06, 1.110488615493335718E-05, 1.784390311306779410E-05, 2.460054645147216775E-05, 3.136851507421684792E-05 ),
 .UNSPECIFIED. ) ;
#45781 = CARTESIAN_POINT ( 'NONE',  ( -1.874158809982179319, 3.299964346911585356, 0.3999999999999993006 ) ) ;
#45782 = CARTESIAN_POINT ( 'NONE',  ( 0.000000000000000000, 5.999999999999998224, 0.000000000000000000 ) ) ;
#45783 = CARTESIAN_POINT ( 'NONE',  ( 2.372138566722302500, -1.154253592077842727, 1.471842878544211031 ) ) ;
#45784 = CARTESIAN_POINT ( 'NONE',  ( 6.802040682177005415, -2.161276877365316818, 0.04550429416337595928 ) ) ;
#45786 = CARTESIAN_POINT ( 'NONE',  ( 6.827182134110177714, 4.703275060517408512, 2.273677308227497917 ) ) ;
#45785 = DIRECTION ( 'NONE',  ( -5.578564026256490882E-16, -1.000000000000000000, -9.066213480720158442E-32 ) ) ;
#45787 = CARTESIAN_POINT ( 'NONE',  ( -1.402160292154681736E-14, -0.3031249996585801965, -1.575800808251665908 ) ) ;
#45788 = CARTESIAN_POINT ( 'NONE',  ( 2.209489775926488431, 1.479274643242427301, 1.211860329591994745 ) ) ;
#45789 = CARTESIAN_POINT ( 'NONE',  ( 3.906921071489596997, 1.517988030950194744, 0.9097272527330434455 ) ) ;
#45790 = CARTESIAN_POINT ( 'NONE',  ( 2.016128127738999076, -1.911839501640894001, 0.04842977492004740814 ) ) ;
#45791 = CARTESIAN_POINT ( 'NONE',  ( -6.566226467720086113, 6.555019055295208119, 1.040834085586084257E-14 ) ) ;
#45792 = CARTESIAN_POINT ( 'NONE',  ( 5.817977454128726578, 0.9396041113334742123, -1.669243033268079879 ) ) ;
#45793 = CARTESIAN_POINT ( 'NONE',  ( -0.7500000000000249800, -0.8083333333333136972, 1.299038105676659116 ) ) ;
#45794 = CARTESIAN_POINT ( 'NONE',  ( 6.443809999611881167, 1.357174585993505378, 1.427557633841854967 ) ) ;
#45795 = CARTESIAN_POINT ( 'NONE',  ( -0.7500000000000215383, 4.191666666666690411, 1.299038105676671107 ) ) ;
#45796 = CARTESIAN_POINT ( 'NONE',  ( -15.75000000000000000, 10.90000000000000036, 1.099999999999996758 ) ) ;
#45797 = CARTESIAN_POINT ( 'NONE',  ( 5.067206508511894469, 0.1826785619755930679, -1.861722072867748823 ) ) ;
#45799 = ORIENTED_EDGE ( 'NONE', *, *, #77256, .T. ) ;
#45798 = CARTESIAN_POINT ( 'NONE',  ( 1.383131112650197281, 1.687622997524572677, -0.6969523973551354779 ) ) ;
#45801 = CARTESIAN_POINT ( 'NONE',  ( 4.607663176575717223, 8.357619647684677133, 0.2284409323990380658 ) ) ;
#45800 = CARTESIAN_POINT ( 'NONE',  ( 4.740968412965463230, 0.3751893352213676591, 2.174603215771487630 ) ) ;
#45802 = CARTESIAN_POINT ( 'NONE',  ( -1.364683531249997417, 5.821875000341418804, 1.214306433183764966E-14 ) ) ;
#45803 = CARTESIAN_POINT ( 'NONE',  ( 2.260285141513069362, -2.062262451202213853, 0.04833688706953364472 ) ) ;
#45804 = CARTESIAN_POINT ( 'NONE',  ( 5.717788096661236885, 7.693838750903348789, 1.599625672291267398 ) ) ;
#45805 = CARTESIAN_POINT ( 'NONE',  ( -7.503547950159405566, 10.84155747757291266, 1.199719254218453823 ) ) ;
#45806 = CARTESIAN_POINT ( 'NONE',  ( 10.22692794340986921, 10.82583744360002243, 0.000000000000000000 ) ) ;
#45807 = CARTESIAN_POINT ( 'NONE',  ( 1.393602545685229011, 3.362046851755900345, 0.1272763605452785218 ) ) ;
#45808 = CARTESIAN_POINT ( 'NONE',  ( 0.07479286986305289098, 7.629137130509083597, -2.455503679634088776 ) ) ;
#45809 = CARTESIAN_POINT ( 'NONE',  ( 4.993145711582793744, 9.047363440147082159, -0.7998128361456481317 ) ) ;
#45810 = ORIENTED_EDGE ( 'NONE', *, *, #201793, .T. ) ;
#45811 = CARTESIAN_POINT ( 'NONE',  ( 5.055165704564410944, 1.723227314588217318, -1.147259442322377865 ) ) ;
#45812 = CARTESIAN_POINT ( 'NONE',  ( 0.6823417656249864960, -1.011458332991911568, -1.181850606188749264 ) ) ;
#45813 = CARTESIAN_POINT ( 'NONE',  ( 3.022914066069124051, 2.034213141994867247, 0.7313807043239917149 ) ) ;
#45814 = CARTESIAN_POINT ( 'NONE',  ( -4.638545736399841246, 8.340143690112583386, 0.3695662286686048903 ) ) ;
#45815 = CARTESIAN_POINT ( 'NONE',  ( 3.457679895445249674, -1.530724978927421986, -1.317682070945853656 ) ) ;
#45816 = CARTESIAN_POINT ( 'NONE',  ( 7.501945787865619941, -5.223163706540480788, 8.013579835756337033 ) ) ;
#45817 = ORIENTED_EDGE ( 'NONE', *, *, #112585, .T. ) ;
#45819 = CARTESIAN_POINT ( 'NONE',  ( 5.978782553946477840, 9.919070713005490703, 1.040834085586084257E-14 ) ) ;
#45818 = CARTESIAN_POINT ( 'NONE',  ( -3.475000000000000533, -1.399999999999998579, 0.000000000000000000 ) ) ;
#45820 = CARTESIAN_POINT ( 'NONE',  ( -5.302647476276252547, 5.359045941843285199, 0.7216878364870257245 ) ) ;
#45821 = CARTESIAN_POINT ( 'NONE',  ( 1.850796360583713884, -1.845628094615419768, -0.8128149310912060610 ) ) ;
#45822 = CARTESIAN_POINT ( 'NONE',  ( 5.794512526436308875, 1.792401445336734733, -1.260760892635464980 ) ) ;
#45823 = CARTESIAN_POINT ( 'NONE',  ( 0.7499999999999902300, 5.097916667349482012, -1.299038105676658228 ) ) ;
#45824 = CARTESIAN_POINT ( 'NONE',  ( 4.570513122935188299, 0.7371126809179430195, 1.764830652192488580 ) ) ;
#45825 = CARTESIAN_POINT ( 'NONE',  ( -4.790108344329849110, 4.482881244673243337, 0.7998128361456341429 ) ) ;
#45826 = CARTESIAN_POINT ( 'NONE',  ( 7.429504990164394584, 7.770103364721017591, 1.040834085586084257E-14 ) ) ;
#45828 = CARTESIAN_POINT ( 'NONE',  ( 3.778922869151004171, 1.701937167235707982, -1.081084515101193633 ) ) ;
#45827 = CARTESIAN_POINT ( 'NONE',  ( -8.093854517234044366, 11.42628545587295186, 1.082531754730549967 ) ) ;
#45829 = CARTESIAN_POINT ( 'NONE',  ( 1.364683531249997417, 13.54687500034139980, 2.602085213965210642E-15 ) ) ;
#45830 = CARTESIAN_POINT ( 'NONE',  ( -3.006876207180748217, 6.730049018344652190, -0.7998128361456481317 ) ) ;
#45831 = CARTESIAN_POINT ( 'NONE',  ( 5.508750344372229435, 1.303470515519134842, -1.129639352617429537 ) ) ;
#45832 = CARTESIAN_POINT ( 'NONE',  ( -0.1399997263889819765, 0.7174702203470960660, -2.082715917450683740 ) ) ;
#45833 = CARTESIAN_POINT ( 'NONE',  ( 4.518945272056516416, 4.166524327021037699, 0.7998128361456341429 ) ) ;
#45834 = CARTESIAN_POINT ( 'NONE',  ( -6.776370306708066060, -7.161464053357566861, -6.781144757626042185 ) ) ;
#45835 = CARTESIAN_POINT ( 'NONE',  ( 3.948449050077836642, 5.629609863222681199, 1.599625672291267398 ) ) ;
#45836 = CARTESIAN_POINT ( 'NONE',  ( 1.734723475976807094E-15, -3.469446951953614189E-15, 0.2971265334020881110 ) ) ;
#45838 = AXIS2_PLACEMENT_3D ( 'NONE', #16374, #66175, #112907 ) ;
#45837 = CARTESIAN_POINT ( 'NONE',  ( 0.5146170122050791607, 0.7890519337857507809, 1.914186188738425942 ) ) ;
#45839 = CARTESIAN_POINT ( 'NONE',  ( 6.812946544903684121, -1.603000239855886466, 1.309962327488790157 ) ) ;
#45840 = VERTEX_POINT ( 'NONE', #153555 ) ;
#45841 = CARTESIAN_POINT ( 'NONE',  ( 4.863805359840983833, 0.5633507197577434233, -1.721726771216978369 ) ) ;
#45843 = CARTESIAN_POINT ( 'NONE',  ( 4.366607992053101128, 7.252070536440704096, -1.199719254218448494 ) ) ;
#45842 = AXIS2_PLACEMENT_3D ( 'NONE', #36396, #69941, #122011 ) ;
#45844 = CARTESIAN_POINT ( 'NONE',  ( -4.909967638851771454, 4.671257834700952571, -0.2941531795261614346 ) ) ;
#45845 = CARTESIAN_POINT ( 'NONE',  ( 6.375650462676996533, 0.3020505593925585375, -1.785944618546008833 ) ) ;
#45846 = CARTESIAN_POINT ( 'NONE',  ( 6.672020991256494504, 6.956648375986938859, 0.000000000000000000 ) ) ;
#45847 = CARTESIAN_POINT ( 'NONE',  ( 11.15780464429275121, 9.116777561061677915, -4.430755320266929864 ) ) ;
#45848 = CARTESIAN_POINT ( 'NONE',  ( 2.519692321801832335, -1.262790281060278907, -1.790845962237663791 ) ) ;
#45849 = ORIENTED_EDGE ( 'NONE', *, *, #177010, .F. ) ;
#45851 = CARTESIAN_POINT ( 'NONE',  ( 7.716561984472250835, 12.15440608185967086, 1.040834085586084257E-14 ) ) ;
#45850 = CARTESIAN_POINT ( 'NONE',  ( 0.7835587076311965049, -1.864072139945194717, 0.6119401183290391621 ) ) ;
#45852 = CARTESIAN_POINT ( 'NONE',  ( 4.481992950489037675, -1.915292616430896544, -0.04288535553729002497 ) ) ;
#45853 = CARTESIAN_POINT ( 'NONE',  ( 0.000000000000000000, -4.517653975874099892, -1.376945625684933061 ) ) ;
#45854 = CARTESIAN_POINT ( 'NONE',  ( -6.502161524297833672, 6.757477167027320597, -0.005777863564433716181 ) ) ;
#45855 = CARTESIAN_POINT ( 'NONE',  ( -0.07968760456310633455, 7.629137130509075604, -2.426417496045676803 ) ) ;
#45856 = CARTESIAN_POINT ( 'NONE',  ( -1.364683531250014514, -0.7614583329919104582, -0.7879004041258359514 ) ) ;
#45858 = ORIENTED_EDGE ( 'NONE', *, *, #15314, .F. ) ;
#45857 = CARTESIAN_POINT ( 'NONE',  ( 6.155038550924155416, 6.283225852274053835, 0.7216878364870317197 ) ) ;
#45859 = CARTESIAN_POINT ( 'NONE',  ( -7.537970219518066450, 11.73812298950569044, -0.7216878364870267237 ) ) ;
#45860 = CARTESIAN_POINT ( 'NONE',  ( 1.850665834824256173, 0.6780317805383448970, 2.052694239800388676 ) ) ;
#45861 = CARTESIAN_POINT ( 'NONE',  ( -3.135678666510573365, 6.880318554229450712, 0.000000000000000000 ) ) ;
#45862 = CARTESIAN_POINT ( 'NONE',  ( 4.903208829997618423, 5.749440385532527564, -1.199719254218450271 ) ) ;
#45863 = CARTESIAN_POINT ( 'NONE',  ( 1.957752326685862077, 1.820926393389955988, -0.1310869387763091420 ) ) ;
#45864 = CARTESIAN_POINT ( 'NONE',  ( -0.01710467543277957581, -1.380256469788909035, 1.610041658517608054 ) ) ;
#45865 = CARTESIAN_POINT ( 'NONE',  ( 4.823181420811452291, -0.08861582515604787824, 1.823562061424352621 ) ) ;
#45866 = CARTESIAN_POINT ( 'NONE',  ( 9.314578176993711267, 12.86557944855549351, 8.945654112524721313 ) ) ;
#45867 = ORIENTED_EDGE ( 'NONE', *, *, #72048, .T. ) ;
#45868 = CARTESIAN_POINT ( 'NONE',  ( 3.385164793666879834, 0.04568167736355076974, 1.969186301724828336 ) ) ;
#45869 = ORIENTED_EDGE ( 'NONE', *, *, #126844, .T. ) ;
#45870 = CARTESIAN_POINT ( 'NONE',  ( 5.952673665805181535, -1.667821083538678861, -0.9947414763863350329 ) ) ;
#45871 = VERTEX_POINT ( 'NONE', #39805 ) ;
#45872 = CARTESIAN_POINT ( 'NONE',  ( -5.264308783856126439, 9.363720357799287797, -0.7998128361456362523 ) ) ;
#45874 = CARTESIAN_POINT ( 'NONE',  ( 5.748313822965784858, 1.043546352714582071, -1.845953426139717246 ) ) ;
#45873 = CARTESIAN_POINT ( 'NONE',  ( 6.367489420273535039, 7.457767740854454708, -1.199719254218452047 ) ) ;
#45875 = CARTESIAN_POINT ( 'NONE',  ( 6.156811153937166381, 10.19704708965311468, 0.000000000000000000 ) ) ;
#45877 = ORIENTED_EDGE ( 'NONE', *, *, #59437, .F. ) ;
#45876 = CARTESIAN_POINT ( 'NONE',  ( 2.947808941170467545, -1.285945688040548207, -1.415481726668985196 ) ) ;
#45878 = CARTESIAN_POINT ( 'NONE',  ( 4.536316240020330071, 7.212700717958764329, -1.298556639521078582 ) ) ;
#45879 = CARTESIAN_POINT ( 'NONE',  ( -15.75000000000000000, 13.79999999999999893, -0.7000000000000009548 ) ) ;
#45880 = DIRECTION ( 'NONE',  ( 1.000000000000000000, -0.000000000000000000, -0.000000000000000000 ) ) ;
#45881 = AXIS2_PLACEMENT_3D ( 'NONE', #6395, #21565, #37855 ) ;
#45882 = CARTESIAN_POINT ( 'NONE',  ( 4.776043607066285723, 1.990852085817075068, -0.2977186459587366496 ) ) ;
#45883 = CARTESIAN_POINT ( 'NONE',  ( -5.884810976140032679, 6.155599488313971079, -0.9398637431582609336 ) ) ;
#45884 = CARTESIAN_POINT ( 'NONE',  ( 6.111906964637446649, -1.811269838261083232, 0.2284818145076653595 ) ) ;
#45885 = CARTESIAN_POINT ( 'NONE',  ( 1.188034388246852480, -1.312013912954514971, -1.601590607232979524 ) ) ;
#45886 = CARTESIAN_POINT ( 'NONE',  ( -6.860062538834774237, 10.94723069537516302, 0.7216878364870458196 ) ) ;
#45887 = CARTESIAN_POINT ( 'NONE',  ( -5.857301623663916601, 7.199535845156014524, -1.157093103336486628 ) ) ;
#45888 = DIRECTION ( 'NONE',  ( 0.000000000000000000, -1.000000000000000000, 0.000000000000000000 ) ) ;
#45889 = CARTESIAN_POINT ( 'NONE',  ( 6.403191318657627029, 1.556466930477506505, 1.037356966126230517 ) ) ;
#45890 = CARTESIAN_POINT ( 'NONE',  ( 7.474622759835693131, 7.614814729430110951, -0.7998128361456281477 ) ) ;
#45891 = DIRECTION ( 'NONE',  ( 0.6507913734559640506, -0.7592566023653004592, 0.000000000000000000 ) ) ;
#45892 = CARTESIAN_POINT ( 'NONE',  ( -8.012344526598182026E-15, 11.35937500034139980, -1.575800808251669460 ) ) ;
#45893 = CARTESIAN_POINT ( 'NONE',  ( -5.786632634934295361, 5.645492917045106473, 0.7998128361456341429 ) ) ;
#45895 = CARTESIAN_POINT ( 'NONE',  ( -6.851666526859749418, 9.086973262793417661, -1.599625672291271394 ) ) ;
#45894 = CARTESIAN_POINT ( 'NONE',  ( 8.072398248062480519, -5.212532583863434432, -7.453913518772576019 ) ) ;
#45896 = ADVANCED_FACE ( 'NONE', ( #122209 ), #188388, .T. ) ;
#45897 = CARTESIAN_POINT ( 'NONE',  ( 3.252318870217449920, 1.690988760736945373, -0.3835568649490900817 ) ) ;
#45898 = AXIS2_PLACEMENT_3D ( 'NONE', #176578, #76923, #196028 ) ;
#45899 = CARTESIAN_POINT ( 'NONE',  ( -5.579343907223557331, 6.467988298970945849, 1.199719254218450271 ) ) ;
#45900 = CIRCLE ( 'NONE', #194614, 0.07999999999999961309 ) ;
#45901 = CARTESIAN_POINT ( 'NONE',  ( 1.745070579777140418, -0.2997347613497360896, -2.048299739058518920 ) ) ;
#45902 = CARTESIAN_POINT ( 'NONE',  ( 1.933370326505511105, -1.702675829696152388, -1.258230627273223545 ) ) ;
#45903 = CARTESIAN_POINT ( 'NONE',  ( 5.515469562660962666, 5.329135999392899947, 0.7998128361456341429 ) ) ;
#45904 = CARTESIAN_POINT ( 'NONE',  ( 7.618792255875527886, 10.97600916757510170, 1.199719254218460707 ) ) ;
#45905 = CARTESIAN_POINT ( 'NONE',  ( -5.346851039111045978, 6.199209027673978412, -1.060622344683157747 ) ) ;
#45906 = CARTESIAN_POINT ( 'NONE',  ( 1.024188300031657617, 0.9657954515097492143, 1.716266578800438536 ) ) ;
#45907 = CARTESIAN_POINT ( 'NONE',  ( 4.919437264989244163, 6.867374270256937585, 1.424029350978267550 ) ) ;
#45908 = CARTESIAN_POINT ( 'NONE',  ( 5.517805331081858888, 5.539787095791365523, 1.040834085586084257E-14 ) ) ;
#45910 = DIRECTION ( 'NONE',  ( 3.347138415753903010E-16, 0.6000000000000018652, -0.7999999999999984901 ) ) ;
#45909 = CARTESIAN_POINT ( 'NONE',  ( 0.000000000000000000, -2.187499999999998668, -4.012584370867899430 ) ) ;
#45911 = CARTESIAN_POINT ( 'NONE',  ( 2.853816628688166990, 2.281129249179119078, -0.2256723309681916978 ) ) ;
#45912 = CARTESIAN_POINT ( 'NONE',  ( 1.189776066567624691, -0.8228614858879386151, 1.629801898503015156 ) ) ;
#45913 = CARTESIAN_POINT ( 'NONE',  ( 3.586107075002854305, 1.066394011600999780, 1.587261316105821551 ) ) ;
#45914 = CARTESIAN_POINT ( 'NONE',  ( 5.169401708560450004, 9.252995436621013425, 0.000000000000000000 ) ) ;
#45915 = CARTESIAN_POINT ( 'NONE',  ( 6.575341312503417690, 10.61505593132193326, -0.7216878364870267237 ) ) ;
#45916 = CARTESIAN_POINT ( 'NONE',  ( -9.494787648271923786, 9.971673765939062406, 1.040834085586084257E-14 ) ) ;
#45917 = CARTESIAN_POINT ( 'NONE',  ( 2.302991897352596684, -0.3483681713834784199, -1.982697776695659053 ) ) ;
#45918 = CARTESIAN_POINT ( 'NONE',  ( 1.621847549879053885, 1.933622029546874010, -0.3300716771732490895 ) ) ;
#45919 = CARTESIAN_POINT ( 'NONE',  ( -7.648771216403934758, 12.07531685244661723, -0.7998128361456291469 ) ) ;
#45920 = CARTESIAN_POINT ( 'NONE',  ( -7.389357414647957256, 8.579670724299436557, 1.199719254218450271 ) ) ;
#45921 = CARTESIAN_POINT ( 'NONE',  ( -11.41381675112460847, 10.06983264508524201, -3.704697986577268232 ) ) ;
#45923 = CARTESIAN_POINT ( 'NONE',  ( 3.854177328971124084, 0.6370089842938561064, 1.651420920916975232 ) ) ;
#45922 = CARTESIAN_POINT ( 'NONE',  ( 5.068349447220681370, -1.968310418947304408, -0.7050240649949056637 ) ) ;
#45924 = CARTESIAN_POINT ( 'NONE',  ( -8.752560967070127873, 15.99999998464634388, 9.356054886183752473 ) ) ;
#45926 = CARTESIAN_POINT ( 'NONE',  ( 0.07648947921621782053, -2.126777779243053779, -0.5280787695999613618 ) ) ;
#45925 =( LENGTH_UNIT ( ) NAMED_UNIT ( * ) SI_UNIT ( .MILLI., .METRE. ) );
#45927 = CARTESIAN_POINT ( 'NONE',  ( 4.892389968643020559, 1.444305832375993637, -0.9706037289107912747 ) ) ;
#45928 = CARTESIAN_POINT ( 'NONE',  ( 8.052653171512838881, 11.48218023581863001, -1.199719254218446718 ) ) ;
#45929 = CARTESIAN_POINT ( 'NONE',  ( 0.7499999999999902300, 4.066666666666690411, -1.299038105676658228 ) ) ;
#45930 = CARTESIAN_POINT ( 'NONE',  ( 4.551880008920849541, 1.548817843433186736, -0.7794160303473545159 ) ) ;
#45931 = B_SPLINE_CURVE_WITH_KNOTS ( 'NONE', 3,
 ( #162240, #30099, #45297, #79900, #78831, #32229, #212019, #97248, #61529, #131902, #196856, #147067 ),
 .UNSPECIFIED., .F., .F.,
 ( 4, 2, 2, 2, 2, 4 ),
 ( 0.000000000000000000, 0.0007281235154085147036, 0.001456247030817029407, 0.001820308788521285892, 0.002184370546225541942, 0.002912494061634051876 ),
 .UNSPECIFIED. ) ;
#45932 = CARTESIAN_POINT ( 'NONE',  ( 4.545498338918555703, 1.941281163200560878, -0.9724488383844475115 ) ) ;
#45933 = CARTESIAN_POINT ( 'NONE',  ( 3.979481780810941949, 4.601482484822914998, 1.199719254218464037 ) ) ;
#45934 = CARTESIAN_POINT ( 'NONE',  ( 6.157435431667657610, 1.928259211291092123, -0.5899821858514133766 ) ) ;
#45935 = CARTESIAN_POINT ( 'NONE',  ( 4.937500000000003553, 1.451031289060916496, -1.451031289061313512 ) ) ;
#45936 = CARTESIAN_POINT ( 'NONE',  ( 0.7499999999999920064, 5.514583334016151639, 1.299038105676669330 ) ) ;
#45937 = CARTESIAN_POINT ( 'NONE',  ( 2.784106279807782247, -0.9919383200396988398, 1.651252367177785230 ) ) ;
#45938 = CARTESIAN_POINT ( 'NONE',  ( 1.499999999999997113, 9.427083334016129967, -0.8660254037844378194 ) ) ;
#45939 = CARTESIAN_POINT ( 'NONE',  ( 6.363560548480147183, -1.783403785914154049, -1.324293268510617017 ) ) ;
#45940 = ORIENTED_EDGE ( 'NONE', *, *, #90754, .F. ) ;
#45941 = CARTESIAN_POINT ( 'NONE',  ( 6.883263157960402445, 0.001763689368145578400, 1.846037217754380011 ) ) ;
#45942 = CARTESIAN_POINT ( 'NONE',  ( -1.402160292154681736E-14, 2.587500000000023892, -1.732050807568863648 ) ) ;
#45943 = CARTESIAN_POINT ( 'NONE',  ( 6.796715079152391148, 6.823922435299587974, 0.7998128361456341429 ) ) ;
#45944 = CARTESIAN_POINT ( 'NONE',  ( 2.965722808067718486, -1.817245444403335020, -1.277177951966218084 ) ) ;
#45945 = CARTESIAN_POINT ( 'NONE',  ( 6.155038550924133212, 10.12470270947942730, 0.7216878364870438212 ) ) ;
#45946 = CARTESIAN_POINT ( 'NONE',  ( -10.45297324601190425, 11.29748299654313470, 0.7216878364870438212 ) ) ;
#45947 = CARTESIAN_POINT ( 'NONE',  ( 4.577813143269636065, 5.369812084349879555, -1.199719254218450271 ) ) ;
#45948 = CARTESIAN_POINT ( 'NONE',  ( 0.2115648487451895210, 1.930418618556551946, 0.5826528611774861588 ) ) ;
#45950 = CARTESIAN_POINT ( 'NONE',  ( 5.687952575977194947, -1.305682642493616541, -1.596842856974973301 ) ) ;
#45949 = CARTESIAN_POINT ( 'NONE',  ( 7.404724451357931336, 11.79059562655963056, 0.7998128361456462443 ) ) ;
#45951 = CARTESIAN_POINT ( 'NONE',  ( 3.566600549852601887, 6.224440002135039229, 1.211718802956414764 ) ) ;
#45952 = CARTESIAN_POINT ( 'NONE',  ( -4.090809663021341969, 5.795697244990093644, 1.599625672291267398 ) ) ;
#45953 = CARTESIAN_POINT ( 'NONE',  ( 1.499999999999991118, 5.285416667349480235, 0.8660254037844524744 ) ) ;
#45954 = CARTESIAN_POINT ( 'NONE',  ( 1.364683531249988757, 1.384375000341421469, 0.000000000000000000 ) ) ;
#45955 = CARTESIAN_POINT ( 'NONE',  ( 6.749288224047839790, -1.502610544577225982, -1.113804566994440970 ) ) ;
#45956 = CARTESIAN_POINT ( 'NONE',  ( 6.117740286212093537, 0.1793736470585994280, 1.724862758254825712 ) ) ;
#45957 = CARTESIAN_POINT ( 'NONE',  ( 5.126372767375061201, 0.1352161506754517850, 1.735264446013358608 ) ) ;
#45958 = CARTESIAN_POINT ( 'NONE',  ( 3.245926457026059531, 2.292545471606484142, -0.001860936589836299044 ) ) ;
#45959 = CARTESIAN_POINT ( 'NONE',  ( 0.6823417656249882723, -0.9072916663252494907, 1.181850606188755259 ) ) ;
#45960 = CARTESIAN_POINT ( 'NONE',  ( 1.112948326906910035, -1.796673262952220629, 0.4014371099074555693 ) ) ;
#45961 = EDGE_CURVE ( 'NONE', #150994, #55454, #149816, .T. ) ;
#45962 = CARTESIAN_POINT ( 'NONE',  ( 9.642873567817520808, 12.27310513391906532, 1.599625672291279388 ) ) ;
#45963 =( NAMED_UNIT ( * ) PLANE_ANGLE_UNIT ( ) SI_UNIT ( $, .RADIAN. ) );
#45964 = CARTESIAN_POINT ( 'NONE',  ( 1.623764174509664260, -1.011042645414115260, -1.519837739365454743 ) ) ;
#45965 = CARTESIAN_POINT ( 'NONE',  ( 2.461564753630896440, -1.930417925741171103, -0.5826551686555282439 ) ) ;
#45966 = CARTESIAN_POINT ( 'NONE',  ( 1.183813618819636870, -0.9825931803647185436, 1.958887836816553429 ) ) ;
#45967 = CARTESIAN_POINT ( 'NONE',  ( 9.223659970357786619, 13.86322243015305844, -6.886736302288140266 ) ) ;
#45968 = CARTESIAN_POINT ( 'NONE',  ( 4.735441112814092079, -1.926550399551892001, 0.8509862954892956077 ) ) ;
#45969 = CARTESIAN_POINT ( 'NONE',  ( -5.689618019229208734, 9.789638122409414223, 0.7998128361456481317 ) ) ;
#45970 = CARTESIAN_POINT ( 'NONE',  ( 8.724987196144599721, 13.71643412956232311, 7.773938044818101467 ) ) ;
#45971 = CARTESIAN_POINT ( 'NONE',  ( 1.100149375694438714, 0.8407228983892693908, -1.892171374333020406 ) ) ;
#45972 = CARTESIAN_POINT ( 'NONE',  ( 4.385172619016207918, 7.203452924572514959, 1.199719254218462483 ) ) ;
#45973 = CARTESIAN_POINT ( 'NONE',  ( 0.6801582343749796866, -0.9114583329919088150, -1.178068619123886718 ) ) ;
#45974 = CARTESIAN_POINT ( 'NONE',  ( 5.145234815219777325, 0.1564148900096741512, 2.114790009947895122 ) ) ;
#45975 = CARTESIAN_POINT ( 'NONE',  ( 0.1527873662319845505, -1.548267161427993255, 1.146224303156289093 ) ) ;
#45976 = EDGE_LOOP ( 'NONE', ( #134278, #10291, #26384, #153107 ) ) ;
#45977 = CARTESIAN_POINT ( 'NONE',  ( -4.793689830883590020, 7.750332681742931662, 1.199719254218452935 ) ) ;
#45978 = CARTESIAN_POINT ( 'NONE',  ( -11.48243876534946040, 11.29999999999999893, -3.200000000000001510 ) ) ;
#45979 = CARTESIAN_POINT ( 'NONE',  ( 7.010974831598141499, 7.352094523052197239, -0.7216878364870317197 ) ) ;
#45980 = CARTESIAN_POINT ( 'NONE',  ( -3.475000000000000533, -2.056249999044083232, 0.000000000000000000 ) ) ;
#45981 = CARTESIAN_POINT ( 'NONE',  ( -5.148345644887285744, 7.029489223833707001, -1.599625672291256295 ) ) ;
#45982 = CARTESIAN_POINT ( 'NONE',  ( -0.1224090711158704881, -1.988194106603015987, -0.9910323345065151779 ) ) ;
#45983 = CARTESIAN_POINT ( 'NONE',  ( 1.096861832941862236, -0.5116358106188825250, -2.042740603722263515 ) ) ;
#45984 = CARTESIAN_POINT ( 'NONE',  ( -4.736594563127865420, 6.619389305106191834, -1.599625672291271394 ) ) ;
#45985 = CARTESIAN_POINT ( 'NONE',  ( 7.228468454380276853, 11.58496363008569574, 1.040834085586084257E-14 ) ) ;
#45986 = CARTESIAN_POINT ( 'NONE',  ( 5.594539833219323022, 1.833072992967394788, 0.3199324213378691439 ) ) ;
#45987 = CARTESIAN_POINT ( 'NONE',  ( 8.751951852821344247, 10.16936423550178503, -1.199719254218446718 ) ) ;
#45988 = EDGE_CURVE ( 'NONE', #73877, #21505, #153508, .T. ) ;
#45989 = CARTESIAN_POINT ( 'NONE',  ( 10.91944002402979130, -8.407420853759269619, -0.1105873483556608222 ) ) ;
#45990 = CARTESIAN_POINT ( 'NONE',  ( -4.821859908315634158, 5.654533310236863564, 1.199719254218452935 ) ) ;
#45991 = CARTESIAN_POINT ( 'NONE',  ( -10.14113571334194930, 10.93367254176152059, -0.7216878364870267237 ) ) ;
#45992 = AXIS2_PLACEMENT_3D ( 'NONE', #166851, #18447, #136493 ) ;
#45994 = CARTESIAN_POINT ( 'NONE',  ( 2.101936620064443151, 0.7537240185569763495, -1.811501260397870405 ) ) ;
#45993 = CARTESIAN_POINT ( 'NONE',  ( -8.030507057996002729, 8.263346410617135263, 1.040834085586084257E-14 ) ) ;
#45995 = CARTESIAN_POINT ( 'NONE',  ( 1.393688021309073433, 1.637156065531343740, 1.411701162175371893 ) ) ;
#45996 = AXIS2_PLACEMENT_3D ( 'NONE', #1519, #82797, #197608 ) ;
#45998 = CARTESIAN_POINT ( 'NONE',  ( -6.136354103119505687, 5.996982182489118962, -0.08184359936842452998 ) ) ;
#45997 = CARTESIAN_POINT ( 'NONE',  ( -5.743814354044916470, 6.730146830254374990, -1.199719254218453823 ) ) ;
#45999 = CARTESIAN_POINT ( 'NONE',  ( -1.364683531250014514, -0.2197916663252438285, 0.7879004041258379498 ) ) ;
#46000 = CARTESIAN_POINT ( 'NONE',  ( 2.565452462605917638, 1.394811117528846900, -1.029664540377094761 ) ) ;
#46001 = CARTESIAN_POINT ( 'NONE',  ( 2.782837888936703585, 1.230821076073612463, 1.230640916823136255 ) ) ;
#46002 = CARTESIAN_POINT ( 'NONE',  ( 5.829642864196151741, 9.745074408296771296, 0.7216878364870438212 ) ) ;
#46003 = CARTESIAN_POINT ( 'NONE',  ( -12.93621305287376089, 7.735084883283615653, -1.079074430401041118 ) ) ;
#46004 = CARTESIAN_POINT ( 'NONE',  ( 0.7728142736522191081, -2.006652962095498260, 0.1948079406639269262 ) ) ;
#46005 = CARTESIAN_POINT ( 'NONE',  ( 6.925078400183578786, 0.5640289027524867382, 2.196098379985710114 ) ) ;
#46006 = CARTESIAN_POINT ( 'NONE',  ( -5.795184315198522285, 5.725746220678519904, -0.7998128361456362523 ) ) ;
#46007 = CARTESIAN_POINT ( 'NONE',  ( 1.481257693138532616, 1.822349276556498143, -0.7526048170787935643 ) ) ;
#46010 = ADVANCED_FACE ( 'NONE', ( #147053 ), #145995, .F. ) ;
#46009 = CARTESIAN_POINT ( 'NONE',  ( -6.468648687495877958, 6.719380688266201496, 0.000000000000000000 ) ) ;
#46008 = CARTESIAN_POINT ( 'NONE',  ( 5.660397963661894849, 1.910509065610028090, 0.08734628876111423523 ) ) ;
#46011 = CARTESIAN_POINT ( 'NONE',  ( -7.092323753280154186, 7.447001598347859463, 0.7216878364870317197 ) ) ;
#46012 = CARTESIAN_POINT ( 'NONE',  ( 6.176621499477501054, 9.363752961769195693, -1.199719254218452047 ) ) ;
#46013 = CARTESIAN_POINT ( 'NONE',  ( -5.284646014276622950, 9.387447126623207794, -0.7998128361456362523 ) ) ;
#46014 = CARTESIAN_POINT ( 'NONE',  ( 1.084635305120797089, -1.279634344436600513, 1.562581769784775920 ) ) ;
#46015 = CARTESIAN_POINT ( 'NONE',  ( 5.165293336682155179, 5.128523102325101668, -0.7216878364870420448 ) ) ;
#46016 = EDGE_CURVE ( 'NONE', #40283, #202706, #213821, .T. ) ;
#46017 = CARTESIAN_POINT ( 'NONE',  ( 4.559805550777903171, 0.5102292677348593264, -2.250327227043275702 ) ) ;
#46018 = CARTESIAN_POINT ( 'NONE',  ( 5.846142468697441252, -0.8834969228576605715, 1.751761657833034613 ) ) ;
#46019 = CARTESIAN_POINT ( 'NONE',  ( 1.973419848571813073, -0.2453196125269933581, 1.946320556625024345 ) ) ;
#46020 = CARTESIAN_POINT ( 'NONE',  ( 10.57266086055835075, 11.22919251360659310, 0.000000000000000000 ) ) ;
#46021 = DIRECTION ( 'NONE',  ( -3.330669073875479482E-16, 3.330669073875479482E-16, 1.000000000000000000 ) ) ;
#46022 = ORIENTED_EDGE ( 'NONE', *, *, #173466, .T. ) ;
#46023 = CARTESIAN_POINT ( 'NONE',  ( 1.622414240495053672, 2.095119945234637182, 0.3050691438145485268 ) ) ;
#46025 = CARTESIAN_POINT ( 'NONE',  ( -8.857554428429624593, 9.228235009456373206, 0.7998128361456462443 ) ) ;
#46024 = CARTESIAN_POINT ( 'NONE',  ( -4.273844736805832767, 6.009238164405336313, 1.599625672291267398 ) ) ;
#46026 = CARTESIAN_POINT ( 'NONE',  ( 1.200829095903386046, -0.4490931065196464012, 1.785404219219708377 ) ) ;
#46027 = ORIENTED_EDGE ( 'NONE', *, *, #138422, .F. ) ;
#46028 = CARTESIAN_POINT ( 'NONE',  ( 11.63116522980375578, 8.263862536643911127, 2.980981896763163608 ) ) ;
#46029 = CARTESIAN_POINT ( 'NONE',  ( 3.410498715577559015, -2.118327196165440185, -0.1003008382433126094 ) ) ;
#46030 = CARTESIAN_POINT ( 'NONE',  ( 0.7499999999999902300, 3.764583334016149863, 1.299038105676669330 ) ) ;
#46031 = CARTESIAN_POINT ( 'NONE',  ( 8.402302512167096893, 10.82577223566020841, -1.599625672291268286 ) ) ;
#46032 = CARTESIAN_POINT ( 'NONE',  ( 3.216142984300340846, -1.012526663717785214, -1.794778392713367587 ) ) ;
#46033 = CIRCLE ( 'NONE', #32238, 4.500000000000000000 ) ;
#46035 = CARTESIAN_POINT ( 'NONE',  ( 0.2331563151865487238, 7.629137130509101361, -2.545728013813946866 ) ) ;
#46034 = CARTESIAN_POINT ( 'NONE',  ( -7.004758919754800139, 11.32396917302262018, 0.000000000000000000 ) ) ;
#46036 = CARTESIAN_POINT ( 'NONE',  ( -1.364683531250012516, 3.238541667008084879, -0.7879004041258289570 ) ) ;
#46037 = CARTESIAN_POINT ( 'NONE',  ( 0.000000000000000000, -4.517653975874099892, 0.000000000000000000 ) ) ;
#46038 = CARTESIAN_POINT ( 'NONE',  ( 1.265299903344048627, 3.779048306927172529, 0.4993168358707211207 ) ) ;
#46039 = CARTESIAN_POINT ( 'NONE',  ( 0.1709339574563934483, -1.438030690398562239, 1.674123062825278563 ) ) ;
#46040 = CARTESIAN_POINT ( 'NONE',  ( 2.970297248839429027, 1.207737455218102829, 1.912895951805194894 ) ) ;
#46041 = CARTESIAN_POINT ( 'NONE',  ( -8.920901888112002354, 11.43080484092926241, 1.443375672974064550 ) ) ;
#46042 = CARTESIAN_POINT ( 'NONE',  ( 2.091809026493749890, 1.116998374171035424, 1.426102431979922702 ) ) ;
#46043 = CARTESIAN_POINT ( 'NONE',  ( 2.114329361022151854, 1.859220375642420819, 0.4613663794279678765 ) ) ;
#46044 = CARTESIAN_POINT ( 'NONE',  ( 2.629418614236479712, 0.1040367438073786233, -2.067886086930009970 ) ) ;
#46045 = CARTESIAN_POINT ( 'NONE',  ( -1.364683531249997417, 3.071875000341423245, 1.214306433183764966E-14 ) ) ;
#46046 = CARTESIAN_POINT ( 'NONE',  ( 1.973447535326333879, 1.887181058671667966, -0.5703184155462033278 ) ) ;
#46047 = CARTESIAN_POINT ( 'NONE',  ( 6.182248986134903035, -1.028413017182037370, 1.628868941788450764 ) ) ;
#46048 = CARTESIAN_POINT ( 'NONE',  ( 2.518242125168220102, 1.223528130051700025, -1.415109699333151561 ) ) ;
#46050 = CARTESIAN_POINT ( 'NONE',  ( 4.890561790263044273, 8.149264200713410844, -1.004099907704804950 ) ) ;
#46049 = CARTESIAN_POINT ( 'NONE',  ( 0.8741376776274005778, 2.222666731570396959, -0.6204599517294244748 ) ) ;
#46051 = CARTESIAN_POINT ( 'NONE',  ( 3.121387120179277996, 0.2756568158089545695, -1.840403582779404745 ) ) ;
#46052 = CARTESIAN_POINT ( 'NONE',  ( 1.364683531249988535, 3.155208333674756283, -0.7879004041258239610 ) ) ;
#46053 = CARTESIAN_POINT ( 'NONE',  ( 5.898899852458296955, 0.3987951208904988443, 2.023601990196000955 ) ) ;
#46054 = VECTOR ( 'NONE', #169829, 1000.000000000000000 ) ;
#46055 = CARTESIAN_POINT ( 'NONE',  ( -3.913499895838973508, 7.717500311787445000, 1.040834085586084257E-14 ) ) ;
#46056 = CARTESIAN_POINT ( 'NONE',  ( -1.430889623655251075, 3.675352821211156140, -0.4691377289697510888 ) ) ;
#46057 = CARTESIAN_POINT ( 'NONE',  ( 6.545935606868724221, 0.8096169477174266493, -1.944322875993751421 ) ) ;
#46058 = CARTESIAN_POINT ( 'NONE',  ( -1.201851678989727383E-14, 3.634375000341422357, 1.575800808251672791 ) ) ;
#46059 = CARTESIAN_POINT ( 'NONE',  ( 6.081358973892866615, 1.999796440023202670, -0.8210498935554910727 ) ) ;
#46060 = CARTESIAN_POINT ( 'NONE',  ( 6.147130067458792091, 0.1999419896685956377, 2.009763438563259008 ) ) ;
#46061 = CARTESIAN_POINT ( 'NONE',  ( -1.402160292154681736E-14, -0.3031249996585801965, -1.575800808251665908 ) ) ;
#46062 = CARTESIAN_POINT ( 'NONE',  ( -4.446711195602245148, 7.171284913969171448, -1.082531754730549967 ) ) ;
#46063 = VECTOR ( 'NONE', #34706, 1000.000000000000000 ) ;
#46066 = CARTESIAN_POINT ( 'NONE',  ( 3.362058906508953449, 6.866226457661676719, -0.7216878364870267237 ) ) ;
#46065 = CARTESIAN_POINT ( 'NONE',  ( 6.825078400183548055, 2.461594334264828987, 2.239602747093616841 ) ) ;
#46064 = CARTESIAN_POINT ( 'NONE',  ( 6.333594036239346359, 7.418223126147930557, 1.199719254218453823 ) ) ;
#46067 = CARTESIAN_POINT ( 'NONE',  ( -4.468294144155606773, 7.370704380560280100, 1.199719254218452935 ) ) ;
#46068 = CARTESIAN_POINT ( 'NONE',  ( 5.032435514249763209, 0.5899841883351600869, 1.928258608204669766 ) ) ;
#46069 = CARTESIAN_POINT ( 'NONE',  ( -7.690499447449645309, 9.995335326823163058, 1.599625672291295375 ) ) ;
#46071 = CARTESIAN_POINT ( 'NONE',  ( -6.794044373779495771, 8.059378203231773341, 1.082531754730549078 ) ) ;
#46070 = CARTESIAN_POINT ( 'NONE',  ( -8.351459436338030784, 11.72682452816096976, -1.082531754730543971 ) ) ;
#46072 = CARTESIAN_POINT ( 'NONE',  ( 0.6823417656249917140, 4.592708333674755394, 1.181850606188765695 ) ) ;
#46074 = CARTESIAN_POINT ( 'NONE',  ( -0.6823417656250039265, 9.817708333674735499, -1.181850606188755259 ) ) ;
#46073 = CARTESIAN_POINT ( 'NONE',  ( 5.717692609583751029, -2.109997883074541392, 0.4692839721026839661 ) ) ;
#46075 = CARTESIAN_POINT ( 'NONE',  ( 1.499999999999990896, 6.344000000000043826, 2.958666666666670331 ) ) ;
#46076 = CARTESIAN_POINT ( 'NONE',  ( -11.45643882766868593, 6.922515100558133128, 3.422322265972647326 ) ) ;
#46078 = CARTESIAN_POINT ( 'NONE',  ( 6.433220217788329087, -1.621194592471734364, -1.198847091081943539 ) ) ;
#46077 = CARTESIAN_POINT ( 'NONE',  ( -6.575341312503472757, 7.733948288417905381, 1.082531754730549967 ) ) ;
#46079 = CARTESIAN_POINT ( 'NONE',  ( -0.6823417656250003738, 0.03020833367475134201, -1.181850606188749264 ) ) ;
#46080 = CONICAL_SURFACE ( 'NONE', #111848, 2.324999999999998845, 0.7853981633974461696 ) ;
#46081 = CARTESIAN_POINT ( 'NONE',  ( 6.539320575229256249, 7.052319431262985105, 2.701414634427783845 ) ) ;
#46082 = CARTESIAN_POINT ( 'NONE',  ( 1.488428555967473921, -0.2500744359604460954, -1.706524604440103898 ) ) ;
#46083 = CARTESIAN_POINT ( 'NONE',  ( 4.435452530326143616, 5.203724702582467998, -1.199719254218452047 ) ) ;
#46084 = CARTESIAN_POINT ( 'NONE',  ( 7.042534447655770080, 7.180988041878682004, -0.7998128361456341429 ) ) ;
#46085 = CARTESIAN_POINT ( 'NONE',  ( -11.99998434469187991, 9.022909391445272931, -0.6142738339537157088 ) ) ;
#46086 = CARTESIAN_POINT ( 'NONE',  ( 6.098880659294531270, 1.529360415809786433, -1.076766019972655197 ) ) ;
#46087 =( BOUNDED_CURVE ( )  B_SPLINE_CURVE ( 2, ( #23933, #168073, #19673, #43423, #126873, #60709, #42361 ),
 .UNSPECIFIED., .F., .T. ) 
 B_SPLINE_CURVE_WITH_KNOTS ( ( 3, 2, 2, 3 ),
 ( 0.000000000000000000, 0.005952380952380876590, 0.01190476190476175318, 0.01785714285714263064 ),
 .UNSPECIFIED. ) 
 CURVE ( )  GEOMETRIC_REPRESENTATION_ITEM ( )  RATIONAL_B_SPLINE_CURVE ( ( 1.000000000000000000, 0.8660254037844387076, 1.000000000000000000, 0.8660254037844387076, 1.000000000000000000, 0.8660254037844438146, 0.9999999999999948930 ) ) 
 REPRESENTATION_ITEM ( '' )  );
#46088 = CARTESIAN_POINT ( 'NONE',  ( 0.5045416345675997061, -1.998124945550180609, -0.2444111669489754113 ) ) ;
#46089 = CARTESIAN_POINT ( 'NONE',  ( -0.3782569160207248093, 3.049340702855435570, -0.4285286083246230282 ) ) ;
#46090 = CARTESIAN_POINT ( 'NONE',  ( 2.358755538653318773, 5.695705861830088423, 1.040834085586084257E-14 ) ) ;
#46091 = CARTESIAN_POINT ( 'NONE',  ( 2.854729849855553780, 0.7423848465729752100, 2.078289375090878632 ) ) ;
#46092 = CARTESIAN_POINT ( 'NONE',  ( 4.926734997883643885, -1.423062915019442043, 1.639699324398981251 ) ) ;
#46093 = EDGE_LOOP ( 'NONE', ( #151490, #193020 ) ) ;
#46094 = CARTESIAN_POINT ( 'NONE',  ( -1.500000000000015099, -1.079166666666641961, 0.8660254037844403729 ) ) ;
#46095 = CARTESIAN_POINT ( 'NONE',  ( 8.215877899756996783, 12.52901528311778989, 1.040834085586084257E-14 ) ) ;
#46097 = CARTESIAN_POINT ( 'NONE',  ( 2.530875249677287719, -1.674875632724934338, 1.122518345125958383 ) ) ;
#46096 = CARTESIAN_POINT ( 'NONE',  ( 2.737105750116640923, 1.997451989420237606, 0.7121958652205606644 ) ) ;
#46099 = ORIENTED_EDGE ( 'NONE', *, *, #189724, .T. ) ;
#46098 = CARTESIAN_POINT ( 'NONE',  ( 1.951130291612662715, -1.617002164660426677, 0.8169817665307582688 ) ) ;
#46100 = CARTESIAN_POINT ( 'NONE',  ( 5.254667053748194760, 8.288139441751686931, 1.199719254218452047 ) ) ;
#46101 = EDGE_LOOP ( 'NONE', ( #28500, #204462, #196158, #179455 ) ) ;
#46102 = CARTESIAN_POINT ( 'NONE',  ( 0.4263524580605422276, 1.788790299270696993, 0.5473224044415525569 ) ) ;
#46103 = CARTESIAN_POINT ( 'NONE',  ( 7.135668919494039031, 7.219368582364847242, 1.040834085586084257E-14 ) ) ;
#46105 = CARTESIAN_POINT ( 'NONE',  ( 1.885809660653874120, -1.915224419731532901, 0.05109022710406836698 ) ) ;
#46104 = CARTESIAN_POINT ( 'NONE',  ( -5.603597561149804562, 5.431951997629870910, 0.7998128361456341429 ) ) ;
#46106 =( NAMED_UNIT ( * ) PLANE_ANGLE_UNIT ( ) SI_UNIT ( $, .RADIAN. ) );
#46107 = DIRECTION ( 'NONE',  ( 1.000000000000000000, 0.000000000000000000, -1.224646799147353207E-16 ) ) ;
#46108 = CARTESIAN_POINT ( 'NONE',  ( -1.364683531250014514, 0.5510416670080878765, -0.7879004041258289570 ) ) ;
#46109 = CARTESIAN_POINT ( 'NONE',  ( 6.115103934187892776, 6.015625209457229339, 1.345820777640227805E-10 ) ) ;
#46110 = CARTESIAN_POINT ( 'NONE',  ( -8.272446282632566650, 12.80293776304669962, 0.7998128361456481317 ) ) ;
#46111 = CARTESIAN_POINT ( 'NONE',  ( 5.225516498768126183, -2.053876642077703707, 0.6744380372525200507 ) ) ;
#46112 = CARTESIAN_POINT ( 'NONE',  ( -4.312902262922974295, 8.045820050136510915, 0.7216878364870338292 ) ) ;
#46113 = CARTESIAN_POINT ( 'NONE',  ( -6.749980374757255319, 8.968339418673846097, 1.599625672291269396 ) ) ;
#46114 = CARTESIAN_POINT ( 'NONE',  ( 3.111701630267147856, 1.674174984267240429, 1.301503359413098249 ) ) ;
#46115 = EDGE_CURVE ( 'NONE', #177149, #205543, #189550, .T. ) ;
#46117 = CARTESIAN_POINT ( 'NONE',  ( -11.83624332731381124, 4.942650230196960592, 4.855242260347336192 ) ) ;
#46116 = CARTESIAN_POINT ( 'NONE',  ( 1.499999999999990896, 5.775000000000023448, 1.040834085586084257E-14 ) ) ;
#46118 = CARTESIAN_POINT ( 'NONE',  ( 4.464113681242611875, 0.9267091202830781693, 1.739933209567791073 ) ) ;
#46119 = CARTESIAN_POINT ( 'NONE',  ( 5.379139070037473935, -1.731557697741787916, -0.8120211572784155063 ) ) ;
#46120 = ORIENTED_EDGE ( 'NONE', *, *, #185379, .F. ) ;
#46121 = CARTESIAN_POINT ( 'NONE',  ( 1.452583904633400591, -1.374772708486727391, 1.500000000000001332 ) ) ;
#46122 = CARTESIAN_POINT ( 'NONE',  ( 0.3091450132529197647, -1.663722454078466306, 1.232067777400827069 ) ) ;
#46123 = CARTESIAN_POINT ( 'NONE',  ( 2.835803868134049388, 1.927321602952759338, 0.2373744266383533696 ) ) ;
#46124 = ORIENTED_EDGE ( 'NONE', *, *, #45047, .T. ) ;
#46125 = DIRECTION ( 'NONE',  ( 0.7592566023653005702, 0.6507913734559639396, 0.000000000000000000 ) ) ;
#46126 = CARTESIAN_POINT ( 'NONE',  ( 7.147083253059300922, 8.367293879104554577, 1.199719254218452935 ) ) ;
#46128 = CARTESIAN_POINT ( 'NONE',  ( 6.494519276145969577, 7.535692896047149425, -1.199719254218446718 ) ) ;
#46127 = CARTESIAN_POINT ( 'NONE',  ( 2.396528757545500099, 1.678484640409601436, -1.246154833996036437 ) ) ;
#46129 = CARTESIAN_POINT ( 'NONE',  ( 3.892599500454941630, 6.595097612955829192, 1.082531754730549078 ) ) ;
#46131 = VERTEX_POINT ( 'NONE', #112464 ) ;
#46130 = CARTESIAN_POINT ( 'NONE',  ( 0.2580964568148482741, 1.806467626183925423, 0.1351022710447576103 ) ) ;
#46132 = CARTESIAN_POINT ( 'NONE',  ( 4.055453297694236348, -1.834216022232620702, -1.226887332174102951 ) ) ;
#46133 = EDGE_CURVE ( 'NONE', #141673, #157888, #113535, .T. ) ;
#46134 = CARTESIAN_POINT ( 'NONE',  ( 3.346891443098894303, 0.5343612633194516626, 2.140983517310310891 ) ) ;
#46135 = CARTESIAN_POINT ( 'NONE',  ( 6.598014311344812199, 10.84943379654430906, 1.040834085586084257E-14 ) ) ;
#46136 = CARTESIAN_POINT ( 'NONE',  ( 1.499999999999991118, 8.673756432004008587, 2.614717076620604264 ) ) ;
#46137 = CARTESIAN_POINT ( 'NONE',  ( 1.945825403448407487, -1.250168254263404277, -1.447093241409423081 ) ) ;
#46138 = AXIS2_PLACEMENT_3D ( 'NONE', #29682, #182301, #114197 ) ;
#46139 = CARTESIAN_POINT ( 'NONE',  ( 9.049177462117294013, 12.64479190819049670, -1.199719254218446718 ) ) ;
#46140 = CARTESIAN_POINT ( 'NONE',  ( 4.158688916442684125, -0.6465363538536234023, -1.966910096795893903 ) ) ;
#46141 = AXIS2_PLACEMENT_3D ( 'NONE', #9860, #211250, #158271 ) ;
#46143 = CARTESIAN_POINT ( 'NONE',  ( 3.344745324850742385, 0.5235245934552492653, 2.097234944377385002 ) ) ;
#46142 = CARTESIAN_POINT ( 'NONE',  ( 0.1888596022590748325, -6.708723052947950904, 10.87247189006428272 ) ) ;
#46144 = CARTESIAN_POINT ( 'NONE',  ( 5.056268342064010213, -1.587557771011731678, 1.511049258477934032 ) ) ;
#46145 = DIRECTION ( 'NONE',  ( 0.6483454320283799088, 0.000000000000000000, -0.7613463080411786432 ) ) ;
#46146 = ADVANCED_FACE ( 'NONE', ( #210945 ), #55564, .T. ) ;
#46147 = DIRECTION ( 'NONE',  ( -0.000000000000000000, 1.000000000000000000, -0.000000000000000000 ) ) ;
#46148 = CARTESIAN_POINT ( 'NONE',  ( -1.797316061902485052, 15.44822828525704850, 11.85333567385661446 ) ) ;
#46149 = CARTESIAN_POINT ( 'NONE',  ( 4.929271367020211514, 7.908511140569038922, 1.199719254218452047 ) ) ;
#46150 = CARTESIAN_POINT ( 'NONE',  ( 1.364683531249997417, 15.29687500034139447, 2.602085213965210642E-15 ) ) ;
#46151 = CARTESIAN_POINT ( 'NONE',  ( -3.169574050544739841, 6.919863168935977527, -0.7998128361456481317 ) ) ;
#46152 = EDGE_CURVE ( 'NONE', #180119, #125532, #139334, .T. ) ;
#46153 = CARTESIAN_POINT ( 'NONE',  ( 0.05336153386781630759, -1.314994204386025434, 1.528742563917218078 ) ) ;
#46154 = CARTESIAN_POINT ( 'NONE',  ( -7.375272376154077492, 11.54830883891436422, -0.7216878364870267237 ) ) ;
#46155 = CARTESIAN_POINT ( 'NONE',  ( 4.346580092118113470, -2.046995731385771400, -0.3088174131898810959 ) ) ;
#46156 = CARTESIAN_POINT ( 'NONE',  ( 3.738824155997504395, 0.2837420414000761393, 1.905379044178076686 ) ) ;
#46157 = CARTESIAN_POINT ( 'NONE',  ( 5.624650681053017465, 0.4137061758265787592, 2.076257688556768066 ) ) ;
#46158 = CARTESIAN_POINT ( 'NONE',  ( 5.931855901178834323, 6.879252291918818152, 1.199719254218462483 ) ) ;
#46159 = CARTESIAN_POINT ( 'NONE',  ( 9.574755896318485782, 4.231292707087955129, 7.158835548396386805 ) ) ;
#46160 = CARTESIAN_POINT ( 'NONE',  ( 3.467590214127397541, -0.3886977184213887271, 1.930520482988388631 ) ) ;
#46161 = CARTESIAN_POINT ( 'NONE',  ( 6.123008101752742682, -2.160436397662615970, 0.7664941572692751670 ) ) ;
#46162 = CARTESIAN_POINT ( 'NONE',  ( 4.090329635444483358, -1.806102819543849769, -0.2658631594732660530 ) ) ;
#46163 = CARTESIAN_POINT ( 'NONE',  ( 6.048345925472178308, 9.110135108809304327, 1.082531754730549967 ) ) ;
#46164 = CARTESIAN_POINT ( 'NONE',  ( 4.839897649954202130, 4.748894801142428790, -0.7216878364870197293 ) ) ;
#46165 = CARTESIAN_POINT ( 'NONE',  ( -5.498713818794216834, 8.572860667638675380, -1.199719254218452047 ) ) ;
#46166 = CARTESIAN_POINT ( 'NONE',  ( 5.987861119090863049, 7.014868056141362551, 1.199719254218452047 ) ) ;
#46167 = ORIENTED_EDGE ( 'NONE', *, *, #130801, .T. ) ;
#46169 = CARTESIAN_POINT ( 'NONE',  ( 5.168231636832498310, 2.010700947019973039, -0.1031825239030410013 ) ) ;
#46168 = CARTESIAN_POINT ( 'NONE',  ( 1.469984750362408388, -1.748608032326857353, -0.5769476384821782267 ) ) ;
#46170 = CARTESIAN_POINT ( 'NONE',  ( 1.036931080102401426, 2.214701571188535834, -0.6144361423649072895 ) ) ;
#46171 = CARTESIAN_POINT ( 'NONE',  ( 5.717619619964247946, 0.3862620380215216476, -1.923179868201368548 ) ) ;
#46172 = CARTESIAN_POINT ( 'NONE',  ( -5.747767057189642870, 8.793146435774861658, -1.199719254218440723 ) ) ;
#46173 = CARTESIAN_POINT ( 'NONE',  ( -3.438964519360665051, 7.163875705896082913, -0.7998128361456281477 ) ) ;
#46174 = DIRECTION ( 'NONE',  ( 5.578564026256490882E-16, 1.000000000000000000, 9.066213480720158442E-32 ) ) ;
#46175 = CARTESIAN_POINT ( 'NONE',  ( -5.581116510680924847, 6.540332679663050541, -1.199719254218453823 ) ) ;
#46177 = CARTESIAN_POINT ( 'NONE',  ( 6.368005316177769437, 0.9137572655052300652, 1.515547905889617519 ) ) ;
#46176 = CARTESIAN_POINT ( 'NONE',  ( 1.575843314401915496, -1.115566239278027671, 1.768056137498266844 ) ) ;
#46178 = CARTESIAN_POINT ( 'NONE',  ( -7.727873494160017565, -5.742104877864247392, 7.828177403543863377 ) ) ;
#46179 = CARTESIAN_POINT ( 'NONE',  ( -0.2104748580754391973, 0.7011259924453935310, -2.185273273056092425 ) ) ;
#46180 = CARTESIAN_POINT ( 'NONE',  ( 1.381927130872797838, -0.2546507840628647878, -1.721584071012570050 ) ) ;
#46181 = CARTESIAN_POINT ( 'NONE',  ( 5.438792177376376991, 9.497007973581119700, 1.040834085586084257E-14 ) ) ;
#46183 = CARTESIAN_POINT ( 'NONE',  ( -3.469446951953614189E-15, 3.487142912321096855, 11.99525683304595702 ) ) ;
#46182 = CARTESIAN_POINT ( 'NONE',  ( 0.4999999999999761302, -2.775557561562891351E-14, 0.4999999999999605316 ) ) ;
#46184 = CARTESIAN_POINT ( 'NONE',  ( 1.963112949512689553, 0.2966733001828375516, -1.698991974238444946 ) ) ;
#46185 = CARTESIAN_POINT ( 'NONE',  ( 1.259612756803454525, 2.158328104161820526, -0.3793702838810895095 ) ) ;
#46186 = CARTESIAN_POINT ( 'NONE',  ( 4.442132104469964204, 0.9450947508268662256, -1.994404356956205326 ) ) ;
#46187 = CARTESIAN_POINT ( 'NONE',  ( -10.74038358936941506, 4.109630040845076770, -4.806702709432750353 ) ) ;
#46188 = CARTESIAN_POINT ( 'NONE',  ( 0.8312205373445592516, -2.043673001365586384, -0.7330250775806450569 ) ) ;
#46189 = CARTESIAN_POINT ( 'NONE',  ( 1.284279953904121641, 3.077889714876734573, -0.7749999999999892530 ) ) ;
#46190 = CARTESIAN_POINT ( 'NONE',  ( 3.643865571896960809, 2.100859469783818323, -0.2634356371126170826 ) ) ;
#46191 = ORIENTED_EDGE ( 'NONE', *, *, #135617, .F. ) ;
#46193 = CARTESIAN_POINT ( 'NONE',  ( 1.364683531249988757, 0.4468750003414206917, 0.000000000000000000 ) ) ;
#46192 = CARTESIAN_POINT ( 'NONE',  ( 3.843561273245421628, 0.7716866907857397040, -2.158722107141448188 ) ) ;
#46194 = LINE ( 'NONE', #80811, #150713 ) ;
#46195 = CARTESIAN_POINT ( 'NONE',  ( 4.599240423533799138, 6.388866465587984322, 1.599625672291267398 ) ) ;
#46196 = CARTESIAN_POINT ( 'NONE',  ( 5.725276803944279180, 1.957897222332797504, 1.049153726691682831 ) ) ;
#46197 = CARTESIAN_POINT ( 'NONE',  ( -7.266807147244793263, 8.540658428949452485, 1.082531754730549967 ) ) ;
#46198 = CARTESIAN_POINT ( 'NONE',  ( 4.690757960648224589, 6.495636925554817864, 1.443375672974062551 ) ) ;
#46199 = VECTOR ( 'NONE', #121503, 1000.000000000000000 ) ;
#46200 = CARTESIAN_POINT ( 'NONE',  ( -7.659993601596726265, 8.039006744725394782, -0.7216878364870267237 ) ) ;
#46201 = STYLED_ITEM ( 'NONE', ( #52285 ), #114026 ) ;
#46202 = CARTESIAN_POINT ( 'NONE',  ( 5.411112705629925301, 5.485588709422586362, 0.000000000000000000 ) ) ;
#46203 = VERTEX_POINT ( 'NONE', #156647 ) ;
#46204 = CARTESIAN_POINT ( 'NONE',  ( 3.621720349255663773, 0.2986264320336135536, 1.994071497604548382 ) ) ;
#46206 = CARTESIAN_POINT ( 'NONE',  ( 1.797792903779442009, -1.491087995953117140, -1.425289625791379411 ) ) ;
#46205 = CARTESIAN_POINT ( 'NONE',  ( 6.043183783389218355, 8.073467052085995022, 1.599625672291267398 ) ) ;
#46207 = CARTESIAN_POINT ( 'NONE',  ( 6.434831245971852631, -8.233137084989849086, 7.097136523687869847 ) ) ;
#46208 = CARTESIAN_POINT ( 'NONE',  ( 4.326460416092276162, 7.101268681199365496, -1.082531754730548412 ) ) ;
#46209 = AXIS2_PLACEMENT_3D ( 'NONE', #131267, #148526, #146417 ) ;
#46210 = DIRECTION ( 'NONE',  ( 0.000000000000000000, 0.000000000000000000, 1.000000000000000000 ) ) ;
#46211 = CARTESIAN_POINT ( 'NONE',  ( -1.364683531249997417, 5.509375000341417916, 1.214306433183764966E-14 ) ) ;
#46212 = CARTESIAN_POINT ( 'NONE',  ( 5.384801694919699067, 1.933943663793664225, -1.030698541907522081 ) ) ;
#46213 = CARTESIAN_POINT ( 'NONE',  ( 2.936172824561166905, -1.650081981912490336, -1.158688413653415239 ) ) ;
#46214 = CARTESIAN_POINT ( 'NONE',  ( 2.507154105146496725, -1.820902139252629448, 0.2722148935128121394 ) ) ;
#46215 = ADVANCED_FACE ( 'NONE', ( #39681 ), #20102, .T. ) ;
#46216 = CARTESIAN_POINT ( 'NONE',  ( 7.096803341749390981, 10.36702210109460154, -1.199719254218441611 ) ) ;
#46217 = CARTESIAN_POINT ( 'NONE',  ( 5.051681782491273864, 0.5714109786712183725, -1.733901259708306331 ) ) ;
#46218 = AXIS2_PLACEMENT_3D ( 'NONE', #206171, #28504, #40500 ) ;
#46219 = CARTESIAN_POINT ( 'NONE',  ( 6.522112240665402183, -1.799906897009293738, 0.9091900463213120620 ) ) ;
#46220 = CARTESIAN_POINT ( 'NONE',  ( -8.715193815486133033, 9.062147627688959872, 0.7998128361456462443 ) ) ;
#46222 = CARTESIAN_POINT ( 'NONE',  ( -6.306477729012051725, 7.386587434382707151, 1.199719254218452047 ) ) ;
#46221 = CARTESIAN_POINT ( 'NONE',  ( 6.121994746204825866, -1.250886037347900270, -1.885104629530814702 ) ) ;
#46223 = CARTESIAN_POINT ( 'NONE',  ( 1.330846195043289493, 2.030104276556158549, 0.5602782565924493419 ) ) ;
#46224 = CARTESIAN_POINT ( 'NONE',  ( -7.435720902452096936, 7.639705572474380091, 0.000000000000000000 ) ) ;
#46225 = CARTESIAN_POINT ( 'NONE',  ( 6.903072767652295383, 11.20533532890304684, 1.040834085586084257E-14 ) ) ;
#46226 = CARTESIAN_POINT ( 'NONE',  ( -3.197497122698730099, 6.431928158754200986, 0.6077543439236172684 ) ) ;
#46227 = CARTESIAN_POINT ( 'NONE',  ( 8.378074386687002217, 17.40827499290271518, 19.88167601428683184 ) ) ;
#46228 = CARTESIAN_POINT ( 'NONE',  ( -6.191269702934848240, 10.37489842006599616, 0.000000000000000000 ) ) ;
#46229 = CARTESIAN_POINT ( 'NONE',  ( 3.022498986271238586, 2.800000000000017586, -2.499999999999995115 ) ) ;
#46230 = CARTESIAN_POINT ( 'NONE',  ( 7.849244587668864348, 8.122149871893999062, 0.7998128361456291469 ) ) ;
#46231 = CARTESIAN_POINT ( 'NONE',  ( 5.283544098290614777, 6.372568566219670494, -1.132182188465682859 ) ) ;
#46232 = CARTESIAN_POINT ( 'NONE',  ( -9.327646496521989405, 10.94497100310623594, -1.082531754730539753 ) ) ;
#46233 = CARTESIAN_POINT ( 'NONE',  ( 3.217226816143878398, 1.749018536054181672, -1.369387470038183396 ) ) ;
#46234 = DIRECTION ( 'NONE',  ( 0.000000000000000000, 0.000000000000000000, 1.000000000000000000 ) ) ;
#46235 = CARTESIAN_POINT ( 'NONE',  ( -5.960744811863571968, 6.983232364376142698, 1.199719254218452935 ) ) ;
#46236 = CARTESIAN_POINT ( 'NONE',  ( 7.284808609244363353, 7.393364887073558656, 0.7998128361456341429 ) ) ;
#46237 = CARTESIAN_POINT ( 'NONE',  ( 2.963279974173158138, 1.655882904019840840, 1.051842618152734499 ) ) ;
#46238 = CARTESIAN_POINT ( 'NONE',  ( 4.476163270806094552, 8.373940915915776273, 0.7998128361456462443 ) ) ;
#46239 = CARTESIAN_POINT ( 'NONE',  ( -4.016817522127867690, 7.623078265842172740, -0.1143880650965305862 ) ) ;
#46240 = CARTESIAN_POINT ( 'NONE',  ( 4.172158584703322681, 5.890604320285754980, -1.599625672291256295 ) ) ;
#46241 = CARTESIAN_POINT ( 'NONE',  ( -5.831415467653581430, 5.975941931783510519, 0.7216878364870257245 ) ) ;
#46242 = CARTESIAN_POINT ( 'NONE',  ( -5.409340102172518705, 9.254721185935849803, 0.000000000000000000 ) ) ;
#46243 = CARTESIAN_POINT ( 'NONE',  ( 2.373420902723611725, -1.847293605357634982, -1.041186957106011723 ) ) ;
#46244 = CARTESIAN_POINT ( 'NONE',  ( -6.459533842268148973, 6.500820668926428958, 0.000000000000000000 ) ) ;
#46245 = CARTESIAN_POINT ( 'NONE',  ( 4.961884481312108797, 2.138711985806662330, -0.3135959325617638238 ) ) ;
#46246 = CARTESIAN_POINT ( 'NONE',  ( 2.612652284633736777, -0.1782932461553646819, 1.832575692395449485 ) ) ;
#46247 = CARTESIAN_POINT ( 'NONE',  ( -5.195561487237588594, 6.467898337602993486, 1.183867312878450484 ) ) ;
#46248 = CARTESIAN_POINT ( 'NONE',  ( -0.6823417656250003738, 0.5302083336747518416, -1.181850606188749264 ) ) ;
#46249 = CARTESIAN_POINT ( 'NONE',  ( 5.982304607080743963, -0.2621144554034166574, -1.720346425911468469 ) ) ;
#46250 = CARTESIAN_POINT ( 'NONE',  ( 11.18654035131437219, 1.000000000000000888, -4.041720556560823852 ) ) ;
#46251 = CARTESIAN_POINT ( 'NONE',  ( 5.504247177468190699, 5.523969249908757817, 0.7216878364870317197 ) ) ;
#46252 = DIRECTION ( 'NONE',  ( 0.000000000000000000, 0.000000000000000000, 1.000000000000000000 ) ) ;
#46253 = CARTESIAN_POINT ( 'NONE',  ( 2.835029207381420502, 0.2633842809251253358, 2.145520918749081574 ) ) ;
#46254 = CARTESIAN_POINT ( 'NONE',  ( 4.604842190751081255, 0.8645911521153251122, -1.821463593394745395 ) ) ;
#46255 = CARTESIAN_POINT ( 'NONE',  ( -7.931156673870055407, 11.23647130528163096, 1.082531754730549967 ) ) ;
#46256 = CARTESIAN_POINT ( 'NONE',  ( 2.659225025413253007, -1.880336703546074073, -1.066323988048665017 ) ) ;
#46257 = CARTESIAN_POINT ( 'NONE',  ( 2.688696339244216915, -0.3334303690454739066, -1.942799078106532074 ) ) ;
#46258 = CARTESIAN_POINT ( 'NONE',  ( -3.474999999999997868, -2.727083332377417957, 2.006292185433951047 ) ) ;
#46259 = CARTESIAN_POINT ( 'NONE',  ( 4.757337479089009058, 1.920383491809660503, -0.2886861380682907430 ) ) ;
#46263 = ORIENTED_EDGE ( 'NONE', *, *, #33969, .T. ) ;
#46262 = ADVANCED_FACE ( 'NONE', ( #190188, #126353 ), #110089, .F. ) ;
#46261 = CARTESIAN_POINT ( 'NONE',  ( 0.000000000000000000, 2.800000000000024691, 1.214306433183764966E-14 ) ) ;
#46260 = CARTESIAN_POINT ( 'NONE',  ( -7.483737604619046913, 11.67485160545682987, 0.000000000000000000 ) ) ;
#46264 = CARTESIAN_POINT ( 'NONE',  ( -4.516274566683622815, 5.401980094953223066, 1.082531754730549078 ) ) ;
#46265 = CARTESIAN_POINT ( 'NONE',  ( -11.88168509644349058, 12.21999999999998288, 1.685788023084328513 ) ) ;
#46267 = EDGE_LOOP ( 'NONE', ( #27202, #205556, #145134, #171190 ) ) ;
#46266 = CARTESIAN_POINT ( 'NONE',  ( -4.305596300791617814, 7.180890229968955651, 1.199719254218452935 ) ) ;
#46268 = CARTESIAN_POINT ( 'NONE',  ( -7.443063143778079649, 10.66702885350765584, 1.082531754730549967 ) ) ;
#46269 = CARTESIAN_POINT ( 'NONE',  ( 1.395868886378356821, 1.671639904693554168, 1.440724375100350008 ) ) ;
#46270 = CARTESIAN_POINT ( 'NONE',  ( -3.285556943750000070, -0.8093749995220431703, 0.000000000000000000 ) ) ;
#46271 = CARTESIAN_POINT ( 'NONE',  ( 5.858247074779933783, -1.961936380223072263, -0.003592477671530979431 ) ) ;
#46272 =( BOUNDED_SURFACE ( )  B_SPLINE_SURFACE ( 3, 2, ( 
 ( #168335, #19929, #86016 ),
 ( #7166, #105800, #21271 ),
 ( #190196, #71092, #188060 ),
 ( #169683, #138272, #206446 ) ),
 .UNSPECIFIED., .F., .F., .T. ) 
 B_SPLINE_SURFACE_WITH_KNOTS ( ( 4, 4 ),
 ( 3, 3 ),
 ( 0.004991389062828482590, 0.008017777006561210146 ),
 ( 0.000000000000000000, 1.000000000000000000 ),
 .UNSPECIFIED. ) 
 GEOMETRIC_REPRESENTATION_ITEM ( )  RATIONAL_B_SPLINE_SURFACE ( (
 ( 1.000000000000000000, 0.7184380228464066764, 1.000000000000000000),
 ( 1.000000000000000000, 0.7185467277397524777, 1.000000000000000000),
 ( 1.000000000000000000, 0.7186585579881034080, 1.000000000000000000),
 ( 1.000000000000000000, 0.7187737999613694750, 1.000000000000000000) ) ) 
 REPRESENTATION_ITEM ( '' )  SURFACE ( )  );
#46273 = CARTESIAN_POINT ( 'NONE',  ( -1.364683531250010295, 5.301041667008085767, -0.7879004041258300672 ) ) ;
#46274 = CARTESIAN_POINT ( 'NONE',  ( -1.499999999999997780, 3.931250000682819046, 1.214306433183764966E-14 ) ) ;
#46275 = CARTESIAN_POINT ( 'NONE',  ( 5.803731464950218744, 6.215061796778338810, -0.9591748237987550718 ) ) ;
#46276 = CARTESIAN_POINT ( 'NONE',  ( 0.1749903794560748460, 0.004523422195302355051, -1.955468523092759314 ) ) ;
#46277 = CARTESIAN_POINT ( 'NONE',  ( 4.347483306186128438, 1.840691044367316120, -0.04759384897683878457 ) ) ;
#46278 = ORIENTED_EDGE ( 'NONE', *, *, #119577, .F. ) ;
#46279 = CARTESIAN_POINT ( 'NONE',  ( 1.360316468749955598, -0.7135416663252973635, -0.7853790794159122290 ) ) ;
#46280 = EDGE_CURVE ( 'NONE', #154266, #70814, #179234, .T. ) ;
#46281 = CARTESIAN_POINT ( 'NONE',  ( -6.821723845970312894, 11.11042825360738284, 0.000000000000000000 ) ) ;
#46282 = DIRECTION ( 'NONE',  ( 1.000000000000000000, 0.000000000000000000, 0.000000000000000000 ) ) ;
#46283 = CARTESIAN_POINT ( 'NONE',  ( 11.88234649872613602, 11.25660782916751579, 0.9090484974825158160 ) ) ;
#46284 = CARTESIAN_POINT ( 'NONE',  ( 9.072916337883725646, 12.13354503355262004, -7.783615223256313165 ) ) ;
#46285 = CARTESIAN_POINT ( 'NONE',  ( 6.810273232766058449, 6.839740281182199233, 1.040834085586084257E-14 ) ) ;
#46286 = CARTESIAN_POINT ( 'NONE',  ( 0.2333700457068142997, -1.884473515381725361, 0.8346939899398809759 ) ) ;
#46289 = CARTESIAN_POINT ( 'NONE',  ( 4.018977146631536712, -1.760761141180338774, 0.5383908109771737838 ) ) ;
#46288 = CARTESIAN_POINT ( 'NONE',  ( 1.996334026009699558, 1.840204857836050367, 0.2769876585018010706 ) ) ;
#46287 = CARTESIAN_POINT ( 'NONE',  ( -9.804626464733818381, 4.469082038635498577, 6.926798510140733001 ) ) ;
#46290 = CARTESIAN_POINT ( 'NONE',  ( 6.598014311344812199, 10.84943379654430906, 1.040834085586084257E-14 ) ) ;
#46291 = DIRECTION ( 'NONE',  ( 0.000000000000000000, 8.546850786086437571E-32, 1.000000000000000000 ) ) ;
#46292 = CIRCLE ( 'NONE', #198388, 9.999999999999996447 ) ;
#46293 = CARTESIAN_POINT ( 'NONE',  ( -6.444921918449773024, 8.612437886315108315, 1.599625672291269396 ) ) ;
#46294 = FACE_OUTER_BOUND ( 'NONE', #44706, .T. ) ;
#46295 = CIRCLE ( 'NONE', #87704, 0.07999999999999997391 ) ;
#46296 = CARTESIAN_POINT ( 'NONE',  ( 3.141465813989018141, -1.946189201368169641, 1.040519825639886431 ) ) ;
#46297 = CARTESIAN_POINT ( 'NONE',  ( 5.536487020692383076, 2.227601090660180638, 0.3946122451431322009 ) ) ;
#46298 = CARTESIAN_POINT ( 'NONE',  ( -5.097502569058207200, 8.890910730635814829, -0.7216878364870207285 ) ) ;
#46299 = CARTESIAN_POINT ( 'NONE',  ( 5.431847905162764611, -1.765542832439458198, 0.4050695418617160648 ) ) ;
#46300 = CARTESIAN_POINT ( 'NONE',  ( 5.964071289222036221, -1.018598136897935547, 1.622275196354412419 ) ) ;
#46301 = CARTESIAN_POINT ( 'NONE',  ( -1.084637062511545347, 3.148878807974804239, -1.105835307554788649 ) ) ;
#46302 = CARTESIAN_POINT ( 'NONE',  ( 5.946149726614579301, 1.868617323842229894, 0.09011704611043556967 ) ) ;
#46303 = DIRECTION ( 'NONE',  ( 0.000000000000000000, 0.000000000000000000, 1.000000000000000000 ) ) ;
#46304 = ADVANCED_FACE ( 'NONE', ( #10368 ), #123963, .F. ) ;
#46305 = CARTESIAN_POINT ( 'NONE',  ( 5.858207189965921380, 0.7206212418228461480, 1.616676333947133504 ) ) ;
#46306 = CARTESIAN_POINT ( 'NONE',  ( 1.077361674225948418, 1.530160568918725872, 1.313541346884481209 ) ) ;
#46308 = CARTESIAN_POINT ( 'NONE',  ( 3.106188079018203041, -2.103647721026543405, 0.1036251941764678303 ) ) ;
#46307 = CARTESIAN_POINT ( 'NONE',  ( -9.341731535015849630, 10.85744053139533349, 1.199719254218462483 ) ) ;
#46309 = CARTESIAN_POINT ( 'NONE',  ( 9.206149998879153529, 10.69926207256923689, 1.199719254218453823 ) ) ;
#46311 = CARTESIAN_POINT ( 'NONE',  ( -7.655550293210764856, 12.08322577538792331, 0.000000000000000000 ) ) ;
#46310 = CARTESIAN_POINT ( 'NONE',  ( 0.7499999999999885647, -1.016666666666644847, 1.299038105676657340 ) ) ;
#46312 = DIRECTION ( 'NONE',  ( 0.000000000000000000, 1.000000000000000000, 0.000000000000000000 ) ) ;
#46313 = CARTESIAN_POINT ( 'NONE',  ( 2.478776341996299593, -1.389826682745049835, 1.465835156725032506 ) ) ;
#46314 = CARTESIAN_POINT ( 'NONE',  ( 1.364683531249988535, 3.113541667008083991, 0.7879004041258500513 ) ) ;
#46315 = CARTESIAN_POINT ( 'NONE',  ( 3.358669367883368118, 4.941533567329135401, -1.599625672291262513 ) ) ;
#46316 = CARTESIAN_POINT ( 'NONE',  ( 3.304151629394710632, -2.159270932758147854, 0.1024373671053082913 ) ) ;
#46317 = CARTESIAN_POINT ( 'NONE',  ( 6.556249800660121529, 9.806652646482286073, 1.199719254218452047 ) ) ;
#46319 = DIRECTION ( 'NONE',  ( -5.551115123125765446E-17, 0.000000000000000000, 1.000000000000000000 ) ) ;
#46318 = CARTESIAN_POINT ( 'NONE',  ( 6.535912570239620578, 9.782925877658371405, 1.199719254218452047 ) ) ;
#46320 = CARTESIAN_POINT ( 'NONE',  ( 10.04622863760192963, 10.82294762006482713, -0.7216878364870257245 ) ) ;
#46322 = FACE_OUTER_BOUND ( 'NONE', #60645, .T. ) ;
#46321 = CARTESIAN_POINT ( 'NONE',  ( 1.276089585440323138, -2.118389508516528519, 0.4752255978458518881 ) ) ;
#46323 = CARTESIAN_POINT ( 'NONE',  ( -6.778713617152821058, 7.971215977175476475, 1.082531754730549967 ) ) ;
#46324 = CARTESIAN_POINT ( 'NONE',  ( 0.6823417656249899377, 0.5927083336747518416, 1.181850606188755259 ) ) ;
#46325 = CARTESIAN_POINT ( 'NONE',  ( 2.314256413632868714, 1.428969747754246233, -1.661726224907192684 ) ) ;
#46326 = CARTESIAN_POINT ( 'NONE',  ( -3.578934198120170329, 6.213868303620019518, 1.151059397407709239 ) ) ;
#46327 = CARTESIAN_POINT ( 'NONE',  ( 2.729655337971720552, -2.111368630554604220, 0.8135341271046038214 ) ) ;
#46328 = CARTESIAN_POINT ( 'NONE',  ( -6.645467848992654858, 10.90479625713344625, 0.7998128361456481317 ) ) ;
#46329 = CARTESIAN_POINT ( 'NONE',  ( 4.522672878804367969, 0.3494810548456111499, 1.985869246038343583 ) ) ;
#46330 = CARTESIAN_POINT ( 'NONE',  ( -4.568734577680899633, 4.432537883490215158, -0.7216878364870207285 ) ) ;
#46331 = CARTESIAN_POINT ( 'NONE',  ( 0.6823417656249917140, 3.655208333674754506, 1.181850606188765695 ) ) ;
#46332 = CARTESIAN_POINT ( 'NONE',  ( 4.826264338009964128, 8.099924789650724932, 0.8724150771263041726 ) ) ;
#46333 = CARTESIAN_POINT ( 'NONE',  ( -0.7500000000000179856, 10.79166666666666430, 1.299038105676658228 ) ) ;
#46334 = CARTESIAN_POINT ( 'NONE',  ( 6.292392690518195941, 8.434487120394948079, -1.443375672974078761 ) ) ;
#46335 = CARTESIAN_POINT ( 'NONE',  ( 3.198275679207917666, -0.5104862868050319413, -1.694526722652128781 ) ) ;
#46336 = CARTESIAN_POINT ( 'NONE',  ( 3.123692395903770347, -0.3905211382968387102, 1.974689860881967407 ) ) ;
#46337 = CARTESIAN_POINT ( 'NONE',  ( 8.615316546479974136, 12.13862083994696839, 1.199719254218450271 ) ) ;
#46338 = CARTESIAN_POINT ( 'NONE',  ( 6.264705869774118696, -1.564926740429407603, 1.556175991035801287 ) ) ;
#46339 = CARTESIAN_POINT ( 'NONE',  ( -0.6823417656250003738, 9.401041667008065872, 1.181850606188754593 ) ) ;
#46340 = CARTESIAN_POINT ( 'NONE',  ( -5.204350862799341115, 7.165104988056252289, -1.599625672291271394 ) ) ;
#46341 = CARTESIAN_POINT ( 'NONE',  ( 5.853138716089107518, 0.1455171034051294665, -2.011206573937059261 ) ) ;
#46342 = EDGE_LOOP ( 'NONE', ( #161148, #91583, #213793, #91136 ) ) ;
#46343 = CARTESIAN_POINT ( 'NONE',  ( 3.748781033766034554, -1.529746656882627232, 1.076398355447941491 ) ) ;
#46344 = CARTESIAN_POINT ( 'NONE',  ( 3.836834752522141567, -1.993853832596056197, -0.5568897355931883286 ) ) ;
#46345 = AXIS2_PLACEMENT_3D ( 'NONE', #49926, #151705, #201474 ) ;
#46346 = CARTESIAN_POINT ( 'NONE',  ( -6.007671464186866928, 8.102312356341712984, 1.443375672974058777 ) ) ;
#46347 = CARTESIAN_POINT ( 'NONE',  ( -9.429315115559251836, 5.003428342543706719, -6.892195246777336415 ) ) ;
#46348 = SURFACE_STYLE_FILL_AREA ( #178475 ) ;
#46349 = CARTESIAN_POINT ( 'NONE',  ( 6.121977807712331909, -1.196819783530624015, -1.799967629666970881 ) ) ;
#46350 = CARTESIAN_POINT ( 'NONE',  ( 1.364683531249986537, -1.136458332991912235, 0.7879004041258500513 ) ) ;
#46351 = CARTESIAN_POINT ( 'NONE',  ( 2.699599903323801620, -1.451799986561516764, -1.319707477925702310 ) ) ;
#46352 = CARTESIAN_POINT ( 'NONE',  ( 1.159529582462547781, -0.4871260124716703666, -1.956262300040665814 ) ) ;
#46353 = DIRECTION ( 'NONE',  ( 1.000000000000000000, -0.000000000000000000, 1.224646799147353207E-16 ) ) ;
#46354 = CARTESIAN_POINT ( 'NONE',  ( 6.747154001095143627, 11.02343010125301959, -0.7998128361456291469 ) ) ;
#46355 = CARTESIAN_POINT ( 'NONE',  ( 1.141631569582121974, 0.7634220068381203372, -1.707866752806507460 ) ) ;
#46356 = CARTESIAN_POINT ( 'NONE',  ( -1.201851678989727383E-14, 3.946875000341423689, -1.575800808251660134 ) ) ;
#46357 = CARTESIAN_POINT ( 'NONE',  ( 3.533450910810581824, -0.1440131911168585910, 2.008084626805274997 ) ) ;
#46359 = CARTESIAN_POINT ( 'NONE',  ( 1.722414120629287337, 2.094725599053618659, 0.3070382465363735158 ) ) ;
#46358 = CARTESIAN_POINT ( 'NONE',  ( -6.724481002698126098, 8.868313807946373473, -1.443375672974059665 ) ) ;
#46360 = CARTESIAN_POINT ( 'NONE',  ( 9.973831171035394405, 9.867947520626652036, -6.611755878741440107 ) ) ;
#46361 = CARTESIAN_POINT ( 'NONE',  ( 4.141125838365485201, -0.1998502692034490602, -2.060677327190631569 ) ) ;
#46362 = CARTESIAN_POINT ( 'NONE',  ( 7.679767667498067496, 7.924426798361372093, 0.000000000000000000 ) ) ;
#46364 = CARTESIAN_POINT ( 'NONE',  ( 4.729096653068339151, 4.411700938201493116, -0.7998128361456211532 ) ) ;
#46363 = CARTESIAN_POINT ( 'NONE',  ( 5.683562130502735954, -0.9407222913834032418, 1.867095764824426851 ) ) ;
#46366 = ORIENTED_EDGE ( 'NONE', *, *, #158371, .F. ) ;
#46365 = CARTESIAN_POINT ( 'NONE',  ( 4.664971680594516279, -1.631047870213175432, -0.8201845326444437978 ) ) ;
#46367 = CARTESIAN_POINT ( 'NONE',  ( 10.05067194643221207, 10.62020544712608938, 0.7998128361456462443 ) ) ;
#46368 = CARTESIAN_POINT ( 'NONE',  ( 4.786522169170392971, 5.141580351323886688, 0.8077998227834035649 ) ) ;
#46369 = CARTESIAN_POINT ( 'NONE',  ( 9.963343620504341303, 12.35838256557349979, -7.799456358664951239 ) ) ;
#46370 = CARTESIAN_POINT ( 'NONE',  ( -10.10575425844435138, 4.358269247758318699, 5.859476710806498900 ) ) ;
#46371 = CARTESIAN_POINT ( 'NONE',  ( 0.6823417656249969321, 11.08854166700806765, -1.181850606188757036 ) ) ;
#46372 = CARTESIAN_POINT ( 'NONE',  ( 5.426388453851806126, -0.8635988772061551355, -1.706256623820540108 ) ) ;
#46373 = CARTESIAN_POINT ( 'NONE',  ( -10.29471871147821282, 10.90492667301307605, -0.7998128361456291469 ) ) ;
#46374 = CARTESIAN_POINT ( 'NONE',  ( 6.120616281565444794, 9.228137197546649517, -1.199719254218440723 ) ) ;
#46375 = CARTESIAN_POINT ( 'NONE',  ( -9.514659125335341649E-15, 1.359375000341400463, -1.570758158831806250 ) ) ;
#46376 = CARTESIAN_POINT ( 'NONE',  ( 2.833290915131624566, 6.249330467721451399, -0.7216878364870267237 ) ) ;
#46377 = CARTESIAN_POINT ( 'NONE',  ( 9.500479199177245704, -7.792108994756139495, -0.01138762994422098072 ) ) ;
#46378 = CARTESIAN_POINT ( 'NONE',  ( 0.6437974683802077935, 0.5340323341261629109, 1.762076181610471526 ) ) ;
#46379 = ORIENTED_EDGE ( 'NONE', *, *, #38367, .F. ) ;
#46380 = EDGE_CURVE ( 'NONE', #21699, #12264, #141235, .T. ) ;
#46381 = FILL_AREA_STYLE ('',( #112499 ) ) ;
#46382 = CARTESIAN_POINT ( 'NONE',  ( 4.340975799156802317, -1.628549031532234403, 0.9200136957008757665 ) ) ;
#46383 = CARTESIAN_POINT ( 'NONE',  ( -0.1937322346335085266, -3.136378490158120425, -3.381421948784809839 ) ) ;
#46384 = CARTESIAN_POINT ( 'NONE',  ( 6.261886844665240481, 8.398896966899865646, 1.599625672291268286 ) ) ;
#46385 = CARTESIAN_POINT ( 'NONE',  ( -1.438721403204643368, 7.870009100113813716, -3.684356824106938877 ) ) ;
#46386 = CARTESIAN_POINT ( 'NONE',  ( -5.710744021720588925, 7.310394840978843511, 1.216594670743395445 ) ) ;
#46388 = CARTESIAN_POINT ( 'NONE',  ( -6.778713617152821058, 7.971215977175476475, 1.082531754730549967 ) ) ;
#46387 = AXIS2_PLACEMENT_3D ( 'NONE', #136582, #55319, #86746 ) ;
#46389 = CARTESIAN_POINT ( 'NONE',  ( 3.174580523894166006, 6.855427711185178019, 0.7998128361456341429 ) ) ;
#46390 = CARTESIAN_POINT ( 'NONE',  ( 0.8484201349984072937, -1.953920032193863232, -0.2464512992164570593 ) ) ;
#46391 = CARTESIAN_POINT ( 'NONE',  ( 2.882435586221145485, -0.5880402899147363360, -1.928746874286999979 ) ) ;
#46392 = CARTESIAN_POINT ( 'NONE',  ( -6.170932472514347289, 10.35117165124207972, 0.000000000000000000 ) ) ;
#46393 = CARTESIAN_POINT ( 'NONE',  ( 4.692003678781083487, 7.631698837623355658, -1.199719254218450271 ) ) ;
#46394 = CYLINDRICAL_SURFACE ( 'NONE', #35478, 1.500000000000000222 ) ;
#46395 = CARTESIAN_POINT ( 'NONE',  ( 4.031328258368102269, -1.510625130563835627, -1.587819133214096734 ) ) ;
#46396 = CARTESIAN_POINT ( 'NONE',  ( 2.393960638069839941, 0.2282907053230429639, -0.4203461706283275201 ) ) ;
#46397 = CARTESIAN_POINT ( 'NONE',  ( -9.833741488613570780, 10.36711991300432345, 0.7998128361456462443 ) ) ;
#46398 = CARTESIAN_POINT ( 'NONE',  ( -1.123270288254055060, 3.033552654332631437, 0.7749999999939939377 ) ) ;
#46399 = CARTESIAN_POINT ( 'NONE',  ( 1.423205080756922314, 7.980384757729337863, 10.65537363484301459 ) ) ;
#46400 = CARTESIAN_POINT ( 'NONE',  ( 4.909461021924256485, 4.900328411765999981, 0.7216878364870338292 ) ) ;
#46401 = CARTESIAN_POINT ( 'NONE',  ( 8.606728586576791074, 8.935604860628076906, 0.7998128361456462443 ) ) ;
#46402 = ADVANCED_FACE ( 'NONE', ( #192313 ), #44254, .T. ) ;
#46403 = CYLINDRICAL_SURFACE ( 'NONE', #119321, 1.250000000000000000 ) ;
#46404 = CARTESIAN_POINT ( 'NONE',  ( 4.746763178560241769, 8.551991118380046331, 0.7216878364870328300 ) ) ;
#46405 = ORIENTED_EDGE ( 'NONE', *, *, #39139, .T. ) ;
#46407 = CARTESIAN_POINT ( 'NONE',  ( 2.121741512283023656, -0.4388329339449773547, 1.964535544105987075 ) ) ;
#46406 = CARTESIAN_POINT ( 'NONE',  ( 4.546344060013487898, -1.475942220874026489, 1.100600019281534836 ) ) ;
#46408 = CARTESIAN_POINT ( 'NONE',  ( 3.743815364168050053, -2.214071480395309433, -0.6165714402358390966 ) ) ;
#46410 = CARTESIAN_POINT ( 'NONE',  ( 1.762329786688419109, -0.6638292341827031207, -1.738725725234435693 ) ) ;
#46409 = CARTESIAN_POINT ( 'NONE',  ( -0.02919842301641033255, 0.7163969788333038879, -2.157531187298274311 ) ) ;
#46411 = CARTESIAN_POINT ( 'NONE',  ( -3.285556943750000070, -2.209374999522041527, 0.000000000000000000 ) ) ;
#46412 = DIRECTION ( 'NONE',  ( -0.000000000000000000, -1.000000000000000000, 0.000000000000000000 ) ) ;
#46413 = CARTESIAN_POINT ( 'NONE',  ( 5.343983030329363615, -1.218012673290536974, -1.474316871017400166 ) ) ;
#46414 = CARTESIAN_POINT ( 'NONE',  ( -8.941766003412679353, 10.39081407785832845, -1.199719254218446718 ) ) ;
#46415 = CARTESIAN_POINT ( 'NONE',  ( -5.316205630334263965, 7.295602216847000498, -1.443375672974066548 ) ) ;
#46417 = CARTESIAN_POINT ( 'NONE',  ( 2.904993682805886213, 1.579364189935757778, 1.002181356900035070 ) ) ;
#46416 = CARTESIAN_POINT ( 'NONE',  ( 5.267163683669145335, 2.014557126142228594, -0.5589344999666242542 ) ) ;
#46418 = CARTESIAN_POINT ( 'NONE',  ( 5.612712406377503349, 8.531619659873665995, -1.082531754730543083 ) ) ;
#46419 = CARTESIAN_POINT ( 'NONE',  ( 5.847170753249844033, 0.5281823367668266878, -1.763884204139199330 ) ) ;
#46420 = CARTESIAN_POINT ( 'NONE',  ( 3.521367211247359741, 5.131347717920458962, -1.599625672291262513 ) ) ;
#46421 = CARTESIAN_POINT ( 'NONE',  ( 0.1360919303235845756, -7.795524846228436999, -10.99936842639231571 ) ) ;
#46422 = CARTESIAN_POINT ( 'NONE',  ( 5.320820994898000755, 1.595919931443249951, 0.6549295409969541071 ) ) ;
#46423 = CARTESIAN_POINT ( 'NONE',  ( -5.201524489137236529, 9.220195670635433771, 0.7998128361456481317 ) ) ;
#46424 = CARTESIAN_POINT ( 'NONE',  ( 0.5274301605363295176, -1.488642097782297835, 0.8892331099567828412 ) ) ;
#46425 = DIRECTION ( 'NONE',  ( 1.276756478318932585E-15, -1.000000000000000000, 1.665334536937738262E-16 ) ) ;
#46426 = CARTESIAN_POINT ( 'NONE',  ( 6.210172754313918908, 1.157103754073171675, -1.651340222398114843 ) ) ;
#46427 = DIRECTION ( 'NONE',  ( 1.000000000000000000, 1.725633230170963762E-31, 8.638326563840814399E-31 ) ) ;
#46428 = CARTESIAN_POINT ( 'NONE',  ( 4.838842012204412235, -2.104300398676747896, -0.5337788192065362480 ) ) ;
#46429 = CARTESIAN_POINT ( 'NONE',  ( 2.771877994228102882, 0.9767612972278701955, 1.542236413651025151 ) ) ;
#46430 = CARTESIAN_POINT ( 'NONE',  ( 1.217545072937670225, 0.3881152535412414339, -1.922811240370206232 ) ) ;
#46431 = CARTESIAN_POINT ( 'NONE',  ( 6.245324861096241520, 0.3598972253578552327, -2.086368836056912368 ) ) ;
#46433 = CARTESIAN_POINT ( 'NONE',  ( -0.6823417656250212460, 4.613541667008086655, 1.181850606188767472 ) ) ;
#46432 = CARTESIAN_POINT ( 'NONE',  ( 0.4281777144111223454, 1.173252442481845126, -1.969132371278771831 ) ) ;
#46434 = CARTESIAN_POINT ( 'NONE',  ( 4.007721930888963335, 7.796164093330856026, -0.2192809687468954827 ) ) ;
#46435 = CARTESIAN_POINT ( 'NONE',  ( 8.076906825439115423, 10.44614393447756129, -1.599625672291262513 ) ) ;
#46436 = CARTESIAN_POINT ( 'NONE',  ( 2.157031413788193852, 0.4673396547767159070, 2.068183735011968061 ) ) ;
#46437 = CARTESIAN_POINT ( 'NONE',  ( -3.578989364327652467, 6.158942777482099729, 1.082531754730560403 ) ) ;
#46438 = DIRECTION ( 'NONE',  ( 0.000000000000000000, 1.000000000000000000, 0.000000000000000000 ) ) ;
#46439 = CARTESIAN_POINT ( 'NONE',  ( -4.351804119862249465, 7.060559992272473551, 1.082531754730560403 ) ) ;
#46440 = CARTESIAN_POINT ( 'NONE',  ( 1.147426569842596722, 1.827566109494669577, -0.9725325914680116313 ) ) ;
#46442 = CARTESIAN_POINT ( 'NONE',  ( 0.7500000000000006661, 14.11458333401613352, 1.299038105676657340 ) ) ;
#46441 = CARTESIAN_POINT ( 'NONE',  ( 6.983263157960370116, 1.251666756963093041, 2.167287073222202931 ) ) ;
#46444 = ORIENTED_EDGE ( 'NONE', *, *, #47557, .T. ) ;
#46443 = CARTESIAN_POINT ( 'NONE',  ( 2.561440534034305827, -1.845267710029829145, 1.236318238231758571 ) ) ;
#46445 = CARTESIAN_POINT ( 'NONE',  ( 0.4757056697715462690, -2.282288811291408148, -0.2737132658124728501 ) ) ;
#46447 = CARTESIAN_POINT ( 'NONE',  ( 5.207907603007337016, 0.6519758639490059737, -1.956853833162349066 ) ) ;
#46446 = CARTESIAN_POINT ( 'NONE',  ( 4.871457266011829823, 4.577788319968905562, -0.7998128361456221525 ) ) ;
#46449 = CARTESIAN_POINT ( 'NONE',  ( 1.001543065824772753E-15, -2.712499999999999911, 4.012584370867899430 ) ) ;
#46448 = CARTESIAN_POINT ( 'NONE',  ( 6.554440917563797875, 6.611545590104705994, -0.7998128361456481317 ) ) ;
#46450 = CARTESIAN_POINT ( 'NONE',  ( 6.547661840756936691, 6.603636667163397256, 0.7998128361456352531 ) ) ;
#46451 = CARTESIAN_POINT ( 'NONE',  ( 0.2331563151865451988, 4.092570554693980789, -2.500672995626152861 ) ) ;
#46452 = CARTESIAN_POINT ( 'NONE',  ( 5.829618728418341611, 0.9018330327132916269, -1.605192750430362025 ) ) ;
#46453 = CARTESIAN_POINT ( 'NONE',  ( 4.701980345841006326, 4.380065246436280368, 0.7998128361456341429 ) ) ;
#46454 = CARTESIAN_POINT ( 'NONE',  ( 1.693959787788183347, -1.716010565565774915, -0.1736237626131422462 ) ) ;
#46455 = CARTESIAN_POINT ( 'NONE',  ( 1.130092623156966347, 2.014433208573155110, 0.09411304420373775570 ) ) ;
#46456 = CARTESIAN_POINT ( 'NONE',  ( 2.286107107991880216, 1.843941258665306115, -1.372366127498450883 ) ) ;
#46457 = CARTESIAN_POINT ( 'NONE',  ( -1.364683531249997417, 4.071875000341417028, 1.214306433183764966E-14 ) ) ;
#46458 = CARTESIAN_POINT ( 'NONE',  ( 2.144175119285938180, 0.8672398327666650530, -2.089775168228876545 ) ) ;
#46459 = CARTESIAN_POINT ( 'NONE',  ( 4.459663826605764214, 0.4620033958209149305, -2.054602365452788071 ) ) ;
#46460 = CARTESIAN_POINT ( 'NONE',  ( -4.442231607132987925, 5.211633625523774960, -1.199719254218453823 ) ) ;
#46461 = CARTESIAN_POINT ( 'NONE',  ( 2.407162768383603435, -0.3926560375935496672, 1.725441652247063251 ) ) ;
#46462 = CARTESIAN_POINT ( 'NONE',  ( 4.611744806942754238, 8.532119374741881757, -0.7998128361456231517 ) ) ;
#46464 = CARTESIAN_POINT ( 'NONE',  ( 4.985981925524552771, -2.274816124779193593, -0.2825110863640226122 ) ) ;
#46463 = CARTESIAN_POINT ( 'NONE',  ( 6.007671464186837618, 6.181573927739029806, 0.7216878364870328300 ) ) ;
#46465 = CARTESIAN_POINT ( 'NONE',  ( 4.066218318298571610, -1.718653781379267276, -0.6607852518168353395 ) ) ;
#46466 = CARTESIAN_POINT ( 'NONE',  ( -3.815730167242251003, 6.539103397502874948, -1.199719254218452047 ) ) ;
#46467 = CARTESIAN_POINT ( 'NONE',  ( 6.602457619730771832, 6.805214765881779648, 0.7216878364870317197 ) ) ;
#46468 = CARTESIAN_POINT ( 'NONE',  ( -1.500000000000013101, 2.879166666666688634, -0.8660254037844313801 ) ) ;
#46469 = CARTESIAN_POINT ( 'NONE',  ( 4.998067021457727854, -0.7363416341295281331, -2.064161796032103258 ) ) ;
#46470 = CARTESIAN_POINT ( 'NONE',  ( -3.761497552787613330, 6.475832013972435242, 1.199719254218464037 ) ) ;
#46471 = CARTESIAN_POINT ( 'NONE',  ( 0.4942839625836501494, 7.528790859548413650, -2.012357903315102448 ) ) ;
#46472 = CARTESIAN_POINT ( 'NONE',  ( 0.4635785636673654952, -6.836568542495036205, 10.85353573482952250 ) ) ;
#46473 = CARTESIAN_POINT ( 'NONE',  ( 1.364683531249990311, 5.134375000341417916, 1.214306433183764966E-14 ) ) ;
#46474 = CARTESIAN_POINT ( 'NONE',  ( 2.684106373981818727, -0.9902706917056921521, 1.652370099195903386 ) ) ;
#46475 = CARTESIAN_POINT ( 'NONE',  ( -1.402160292154681736E-14, 8.921875000341405126, 1.575800808251682339 ) ) ;
#46476 = CARTESIAN_POINT ( 'NONE',  ( -4.609409038966248318, 5.440360635957812718, -1.082531754730544860 ) ) ;
#46477 = CARTESIAN_POINT ( 'NONE',  ( 5.572555445586866441, 0.8612648569810870125, 1.938019255899057658 ) ) ;
#46478 = CARTESIAN_POINT ( 'NONE',  ( -6.943184063974186415, 7.273005294157565359, -0.7216878364870338292 ) ) ;
#46479 = ORIENTED_EDGE ( 'NONE', *, *, #104334, .F. ) ;
#46481 = DIRECTION ( 'NONE',  ( -0.6260462619842731558, 0.7797859179643593652, 0.000000000000000000 ) ) ;
#46480 = CARTESIAN_POINT ( 'NONE',  ( -4.502716413514301408, 7.306900678191715848, -1.082531754730549967 ) ) ;
#46482 = CARTESIAN_POINT ( 'NONE',  ( 4.542145155778077203, 5.257923088951247159, -1.199719254218452047 ) ) ;
#46483 = CARTESIAN_POINT ( 'NONE',  ( -1.201851678989727383E-14, 3.087500000000026112, -1.732050807568863648 ) ) ;
#46484 = CARTESIAN_POINT ( 'NONE',  ( -5.614485009390564940, 5.722856397143323726, 0.000000000000000000 ) ) ;
#46485 = CARTESIAN_POINT ( 'NONE',  ( -0.1021852871783673899, 7.053056311350172969, -4.037408415133502793 ) ) ;
#46486 = CARTESIAN_POINT ( 'NONE',  ( -1.364683531250012516, 4.051041667008088432, -0.7879004041258300672 ) ) ;
#46487 = CARTESIAN_POINT ( 'NONE',  ( 1.909305195714078307, -0.8207579233160157139, -1.534770245041901182 ) ) ;
#46488 = CARTESIAN_POINT ( 'NONE',  ( 3.540436255445079894, 7.352535741319725204, -0.1172168222480891864 ) ) ;
#46489 = CARTESIAN_POINT ( 'NONE',  ( 0.3440982351944205653, -0.9282241650855774795, 1.728402704573736903 ) ) ;
#46490 = CARTESIAN_POINT ( 'NONE',  ( 1.364683531249988757, 0.4468750003414206917, 0.000000000000000000 ) ) ;
#46491 = DIRECTION ( 'NONE',  ( 0.000000000000000000, 0.3953086839949069842, 0.9185483353412680074 ) ) ;
#46492 = CARTESIAN_POINT ( 'NONE',  ( 5.840740251263128791, 0.4172088472891195554, 2.120894824392767664 ) ) ;
#46493 = CARTESIAN_POINT ( 'NONE',  ( -10.30827686509187835, 10.92074451889568643, 1.040834085586084257E-14 ) ) ;
#46494 = CARTESIAN_POINT ( 'NONE',  ( -7.171900071504754060, 7.469564292951421436, -0.7216878364870267237 ) ) ;
#46495 = CARTESIAN_POINT ( 'NONE',  ( 6.262596564776618635, -1.532251275270900326, 1.525113613579494709 ) ) ;
#46497 = ORIENTED_EDGE ( 'NONE', *, *, #47186, .T. ) ;
#46496 = CARTESIAN_POINT ( 'NONE',  ( -0.2104748580754183807, 4.084054299358617079, -2.658391380015924010 ) ) ;
#46498 = CARTESIAN_POINT ( 'NONE',  ( -1.364683531250012516, 4.988541667008084879, -0.7879004041258300672 ) ) ;
#46499 = CARTESIAN_POINT ( 'NONE',  ( 0.1806930697454533219, -0.1309388314422038346, -1.840455529407057256 ) ) ;
#46500 = CARTESIAN_POINT ( 'NONE',  ( 6.679014442879065427, -0.8212242018711314318, -1.526972759001248514 ) ) ;
#46501 = VECTOR ( 'NONE', #140994, 1000.000000000000000 ) ;
#46503 = CARTESIAN_POINT ( 'NONE',  ( 2.630644284709309666, 0.2711686948545319886, 2.174668582101045633 ) ) ;
#46502 = CARTESIAN_POINT ( 'NONE',  ( -3.755786496842897795E-14, 1.078125000341431106, -1.570758158831814466 ) ) ;
#46504 = CARTESIAN_POINT ( 'NONE',  ( 3.346982425237558179, 0.5585957852003355928, 2.238849765380794832 ) ) ;
#46505 = CARTESIAN_POINT ( 'NONE',  ( 6.292271403379039896, -2.050439857688883372, -0.2063938634464974886 ) ) ;
#46506 = CARTESIAN_POINT ( 'NONE',  ( 0.9549039013059671399, 0.3793949951976150481, -1.904366508208689357 ) ) ;
#46507 = B_SPLINE_CURVE_WITH_KNOTS ( 'NONE', 3,
 ( #60789, #112812, #75975, #25078, #160424, #43501 ),
 .UNSPECIFIED., .F., .F.,
 ( 4, 2, 4 ),
 ( 0.000000000000000000, 0.0003205138222656014457, 0.0006410276445312028913 ),
 .UNSPECIFIED. ) ;
#46509 = EDGE_CURVE ( 'NONE', #190376, #146171, #58158, .T. ) ;
#46508 = CARTESIAN_POINT ( 'NONE',  ( -6.873620692004104527, 7.121571683533994168, 0.7216878364870317197 ) ) ;
#46510 = DIRECTION ( 'NONE',  ( 0.000000000000000000, 0.000000000000000000, 1.000000000000000000 ) ) ;
#46511 = CARTESIAN_POINT ( 'NONE',  ( 3.920270587443940080, -2.114697630030224929, 0.1593259359235904837 ) ) ;
#46512 =( LENGTH_UNIT ( ) NAMED_UNIT ( * ) SI_UNIT ( .MILLI., .METRE. ) );
#46513 = CARTESIAN_POINT ( 'NONE',  ( 2.690077459517980163, 1.704938782060089864, 1.076316768488336351 ) ) ;
#46514 = CARTESIAN_POINT ( 'NONE',  ( -6.385527161912131433, 6.552129231760014605, 0.7216878364870317197 ) ) ;
#46515 = CARTESIAN_POINT ( 'NONE',  ( 4.014836333542094238, 1.562590183666902943, -1.558512549626612342 ) ) ;
#46516 = PLANE ( 'NONE',  #32274 ) ;
#46517 = CARTESIAN_POINT ( 'NONE',  ( -2.446432203289806484, -3.110604623059922247, -2.379386263155008674 ) ) ;
#46518 = CIRCLE ( 'NONE', #153805, 0.1000000000000000333 ) ;
#46519 = CARTESIAN_POINT ( 'NONE',  ( 0.3635304476994546952, 1.806310985241452949, -0.2645042207462811046 ) ) ;
#46520 = CARTESIAN_POINT ( 'NONE',  ( -6.563028877466991595, 9.814561569423593923, 1.199719254218452935 ) ) ;
#46522 = CARTESIAN_POINT ( 'NONE',  ( 0.000000000000000000, 6.999999999999999112, 0.000000000000000000 ) ) ;
#46521 = CARTESIAN_POINT ( 'NONE',  ( -4.601933621211449221, 8.477299672830683974, 0.2703350597391823706 ) ) ;
#46523 = CARTESIAN_POINT ( 'NONE',  ( -9.470186914265017464, 4.005096909781187264, 6.837150237413082365 ) ) ;
#46524 = VERTEX_POINT ( 'NONE', #189131 ) ;
#46525 = CARTESIAN_POINT ( 'NONE',  ( 4.961820856888925491, 2.038780864349061250, -0.3001439806698430468 ) ) ;
#46526 = FACE_OUTER_BOUND ( 'NONE', #169309, .T. ) ;
#46527 = EDGE_CURVE ( 'NONE', #55695, #166004, #6154, .T. ) ;
#46528 = CARTESIAN_POINT ( 'NONE',  ( -0.03919461954072858689, -7.818966704647663413, 9.500338091956020747 ) ) ;
#46529 = CARTESIAN_POINT ( 'NONE',  ( -5.901876940650454095, 5.779944607047298177, -0.7998128361456291469 ) ) ;
#46530 = CARTESIAN_POINT ( 'NONE',  ( -3.481411583659053566, 7.283673624236017830, 0.000000000000000000 ) ) ;
#46531 = CARTESIAN_POINT ( 'NONE',  ( 3.281903422188407138, 1.969933747823931380, -0.4446889725447465413 ) ) ;
#46532 = CARTESIAN_POINT ( 'NONE',  ( -1.402160292154681736E-14, 0.3375000000000208389, -1.732050807568870754 ) ) ;
#46534 = CARTESIAN_POINT ( 'NONE',  ( 7.944714827928039291, 11.25228915168265864, 1.082531754730557072 ) ) ;
#46533 = CARTESIAN_POINT ( 'NONE',  ( -5.276058054373441664, 6.184431147304315424, -1.199719254218453823 ) ) ;
#46535 = CARTESIAN_POINT ( 'NONE',  ( 6.283314124929436417, 9.417951348137970413, -1.199719254218440723 ) ) ;
#46536 = CARTESIAN_POINT ( 'NONE',  ( 3.538010501442095723, 0.9279861380482921085, -1.840221436749614803 ) ) ;
#46537 = CARTESIAN_POINT ( 'NONE',  ( 3.270157880292836605, 1.821742160604752137, -0.8647241845514612724 ) ) ;
#46538 = CARTESIAN_POINT ( 'NONE',  ( 1.886017674307032266, 3.298060805577429644, -0.4014564593431638739 ) ) ;
#46539 = CARTESIAN_POINT ( 'NONE',  ( 6.491656622844908853, 6.468020902940851968, 0.7998128361456341429 ) ) ;
#46540 = CARTESIAN_POINT ( 'NONE',  ( -11.41381675112453564, 10.06994333910004613, 3.704697986577180302 ) ) ;
#46541 = CARTESIAN_POINT ( 'NONE',  ( 2.759138561942891421, -2.010518527590241966, -0.1511176148010634768 ) ) ;
#46543 = AXIS2_PLACEMENT_3D ( 'NONE', #102595, #168651, #86339 ) ;
#46542 = CARTESIAN_POINT ( 'NONE',  ( 1.359045109759978498, 1.814150759811587355, -0.3131490413979670651 ) ) ;
#46544 = CARTESIAN_POINT ( 'NONE',  ( 0.3820104410975051490, 2.150944695799131612, -0.8364647861166041309 ) ) ;
#46545 = CARTESIAN_POINT ( 'NONE',  ( 6.398522151006641678, 6.429640362454684954, 0.000000000000000000 ) ) ;
#46546 = CARTESIAN_POINT ( 'NONE',  ( 2.671339989782473001, 0.1089736159370843782, -2.158987078831893669 ) ) ;
#46547 = CARTESIAN_POINT ( 'NONE',  ( -3.877268743828284681, 5.546566172598190292, 1.443375672974064550 ) ) ;
#46548 = CARTESIAN_POINT ( 'NONE',  ( 4.522735144945882801, 0.3654406173194921781, 2.085432885242066270 ) ) ;
#46549 = CARTESIAN_POINT ( 'NONE',  ( 0.1377316631404259251, 3.380484790530137840, -2.074674412079231089 ) ) ;
#46550 = CARTESIAN_POINT ( 'NONE',  ( 0.6900581440293825919, -1.856003987442723657, -0.2331820809091043056 ) ) ;
#46551 = ADVANCED_FACE ( 'NONE', ( #141502 ), #207510, .F. ) ;
#46552 = CARTESIAN_POINT ( 'NONE',  ( 4.803572714498323570, -0.5265354887679043472, 1.899778226852407936 ) ) ;
#46553 = AXIS2_PLACEMENT_3D ( 'NONE', #174655, #9981, #59806 ) ;
#46555 = CARTESIAN_POINT ( 'NONE',  ( 7.727784369665023689, 11.95957283134381477, 1.040834085586084257E-14 ) ) ;
#46554 = CARTESIAN_POINT ( 'NONE',  ( 0.6823417656249899377, 2.842708333674753618, 1.181850606188765695 ) ) ;
#46557 = CARTESIAN_POINT ( 'NONE',  ( 6.006491595720174104, -0.7565722652288708883, -1.965664901909335738 ) ) ;
#46556 = CARTESIAN_POINT ( 'NONE',  ( -5.768104287610143821, 8.816873204598778102, -1.199719254218440723 ) ) ;
#46558 = CARTESIAN_POINT ( 'NONE',  ( 6.478973898625433492, 1.930320082341809629, 0.7489585856828018251 ) ) ;
#46559 = CARTESIAN_POINT ( 'NONE',  ( 6.144869935491714230, 8.192100896205568361, -1.599625672291262513 ) ) ;
#46560 = CARTESIAN_POINT ( 'NONE',  ( -6.307567778855718288, 8.381915046796901692, -1.599625672291263179 ) ) ;
#46561 = CARTESIAN_POINT ( 'NONE',  ( 6.539320575229276677, 6.035451701470580410, 2.698157228745074576 ) ) ;
#46562 = CARTESIAN_POINT ( 'NONE',  ( 5.260604563723265237, -1.428518960016441186, 1.358918391201448417 ) ) ;
#46563 = CARTESIAN_POINT ( 'NONE',  ( 6.047130097259819870, 0.2019483658235003143, 2.009690058136243351 ) ) ;
#46564 = CARTESIAN_POINT ( 'NONE',  ( 1.499999999999989120, 0.5562500006828161592, 0.000000000000000000 ) ) ;
#46565 = CARTESIAN_POINT ( 'NONE',  ( 4.512551404143492206, -0.9841529367882025925, -2.087457756972084244 ) ) ;
#46566 = VECTOR ( 'NONE', #47181, 1000.000000000000000 ) ;
#46567 = CARTESIAN_POINT ( 'NONE',  ( 1.780209297579591565, -1.142364670758776013, -1.717135550327288485 ) ) ;
#46568 = CARTESIAN_POINT ( 'NONE',  ( 6.887178846062110615, 9.058127958537705027, -1.443375672974057666 ) ) ;
#46569 = CARTESIAN_POINT ( 'NONE',  ( 6.540882763950133238, 6.595727744222092959, 0.000000000000000000 ) ) ;
#46570 = CARTESIAN_POINT ( 'NONE',  ( 4.736594563127852098, 6.619389305106191834, -1.599625672291273171 ) ) ;
#46571 = CARTESIAN_POINT ( 'NONE',  ( -0.6823417656250003738, 2.530208333674753618, -1.181850606188749264 ) ) ;
#46572 = CARTESIAN_POINT ( 'NONE',  ( -3.007794483472536307, 14.52974340527628527, 11.62584731636876789 ) ) ;
#46573 = CARTESIAN_POINT ( 'NONE',  ( 6.331294547457450683, 7.449227062530913379, -1.082531754730543083 ) ) ;
#46574 = CARTESIAN_POINT ( 'NONE',  ( 3.930270145471780996, 1.203169952209550919, 1.807132499170207351 ) ) ;
#46575 = DIRECTION ( 'NONE',  ( 0.7592566023653005702, 0.6507913734559639396, 0.000000000000000000 ) ) ;
#46577 = CARTESIAN_POINT ( 'NONE',  ( 3.966218424140379728, -1.719484690100345325, -0.6589542199007536460 ) ) ;
#46576 = CARTESIAN_POINT ( 'NONE',  ( -4.948362879307902418, 4.875437568721725512, 1.214306433183764966E-14 ) ) ;
#46579 = FACE_BOUND ( 'NONE', #104372, .T. ) ;
#46578 = CARTESIAN_POINT ( 'NONE',  ( -0.6823417656249969321, 4.467708333674755394, -1.181850606188749264 ) ) ;
#46580 = CARTESIAN_POINT ( 'NONE',  ( 5.970311429539967740, -2.080533979117826782, -0.6889730390344513955 ) ) ;
#46581 = CARTESIAN_POINT ( 'NONE',  ( -11.01135777277262129, 12.69999999999998153, 1.399999999999998579 ) ) ;
#46582 = CARTESIAN_POINT ( 'NONE',  ( 6.086863830973287648, -0.3249354738291005407, -2.238958312302678610 ) ) ;
#46583 = ORIENTED_EDGE ( 'NONE', *, *, #97341, .F. ) ;
#46584 = CARTESIAN_POINT ( 'NONE',  ( -4.764280463835226520, 6.994423760310605864, -1.426210198329436851 ) ) ;
#46585 = CARTESIAN_POINT ( 'NONE',  ( 5.502223863662048409, 7.574938096329499437, 1.338028725624084148 ) ) ;
#46586 = CARTESIAN_POINT ( 'NONE',  ( -4.611181641979265500, 8.393812659035525314, 0.000000000000000000 ) ) ;
#46587 = CARTESIAN_POINT ( 'NONE',  ( 3.851925040058331806, 5.587274861525073355, -1.443375672974066548 ) ) ;
#46588 = CARTESIAN_POINT ( 'NONE',  ( 1.164531557977426912, -1.597865870565655877, -0.7613500884297589311 ) ) ;
#46589 = CARTESIAN_POINT ( 'NONE',  ( 4.723295704472612044, 1.752545568416422173, 0.9903661003969994603 ) ) ;
#46590 = CARTESIAN_POINT ( 'NONE',  ( 7.644099680006512187, 7.812537802962739697, 1.040834085586084257E-14 ) ) ;
#46591 = CARTESIAN_POINT ( 'NONE',  ( 4.049914914165038127, 0.7116930038560628224, -1.982186593211773706 ) ) ;
#46592 = CARTESIAN_POINT ( 'NONE',  ( 2.231924035814872642, 1.915248681264541508, 0.04463030589317053265 ) ) ;
#46593 = CARTESIAN_POINT ( 'NONE',  ( 4.695201269034174452, 4.372156323494968966, 1.214306433183764966E-14 ) ) ;
#46594 = CARTESIAN_POINT ( 'NONE',  ( 3.402753045726066183, 0.4761229057644749130, 1.911014528907057697 ) ) ;
#46595 = CARTESIAN_POINT ( 'NONE',  ( 5.924083597509600452, -2.004057273996622701, 0.2512124657789679971 ) ) ;
#46596 = CARTESIAN_POINT ( 'NONE',  ( 1.990876257202532695, 1.628914321797021669, -0.9196232060951770038 ) ) ;
#46597 = CARTESIAN_POINT ( 'NONE',  ( 1.890992312513404716, 0.1891058464698439912, 1.952711869325058691 ) ) ;
#46600 = ORIENTED_EDGE ( 'NONE', *, *, #128539, .T. ) ;
#46599 = CARTESIAN_POINT ( 'NONE',  ( 1.529408426332915960, -0.2309274165002393187, 1.898302859121250297 ) ) ;
#46598 = CARTESIAN_POINT ( 'NONE',  ( 4.107791765966132047, -1.720061694268668395, 0.1296855704675456133 ) ) ;
#46602 = CARTESIAN_POINT ( 'NONE',  ( 6.168596704537822717, 6.299043698156668647, 1.040834085586084257E-14 ) ) ;
#46601 = CARTESIAN_POINT ( 'NONE',  ( 1.243116305521356990, 0.4334984505205765060, 2.163720904216937857 ) ) ;
#46603 = CARTESIAN_POINT ( 'NONE',  ( -0.6823417656250212460, 1.613541667008083769, 1.181850606188755259 ) ) ;
#46604 = CARTESIAN_POINT ( 'NONE',  ( 7.404724451357931336, 11.79059562655963056, 0.7998128361456462443 ) ) ;
#46605 = CARTESIAN_POINT ( 'NONE',  ( 4.182432031930847440E-16, 4.000000000000001776, -2.350000000000007194 ) ) ;
#46606 = CARTESIAN_POINT ( 'NONE',  ( 0.000000000000000000, 11.29999999999998117, 0.000000000000000000 ) ) ;
#46607 = CARTESIAN_POINT ( 'NONE',  ( -5.199715606040888005, 6.025088614257851027, -1.199719254218446718 ) ) ;
#46608 = CARTESIAN_POINT ( 'NONE',  ( 6.543811353064236336, 1.423268159695538326, 1.503672778047180136 ) ) ;
#46609 = CARTESIAN_POINT ( 'NONE',  ( 0.3618904354094238385, -0.5536326762660361833, 1.994880328902041589 ) ) ;
#46610 = CARTESIAN_POINT ( 'NONE',  ( 0.7499999999999902300, 2.233333333333351156, 1.299038105676669330 ) ) ;
#46611 = CARTESIAN_POINT ( 'NONE',  ( 6.693975156845185737, 8.832723654451292816, 1.599625672291281386 ) ) ;
#46612 = CARTESIAN_POINT ( 'NONE',  ( -8.850775351622791831, 9.220326086515070685, -0.7998128361456291469 ) ) ;
#46613 = CARTESIAN_POINT ( 'NONE',  ( 6.066347387471824781, 6.042103138330730872, -0.7998128361456481317 ) ) ;
#46614 = CARTESIAN_POINT ( 'NONE',  ( 5.637388408723053246, -0.05200288984260474645, 2.120005899716829401 ) ) ;
#46615 = CARTESIAN_POINT ( 'NONE',  ( 3.562760505341037831, 7.378580699531681830, -1.734723475976807094E-15 ) ) ;
#46616 = CARTESIAN_POINT ( 'NONE',  ( -0.6823417656250212460, 2.551041667008084435, 1.181850606188767472 ) ) ;
#46617 = ORIENTED_EDGE ( 'NONE', *, *, #140381, .F. ) ;
#46618 = CARTESIAN_POINT ( 'NONE',  ( -0.7499999999999972244, 3.608333333333359150, -1.299038105676652011 ) ) ;
#46620 = CARTESIAN_POINT ( 'NONE',  ( 2.184835310096557404, 5.700724961754617404, 1.040834085586084257E-14 ) ) ;
#46619 = CARTESIAN_POINT ( 'NONE',  ( 6.725062055625550705, -1.793239977796506457, -0.7961783947641184467 ) ) ;
#46621 = CARTESIAN_POINT ( 'NONE',  ( 3.919295934624257960, 0.7230291454519314209, 1.882185965797255278 ) ) ;
#46622 = CARTESIAN_POINT ( 'NONE',  ( 3.098755142807321672, 1.734096097442457518, 0.8144269386064789673 ) ) ;
#46623 = CARTESIAN_POINT ( 'NONE',  ( 1.347511689332027807, 0.6317163119916607839, -2.098556723903362009 ) ) ;
#46624 = CARTESIAN_POINT ( 'NONE',  ( -0.7500000000000215383, 1.222916667349485564, 1.299038105676659116 ) ) ;
#46625 = CARTESIAN_POINT ( 'NONE',  ( 5.238544184099147571, 1.195677241517135281, -1.619561112405358827 ) ) ;
#46626 = CARTESIAN_POINT ( 'NONE',  ( -7.369020184227459858, 8.555943955475521889, 1.199719254218450271 ) ) ;
#46628 = CARTESIAN_POINT ( 'NONE',  ( 5.853141746508254251, 0.1553614259057617408, -2.111562834372962438 ) ) ;
#46627 = CARTESIAN_POINT ( 'NONE',  ( -3.226477370372317743, 4.787309570232886280, 1.443375672974064550 ) ) ;
#46629 = CARTESIAN_POINT ( 'NONE',  ( 1.364683531249996529, 8.526041667008065872, 0.7879004041258405033 ) ) ;
#46631 = CARTESIAN_POINT ( 'NONE',  ( -8.093291352714894415, 8.406871097780989288, -0.7998128361456362523 ) ) ;
#46630 = CARTESIAN_POINT ( 'NONE',  ( 3.509396081178951743, -2.059435208860632915, 0.3595599189689518416 ) ) ;
#46633 = EDGE_LOOP ( 'NONE', ( #20250, #159314, #154609, #4664 ) ) ;
#46632 = CARTESIAN_POINT ( 'NONE',  ( 2.274029058727170316, -1.063862581237082550, 1.357477553621669442 ) ) ;
#46634 = CARTESIAN_POINT ( 'NONE',  ( 5.502226937873657242, -0.9515977829631333540, 1.895136135177949877 ) ) ;
#46635 = CARTESIAN_POINT ( 'NONE',  ( 4.449046963578762615, 8.342305224150557308, -0.7998128361456231517 ) ) ;
#46636 = CARTESIAN_POINT ( 'NONE',  ( -1.434937167926458423, 13.25321981955314143, 0.4065227821781826623 ) ) ;
#46637 = CARTESIAN_POINT ( 'NONE',  ( 7.401194801146942837, -6.836289462023670715, 7.952857047016752112 ) ) ;
#46638 = FACE_OUTER_BOUND ( 'NONE', #108779, .T. ) ;
#46639 = CARTESIAN_POINT ( 'NONE',  ( 6.470265622219697477, 8.571729197388226140, -1.599625672291262513 ) ) ;
#46640 = ORIENTED_EDGE ( 'NONE', *, *, #165017, .F. ) ;
#46641 = CARTESIAN_POINT ( 'NONE',  ( -1.115562610750309283E-14, 9.562500000000000000, 1.500000000000001554 ) ) ;
#46642 = ORIENTED_EDGE ( 'NONE', *, *, #156015, .T. ) ;
#46644 = CARTESIAN_POINT ( 'NONE',  ( 1.681973674898680216, 0.9313724848135003231, 1.553549296804368707 ) ) ;
#46643 = CARTESIAN_POINT ( 'NONE',  ( 6.866278450678116485, 6.975356045404744521, 0.000000000000000000 ) ) ;
#46645 = CARTESIAN_POINT ( 'NONE',  ( -6.235860587281615075, 9.362588887548838557, -1.199719254218440723 ) ) ;
#46646 = ORIENTED_EDGE ( 'NONE', *, *, #104111, .T. ) ;
#46647 = CARTESIAN_POINT ( 'NONE',  ( 3.999819011231439347, 4.625209253646830554, 1.199719254218464037 ) ) ;
#46648 = VERTEX_POINT ( 'NONE', #29846 ) ;
#46649 = CARTESIAN_POINT ( 'NONE',  ( 5.091969210384201361, 8.098325291160362482, 1.199719254218452047 ) ) ;
#46650 = CARTESIAN_POINT ( 'NONE',  ( 2.191808917380858812, 1.115356421127197351, 1.427258924012535735 ) ) ;
#46651 = CARTESIAN_POINT ( 'NONE',  ( 6.539320575229249144, 0.007148032025052972194, 1.896977914940492393 ) ) ;
#46652 = FACE_OUTER_BOUND ( 'NONE', #165548, .T. ) ;
#46653 = CARTESIAN_POINT ( 'NONE',  ( 4.722716239034094876, 6.809985054512954328, 1.237095216770202954 ) ) ;
#46654 = ORIENTED_EDGE ( 'NONE', *, *, #14059, .F. ) ;
#46655 = EDGE_CURVE ( 'NONE', #122458, #167565, #73298, .T. ) ;
#46656 = CARTESIAN_POINT ( 'NONE',  ( 4.140933978860473985, -0.1807793374023874688, -1.852226635870577898 ) ) ;
#46657 = CARTESIAN_POINT ( 'NONE',  ( 1.511203358410578179, -1.803099835331838818, 0.6471475864035965975 ) ) ;
#46658 = CARTESIAN_POINT ( 'NONE',  ( 0.1998643617870856648, -1.825052844667142349, -0.05062755788937112200 ) ) ;
#46659 = AXIS2_PLACEMENT_3D ( 'NONE', #175370, #142892, #156987 ) ;
#46660 = CARTESIAN_POINT ( 'NONE',  ( 1.408069224121391017, 4.235466930450527023, -0.5223881139200245993 ) ) ;
#46661 = CARTESIAN_POINT ( 'NONE',  ( -4.624739795592936353, 7.449261290616792763, -1.082531754730549967 ) ) ;
#46662 = CARTESIAN_POINT ( 'NONE',  ( 4.600487305768355739, 8.366733224642864286, -0.1591645125929436189 ) ) ;
#46663 = CARTESIAN_POINT ( 'NONE',  ( -2.643476764984671767, 6.027880625883323518, 1.040834085586084257E-14 ) ) ;
#46664 = CARTESIAN_POINT ( 'NONE',  ( 8.026063749610047537, 10.38682701267698150, -1.443375672974057666 ) ) ;
#46665 = CARTESIAN_POINT ( 'NONE',  ( 5.119951519371389814, 1.948576354197928628, -0.2848888285253112218 ) ) ;
#46666 = CARTESIAN_POINT ( 'NONE',  ( -4.608882153641705059, 7.464447381635583412, -1.199719254218452047 ) ) ;
#46667 = FACE_OUTER_BOUND ( 'NONE', #201122, .T. ) ;
#46668 = CARTESIAN_POINT ( 'NONE',  ( 6.720655732516648939, -0.004400176169771368405, 2.173773060281408487 ) ) ;
#46669 = FACE_OUTER_BOUND ( 'NONE', #12489, .T. ) ;
#46670 = CARTESIAN_POINT ( 'NONE',  ( 5.438475939130889891, 1.897888883619626821, 0.3293186976999362137 ) ) ;
#46671 = CARTESIAN_POINT ( 'NONE',  ( -6.507023659554960204, 9.678945805201045971, 1.199719254218452047 ) ) ;
#46672 = CARTESIAN_POINT ( 'NONE',  ( 1.430379662499326354, 1.758314708518812663, 0.4907259477668829972 ) ) ;
#46673 = CARTESIAN_POINT ( 'NONE',  ( 2.420803835572300500, 1.440536793087299205, -1.671967039616916617 ) ) ;
#46674 = CARTESIAN_POINT ( 'NONE',  ( -6.305084897752638362, 6.885715524493735806, 0.7263500631976427258 ) ) ;
#46675 = CARTESIAN_POINT ( 'NONE',  ( 0.3516297456669579269, -1.353986107606550471, -1.350798769753497552 ) ) ;
#46676 = ORIENTED_EDGE ( 'NONE', *, *, #76035, .F. ) ;
#46677 =( BOUNDED_SURFACE ( )  B_SPLINE_SURFACE ( 3, 2, ( 
 ( #122285, #24673, #204474 ),
 ( #155765, #52917, #86488 ),
 ( #88638, #22529, #36659 ),
 ( #57194, #137390, #55059 ),
 ( #70208, #102744, #121210 ),
 ( #168800, #173092, #156841 ),
 ( #152552, #136320, #202338 ),
 ( #153630, #53991, #187179 ) ),
 .UNSPECIFIED., .F., .F., .F. ) 
 B_SPLINE_SURFACE_WITH_KNOTS ( ( 4, 2, 2, 4 ),
 ( 3, 3 ),
 ( 0.000000000000000000, 0.003135730046001661882, 0.004703595069002492607, 0.006271460092003323765 ),
 ( 0.000000000000000000, 1.000000000000000000 ),
 .UNSPECIFIED. ) 
 GEOMETRIC_REPRESENTATION_ITEM ( )  RATIONAL_B_SPLINE_SURFACE ( (
 ( 1.000000000000000000, 0.7762074382822415908, 1.000000000000000000),
 ( 1.000000000000000000, 0.7833603871956243969, 1.000000000000000000),
 ( 1.000000000000000000, 0.7921476697835092562, 1.000000000000000000),
 ( 1.000000000000000000, 0.8128220030700816778, 1.000000000000000000),
 ( 1.000000000000000000, 0.8210052159720273579, 1.000000000000000000),
 ( 1.000000000000000000, 0.8412342355963777774, 1.000000000000000000),
 ( 1.000000000000000000, 0.8534349975675549205, 1.000000000000000000),
 ( 1.000000000000000000, 0.8671614222306939235, 1.000000000000000000) ) ) 
 REPRESENTATION_ITEM ( '' )  SURFACE ( )  );
#46678 = CIRCLE ( 'NONE', #139923, 0.05000000000000002359 ) ;
#46679 = ORIENTED_EDGE ( 'NONE', *, *, #40952, .F. ) ;
#46680 = CARTESIAN_POINT ( 'NONE',  ( 0.5374760852590576565, 1.839023226330655625, -0.7055796775109841601 ) ) ;
#46681 = CARTESIAN_POINT ( 'NONE',  ( 1.434995430731567101, -1.407912642168735573, -1.337921467293776923 ) ) ;
#46682 = ORIENTED_EDGE ( 'NONE', *, *, #72282, .F. ) ;
#46683 = CARTESIAN_POINT ( 'NONE',  ( 1.054064285791616262, 1.779355684154381834, -0.9478921834336280217 ) ) ;
#46685 = CARTESIAN_POINT ( 'NONE',  ( 6.016418624437367413, 0.7528656616105857680, 1.702022903989255376 ) ) ;
#46684 = CARTESIAN_POINT ( 'NONE',  ( -6.414942957921379474, 7.513130201443591005, -1.199719254218452047 ) ) ;
#46686 = CARTESIAN_POINT ( 'NONE',  ( 6.561219994370630637, 6.619454513046008515, 0.000000000000000000 ) ) ;
#46687 = B_SPLINE_CURVE_WITH_KNOTS ( 'NONE', 3,
 ( #66759, #179504, #150200, #19100 ),
 .UNSPECIFIED., .F., .F.,
 ( 4, 4 ),
 ( 2.884874348012686430E-17, 0.0001292189244443286045 ),
 .UNSPECIFIED. ) ;
#46688 = CARTESIAN_POINT ( 'NONE',  ( -1.436838838544729491, 7.449283400311743186, -4.203727439823575551 ) ) ;
#46689 = DIRECTION ( 'NONE',  ( 0.000000000000000000, -1.000000000000000000, 0.000000000000000000 ) ) ;
#46690 = CARTESIAN_POINT ( 'NONE',  ( -5.229694566569281555, 7.124396299129368337, 1.599625672291267398 ) ) ;
#46691 = CARTESIAN_POINT ( 'NONE',  ( -7.923814432544069142, 8.209148024248356990, 0.000000000000000000 ) ) ;
#46692 = CARTESIAN_POINT ( 'NONE',  ( 1.927518781310177509, -1.434474475899261581, -1.656937093973806396 ) ) ;
#46693 = CARTESIAN_POINT ( 'NONE',  ( 4.528060117284240071, 5.345453560662148718, 1.082531754730560403 ) ) ;
#46694 = CARTESIAN_POINT ( 'NONE',  ( 6.339319342841494453, 9.553567112360518365, -1.199719254218452047 ) ) ;
#46696 =( BOUNDED_CURVE ( )  B_SPLINE_CURVE ( 1, ( #38100, #151858 ),
 .UNSPECIFIED., .F., .T. ) 
 B_SPLINE_CURVE_WITH_KNOTS ( ( 2, 2 ),
 ( 0.000000000000000000, 6.249999999999788711E-05 ),
 .UNSPECIFIED. ) 
 CURVE ( )  GEOMETRIC_REPRESENTATION_ITEM ( )  RATIONAL_B_SPLINE_CURVE ( ( 0.9345202395942817652, 0.9345202395942817652 ) ) 
 REPRESENTATION_ITEM ( '' )  );
#46695 = CARTESIAN_POINT ( 'NONE',  ( -1.420000000000001039, 6.280000000000042881, -2.579999999999995630 ) ) ;
#46697 = CARTESIAN_POINT ( 'NONE',  ( 1.189776066567624691, -0.8228614858879386151, 1.629801898503015156 ) ) ;
#46698 = CARTESIAN_POINT ( 'NONE',  ( -3.297657676621885692, 4.870353260857385180, 1.599625672291267398 ) ) ;
#46699 = CARTESIAN_POINT ( 'NONE',  ( -6.581660514134937578, 6.779899958900003298, -0.3344319070191399401 ) ) ;
#46700 = CARTESIAN_POINT ( 'NONE',  ( 6.509000000000014552, 2.444259026362519904, 2.383015625331697862 ) ) ;
#46701 = AXIS2_PLACEMENT_3D ( 'NONE', #13813, #113534, #114598 ) ;
#46702 = CARTESIAN_POINT ( 'NONE',  ( 9.348510611822643313, 10.86534945433664134, 1.199719254218453823 ) ) ;
#46704 = EDGE_CURVE ( 'NONE', #42744, #204603, #27071, .T. ) ;
#46703 = CARTESIAN_POINT ( 'NONE',  ( 1.453605159173555705, 0.5596597320992221514, -1.843422129977128954 ) ) ;
#46705 = CARTESIAN_POINT ( 'NONE',  ( 3.942202469084721272, -0.9707516781715104237, 1.704694321266352786 ) ) ;
#46706 = CARTESIAN_POINT ( 'NONE',  ( -7.004758919754800139, 11.32396917302262018, 0.000000000000000000 ) ) ;
#46707 = CARTESIAN_POINT ( 'NONE',  ( 4.635998460869027227, 7.496083073400806818, -1.199719254218452047 ) ) ;
#46708 = CARTESIAN_POINT ( 'NONE',  ( 4.599289333468261631, -0.5842463895667610041, 2.112197083089427885 ) ) ;
#46709 = AXIS2_PLACEMENT_3D ( 'NONE', #39397, #154218, #55643 ) ;
#46710 = CARTESIAN_POINT ( 'NONE',  ( 3.337278367258157630, 7.045241861776501580, 0.7998128361456341429 ) ) ;
#46711 = EDGE_CURVE ( 'NONE', #118245, #53554, #205282, .T. ) ;
#46712 = CARTESIAN_POINT ( 'NONE',  ( 4.364170320198999420, -2.065056620294950740, 0.1471644388686063065 ) ) ;
#46714 = CARTESIAN_POINT ( 'NONE',  ( 1.364683531249988757, 1.696875000341414808, 0.000000000000000000 ) ) ;
#46713 = CARTESIAN_POINT ( 'NONE',  ( 3.599450258230072475, 3.565770338845029919, 2.499999999999999112 ) ) ;
#46715 = EDGE_LOOP ( 'NONE', ( #129430, #30648, #128488, #88463 ) ) ;
#46716 = CARTESIAN_POINT ( 'NONE',  ( 3.481312804724666421, -2.296076454524886845, -0.1115701876132721843 ) ) ;
#46718 = ORIENTED_EDGE ( 'NONE', *, *, #33948, .F. ) ;
#46717 = CARTESIAN_POINT ( 'NONE',  ( 7.293923454472080792, 9.532663335016016148, 1.443375672974076540 ) ) ;
#46720 = CARTESIAN_POINT ( 'NONE',  ( 3.285556943750000070, -0.9843749995220412163, 0.000000000000000000 ) ) ;
#46719 = CARTESIAN_POINT ( 'NONE',  ( 7.051649292883499953, 7.399548061218447437, -0.7216878364870317197 ) ) ;
#46721 = CARTESIAN_POINT ( 'NONE',  ( -7.583532603600728450, -5.197284395437328897, -7.968353659517138254 ) ) ;
#46722 = CARTESIAN_POINT ( 'NONE',  ( -9.984480469316341811, 4.552642677847350328, -6.658573114549724892 ) ) ;
#46723 = CARTESIAN_POINT ( 'NONE',  ( 3.363160477839432172, 1.894460165981373789, -0.4261612883773926441 ) ) ;
#46724 = ORIENTED_EDGE ( 'NONE', *, *, #166817, .T. ) ;
#46726 = CARTESIAN_POINT ( 'NONE',  ( 0.07933194154487849259, -9.746166700180788567, 9.499668754385625746 ) ) ;
#46725 = PRESENTATION_LAYER_ASSIGNMENT (  '', '', ( #140119 ) ) ;
#46727 = CARTESIAN_POINT ( 'NONE',  ( 4.869353489999923568, -1.618680692612521455, -1.018082601613921723 ) ) ;
#46728 = CARTESIAN_POINT ( 'NONE',  ( 7.065207446497155708, 9.336104335703744539, 0.000000000000000000 ) ) ;
#46729 = CARTESIAN_POINT ( 'NONE',  ( 5.684504558281781250, -1.683600953293447944, -0.3737579273616030706 ) ) ;
#46730 = CARTESIAN_POINT ( 'NONE',  ( 4.628138809701114020, 2.011451458044950069, 0.1435230606586651581 ) ) ;
#46731 = CARTESIAN_POINT ( 'NONE',  ( 5.168667805954368255, 1.541955118739355424, 1.704926945024546336 ) ) ;
#46732 = CARTESIAN_POINT ( 'NONE',  ( -0.7500000000000179856, 9.791666666666671404, 1.299038105676658228 ) ) ;
#46733 = CARTESIAN_POINT ( 'NONE',  ( 0.9091299924109221831, 1.668792687453458878, -1.444214864661397035 ) ) ;
#46735 = CARTESIAN_POINT ( 'NONE',  ( -4.421367491832313590, 6.251624388594711590, 1.443375672974065660 ) ) ;
#46734 = CARTESIAN_POINT ( 'NONE',  ( -10.65400978224035811, 11.32409958890225710, 1.040834085586084257E-14 ) ) ;
#46736 = CARTESIAN_POINT ( 'NONE',  ( 0.3030915354301273457, -0.4787081777068747934, 1.703804975073195394 ) ) ;
#46737 = CARTESIAN_POINT ( 'NONE',  ( 6.065077313367789102, -1.076319894221990259, 1.704936797084610101 ) ) ;
#46739 = CARTESIAN_POINT ( 'NONE',  ( 2.853816628688166990, 2.281129249179119078, -0.2256723309681916978 ) ) ;
#46738 = CARTESIAN_POINT ( 'NONE',  ( 4.227110032410640095, 8.153655147779589996, 0.7998128361456271485 ) ) ;
#46740 = CARTESIAN_POINT ( 'NONE',  ( 1.130330966444204277, -1.574854822160208556, 0.7409792249596267588 ) ) ;
#46741 = CARTESIAN_POINT ( 'NONE',  ( 2.011244508837064071, -3.469446951953614189E-15, 0.2971265334020881110 ) ) ;
#46742 = CARTESIAN_POINT ( 'NONE',  ( 1.563399581876812716, 1.420944641023152322, -0.9932112465018216874 ) ) ;
#46743 = CARTESIAN_POINT ( 'NONE',  ( 0.6801582343749726922, 0.7552083336747339448, 1.178068619123784355 ) ) ;
#46744 = CARTESIAN_POINT ( 'NONE',  ( -11.89942855770813956, 13.79999999999999893, -0.7000000000000009548 ) ) ;
#46745 = CARTESIAN_POINT ( 'NONE',  ( 1.539757937649718800, 2.006347644133343433, -0.8302594476135690682 ) ) ;
#46746 = CARTESIAN_POINT ( 'NONE',  ( 2.817592499383800853, -1.357869084745389809, -1.490969456672403881 ) ) ;
#46747 = CARTESIAN_POINT ( 'NONE',  ( 4.343750000000002665, 1.895863743164175608, 0.7852924748297558377 ) ) ;
#46748 =( BOUNDED_SURFACE ( )  B_SPLINE_SURFACE ( 3, 2, ( 
 ( #100173, #150002, #67633 ),
 ( #82851, #51433, #198715 ),
 ( #183547, #2639, #54622 ),
 ( #152131, #52488, #165173 ),
 ( #1572, #69776, #166238 ),
 ( #66568, #169438, #117553 ),
 ( #50361, #167313, #18900 ),
 ( #17828, #21022, #135884 ) ),
 .UNSPECIFIED., .F., .F., .T. ) 
 B_SPLINE_SURFACE_WITH_KNOTS ( ( 4, 2, 2, 4 ),
 ( 3, 3 ),
 ( 0.000000000000000000, 0.0002204160392919248825, 0.0004408320785838497650, 0.0008816641571676995300 ),
 ( 0.000000000000000000, 1.000000000000000000 ),
 .UNSPECIFIED. ) 
 GEOMETRIC_REPRESENTATION_ITEM ( )  RATIONAL_B_SPLINE_SURFACE ( (
 ( 1.000000000000000000, 0.4127341956165090364, 1.000000000000000000),
 ( 1.000000000000000000, 0.4103180386329450813, 1.000000000000000000),
 ( 1.000000000000000000, 0.4223234233960728723, 1.000000000000000000),
 ( 1.000000000000000000, 0.4613847219396438604, 1.000000000000000000),
 ( 1.000000000000000000, 0.4878744032655865093, 1.000000000000000000),
 ( 1.000000000000000000, 0.5702658980234648345, 1.000000000000000000),
 ( 1.000000000000000000, 0.6280001242509933856, 1.000000000000000000),
 ( 1.000000000000000000, 0.6787756258918243857, 1.000000000000000000) ) ) 
 REPRESENTATION_ITEM ( '' )  SURFACE ( )  );
#46749 = CARTESIAN_POINT ( 'NONE',  ( 1.499999999999987121, 1.535416667349486453, 0.8660254037844524744 ) ) ;
#46750 = CARTESIAN_POINT ( 'NONE',  ( 6.727182134110236689, 0.003007720480393410133, 1.910970182385362870 ) ) ;
#46752 = B_SPLINE_CURVE_WITH_KNOTS ( 'NONE', 3,
 ( #194132, #144375, #65180, #163787, #111899, #47925, #29515, #97729 ),
 .UNSPECIFIED., .F., .F.,
 ( 4, 2, 2, 4 ),
 ( 0.000000000000000000, 0.001555696184809488535, 0.003111392369618977069, 0.006222784739237952403 ),
 .UNSPECIFIED. ) ;
#46751 = CARTESIAN_POINT ( 'NONE',  ( -0.6823417656250039265, 13.31770833367473195, -1.181850606188755259 ) ) ;
#46753 = CARTESIAN_POINT ( 'NONE',  ( 3.920361760358490599, -2.215291009692350599, 0.1660125995653055075 ) ) ;
#46754 = EDGE_LOOP ( 'NONE', ( #29759, #71144, #123331, #151956, #84549, #145919 ) ) ;
#46755 = CYLINDRICAL_SURFACE ( 'NONE', #205408, 0.08000000000000020983 ) ;
#46756 = CARTESIAN_POINT ( 'NONE',  ( -1.500000000000001332, -0.8499999999999757749, 0.000000000000000000 ) ) ;
#46757 = CARTESIAN_POINT ( 'NONE',  ( 8.076906825439115423, 10.44614393447756129, -1.599625672291262513 ) ) ;
#46758 = CARTESIAN_POINT ( 'NONE',  ( 7.960045584554727327, 8.459343734834927631, 0.7216878364870267237 ) ) ;
#46759 = FILL_AREA_STYLE_COLOUR ( '', #66341 ) ;
#46760 = CARTESIAN_POINT ( 'NONE',  ( 5.196709787541290204, 1.427093291641279293, 0.9959802872364865722 ) ) ;
#46761 = CARTESIAN_POINT ( 'NONE',  ( 3.543363863352413823, 1.774678991803163575, -0.8365776047038612218 ) ) ;
#46763 = CARTESIAN_POINT ( 'NONE',  ( -5.897433632264490910, 9.824163637709826702, 0.000000000000000000 ) ) ;
#46762 = CARTESIAN_POINT ( 'NONE',  ( 4.196412238629597447, 4.854568018944682706, -1.199719254218452047 ) ) ;
#46764 = DIRECTION ( 'NONE',  ( -7.993605777301127091E-15, 0.000000000000000000, -1.000000000000000000 ) ) ;
#46765 = CARTESIAN_POINT ( 'NONE',  ( 4.780719109985231974, -2.192918799143634079, -0.5559354454096259168 ) ) ;
#46766 = CARTESIAN_POINT ( 'NONE',  ( 1.609910828531309956, 0.6006481715085715267, -1.973267531027416810 ) ) ;
#46767 = CARTESIAN_POINT ( 'NONE',  ( -5.520141099058386125, 9.591915048876776595, 0.000000000000000000 ) ) ;
#46768 = CARTESIAN_POINT ( 'NONE',  ( 2.307839474932214419, -0.4956500345179111200, 2.207406129587013766 ) ) ;
#46769 = ORIENTED_EDGE ( 'NONE', *, *, #43069, .T. ) ;
#46770 = CARTESIAN_POINT ( 'NONE',  ( -0.7500000000000215383, 0.7229166673494852313, 1.299038105676659116 ) ) ;
#46771 = CARTESIAN_POINT ( 'NONE',  ( 3.180766902908559235, -0.1340872481324743570, -1.865776598943262199 ) ) ;
#46772 = CARTESIAN_POINT ( 'NONE',  ( 2.021687164805381354, -1.548805232022354650, 0.7802212711869142003 ) ) ;
#46773 = CARTESIAN_POINT ( 'NONE',  ( -0.1288028175206907822, -0.008968661790493319408, -2.273875003271645934 ) ) ;
#46774 = CARTESIAN_POINT ( 'NONE',  ( 0.3060867131535297547, -0.5861141839358529060, 2.127432003918772629 ) ) ;
#46775 = CARTESIAN_POINT ( 'NONE',  ( 4.540002997438313592, 0.9271085556134452954, -1.952944755896801610 ) ) ;
#46776 = CARTESIAN_POINT ( 'NONE',  ( 4.997963218837587540, -0.6557800786283998207, -1.827999027568379509 ) ) ;
#46777 = CARTESIAN_POINT ( 'NONE',  ( -10.15522075183580419, 11.80651128435196462, 1.199719254218462483 ) ) ;
#46778 = CARTESIAN_POINT ( 'NONE',  ( 6.696569769017397533, -0.4992639023812007193, -1.802638941973549569 ) ) ;
#46779 =( NAMED_UNIT ( * ) PLANE_ANGLE_UNIT ( ) SI_UNIT ( $, .RADIAN. ) );
#46780 = CARTESIAN_POINT ( 'NONE',  ( 4.895304229855391043, 6.665267352516039523, 1.249363049274658799 ) ) ;
#46781 = CARTESIAN_POINT ( 'NONE',  ( 6.983263157960365675, -0.006178392973848687020, 2.053544886540019210 ) ) ;
#46782 = CARTESIAN_POINT ( 'NONE',  ( 3.106226591306694651, 6.638031766584184368, 0.000000000000000000 ) ) ;
#46783 = CARTESIAN_POINT ( 'NONE',  ( -4.757329562667670667E-14, 1.953125000341451312, 1.570758158831762286 ) ) ;
#46784 = CARTESIAN_POINT ( 'NONE',  ( 5.643203987388664800, 0.8197706014990979728, 1.842448445624145226 ) ) ;
#46785 = CARTESIAN_POINT ( 'NONE',  ( -10.16591625214838679, 10.75465713712827487, 1.040834085586084257E-14 ) ) ;
#46786 = CARTESIAN_POINT ( 'NONE',  ( 8.796542737168120851, 9.157054702984622097, -0.7998128361456211532 ) ) ;
#46787 = CARTESIAN_POINT ( 'NONE',  ( 2.680971279526301210, -0.4847509252939742885, -0.1005634232587017118 ) ) ;
#46789 = FACE_OUTER_BOUND ( 'NONE', #41606, .T. ) ;
#46788 = CARTESIAN_POINT ( 'NONE',  ( 3.650846181029033133, -1.491723252493650564, 1.052289205326197852 ) ) ;
#46790 = CARTESIAN_POINT ( 'NONE',  ( 11.92619526913699879, 10.07218333338756722, -1.328859060402686199 ) ) ;
#46791 = VERTEX_POINT ( 'NONE', #111155 ) ;
#46792 = CARTESIAN_POINT ( 'NONE',  ( -4.245111494410291897, 7.006361605903701495, 1.082531754730549967 ) ) ;
#46793 = EDGE_CURVE ( 'NONE', #126082, #92893, #1751, .T. ) ;
#46794 = CARTESIAN_POINT ( 'NONE',  ( 3.285556943750000514, -3.901041666188710177, 1.896917185911906500 ) ) ;
#46795 = CARTESIAN_POINT ( 'NONE',  ( -6.821723845970312894, 11.11042825360738284, 0.000000000000000000 ) ) ;
#46796 = CARTESIAN_POINT ( 'NONE',  ( 0.4045644467639066821, -2.005039209919571075, -0.2428365769681257724 ) ) ;
#46797 = CARTESIAN_POINT ( 'NONE',  ( 1.717596852896427606, 1.764750374324057347, 1.175337852406685757 ) ) ;
#46798 = ORIENTED_EDGE ( 'NONE', *, *, #168648, .T. ) ;
#46799 = CARTESIAN_POINT ( 'NONE',  ( -4.773352600463090845, 7.726605912919016106, 1.199719254218452935 ) ) ;
#46800 = CARTESIAN_POINT ( 'NONE',  ( 1.445918188014534422, -0.8427435445049488161, 1.659298548423918884 ) ) ;
#46801 = CARTESIAN_POINT ( 'NONE',  ( 4.487912541323413329, 5.194651705420806564, 1.199719254218462483 ) ) ;
#46802 = CARTESIAN_POINT ( 'NONE',  ( 0.09294085500742564621, -0.4768749645070144982, -2.116232079886640971 ) ) ;
#46803 = DIRECTION ( 'NONE',  ( -5.551115123125764829E-17, 0.000000000000000000, 1.000000000000000000 ) ) ;
#46804 = ORIENTED_EDGE ( 'NONE', *, *, #28580, .T. ) ;
#46805 = CARTESIAN_POINT ( 'NONE',  ( -8.597841969360544567, 13.18256606422934674, 0.7998128361456341429 ) ) ;
#46806 = CARTESIAN_POINT ( 'NONE',  ( -0.2108831679770960255, -0.001785917861228669690, -1.896958272444612792 ) ) ;
#46808 = CARTESIAN_POINT ( 'NONE',  ( -5.085529380082158823, 6.726364094520411285, -1.441608068093344741 ) ) ;
#46807 = CARTESIAN_POINT ( 'NONE',  ( -5.679940009482361774, 5.591294530676332641, 0.7998128361456281477 ) ) ;
#46809 = CARTESIAN_POINT ( 'NONE',  ( 6.472394699177205446, 6.854181287346997387, 0.6349317888264572884 ) ) ;
#46810 = CARTESIAN_POINT ( 'NONE',  ( 6.292342264464226176, -1.899326897351862664, 0.6766127494588560776 ) ) ;
#46811 = CARTESIAN_POINT ( 'NONE',  ( 6.193280126971262511, -0.6156851667328180344, 1.735278506779000640 ) ) ;
#46812 = CARTESIAN_POINT ( 'NONE',  ( -0.02319159430949970999, 2.891346550825595774, -2.299931007135449512 ) ) ;
#46813 = CARTESIAN_POINT ( 'NONE',  ( 3.774305527563319274, 1.280948863717756847, 1.919355958833997233 ) ) ;
#46814 = CARTESIAN_POINT ( 'NONE',  ( 6.391743074199808916, 6.421731439513382433, -0.7998128361456481317 ) ) ;
#46815 = CARTESIAN_POINT ( 'NONE',  ( 5.466167184710096549, 1.060119519021487378, 1.883692621652333532 ) ) ;
#46816 = CARTESIAN_POINT ( 'NONE',  ( 7.741869408603235136, 8.990934717247309749, 1.199719254218462483 ) ) ;
#46817 = CARTESIAN_POINT ( 'NONE',  ( 0.8549040543346017040, 0.3774493213832031402, -1.904865965088814228 ) ) ;
#46818 = CARTESIAN_POINT ( 'NONE',  ( -3.574546055497324737, 7.322054164722185732, 0.7998128361456341429 ) ) ;
#46819 = ORIENTED_EDGE ( 'NONE', *, *, #142903, .F. ) ;
#46820 = CARTESIAN_POINT ( 'NONE',  ( 4.956595877991936128, 1.698763664877179780, 1.548309420705455741 ) ) ;
#46821 = DIRECTION ( 'NONE',  ( 0.000000000000000000, -1.000000000000000000, 0.000000000000000000 ) ) ;
#46823 = PRESENTATION_LAYER_ASSIGNMENT (  '', '', ( #126503 ) ) ;
#46822 = CARTESIAN_POINT ( 'NONE',  ( -4.787964524281469458, 5.614988695530339413, -1.199719254218453823 ) ) ;
#46824 = CARTESIAN_POINT ( 'NONE',  ( 4.803500792215161574, -0.4985019455652460740, 1.802925825644098534 ) ) ;
#46825 = VECTOR ( 'NONE', #156202, 1000.000000000000114 ) ;
#46828 = CARTESIAN_POINT ( 'NONE',  ( -5.635349125135588721, 6.603604063193491136, 1.199719254218452935 ) ) ;
#46827 = CARTESIAN_POINT ( 'NONE',  ( 1.499999999999987121, 0.3270833340161527492, -0.8660254037844323793 ) ) ;
#46826 = CARTESIAN_POINT ( 'NONE',  ( 0.7559434568639655794, 0.7726834774516875282, -1.749509110286852742 ) ) ;
#46829 = CARTESIAN_POINT ( 'NONE',  ( 3.510573375967055654, -0.8941257848905452832, -2.017821460644920073 ) ) ;
#46830 = CARTESIAN_POINT ( 'NONE',  ( -3.246376473470825363, -0.8887487162375362626, 0.5058895364790267912 ) ) ;
#46831 = CARTESIAN_POINT ( 'NONE',  ( 3.623053363349855172, 5.249981562040033189, 1.599625672291267398 ) ) ;
#46832 = CARTESIAN_POINT ( 'NONE',  ( 5.167065940139554669, 9.042344340222555843, -0.7216878364870458196 ) ) ;
#46833 = CARTESIAN_POINT ( 'NONE',  ( -2.435661151949389147, 5.993355110582911038, 0.7998128361456341429 ) ) ;
#46834 = CARTESIAN_POINT ( 'NONE',  ( -6.143253000323532831, 7.300121600866474658, 1.082531754730548412 ) ) ;
#46835 = CARTESIAN_POINT ( 'NONE',  ( 2.161341668630599955, 0.3408821015241836894, -1.941522824740661290 ) ) ;
#46836 = CARTESIAN_POINT ( 'NONE',  ( 0.9917865004017255570, 2.033541294120873033, -1.090684920485317733 ) ) ;
#46837 = CARTESIAN_POINT ( 'NONE',  ( 2.101936620064443151, 0.7537240185569763495, -1.811501260397870405 ) ) ;
#46838 = CARTESIAN_POINT ( 'NONE',  ( 4.944214452789121417, -0.9770834884576683477, 1.816490783314741231 ) ) ;
#46839 = CARTESIAN_POINT ( 'NONE',  ( 5.355107487717867265, 5.349972945200037522, 1.040834085586084257E-14 ) ) ;
#46840 = CARTESIAN_POINT ( 'NONE',  ( 4.908934136599710563, 7.884784371745123366, 1.199719254218451159 ) ) ;
#46841 = ORIENTED_EDGE ( 'NONE', *, *, #165880, .T. ) ;
#46842 = CARTESIAN_POINT ( 'NONE',  ( -4.900701038327225589, 4.857544330914580044, 0.2781515650015027319 ) ) ;
#46843 = CARTESIAN_POINT ( 'NONE',  ( 6.534012848836709075, -6.583711766989043035, 7.055786748303249922 ) ) ;
#46844 = CARTESIAN_POINT ( 'NONE',  ( 3.728129053633592704, 4.412200653069714207, -1.082531754730543083 ) ) ;
#46845 = CARTESIAN_POINT ( 'NONE',  ( 0.9190777403676134716, -1.573854924298900615, 1.495750265368815946 ) ) ;
#46847 = CARTESIAN_POINT ( 'NONE',  ( 6.229045230835819069, 6.231917288922055320, -0.7998128361456481317 ) ) ;
#46846 = CARTESIAN_POINT ( 'NONE',  ( 2.857890832048201712, 6.434070695103256021, -0.3041713968356236086 ) ) ;
#46848 = CARTESIAN_POINT ( 'NONE',  ( 11.44800751629994906, 11.29999999999999893, -3.302956944461097777 ) ) ;
#46849 = CARTESIAN_POINT ( 'NONE',  ( -6.726765609221550868, -8.198316280115697907, 6.726765609221573960 ) ) ;
#46850 = CARTESIAN_POINT ( 'NONE',  ( 2.126040175964475143, 1.080828230516362121, -1.526477596812993553 ) ) ;
#46851 = CARTESIAN_POINT ( 'NONE',  ( 6.643834073375672666, 0.8340821395082242962, -1.994398315854857495 ) ) ;
#46853 = CARTESIAN_POINT ( 'NONE',  ( 6.727182134110210043, 6.040083938853186396, 2.305853406558423302 ) ) ;
#46852 = CARTESIAN_POINT ( 'NONE',  ( 0.000000000000000000, 13.88000000000000078, 0.000000000000000000 ) ) ;
#46854 = CARTESIAN_POINT ( 'NONE',  ( -0.6823417656250003738, -1.032291666325242607, -1.181850606188749264 ) ) ;
#46855 = CARTESIAN_POINT ( 'NONE',  ( 2.578645926699867363, -1.317302948579327504, 1.386430337501590282 ) ) ;
#46856 = CARTESIAN_POINT ( 'NONE',  ( 4.293650081035056409, -0.6766669130573493840, 1.635584247362771304 ) ) ;
#46857 = CIRCLE ( 'NONE', #129933, 2.150000000000006573 ) ;
#46858 = CARTESIAN_POINT ( 'NONE',  ( 1.611815888142430264, -0.6431676737995162263, 1.801018335096972400 ) ) ;
#46859 = CARTESIAN_POINT ( 'NONE',  ( -3.730464822054482710, 7.503959392372201442, 1.040834085586084257E-14 ) ) ;
#46861 = CARTESIAN_POINT ( 'NONE',  ( 5.167565342116251514, 1.290006671357433632, 1.416291653197629952 ) ) ;
#46860 = CARTESIAN_POINT ( 'NONE',  ( -1.850000000000000089, 2.265596578422597184E-16, -5.732590180780448463 ) ) ;
#46862 = CARTESIAN_POINT ( 'NONE',  ( 0.1333692844072559280, 0.001398348041498076455, -2.053671342968105051 ) ) ;
#46863 = CARTESIAN_POINT ( 'NONE',  ( -1.500000000000011324, 4.670833333333353821, 0.8660254037844403729 ) ) ;
#46864 = CARTESIAN_POINT ( 'NONE',  ( 2.039458538997685366, 0.004855507148140979744, 2.120778211687989856 ) ) ;
#46865 =( LENGTH_UNIT ( ) NAMED_UNIT ( * ) SI_UNIT ( .MILLI., .METRE. ) );
#46866 = CARTESIAN_POINT ( 'NONE',  ( 5.155093292349416600, -1.580716073637401076, -1.000049079914612449 ) ) ;
#46868 = ORIENTED_EDGE ( 'NONE', *, *, #119448, .T. ) ;
#46867 = CARTESIAN_POINT ( 'NONE',  ( 1.523764310407935030, -1.012771255265769943, -1.518815351243132383 ) ) ;
#46870 = CARTESIAN_POINT ( 'NONE',  ( 0.7499999999999902300, 4.316666666666691299, -1.299038105676658228 ) ) ;
#46869 = CARTESIAN_POINT ( 'NONE',  ( 4.231241840954825584, 0.1069408422738199749, 2.204416794138922331 ) ) ;
#46871 = CARTESIAN_POINT ( 'NONE',  ( -1.602468905319636405E-14, -1.053124999658583638, -1.575800808251665908 ) ) ;
#46872 = CARTESIAN_POINT ( 'NONE',  ( 1.803259461591859347, -1.743671650923955374, 1.101644963814436329 ) ) ;
#46873 = CARTESIAN_POINT ( 'NONE',  ( 5.289652487626049115, 9.323011668872403845, 0.7998128361456462443 ) ) ;
#46874 = CARTESIAN_POINT ( 'NONE',  ( -8.015895134177625891, 10.37496362800581018, 1.599625672291295375 ) ) ;
#46875 = FACE_OUTER_BOUND ( 'NONE', #88999, .T. ) ;
#46877 = CARTESIAN_POINT ( 'NONE',  ( -0.4153311931459208184, 3.850000000000006306, -0.4999999999999961142 ) ) ;
#46876 = VECTOR ( 'NONE', #59422, 1000.000000000000000 ) ;
#46878 = LINE ( 'NONE', #197355, #65193 ) ;
#46879 = ORIENTED_EDGE ( 'NONE', *, *, #117958, .T. ) ;
#46880 = CARTESIAN_POINT ( 'NONE',  ( 3.824723168590526523, -1.392635068473629500, 1.532133406949770960 ) ) ;
#46881 = CARTESIAN_POINT ( 'NONE',  ( -0.6823417656250003738, -0.9697916663252494907, -1.181850606188749264 ) ) ;
#46882 = CARTESIAN_POINT ( 'NONE',  ( 2.495597164219889308, 1.669172397749154380, 1.373402732410613947 ) ) ;
#46883 = CARTESIAN_POINT ( 'NONE',  ( -6.237206930280429162, 6.931128591455327559, -0.8289643595828979361 ) ) ;
#46884 = CARTESIAN_POINT ( 'NONE',  ( 2.367837350726550660, 0.5366352218779540939, -1.947015567076612941 ) ) ;
#46885 = DIRECTION ( 'NONE',  ( 5.551115123125766062E-17, 0.000000000000000000, -1.000000000000000000 ) ) ;
#46886 = ORIENTED_EDGE ( 'NONE', *, *, #127184, .T. ) ;
#46887 = AXIS2_PLACEMENT_3D ( 'NONE', #66365, #194525, #32837 ) ;
#46889 = CARTESIAN_POINT ( 'NONE',  ( 7.537970219518073556, 9.817384560903001045, -1.443375672974057666 ) ) ;
#46888 = CARTESIAN_POINT ( 'NONE',  ( -1.737500000000000266, -2.158333333333331439, -3.009438278150923907 ) ) ;
#46890 = CARTESIAN_POINT ( 'NONE',  ( -3.594320120954326292, 6.247105003538398371, 1.082531754730549967 ) ) ;
#46891 = CARTESIAN_POINT ( 'NONE',  ( 0.1281391398850126040, 2.011452084832816123, 0.1435147193784985509 ) ) ;
#46892 = CARTESIAN_POINT ( 'NONE',  ( 4.511385190476093321, -2.149204750630455241, 0.4279282578087198474 ) ) ;
#46893 = CARTESIAN_POINT ( 'NONE',  ( 1.499999999999987121, 4.077083334016147198, -0.8660254037844323793 ) ) ;
#46894 = CARTESIAN_POINT ( 'NONE',  ( 4.236511230858605259, 1.172298487584079396, -1.510895503047122945 ) ) ;
#46895 = CARTESIAN_POINT ( 'NONE',  ( -3.765413976293358278, 5.416068943807445635, 1.599625672291267398 ) ) ;
#46896 = CARTESIAN_POINT ( 'NONE',  ( 5.599154252319471503, 9.476171027773981237, -0.7216878364870267237 ) ) ;
#46898 = CARTESIAN_POINT ( 'NONE',  ( 2.407827563459669307, -1.163288551851604513, -1.646826728940099738 ) ) ;
#46897 = CARTESIAN_POINT ( 'NONE',  ( -9.015808962963337336, 10.58116054728778366, 1.082531754730558626 ) ) ;
#46899 = CARTESIAN_POINT ( 'NONE',  ( 1.364683531249997417, 12.04687500034139980, 2.602085213965210642E-15 ) ) ;
#46900 = B_SPLINE_CURVE_WITH_KNOTS ( 'NONE', 3,
 ( #27974, #126624, #109301, #46368 ),
 .UNSPECIFIED., .F., .F.,
 ( 4, 4 ),
 ( 0.001812203442042620034, 0.002059939351771558277 ),
 .UNSPECIFIED. ) ;
#46901 = CARTESIAN_POINT ( 'NONE',  ( -2.979759899953417612, 6.698413326579433225, 0.7998128361456352531 ) ) ;
#46902 = CARTESIAN_POINT ( 'NONE',  ( 5.403229623239121260, 1.412049869051584361, 0.9901104176405839397 ) ) ;
#46903 = CARTESIAN_POINT ( 'NONE',  ( -0.1399997263889819488, 4.088450529495776919, -2.555104583160577203 ) ) ;
#46904 = CARTESIAN_POINT ( 'NONE',  ( 8.595506201383999567, 12.97191496834930113, 0.7216878364870438212 ) ) ;
#46905 = CYLINDRICAL_SURFACE ( 'NONE', #26250, 0.08000000000000020983 ) ;
#46906 = ORIENTED_EDGE ( 'NONE', *, *, #78821, .F. ) ;
#46907 = CARTESIAN_POINT ( 'NONE',  ( 0.8134373588399683719, -1.746984811521329339, -1.110588058507409936 ) ) ;
#46908 = ORIENTED_EDGE ( 'NONE', *, *, #80448, .F. ) ;
#46909 = CARTESIAN_POINT ( 'NONE',  ( 4.898965649768390662, -0.2269230896460339986, -1.797137895798770479 ) ) ;
#46910 = CARTESIAN_POINT ( 'NONE',  ( 5.903649544107831382, 5.852288987739402870, -0.7998128361456481317 ) ) ;
#46911 = CARTESIAN_POINT ( 'NONE',  ( 6.775478006741562531, -7.217909409563599610, -6.775478006741584736 ) ) ;
#46912 = CARTESIAN_POINT ( 'NONE',  ( 5.848286676205444401, 0.8867688175292733899, -1.579494629471886791 ) ) ;
#46913 = CARTESIAN_POINT ( 'NONE',  ( 5.519577934094861860, 6.572500690266394940, 1.082531754730549078 ) ) ;
#46914 = CARTESIAN_POINT ( 'NONE',  ( 1.123270288250309612, 3.221052654332833054, -0.7749999999993620881 ) ) ;
#46915 = CARTESIAN_POINT ( 'NONE',  ( 2.836070844659248191, 2.175002134116140518, 0.2674123886829762875 ) ) ;
#46916 = ORIENTED_EDGE ( 'NONE', *, *, #87162, .F. ) ;
#46917 = EDGE_CURVE ( 'NONE', #168291, #160543, #129033, .T. ) ;
#46919 = CARTESIAN_POINT ( 'NONE',  ( 7.944187942603509356, 11.35563746875774882, 1.199719254218460707 ) ) ;
#46918 = CARTESIAN_POINT ( 'NONE',  ( 6.877413160773132361, -0.1400689347856296230, 1.829862831089356545 ) ) ;
#46920 = CARTESIAN_POINT ( 'NONE',  ( 5.325768798837505535, 0.7719732895165082320, -1.753353820041517741 ) ) ;
#46921 = FACE_OUTER_BOUND ( 'NONE', #72671, .T. ) ;
#46922 = SURFACE_STYLE_FILL_AREA ( #210450 ) ;
#46923 = CARTESIAN_POINT ( 'NONE',  ( 1.364683531249986537, 0.3635416670080869328, 0.7879004041258500513 ) ) ;
#46924 = CARTESIAN_POINT ( 'NONE',  ( 6.331294547901813452, 6.488857848747989543, 1.040834085586084257E-14 ) ) ;
#46925 = CARTESIAN_POINT ( 'NONE',  ( -8.595506201384022660, 11.05117653974661529, 1.443375672974064550 ) ) ;
#46926 = CARTESIAN_POINT ( 'NONE',  ( 1.376082401959723089, 1.288024388040419632, 1.735935173841046675 ) ) ;
#46927 = CARTESIAN_POINT ( 'NONE',  ( -4.797606254389363833, 6.690569611577942943, 1.599625672291263179 ) ) ;
#46928 = CARTESIAN_POINT ( 'NONE',  ( 5.228604516725597229, 6.129068686715179126, -1.199719254218450271 ) ) ;
#46929 = CARTESIAN_POINT ( 'NONE',  ( 2.309345278970798887, -0.4025885200794159235, 1.780468244869021222 ) ) ;
#46930 = CARTESIAN_POINT ( 'NONE',  ( -3.578462479003122976, 6.262291094557191684, 1.199719254218464037 ) ) ;
#46931 = CARTESIAN_POINT ( 'NONE',  ( 5.157177646623883227, -1.542991646335686973, -0.9753701268572569916 ) ) ;
#46932 = CARTESIAN_POINT ( 'NONE',  ( 12.65758923026637817, 7.325950736540248087, -3.630282196008513651 ) ) ;
#46933 = CARTESIAN_POINT ( 'NONE',  ( 2.707167837304753633, 1.638089068140319071, -0.9866689735503200165 ) ) ;
#46934 = ORIENTED_EDGE ( 'NONE', *, *, #182978, .F. ) ;
#46935 = CARTESIAN_POINT ( 'NONE',  ( 3.455474441396837904, 1.550956523109302543, 1.213803446622195636 ) ) ;
#46936 = ORIENTED_EDGE ( 'NONE', *, *, #165880, .F. ) ;
#46937 = CARTESIAN_POINT ( 'NONE',  ( 4.933121067701986995, -1.376026015944699088, -1.370709014919595958 ) ) ;
#46938 = ORIENTED_EDGE ( 'NONE', *, *, #207112, .F. ) ;
#46939 = CARTESIAN_POINT ( 'NONE',  ( -7.099629715411508890, 8.311931418515415615, 1.199719254218452047 ) ) ;
#46941 = CARTESIAN_POINT ( 'NONE',  ( 4.887034483293543730, -1.997634423138573867, -0.7120497732875651353 ) ) ;
#46940 = CARTESIAN_POINT ( 'NONE',  ( 6.866278450678116485, 6.975356045404744521, 0.000000000000000000 ) ) ;
#46942 = CARTESIAN_POINT ( 'NONE',  ( 10.98545788874447560, 9.842562204520739044, 1.592267205258850238 ) ) ;
#46944 = ORIENTED_EDGE ( 'NONE', *, *, #154810, .T. ) ;
#46943 = CARTESIAN_POINT ( 'NONE',  ( 3.316961667764028121, 1.505919282548912719, -1.178437403786938731 ) ) ;
#46945 = CARTESIAN_POINT ( 'NONE',  ( 4.930363510330384003, 6.858250545851714008, -1.424563464522425882 ) ) ;
#46946 = DIRECTION ( 'NONE',  ( 1.000000000000000000, -0.000000000000000000, -0.000000000000000000 ) ) ;
#46947 = VERTEX_POINT ( 'NONE', #80722 ) ;
#46948 = CARTESIAN_POINT ( 'NONE',  ( 1.608462485350599769, 8.735270501766756013, 2.463594439587641904 ) ) ;
#46949 = CARTESIAN_POINT ( 'NONE',  ( 4.723295704472612044, 1.752545568416422173, 0.9903661003969994603 ) ) ;
#46950 = CARTESIAN_POINT ( 'NONE',  ( -3.975509539288551775, 7.849563252032789151, -0.3275587863690732071 ) ) ;
#46951 = CARTESIAN_POINT ( 'NONE',  ( 5.250558533952181861, 0.5335417292645014964, 1.745990657226546894 ) ) ;
#46952 = CARTESIAN_POINT ( 'NONE',  ( 1.029834584532058672, 1.995790600324919506, -0.5504719462680053299 ) ) ;
#46953 = CARTESIAN_POINT ( 'NONE',  ( -6.832946231607472498, 9.955225789308602913, 1.082531754730549967 ) ) ;
#46954 = CARTESIAN_POINT ( 'NONE',  ( -6.502837976706968171, 6.831778935668112673, 0.5908271424688981144 ) ) ;
#46955 = CARTESIAN_POINT ( 'NONE',  ( -0.4123176713736718679, 3.999999999999981348, -0.8977835139438229417 ) ) ;
#46956 = CARTESIAN_POINT ( 'NONE',  ( 6.209813078548920728, -1.856259414618817383, 0.2309603555875269776 ) ) ;
#46957 = CARTESIAN_POINT ( 'NONE',  ( 6.368579470117202490, 8.453095353268645695, 1.599625672291281386 ) ) ;
#46958 = EDGE_CURVE ( 'NONE', #175863, #136449, #79977, .T. ) ;
#46959 = DIRECTION ( 'NONE',  ( 0.7592566023653005702, 0.6507913734559639396, 0.000000000000000000 ) ) ;
#46960 = CARTESIAN_POINT ( 'NONE',  ( -1.364683531250010295, 10.19270833367473017, 0.7879004041258445001 ) ) ;
#46961 = CARTESIAN_POINT ( 'NONE',  ( -4.412288926243578935, 7.235088616337731260, 1.199719254218464037 ) ) ;
#46962 = CARTESIAN_POINT ( 'NONE',  ( -5.126391479298592735, 5.153413945369351268, 0.000000000000000000 ) ) ;
#46963 = CIRCLE ( 'NONE', #195691, 0.07999999999999983513 ) ;
#46964 = CARTESIAN_POINT ( 'NONE',  ( -4.218558352146454915, 8.073401844146177453, 1.040834085586084257E-14 ) ) ;
#46965 = CARTESIAN_POINT ( 'NONE',  ( 1.375928118113247667, -2.020660359122231409, 0.4497719141252010111 ) ) ;
#46966 = CARTESIAN_POINT ( 'NONE',  ( 2.495853057047519030, -2.093741659442478920, 0.3138373457529738397 ) ) ;
#46967 = AXIS2_PLACEMENT_3D ( 'NONE', #199644, #137888, #45448 ) ;
#46968 = CARTESIAN_POINT ( 'NONE',  ( 8.158255747121103241, 10.54105100977322174, 1.599625672291281386 ) ) ;
#46969 = EDGE_CURVE ( 'NONE', #144059, #39789, #114355, .T. ) ;
#46970 = CARTESIAN_POINT ( 'NONE',  ( 0.4968415868889561882, 0.3310222599195339899, 1.941247527895247904 ) ) ;
#46971 = CARTESIAN_POINT ( 'NONE',  ( 4.044190953901719787, 7.767772900817621284, 0.4663397696828552874 ) ) ;
#46972 = CARTESIAN_POINT ( 'NONE',  ( 3.823036129373602154, 6.443664003369091731, -1.082531754730548412 ) ) ;
#46974 = CARTESIAN_POINT ( 'NONE',  ( -0.08000000000000367928, -7.246166700194011767, 9.579665964948883783 ) ) ;
#46973 = CARTESIAN_POINT ( 'NONE',  ( 1.737499999999999378, -3.616666666666667140, -3.009438278150925683 ) ) ;
#46975 = CARTESIAN_POINT ( 'NONE',  ( 2.783473570837506017, 1.621738419858234304, 1.620254553110695772 ) ) ;
#46976 = CARTESIAN_POINT ( 'NONE',  ( 0.7151340513122245168, -0.2707656271505008982, 1.805370379145049275 ) ) ;
#46977 = CARTESIAN_POINT ( 'NONE',  ( 1.968876373762207255, -1.476028252698018628, 1.215921256797661609 ) ) ;
#46978 = EDGE_CURVE ( 'NONE', #123356, #110637, #140493, .T. ) ;
#46979 = CARTESIAN_POINT ( 'NONE',  ( 6.855582950365507244, 8.027210192628430718, -1.199719254218452047 ) ) ;
#46980 = CARTESIAN_POINT ( 'NONE',  ( 7.253248993186731219, 8.524840582548424806, 1.082531754730558626 ) ) ;
#46981 = CARTESIAN_POINT ( 'NONE',  ( 1.722903956744771481, 1.489010464042400450, -1.355078301658399820 ) ) ;
#46982 = CARTESIAN_POINT ( 'NONE',  ( 2.588659458060487584, 1.901619664775334728, 0.4814403318105645591 ) ) ;
#46983 = CARTESIAN_POINT ( 'NONE',  ( -8.136864746495904299, 12.64475930422059768, -0.7998128361456281477 ) ) ;
#46984 = CARTESIAN_POINT ( 'NONE',  ( -6.015013705957189316, 10.16926642359206134, 0.7998128361456481317 ) ) ;
#46985 = CARTESIAN_POINT ( 'NONE',  ( -11.88533610222442505, 7.946055938851326772, -1.309387650900987854 ) ) ;
#46987 = CARTESIAN_POINT ( 'NONE',  ( 3.274023454312132486, -1.055227348164128331, 1.420681018326484413 ) ) ;
#46986 = CARTESIAN_POINT ( 'NONE',  ( 4.769523239323490316, 1.203412094891454842, 1.709343392706575315 ) ) ;
#46988 = CARTESIAN_POINT ( 'NONE',  ( -11.86239285000045918, 12.21999999999998288, 1.812080536912751061 ) ) ;
#46990 = CARTESIAN_POINT ( 'NONE',  ( 6.333931935734662844, 2.266371222927834772, 0.3428166536569366984 ) ) ;
#46989 = DIRECTION ( 'NONE',  ( -1.000000000000000000, 0.000000000000000000, -5.551115123125765446E-17 ) ) ;
#46991 = CARTESIAN_POINT ( 'NONE',  ( 4.470479574576804005, -0.003715868306445029284, -1.740516468156935836 ) ) ;
#46992 = CARTESIAN_POINT ( 'NONE',  ( 8.402302512167096893, 10.82577223566020841, -1.599625672291268286 ) ) ;
#46993 = CARTESIAN_POINT ( 'NONE',  ( 0.000000000000000000, -11.15905291171102931, 0.000000000000000000 ) ) ;
#46994 = CARTESIAN_POINT ( 'NONE',  ( 4.253097392439049607, -1.714905526014463666, -0.2545648513426115311 ) ) ;
#46995 = CARTESIAN_POINT ( 'NONE',  ( 4.826735082517537023, -1.421624449711873295, 1.641102681368050487 ) ) ;
#46996 = CARTESIAN_POINT ( 'NONE',  ( 4.546061579283848353, 4.198160018786257552, -0.7998128361456211532 ) ) ;
#46997 = CARTESIAN_POINT ( 'NONE',  ( 5.893767612163585135, -2.000732204962274441, 0.2516274335107801519 ) ) ;
#46999 = VECTOR ( 'NONE', #20993, 1000.000000000000000 ) ;
#46998 = CARTESIAN_POINT ( 'NONE',  ( 5.625000000000003553, -2.052068128417940951, 3.204627906038193246E-13 ) ) ;
#47000 = CARTESIAN_POINT ( 'NONE',  ( -1.001543065824772872E-14, 5.493750000682816825, 1.732050807568877637 ) ) ;
#47001 = CARTESIAN_POINT ( 'NONE',  ( 2.731371607455813422, -1.798138232897347644, 0.6916047562727283271 ) ) ;
#47002 = CARTESIAN_POINT ( 'NONE',  ( -6.009258394948636914E-15, 9.468750000682799595, -1.732050807568875195 ) ) ;
#47003 = CARTESIAN_POINT ( 'NONE',  ( 0.5400543498376106921, -2.107395444675621121, 0.7023712877645065245 ) ) ;
#47004 = EDGE_LOOP ( 'NONE', ( #88548, #65060, #37529, #107599 ) ) ;
#47005 = CARTESIAN_POINT ( 'NONE',  ( 6.883263157960371359, 6.037760411968411844, 2.441088155713948549 ) ) ;
#47006 = CARTESIAN_POINT ( 'NONE',  ( 1.499999999999989120, 3.004166666666689522, 0.8660254037844524744 ) ) ;
#47007 = CARTESIAN_POINT ( 'NONE',  ( 4.150767584078112193, 7.994312614733129152, 0.7998128361456321445 ) ) ;
#47008 = CARTESIAN_POINT ( 'NONE',  ( 1.506789913206330489, -2.211016841974380309, -0.2134033219785695379 ) ) ;
#47009 = CARTESIAN_POINT ( 'NONE',  ( -2.324088772396477673E-16, -1.093749999044084653, -3.475000000000000089 ) ) ;
#47010 = CARTESIAN_POINT ( 'NONE',  ( 8.161645285746708112, 9.584636257201740506, -1.082531754730543083 ) ) ;
#47011 = CARTESIAN_POINT ( 'NONE',  ( 0.4241069589249533700, 7.990617654048686624, 1.998204128839474958 ) ) ;
#47012 = CARTESIAN_POINT ( 'NONE',  ( 3.366167277942881064, 7.149221934233827014, -0.7998128361456362523 ) ) ;
#47013 = AXIS2_PLACEMENT_3D ( 'NONE', #143677, #127474, #209670 ) ;
#47014 = CARTESIAN_POINT ( 'NONE',  ( -0.03452862918938356951, -1.956592590566148093, -0.4871966601913205186 ) ) ;
#47016 = CARTESIAN_POINT ( 'NONE',  ( 5.072745416573516408, 1.424789591659934684, -1.491725785151225336 ) ) ;
#47015 = CARTESIAN_POINT ( 'NONE',  ( 8.530051201292206287, 13.10347683481629488, 0.000000000000000000 ) ) ;
#47017 = DIRECTION ( 'NONE',  ( -0.000000000000000000, -1.000000000000000000, -0.000000000000000000 ) ) ;
#47018 = CARTESIAN_POINT ( 'NONE',  ( -4.776550190716183586, 4.467063398790632966, 1.214306433183764966E-14 ) ) ;
#47019 = CARTESIAN_POINT ( 'NONE',  ( -1.001543065824772872E-14, 5.493750000682816825, 1.732050807568877637 ) ) ;
#47020 = CARTESIAN_POINT ( 'NONE',  ( 0.6823417656249899377, 1.592708333674752730, 1.181850606188755259 ) ) ;
#47021 = CARTESIAN_POINT ( 'NONE',  ( 0.2800358821246723418, -1.714356997462190835, -0.4388462949536375279 ) ) ;
#47022 = CARTESIAN_POINT ( 'NONE',  ( 5.484916526786003388, -1.734343006517705676, 0.008455456694493946809 ) ) ;
#47023 = CARTESIAN_POINT ( 'NONE',  ( 4.897892112245933127, -0.5929259483795108476, -1.636466244661118452 ) ) ;
#47024 = CARTESIAN_POINT ( 'NONE',  ( 4.695201269034174452, 4.372156323494968966, 1.214306433183764966E-14 ) ) ;
#47025 = CARTESIAN_POINT ( 'NONE',  ( 3.122906911094673887, 0.05843746759831092152, 2.291794357358638123 ) ) ;
#47026 = CARTESIAN_POINT ( 'NONE',  ( -0.6823417656249969321, 5.530208333674756283, -1.181850606188749264 ) ) ;
#47027 = CARTESIAN_POINT ( 'NONE',  ( 1.657894046870052485, -1.302874822933766774, 1.301145727299134025 ) ) ;
#47028 = AXIS2_PLACEMENT_3D ( 'NONE', #50168, #64288, #184414 ) ;
#47029 = DIRECTION ( 'NONE',  ( -0.000000000000000000, -1.000000000000000000, -0.000000000000000000 ) ) ;
#47030 = CARTESIAN_POINT ( 'NONE',  ( -11.82542156384632293, 8.168199132635775683, -2.262599552454852336 ) ) ;
#47031 = CARTESIAN_POINT ( 'NONE',  ( 2.291784574284541964, -0.7830779901500490858, 1.649245556672715995 ) ) ;
#47032 = CARTESIAN_POINT ( 'NONE',  ( 2.338517726396415863, 0.5350873343827439177, -1.944071628254496087 ) ) ;
#47033 = CARTESIAN_POINT ( 'NONE',  ( 1.746283639092637729, 0.6896231194409886411, 2.080178558289603963 ) ) ;
#47034 = CARTESIAN_POINT ( 'NONE',  ( 8.745069225198347951, 13.65147899241842744, -7.752220443290712026 ) ) ;
#47035 = CARTESIAN_POINT ( 'NONE',  ( 4.190527447551747109, -2.082725220463335081, -0.3111483248238402499 ) ) ;
#47036 = CARTESIAN_POINT ( 'NONE',  ( -6.015013705957189316, 10.16926642359206134, 0.7998128361456481317 ) ) ;
#47037 = CARTESIAN_POINT ( 'NONE',  ( 8.060410475752370019, 13.54723888396606135, 8.643090488201771393 ) ) ;
#47038 = CARTESIAN_POINT ( 'NONE',  ( 1.416557266959647787, 0.8372786474034592530, 1.893679232998768391 ) ) ;
#47039 = CARTESIAN_POINT ( 'NONE',  ( 5.840865249388943248, 5.708764300575555062, 0.7998128361456341429 ) ) ;
#47040 = CARTESIAN_POINT ( 'NONE',  ( -2.353626204688216217E-14, 2.828125000341407347, -1.570758158831798257 ) ) ;
#47041 = CARTESIAN_POINT ( 'NONE',  ( 3.844477943020713440, 1.133112341739877849, -1.792160191984671691 ) ) ;
#47042 = CARTESIAN_POINT ( 'NONE',  ( 6.656878040733529289, -1.407521694628325770, 1.162499734694094844 ) ) ;
#47043 = ORIENTED_EDGE ( 'NONE', *, *, #42234, .T. ) ;
#47044 = CARTESIAN_POINT ( 'NONE',  ( -6.330731382938325602, 6.350551133041632212, 0.7998128361456281477 ) ) ;
#47045 = EDGE_CURVE ( 'NONE', #35911, #158170, #31617, .T. ) ;
#47046 = CARTESIAN_POINT ( 'NONE',  ( 8.992082194361556091, 11.51384853155376220, 1.599625672291279388 ) ) ;
#47047 = CARTESIAN_POINT ( 'NONE',  ( 7.160114521348466710, 7.526090827760914870, 0.000000000000000000 ) ) ;
#47048 = CARTESIAN_POINT ( 'NONE',  ( 3.475000000000000533, -2.581249999044084475, 0.000000000000000000 ) ) ;
#47049 = CARTESIAN_POINT ( 'NONE',  ( -6.403528624356093601, 6.365204904703887223, 1.040834085586084257E-14 ) ) ;
#47050 = CARTESIAN_POINT ( 'NONE',  ( 6.029554895997981667, -0.2579198037528374066, 2.104758538420265168 ) ) ;
#47051 = CARTESIAN_POINT ( 'NONE',  ( 0.6398468662271715734, -1.489381099377089512, -1.489160694218383485 ) ) ;
#47052 = CARTESIAN_POINT ( 'NONE',  ( -4.294900800479008574, 8.232744377192641849, 0.000000000000000000 ) ) ;
#47053 = CARTESIAN_POINT ( 'NONE',  ( 8.052653171512838881, 11.48218023581863001, -1.199719254218446718 ) ) ;
#47054 = CARTESIAN_POINT ( 'NONE',  ( 4.926513725511825648, -1.217676453003987191, 1.407301474667689956 ) ) ;
#47055 = CARTESIAN_POINT ( 'NONE',  ( 7.239163954692881653, 10.53310948286200599, -1.199719254218441611 ) ) ;
#47056 = DIRECTION ( 'NONE',  ( -1.000000000000000000, 0.000000000000000000, 0.000000000000000000 ) ) ;
#47057 = CARTESIAN_POINT ( 'NONE',  ( -3.149236820124241110, 6.896136400112061970, -0.7998128361456481317 ) ) ;
#47058 = CARTESIAN_POINT ( 'NONE',  ( -8.622622508611375025, 12.04318144581317895, 1.082531754730560403 ) ) ;
#47060 = CARTESIAN_POINT ( 'NONE',  ( 1.890992312513404716, 0.1891058464698439912, 1.952711869325058691 ) ) ;
#47059 = CARTESIAN_POINT ( 'NONE',  ( -5.357443255694392725, 9.402100898285455699, 0.000000000000000000 ) ) ;
#47061 = CARTESIAN_POINT ( 'NONE',  ( 1.147603855448702248, -1.704515299458901012, -1.329379018566230641 ) ) ;
#47063 = CARTESIAN_POINT ( 'NONE',  ( -5.511734814698080243, 6.408623376260899285, 1.272316098655206229 ) ) ;
#47062 = CARTESIAN_POINT ( 'NONE',  ( -5.936491157937300756, 8.019268665717216749, 1.599625672291263179 ) ) ;
#47064 = CARTESIAN_POINT ( 'NONE',  ( -0.6823417656250246877, 0.5510416670080897639, 1.181850606188755259 ) ) ;
#47065 = CARTESIAN_POINT ( 'NONE',  ( 2.846726617453724906, -0.8940771029739991160, 1.485372309294562543 ) ) ;
#47066 = CARTESIAN_POINT ( 'NONE',  ( 2.202700171921621042, -0.3823900931277899318, 1.697618373880743325 ) ) ;
#47068 = CARTESIAN_POINT ( 'NONE',  ( 7.293923454472087897, 8.572294120714675003, 1.082531754730558626 ) ) ;
#47067 = CARTESIAN_POINT ( 'NONE',  ( 6.727182134110239353, -0.007837387828812587484, 2.289081727344749684 ) ) ;
#47069 = CARTESIAN_POINT ( 'NONE',  ( -11.82198925196379946, 4.889592154110854239, -4.884635108899213485 ) ) ;
#47070 = CARTESIAN_POINT ( 'NONE',  ( 2.337248977212981860, -1.842284197780035493, 0.9235709308827669828 ) ) ;
#47071 = CARTESIAN_POINT ( 'NONE',  ( 0.6497672626537411844, -0.2439889887937417567, -2.001205234435725622 ) ) ;
#47072 = CARTESIAN_POINT ( 'NONE',  ( 6.825078400183554272, 2.951006455646578264, 2.596623860847916188 ) ) ;
#47073 = CARTESIAN_POINT ( 'NONE',  ( -3.800028193580205382, 7.655393002477360653, -0.7998128361456481317 ) ) ;
#47074 = CARTESIAN_POINT ( 'NONE',  ( 1.305477374917118016, -0.4809445013957516779, 1.911780493352131183 ) ) ;
#47076 = CARTESIAN_POINT ( 'NONE',  ( -5.139949633356594383, 9.010708648975750634, 0.000000000000000000 ) ) ;
#47075 = CARTESIAN_POINT ( 'NONE',  ( 5.625241921295836889, 1.689600096388569561, 0.8957793909229803120 ) ) ;
#47077 = CARTESIAN_POINT ( 'NONE',  ( -5.763624699140874164, 8.777960344756069233, -1.082531754730549967 ) ) ;
#47078 = CARTESIAN_POINT ( 'NONE',  ( 6.933015448541703485, 9.181880338089085214, 1.599625672291268286 ) ) ;
#47079 = CARTESIAN_POINT ( 'NONE',  ( -6.851666526859749418, 9.086973262793417661, -1.599625672291271394 ) ) ;
#47080 = CARTESIAN_POINT ( 'NONE',  ( 0.6627674568651781284, 0.5885975752501994007, 1.931983969097182063 ) ) ;
#47081 = CARTESIAN_POINT ( 'NONE',  ( 3.321384445223568793, 6.818772919495456719, -0.7216878364870045193 ) ) ;
#47082 = CARTESIAN_POINT ( 'NONE',  ( 5.122255714018879580, -1.229368216938999003, -1.952684467508845056 ) ) ;
#47083 = CARTESIAN_POINT ( 'NONE',  ( 5.512146440779991607, 1.959692598237902761, -0.09458084330612320789 ) ) ;
#47084 = CARTESIAN_POINT ( 'NONE',  ( 1.657006586592904673, 1.606862555911577006, -1.125131163738995577 ) ) ;
#47085 = CARTESIAN_POINT ( 'NONE',  ( 8.452618703115982512, 11.94880668935564216, 1.199719254218450271 ) ) ;
#47086 = CARTESIAN_POINT ( 'NONE',  ( -9.453683584308942400, 14.52894124707535717, 7.391106286152997917 ) ) ;
#47087 = ORIENTED_EDGE ( 'NONE', *, *, #151210, .T. ) ;
#47088 = CARTESIAN_POINT ( 'NONE',  ( 1.112693368687894369, 2.042276985739148731, 0.5586806735067056939 ) ) ;
#47090 = CARTESIAN_POINT ( 'NONE',  ( -7.100719765255177229, 9.307259030929609267, -1.599625672291263179 ) ) ;
#47089 = CARTESIAN_POINT ( 'NONE',  ( -5.545448523189368650, 6.428443684264421698, -1.199719254218446718 ) ) ;
#47091 = CARTESIAN_POINT ( 'NONE',  ( 0.7789528443887736575, 1.234723402293058214, 1.365900241759879119 ) ) ;
#47092 = ORIENTED_EDGE ( 'NONE', *, *, #191961, .T. ) ;
#47094 = CIRCLE ( 'NONE', #150981, 0.08000000000000020983 ) ;
#47093 = CARTESIAN_POINT ( 'NONE',  ( 4.311506836774354312, -1.801752502381037457, -1.211023186257336404 ) ) ;
#47095 = B_SPLINE_CURVE_WITH_KNOTS ( 'NONE', 3,
 ( #179300, #30921, #147862, #96997, #146814, #196602, #48243, #114356 ),
 .UNSPECIFIED., .F., .F.,
 ( 4, 2, 2, 4 ),
 ( 0.000000000000000000, 0.0003954713701971457199, 0.0005932070552957175499, 0.0007909427403942893798 ),
 .UNSPECIFIED. ) ;
#47096 = CARTESIAN_POINT ( 'NONE',  ( 11.88154125640529912, 7.838767436447524162, -1.736782259460240452 ) ) ;
#47097 = CARTESIAN_POINT ( 'NONE',  ( 1.424255164902767934, -2.103954720533041556, 0.2648648325892372646 ) ) ;
#47098 = CARTESIAN_POINT ( 'NONE',  ( 0.7499999999999902300, 2.764583334016148974, 1.299038105676669330 ) ) ;
#47099 = CARTESIAN_POINT ( 'NONE',  ( 7.564559641420864899, 10.91273778404466199, -1.199719254218446718 ) ) ;
#47100 = SURFACE_SIDE_STYLE ('',( #29770 ) ) ;
#47101 = ORIENTED_EDGE ( 'NONE', *, *, #176346, .T. ) ;
#47102 = CARTESIAN_POINT ( 'NONE',  ( 3.093097461593071973, 1.769307450888421673, -1.056303779743078985 ) ) ;
#47104 = CARTESIAN_POINT ( 'NONE',  ( 0.5558949066124979632, -1.334021266253348381, 1.269314063962425854 ) ) ;
#47103 = CARTESIAN_POINT ( 'NONE',  ( -7.343712760096452463, 11.71941532008788833, -0.7998128361456291469 ) ) ;
#47105 = CARTESIAN_POINT ( 'NONE',  ( -0.6823417656250212460, 3.551041667008085323, 1.181850606188767472 ) ) ;
#47106 = CARTESIAN_POINT ( 'NONE',  ( -0.02264175331116376200, 2.864903628641465971, -2.577409799940860946 ) ) ;
#47107 = CARTESIAN_POINT ( 'NONE',  ( 10.91944002402978775, -9.999999999999994671, -0.1105873483556677611 ) ) ;
#47108 = CARTESIAN_POINT ( 'NONE',  ( 0.3994152196779980346, 1.832435997337564348, -1.229551327501000380 ) ) ;
#47109 = CARTESIAN_POINT ( 'NONE',  ( 2.091474534086060544, 1.969063197997424686, -1.113951356575371365 ) ) ;
#47110 = CARTESIAN_POINT ( 'NONE',  ( -9.842856333841300653, 10.58567993234409421, 0.7216878364870438212 ) ) ;
#47111 = CARTESIAN_POINT ( 'NONE',  ( 2.302729407678519191, -0.3129977310964130455, -1.784170229015415332 ) ) ;
#47112 = CARTESIAN_POINT ( 'NONE',  ( 2.395587962911712498, -1.894220731477358921, 0.2854614921951497686 ) ) ;
#47113 = CARTESIAN_POINT ( 'NONE',  ( 3.332542965736586371, -1.235447621225284509, 1.661183390374972424 ) ) ;
#47114 = CARTESIAN_POINT ( 'NONE',  ( 1.364683531249988757, 1.946875000341415030, 0.000000000000000000 ) ) ;
#47115 = CARTESIAN_POINT ( 'NONE',  ( 1.375784083019690351, 1.172551417808114893, 1.584734682399450145 ) ) ;
#47116 = CARTESIAN_POINT ( 'NONE',  ( 6.721331456258776704, -0.1291123375851965516, 1.896827325797964869 ) ) ;
#47117 = CARTESIAN_POINT ( 'NONE',  ( 2.535844406030359544, 0.8837261853790435717, -1.648756255988912400 ) ) ;
#47118 = EDGE_CURVE ( 'NONE', #164652, #3975, #69602, .T. ) ;
#47120 = CARTESIAN_POINT ( 'NONE',  ( 4.616554244727909762, 8.463227371007752353, -0.2998622348379786362 ) ) ;
#47119 = CARTESIAN_POINT ( 'NONE',  ( 0.9796492596481393145, -0.06170110713811990943, -2.307032891211552084 ) ) ;
#47121 = CARTESIAN_POINT ( 'NONE',  ( 2.910441987356562787, 0.6243205138760847817, 1.753359951907756065 ) ) ;
#47122 = CARTESIAN_POINT ( 'NONE',  ( -0.6823417656250003738, 2.467708333674753618, -1.181850606188749264 ) ) ;
#47123 = AXIS2_PLACEMENT_3D ( 'NONE', #45989, #61146, #15571 ) ;
#47124 = CARTESIAN_POINT ( 'NONE',  ( 5.705554990011762584, -1.623920158085298437, -1.271698733341574350 ) ) ;
#47125 = CARTESIAN_POINT ( 'NONE',  ( -4.238895582566952314, 8.097128612970093897, 1.040834085586084257E-14 ) ) ;
#47126 = CARTESIAN_POINT ( 'NONE',  ( 6.751070424600909448, 9.963667031088037973, -1.199719254218441611 ) ) ;
#47127 = CARTESIAN_POINT ( 'NONE',  ( -1.467608305004828750, 3.323697079694280632, -0.3199191423968864023 ) ) ;
#47128 = CARTESIAN_POINT ( 'NONE',  ( 6.721705546354253435, -2.043712959172855115, 0.5078683761520035311 ) ) ;
#47129 = PRESENTATION_LAYER_ASSIGNMENT (  '', '', ( #154403 ) ) ;
#47130 = CARTESIAN_POINT ( 'NONE',  ( -0.6823417656250212460, 2.363541667008084435, 1.181850606188767472 ) ) ;
#47131 = CARTESIAN_POINT ( 'NONE',  ( 5.448557382023540896, 0.6217387762853660016, 2.070273951448368788 ) ) ;
#47132 = CARTESIAN_POINT ( 'NONE',  ( -0.07004771093476865051, -1.979950378243084730, 0.3982260095720979165 ) ) ;
#47133 = CARTESIAN_POINT ( 'NONE',  ( -0.6823417656250003738, -0.5322916663252491576, -1.181850606188749264 ) ) ;
#47134 = CARTESIAN_POINT ( 'NONE',  ( -4.934804725694224459, 6.780358151441803649, -1.443375672974053447 ) ) ;
#47137 = CARTESIAN_POINT ( 'NONE',  ( 4.853455804012216213, 6.685451076146141425, 1.443375672974062551 ) ) ;
#47136 = CARTESIAN_POINT ( 'NONE',  ( 3.285556943749998737, -0.6052083328553753416, -1.896917185911906500 ) ) ;
#47135 = CARTESIAN_POINT ( 'NONE',  ( 6.200875153403774043, 8.327716660428123419, -1.599625672291283607 ) ) ;
#47138 = CARTESIAN_POINT ( 'NONE',  ( -4.736594563127865420, 6.619389305106191834, -1.599625672291271394 ) ) ;
#47139 = CARTESIAN_POINT ( 'NONE',  ( 4.856657812281613751, -1.900414607462055816, -0.6748505307947461063 ) ) ;
#47140 = CARTESIAN_POINT ( 'NONE',  ( -8.850775351622791831, 9.220326086515070685, -0.7998128361456291469 ) ) ;
#47142 = CARTESIAN_POINT ( 'NONE',  ( -5.872089928050201024, 8.904503111816948646, 1.082531754730550855 ) ) ;
#47141 = CARTESIAN_POINT ( 'NONE',  ( -10.33094986393327197, 11.15512238411806578, 0.7216878364870438212 ) ) ;
#47143 = ADVANCED_BREP_SHAPE_REPRESENTATION ( '', ( #168834, #155333, #158197, #164931, #94059, #158894, #89439, #161027, #24912, #162819, #169543, #162104, #106770, #200407 ), #124915 ) ;
#47144 = CARTESIAN_POINT ( 'NONE',  ( -1.364683531250012516, 4.988541667008084879, -0.7879004041258300672 ) ) ;
#47146 = CARTESIAN_POINT ( 'NONE',  ( -1.364683531250000748, 9.359375000341396245, 0.000000000000000000 ) ) ;
#47145 = CARTESIAN_POINT ( 'NONE',  ( 5.682550338946039226, -2.108058120380253087, -0.4779004524640489970 ) ) ;
#47147 = CARTESIAN_POINT ( 'NONE',  ( -11.78331023100045627, 13.79999999999998295, 1.799999999999999600 ) ) ;
#47148 = CARTESIAN_POINT ( 'NONE',  ( -11.81677561662610110, 7.791008328563874485, 1.827277289630534929 ) ) ;
#47150 = CARTESIAN_POINT ( 'NONE',  ( 5.536732523015378327, -1.587826920732600122, 1.242742243127918700 ) ) ;
#47149 = CARTESIAN_POINT ( 'NONE',  ( -5.544921637864820951, 9.412899644243539754, -0.7216878364870207285 ) ) ;
#47151 = CARTESIAN_POINT ( 'NONE',  ( -1.364683531250000748, -0.6781249996585803075, 0.000000000000000000 ) ) ;
#47152 = EDGE_CURVE ( 'NONE', #188684, #50747, #18885, .T. ) ;
#47153 = CARTESIAN_POINT ( 'NONE',  ( 2.279564191164831666, 1.060311948399524695, 1.360390198354200386 ) ) ;
#47154 = CARTESIAN_POINT ( 'NONE',  ( 4.899292406491845497, 6.809203455697518947, -1.599625672291273171 ) ) ;
#47156 = CARTESIAN_POINT ( 'NONE',  ( 8.005163354226054295, 8.304055099544019214, 0.000000000000000000 ) ) ;
#47155 = CARTESIAN_POINT ( 'NONE',  ( 7.049876689426101350, 9.247942109129029475, -1.443375672974057666 ) ) ;
#47157 = CARTESIAN_POINT ( 'NONE',  ( -11.13073163568576263, 7.259140372625044080, -4.368349261952645612 ) ) ;
#47158 = CARTESIAN_POINT ( 'NONE',  ( 6.872336254976084469, -1.150436037642876608, 1.475500831757702969 ) ) ;
#47159 = CARTESIAN_POINT ( 'NONE',  ( 0.4869769290230832048, -1.896302947978160791, -0.6760925243112311245 ) ) ;
#47160 = DIRECTION ( 'NONE',  ( 0.000000000000000000, -1.000000000000000000, 0.000000000000000000 ) ) ;
#47162 = AXIS2_PLACEMENT_3D ( 'NONE', #92209, #71631, #173449 ) ;
#47161 = CARTESIAN_POINT ( 'NONE',  ( 3.135963548190400019, -1.480894843444351849, -1.636267651353009223 ) ) ;
#47163 = CARTESIAN_POINT ( 'NONE',  ( 5.928641807120487606, -1.383276364288194893, 1.673324517764721575 ) ) ;
#47164 = ORIENTED_EDGE ( 'NONE', *, *, #28177, .F. ) ;
#47165 = B_SPLINE_CURVE_WITH_KNOTS ( 'NONE', 3,
 ( #202647, #75871, #124710, #190669, #5500, #122588 ),
 .UNSPECIFIED., .F., .F.,
 ( 4, 2, 4 ),
 ( 0.000000000000000000, 0.0003155923098472861849, 0.0006311846196945723698 ),
 .UNSPECIFIED. ) ;
#47166 = CARTESIAN_POINT ( 'NONE',  ( 5.246079093845007257, 5.085123462432798114, 0.7998128361456352531 ) ) ;
#47167 = CARTESIAN_POINT ( 'NONE',  ( 8.717529583462646059, 11.19353715217169309, 1.443375672974076540 ) ) ;
#47169 = CARTESIAN_POINT ( 'NONE',  ( 2.214470461757975794, 1.956567829827577931, 0.4871813834786202224 ) ) ;
#47168 = CARTESIAN_POINT ( 'NONE',  ( 2.684367718930933844, 1.136400967617630986, 1.790090880730066392 ) ) ;
#47171 = ORIENTED_EDGE ( 'NONE', *, *, #52529, .F. ) ;
#47170 = CARTESIAN_POINT ( 'NONE',  ( 2.214858347191206445, 1.452946758456060250, -1.081763258146416939 ) ) ;
#47172 = CARTESIAN_POINT ( 'NONE',  ( 6.333594036239346359, 7.418223126147930557, 1.199719254218453823 ) ) ;
#47173 = ORIENTED_EDGE ( 'NONE', *, *, #157223, .F. ) ;
#47174 = CARTESIAN_POINT ( 'NONE',  ( 4.625302960556422427, 8.547937220624488575, 1.040834085586084257E-14 ) ) ;
#47176 = CARTESIAN_POINT ( 'NONE',  ( 0.9717394072371825509, -0.8581575513351351603, 1.712793540333819919 ) ) ;
#47175 = CARTESIAN_POINT ( 'NONE',  ( -3.307299406729781399, 5.945934176904983381, -1.199719254218452935 ) ) ;
#47177 = CARTESIAN_POINT ( 'NONE',  ( 0.3868823266961737839, 2.515145635913770494, -11.70808416779823524 ) ) ;
#47178 = DIRECTION ( 'NONE',  ( 3.497202527569253358E-15, -0.000000000000000000, 1.000000000000000000 ) ) ;
#47179 = CARTESIAN_POINT ( 'NONE',  ( 6.778713616708431644, 7.010846762355714468, 1.040834085586084257E-14 ) ) ;
#47180 = CARTESIAN_POINT ( 'NONE',  ( -1.402160292154681736E-14, -0.1156249996585793222, 1.575800808251672791 ) ) ;
#47181 = DIRECTION ( 'NONE',  ( 0.000000000000000000, -1.000000000000000000, 0.000000000000000000 ) ) ;
#47182 = CARTESIAN_POINT ( 'NONE',  ( -9.429859533504656000, 10.96025652963230534, -1.199719254218441611 ) ) ;
#47183 = MECHANICAL_DESIGN_GEOMETRIC_PRESENTATION_REPRESENTATION (  '', ( #50555 ), #92188 ) ;
#47184 = CARTESIAN_POINT ( 'NONE',  ( 4.926735330553583481, 2.067573386176469796, 0.6309256262674378668 ) ) ;
#47185 = CARTESIAN_POINT ( 'NONE',  ( -4.990809943606281607, 6.915973915664348937, -1.443375672974066548 ) ) ;
#47186 = EDGE_CURVE ( 'NONE', #86388, #24037, #11258, .T. ) ;
#47187 = CARTESIAN_POINT ( 'NONE',  ( 5.478903473698239601, 7.485416367438324059, -1.443375672974078761 ) ) ;
#47188 = CARTESIAN_POINT ( 'NONE',  ( 1.406653384705614629, -2.110883996484512970, -0.2024971186788473154 ) ) ;
#47190 = CARTESIAN_POINT ( 'NONE',  ( -11.38502332509229831, 5.468749262791421373, -5.576278951475440948 ) ) ;
#47189 = CARTESIAN_POINT ( 'NONE',  ( 0.07933194154487524519, -7.246166700194011767, -9.499668754385622194 ) ) ;
#47191 = CARTESIAN_POINT ( 'NONE',  ( 3.356668533229437923, -1.495150621271496671, 1.284956859879735402 ) ) ;
#47192 = CARTESIAN_POINT ( 'NONE',  ( 5.677967274442059953, 1.882970570262190835, -0.3333453579756898155 ) ) ;
#47193 = ORIENTED_EDGE ( 'NONE', *, *, #36937, .T. ) ;
#47194 = CARTESIAN_POINT ( 'NONE',  ( 0.1685321339487330372, -0.8835925182541467526, -1.870455940253319183 ) ) ;
#47195 = CARTESIAN_POINT ( 'NONE',  ( 2.378764330827160212, 1.775374922424903801, -0.7872989649762071052 ) ) ;
#47196 = ORIENTED_EDGE ( 'NONE', *, *, #165187, .T. ) ;
#47197 = DIRECTION ( 'NONE',  ( 0.000000000000000000, 1.000000000000000000, 0.000000000000000000 ) ) ;
#47199 = CARTESIAN_POINT ( 'NONE',  ( 5.840530312436913007, 10.03597880781023299, 0.000000000000000000 ) ) ;
#47198 = CARTESIAN_POINT ( 'NONE',  ( -5.790741006812557323, 9.769965251341050205, 0.000000000000000000 ) ) ;
#47201 = CARTESIAN_POINT ( 'NONE',  ( 6.844168616800228477, 6.879284895888727824, -0.7998128361456281477 ) ) ;
#47200 = CARTESIAN_POINT ( 'NONE',  ( 2.677772397998368081, -1.073972967945693080, 1.793542233829773291 ) ) ;
#47202 = CARTESIAN_POINT ( 'NONE',  ( 5.844973620822844218, 5.991759777147701804, 0.7216878364870328300 ) ) ;
#47204 = ORIENTED_EDGE ( 'NONE', *, *, #94657, .T. ) ;
#47203 = CARTESIAN_POINT ( 'NONE',  ( 6.445967652843097362, -1.252902786447611883, -1.444740716957277904 ) ) ;
#47205 = CARTESIAN_POINT ( 'NONE',  ( 4.811249113497881424, 1.919052844561389692, 1.089612025192594258 ) ) ;
#47206 = CARTESIAN_POINT ( 'NONE',  ( 2.696532018272995490, -2.200798769047443759, -0.1632673417703081331 ) ) ;
#47207 = CARTESIAN_POINT ( 'NONE',  ( 7.259501185113382604, 10.55683625168592243, -1.199719254218441611 ) ) ;
#47208 = CARTESIAN_POINT ( 'NONE',  ( -11.89839339040395139, 12.27122531596087818, 1.560885614203548100 ) ) ;
#47209 = EDGE_CURVE ( 'NONE', #66179, #75921, #69763, .T. ) ;
#47210 = CARTESIAN_POINT ( 'NONE',  ( 1.840342752298686380, 1.099902316243700939, -1.564109231055022864 ) ) ;
#47211 = DIRECTION ( 'NONE',  ( 0.000000000000000000, -1.000000000000000000, 0.000000000000000000 ) ) ;
#47212 = CARTESIAN_POINT ( 'NONE',  ( 8.374132434735052755, 12.92157160716627295, -0.7998128361456352531 ) ) ;
#47213 = CARTESIAN_POINT ( 'NONE',  ( 4.527825515032589898, 2.008996319933327612, -0.4998958796476050681 ) ) ;
#47214 = CARTESIAN_POINT ( 'NONE',  ( 1.885829143180400624, 1.490600019384461072, 1.565824011241300440 ) ) ;
#47215 = CARTESIAN_POINT ( 'NONE',  ( 5.337503337980974649, 0.8888059580158399475, -2.003405333693850654 ) ) ;
#47216 = CARTESIAN_POINT ( 'NONE',  ( -5.845336483073759304, 6.639953436172111978, 0.9360796054654503262 ) ) ;
#47217 = CARTESIAN_POINT ( 'NONE',  ( -0.2791710057858245442, 8.178600120975007215, 1.982899171336969912 ) ) ;
#47218 = CARTESIAN_POINT ( 'NONE',  ( 6.086684617892325733, 6.065829907154645539, -0.7998128361456481317 ) ) ;
#47219 = CARTESIAN_POINT ( 'NONE',  ( 0.6823417656249969321, 14.08854166700806232, -1.181850606188757036 ) ) ;
#47220 = CARTESIAN_POINT ( 'NONE',  ( -3.657667580636712934, 7.489305620709952649, -0.7998128361456481317 ) ) ;
#47221 = CARTESIAN_POINT ( 'NONE',  ( 0.7564826839323666174, 1.942540863013635821, -0.5404934282097761944 ) ) ;
#47222 = CARTESIAN_POINT ( 'NONE',  ( -8.568389894156720032, 10.05917163368005163, 1.082531754730558626 ) ) ;
#47223 = CARTESIAN_POINT ( 'NONE',  ( 5.243061650278370678, -0.2479348644398685908, -2.055265572831247667 ) ) ;
#47224 = CARTESIAN_POINT ( 'NONE',  ( 3.334515964829305457, 1.879714267205140565, 0.4213298384171912381 ) ) ;
#47225 = CARTESIAN_POINT ( 'NONE',  ( 5.730101960677154160, 2.114805460001396575, 0.1033778851832044821 ) ) ;
#47226 = CARTESIAN_POINT ( 'NONE',  ( 4.123651276850781144, 7.962676922967908411, -0.7998128361456221525 ) ) ;
#47228 = ADVANCED_FACE ( 'NONE', ( #2625 ), #104434, .F. ) ;
#47227 = CARTESIAN_POINT ( 'NONE',  ( 9.367496997597644537, 4.518459255873317204, 7.499999999999945821 ) ) ;
#47229 = CARTESIAN_POINT ( 'NONE',  ( 4.293777937636614972, -1.355062202172536034, -1.429424366026492033 ) ) ;
#47230 = CARTESIAN_POINT ( 'NONE',  ( 5.543040349607136541, -1.804139640619137230, -1.413977440569001542 ) ) ;
#47231 = CARTESIAN_POINT ( 'NONE',  ( 4.248545464119923842, 0.4890907236730773766, 1.758887239191930796 ) ) ;
#47232 = PRODUCT_DEFINITION_SHAPE ( 'NONE', 'NONE',  #151058 ) ;
#47233 = EDGE_CURVE ( 'NONE', #193425, #135649, #118093, .T. ) ;
#47234 = CARTESIAN_POINT ( 'NONE',  ( 6.319508997745523438, 9.426492026461511742, -1.082531754730548412 ) ) ;
#47235 = CARTESIAN_POINT ( 'NONE',  ( 4.406036734316882253, 6.163462161501577441, -1.443375672974051449 ) ) ;
#47236 = CARTESIAN_POINT ( 'NONE',  ( -7.469616286486262524, 7.679250187180907794, 0.7998128361456341429 ) ) ;
#47237 = CARTESIAN_POINT ( 'NONE',  ( 6.204791576909545192, 7.267953590263130259, -1.199719254218452047 ) ) ;
#47238 = VERTEX_POINT ( 'NONE', #154250 ) ;
#47240 = CARTESIAN_POINT ( 'NONE',  ( 5.203390118303760303, 1.773417465902687562, -0.9529421280250712778 ) ) ;
#47239 = CARTESIAN_POINT ( 'NONE',  ( 0.9953642579336658969, -1.841430844361633845, 2.783310008858119066E-05 ) ) ;
#47241 = CARTESIAN_POINT ( 'NONE',  ( 6.240923344934847350, 2.292853006454723452, -0.1649963611656188323 ) ) ;
#47242 = CARTESIAN_POINT ( 'NONE',  ( 5.084793414397763556, 1.876112756342168675, 0.5732009990792874543 ) ) ;
#47243 = CARTESIAN_POINT ( 'NONE',  ( -6.989391883044787868, 8.113044270762433285, -1.199719254218446718 ) ) ;
#47244 = AXIS2_PLACEMENT_3D ( 'NONE', #197633, #185644, #166207 ) ;
#47245 = CARTESIAN_POINT ( 'NONE',  ( -3.764360206088648297, 7.543504007078730922, -0.7998128361456281477 ) ) ;
#47246 = CARTESIAN_POINT ( 'NONE',  ( -10.00050683067327384, 3.975933801733735784, -5.773795310721868468 ) ) ;
#47247 = CARTESIAN_POINT ( 'NONE',  ( -5.960744811863571968, 6.983232364376142698, 1.199719254218452935 ) ) ;
#47249 = CARTESIAN_POINT ( 'NONE',  ( 0.6021629784135495989, -0.6261829430146518272, -1.762877433595814614 ) ) ;
#47248 = CARTESIAN_POINT ( 'NONE',  ( 1.417645169044414288, -1.164320182712182294, -1.736329362061867387 ) ) ;
#47250 = CARTESIAN_POINT ( 'NONE',  ( -7.777446446097295407, -5.502990254781792601, 7.779015489124650351 ) ) ;
#47251 = CARTESIAN_POINT ( 'NONE',  ( 5.771417317170061345, 1.158396453637217993, 1.558476049558398913 ) ) ;
#47252 = CARTESIAN_POINT ( 'NONE',  ( -0.2104748580754201015, 7.629137130509078268, -2.703678718140526627 ) ) ;
#47253 = CARTESIAN_POINT ( 'NONE',  ( 0.6787880507331369717, 1.167388449615349044, 1.291009837513588998 ) ) ;
#47254 = CARTESIAN_POINT ( 'NONE',  ( 5.425234023762710578, 9.481190127698507553, -0.7998128361456291469 ) ) ;
#47255 = CARTESIAN_POINT ( 'NONE',  ( 5.999999999964367170E-05, 14.55305236562399607, 11.95586206881391433 ) ) ;
#47256 = CARTESIAN_POINT ( 'NONE',  ( 1.453258822912409043, 0.5037300415833938505, -1.649688963556243282 ) ) ;
#47257 = CARTESIAN_POINT ( 'NONE',  ( 1.997856853652695497, -2.190977152517746163, 0.05759783203293508680 ) ) ;
#47258 = CARTESIAN_POINT ( 'NONE',  ( 6.872404467231180369, -0.3655807773644218495, 1.700417682701503841 ) ) ;
#47259 = CARTESIAN_POINT ( 'NONE',  ( 4.459734715955371520, 0.4851516707722826061, -2.152740496749529608 ) ) ;
#47260 = CARTESIAN_POINT ( 'NONE',  ( -10.10707714348148301, 4.359868340440408829, -5.857196085253971063 ) ) ;
#47261 = CARTESIAN_POINT ( 'NONE',  ( 1.657326198882978385, 1.776537685197575822, -1.247748726553777221 ) ) ;
#47262 = CARTESIAN_POINT ( 'NONE',  ( 0.4514209555319322331, 0.5758240286459560542, -1.732582669633643047 ) ) ;
#47263 = CARTESIAN_POINT ( 'NONE',  ( 1.886098781581479145, -2.116736904955533571, 0.05756534462913154987 ) ) ;
#47264 = VERTEX_POINT ( 'NONE', #4749 ) ;
#47266 = CARTESIAN_POINT ( 'NONE',  ( 0.6823417656249882723, 0.4052083336747516751, 1.181850606188755259 ) ) ;
#47265 = CARTESIAN_POINT ( 'NONE',  ( 2.947136817621052618, -1.875550406973557349, -1.317825558608209713 ) ) ;
#47267 = CARTESIAN_POINT ( 'NONE',  ( 4.493637847925535667, 7.329995691633395261, -1.199719254218452047 ) ) ;
#47268 = CARTESIAN_POINT ( 'NONE',  ( 5.057398377711723292, -1.905748072847958108, 1.140992067822230505 ) ) ;
#47269 = CARTESIAN_POINT ( 'NONE',  ( -6.399085315970137522, 9.449054721065074602, -1.082531754730538864 ) ) ;
#47270 = CIRCLE ( 'NONE', #74925, 0.07999999999999994615 ) ;
#47271 = CARTESIAN_POINT ( 'NONE',  ( 4.528060117284232966, 6.305822774963486310, 1.443375672974062551 ) ) ;
#47272 = CARTESIAN_POINT ( 'NONE',  ( -7.985389288324703294, 9.379004260209384825, -1.082531754730543083 ) ) ;
#47273 = SHAPE_REPRESENTATION ( 'isolation positive negative', ( #200407 ), #151904 ) ;
#47274 = CARTESIAN_POINT ( 'NONE',  ( 3.770576118376306241, 6.452737000530752276, 1.082531754730549078 ) ) ;
#47276 = ORIENTED_EDGE ( 'NONE', *, *, #152637, .T. ) ;
#47275 = COLOUR_RGB ( '', 0.31764706, 0.68627451, 0.89019608) ;
#47277 = CARTESIAN_POINT ( 'NONE',  ( 2.496720397819631732, -1.994071314890283553, 0.2986276487200872354 ) ) ;
#47279 = CARTESIAN_POINT ( 'NONE',  ( 1.973554268250839350, -0.2567932339846226708, 2.046489673661837205 ) ) ;
#47278 = CARTESIAN_POINT ( 'NONE',  ( 7.019370843573166319, 9.212351955633947043, 1.599625672291281386 ) ) ;
#47280 = DIRECTION ( 'NONE',  ( -0.6716942845482061220, 0.000000000000000000, -0.7408284471490504952 ) ) ;
#47281 = CARTESIAN_POINT ( 'NONE',  ( 6.170369307550831017, 6.371388078330353366, 0.7216878364870328300 ) ) ;
#47282 = VERTEX_POINT ( 'NONE', #200824 ) ;
#47283 = CARTESIAN_POINT ( 'NONE',  ( -6.801849727212544217, -7.605490242344541407, -7.458876343101966455 ) ) ;
#47284 = CARTESIAN_POINT ( 'NONE',  ( -0.6823417656250212460, 5.301041667008086655, 1.181850606188767472 ) ) ;
#47285 = CARTESIAN_POINT ( 'NONE',  ( 4.769572470968366673, 1.260305947291120221, 1.792593939366843303 ) ) ;
#47286 = CARTESIAN_POINT ( 'NONE',  ( 2.356092462967720458, 0.09613450340887133572, -2.014232768679749430 ) ) ;
#47287 = CARTESIAN_POINT ( 'NONE',  ( 2.682954136603598272, 1.303717545168959990, 1.300458928786947688 ) ) ;
#47288 = CARTESIAN_POINT ( 'NONE',  ( 8.606728586576791074, 8.935604860628076906, 0.7998128361456462443 ) ) ;
#47289 = CARTESIAN_POINT ( 'NONE',  ( 5.174738384962677351, -1.719472664011096219, -0.6136495084824307167 ) ) ;
#47290 = CARTESIAN_POINT ( 'NONE',  ( 5.572888750952301073, -0.9041123360693378297, 1.802415994888312722 ) ) ;
#47291 = CARTESIAN_POINT ( 'NONE',  ( -7.609150525767646833, 9.900428251527500834, -1.599625672291263179 ) ) ;
#47293 = CARTESIAN_POINT ( 'NONE',  ( -5.336015975430226099, 8.383046517047350932, -1.199719254218453823 ) ) ;
#47292 = CARTESIAN_POINT ( 'NONE',  ( 5.155258101147136784, -1.908469616433384086, -1.214953784003909520 ) ) ;
#47294 = CARTESIAN_POINT ( 'NONE',  ( 0.8562495616285453748, 2.103569811481691865, -0.1051806538951201714 ) ) ;
#47295 = CARTESIAN_POINT ( 'NONE',  ( -5.562588163356775972, 9.711712967216715953, 0.7998128361456291469 ) ) ;
#47296 = CARTESIAN_POINT ( 'NONE',  ( 9.562578416340237197, 10.05076299535211781, 0.7998128361456462443 ) ) ;
#47297 = CARTESIAN_POINT ( 'NONE',  ( -10.12374542407608402, 0.7598076211376182387, 4.551898349974277558 ) ) ;
#47298 = DIRECTION ( 'NONE',  ( 0.000000000000000000, -1.000000000000000000, 0.000000000000000000 ) ) ;
#47299 = CARTESIAN_POINT ( 'NONE',  ( -8.259941899223614215, 10.65968485389279508, -1.599625672291263179 ) ) ;
#47300 = UNCERTAINTY_MEASURE_WITH_UNIT (LENGTH_MEASURE( 1.000000000000000082E-05 ), #129018, 'distance_accuracy_value', 'NONE');
#47301 = CARTESIAN_POINT ( 'NONE',  ( 3.553238514845298734, 7.337208092372121904, -0.2327671511505452484 ) ) ;
#47302 = CARTESIAN_POINT ( 'NONE',  ( 8.039058738260216330, 8.343599714250547805, -0.7998128361456341429 ) ) ;
#47303 = CARTESIAN_POINT ( 'NONE',  ( 5.770924896911269641, 6.051163903260999177, -0.5763553215429690901 ) ) ;
#47304 = CARTESIAN_POINT ( 'NONE',  ( -8.134528978519403708, 11.47373899403920205, 1.082531754730549967 ) ) ;
#47306 = CARTESIAN_POINT ( 'NONE',  ( 2.654761906407083760, 2.205155901917950967, 0.2675573109941364880 ) ) ;
#47305 = CARTESIAN_POINT ( 'NONE',  ( 1.758217466200185042, 0.8068918862002281145, -1.961288232260410380 ) ) ;
#47307 = FACE_OUTER_BOUND ( 'NONE', #43450, .T. ) ;
#47308 = CARTESIAN_POINT ( 'NONE',  ( -6.635789839245807897, 6.706452665400368218, 0.7998128361456341429 ) ) ;
#47309 = CARTESIAN_POINT ( 'NONE',  ( 4.611744806942754238, 8.532119374741881757, -0.7998128361456231517 ) ) ;
#47310 = CARTESIAN_POINT ( 'NONE',  ( 2.998438581075290710, 1.946722116546204306, 0.2428724957088539971 ) ) ;
#47311 = CARTESIAN_POINT ( 'NONE',  ( 6.094553744542824170, 7.069066442510145265, 1.199719254218462483 ) ) ;
#47312 = CARTESIAN_POINT ( 'NONE',  ( -4.118090981180881016, 7.482401814132296103, -0.6348448669579254133 ) ) ;
#47313 = CARTESIAN_POINT ( 'NONE',  ( 3.928111819657337911, 5.605883094398769195, 1.599625672291267398 ) ) ;
#47314 = CARTESIAN_POINT ( 'NONE',  ( -4.990809943606281607, 6.915973915664348937, -1.443375672974066548 ) ) ;
#47316 = CARTESIAN_POINT ( 'NONE',  ( -6.019457014787517046, 9.006155036351978893, 1.082531754730548412 ) ) ;
#47315 =( GEOMETRIC_REPRESENTATION_CONTEXT ( 3 ) GLOBAL_UNCERTAINTY_ASSIGNED_CONTEXT ( ( #16373 ) ) GLOBAL_UNIT_ASSIGNED_CONTEXT ( ( #147075, #100432, #84182 ) ) REPRESENTATION_CONTEXT ( 'NONE', 'WORKASPACE' ) );
#47317 = CARTESIAN_POINT ( 'NONE',  ( 2.461320219219771843, -1.760565900816572826, 1.181798851529712646 ) ) ;
#47318 = CARTESIAN_POINT ( 'NONE',  ( -5.971440312176176768, 5.931378217152456500, 0.000000000000000000 ) ) ;
#47319 = CARTESIAN_POINT ( 'NONE',  ( 4.381803836707322652, 1.409801062080328959, 1.638821348427916602 ) ) ;
#47320 = CARTESIAN_POINT ( 'NONE',  ( 2.823586671956069605, 1.020774559177588081, -1.532180179759069283 ) ) ;
#47321 = CARTESIAN_POINT ( 'NONE',  ( -4.774234299259712877, 6.798759937490593153, 1.242976086189879759 ) ) ;
#47322 = CARTESIAN_POINT ( 'NONE',  ( -0.6823417656250246877, 0.1135416670080893753, 1.181850606188755259 ) ) ;
#47323 = CARTESIAN_POINT ( 'NONE',  ( 5.384588317801639157, 1.532214865288351158, -0.8252546180599307224 ) ) ;
#47324 = CARTESIAN_POINT ( 'NONE',  ( 4.528060117284232966, 6.305822774963486310, 1.443375672974062551 ) ) ;
#47325 = PRESENTATION_STYLE_ASSIGNMENT (( #196749 ) ) ;
#47326 = CARTESIAN_POINT ( 'NONE',  ( 2.641676655999642076, -1.601130012699041982, -1.452526871000489495 ) ) ;
#47327 = CARTESIAN_POINT ( 'NONE',  ( 4.534529724472468715, 1.956261425488527106, -0.4871295050740409582 ) ) ;
#47328 = CARTESIAN_POINT ( 'NONE',  ( -8.961576348508652146, 10.51788916375733685, -1.082531754730543083 ) ) ;
#47329 = B_SPLINE_CURVE_WITH_KNOTS ( 'NONE', 3,
 ( #82791, #99059, #133721, #19912, #151012, #32983, #15644, #16706, #181357, #2581 ),
 .UNSPECIFIED., .F., .F.,
 ( 4, 3, 3, 4 ),
 ( 0.000000000000000000, 8.893179197954989991E-05, 0.0001334007970840231242, 0.0001778705873658994649 ),
 .UNSPECIFIED. ) ;
#47330 = CARTESIAN_POINT ( 'NONE',  ( 2.448304249002517974, 2.161202317112873139, 0.05382173394478938222 ) ) ;
#47331 = CARTESIAN_POINT ( 'NONE',  ( 3.093000238167437743, 1.692540756771460764, -1.010471881233595104 ) ) ;
#47332 = FACE_OUTER_BOUND ( 'NONE', #191007, .T. ) ;
#47333 = CARTESIAN_POINT ( 'NONE',  ( 4.933121067701986995, -1.376026015944699088, -1.370709014919595958 ) ) ;
#47336 = ORIENTED_EDGE ( 'NONE', *, *, #176754, .F. ) ;
#47335 = CARTESIAN_POINT ( 'NONE',  ( 1.579999999999989413, 8.674529973577531194, -2.419999999999988827 ) ) ;
#47334 = CARTESIAN_POINT ( 'NONE',  ( -9.286972035236630063, 10.89751746493999107, -1.082531754730537976 ) ) ;
#47337 = STYLED_ITEM ( 'NONE', ( #173823 ), #143583 ) ;
#47338 = CARTESIAN_POINT ( 'NONE',  ( -5.772739544368596043, 9.956889578397179363, -0.7998128361456362523 ) ) ;
#47339 = DIRECTION ( 'NONE',  ( 0.000000000000000000, -3.252606517456504467E-14, -1.000000000000000000 ) ) ;
#47341 = ORIENTED_EDGE ( 'NONE', *, *, #98243, .F. ) ;
#47340 = CARTESIAN_POINT ( 'NONE',  ( -4.793689830883590020, 7.750332681742931662, 1.199719254218452935 ) ) ;
#47342 = CARTESIAN_POINT ( 'NONE',  ( -9.300530188850304469, 9.952966096521256745, 1.040834085586084257E-14 ) ) ;
#47343 = CARTESIAN_POINT ( 'NONE',  ( 1.606762454812577179, -0.7948807482080816333, -2.058825234118460745 ) ) ;
#47344 = CARTESIAN_POINT ( 'NONE',  ( -1.642778471874998480, -2.151041666188707957, 2.845375778867863303 ) ) ;
#47345 = CARTESIAN_POINT ( 'NONE',  ( 4.909014596843685574, -1.577992517845404619, 1.165349624694256958 ) ) ;
#47346 = CARTESIAN_POINT ( 'NONE',  ( -1.001543065824772872E-14, 4.884375000341420581, 1.575800808251672791 ) ) ;
#47347 = CARTESIAN_POINT ( 'NONE',  ( 1.499999999999989120, 3.035416667349485564, 0.8660254037844524744 ) ) ;
#47348 = CARTESIAN_POINT ( 'NONE',  ( 5.563869425686542414, 6.377698570463163463, -1.204193420357344557 ) ) ;
#47349 = FACE_OUTER_BOUND ( 'NONE', #133779, .T. ) ;
#47350 = CARTESIAN_POINT ( 'NONE',  ( 4.171694865975253741, -1.058263924308279424, 1.506412014522513720 ) ) ;
#47351 = EDGE_LOOP ( 'NONE', ( #144330, #36799, #78048, #192926 ) ) ;
#47352 = CARTESIAN_POINT ( 'NONE',  ( 1.360316468749969587, -0.7343749996585879902, -3.642919299551294898E-14 ) ) ;
#47353 = CARTESIAN_POINT ( 'NONE',  ( -7.802881099864745984, 9.062115023719057305, -1.199719254218446718 ) ) ;
#47354 = CARTESIAN_POINT ( 'NONE',  ( 7.055228938194279209, -8.176568542494891290, -6.396834479292358822 ) ) ;
#47355 = CARTESIAN_POINT ( 'NONE',  ( 5.291314375706784645, -0.05428322906628547939, -2.120082430678168706 ) ) ;
#47356 = CARTESIAN_POINT ( 'NONE',  ( 11.49097317489974834, 7.329182238404295724, -3.312691226010819889 ) ) ;
#47357 = CARTESIAN_POINT ( 'NONE',  ( 5.555090253297246150, 7.504024600312024340, 1.599625672291267398 ) ) ;
#47358 = EDGE_CURVE ( 'NONE', #120674, #128658, #1559, .T. ) ;
#47359 = CARTESIAN_POINT ( 'NONE',  ( 6.380161626619829107, -1.106262522808113324, 1.738493956250926287 ) ) ;
#47362 = CARTESIAN_POINT ( 'NONE',  ( 4.124425300631988200, 0.09459923933386081563, 1.838956108544815171 ) ) ;
#47361 = CARTESIAN_POINT ( 'NONE',  ( 1.592022279046673816, 0.9211323807055901147, -1.617040898905151458 ) ) ;
#47360 = DIRECTION ( 'NONE',  ( -1.000000000000000000, 0.000000000000000000, 0.000000000000000000 ) ) ;
#47363 = CARTESIAN_POINT ( 'NONE',  ( 8.121497709785879593, 9.433834401960398353, -1.199719254218445830 ) ) ;
#47364 = CARTESIAN_POINT ( 'NONE',  ( 8.855744143575730476, 3.691791674785632082, 7.453352967675146878 ) ) ;
#47365 =( BOUNDED_CURVE ( )  B_SPLINE_CURVE ( 3, ( #115583, #181577, #182645, #199957 ),
 .UNSPECIFIED., .F., .T. ) 
 B_SPLINE_CURVE_WITH_KNOTS ( ( 4, 4 ),
 ( 0.4999999999999948930, 1.000000000000000000 ),
 .UNSPECIFIED. ) 
 CURVE ( )  GEOMETRIC_REPRESENTATION_ITEM ( )  RATIONAL_B_SPLINE_CURVE ( ( 1.000000000000007327, 0.3333333333333334814, 0.3333333333333266535, 1.000000000000000444 ) ) 
 REPRESENTATION_ITEM ( '' )  );
#47366 = CARTESIAN_POINT ( 'NONE',  ( -7.767895665986912057, 8.027242796598338614, -0.7998128361456362523 ) ) ;
#47367 = LINE ( 'NONE', #32159, #129512 ) ;
#47368 = CARTESIAN_POINT ( 'NONE',  ( 3.862124860921032354, 2.190326239153097543, -0.2693113811002012525 ) ) ;
#47369 = CARTESIAN_POINT ( 'NONE',  ( 6.134080777514242300, 1.123080384508338136, -1.963935940973794869 ) ) ;
#47370 = CARTESIAN_POINT ( 'NONE',  ( -7.239690840017442675, 7.548653522882887934, 0.7216878364870317197 ) ) ;
#47371 = CARTESIAN_POINT ( 'NONE',  ( 5.765820309002536170, 0.5175119463115984697, -1.736122601384345820 ) ) ;
#47372 = CARTESIAN_POINT ( 'NONE',  ( 4.786306776965392196, -0.6515362397919061133, -1.801638605214391342 ) ) ;
#47373 = EDGE_CURVE ( 'NONE', #146105, #210172, #163036, .T. ) ;
#47374 = CARTESIAN_POINT ( 'NONE',  ( -1.364683531249997417, 5.571875000341417916, 1.214306433183764966E-14 ) ) ;
#47375 = CARTESIAN_POINT ( 'NONE',  ( 6.614126560844452385, -0.8839695271746010885, -1.648598838400926692 ) ) ;
#47376 = EDGE_CURVE ( 'NONE', #104947, #158693, #184563, .T. ) ;
#47377 = CARTESIAN_POINT ( 'NONE',  ( 5.810971417242416948, -1.466730511752023958, 1.145431029696217573 ) ) ;
#47378 = CARTESIAN_POINT ( 'NONE',  ( 4.764381983412778688E-15, 12.93749999999999645, -1.499999999999998446 ) ) ;
#47379 = CARTESIAN_POINT ( 'NONE',  ( 6.772329494929559601, -1.084452473627237845, 1.399072979944876449 ) ) ;
#47380 = CARTESIAN_POINT ( 'NONE',  ( 1.727750297885573882, 0.7672897036171549834, -1.865047645237365215 ) ) ;
#47382 = CARTESIAN_POINT ( 'NONE',  ( 2.490967578435684615, -0.3607690000238995554, -2.074772605841824991 ) ) ;
#47381 = CARTESIAN_POINT ( 'NONE',  ( -8.154339323615371171, 11.60081407993821045, 1.199719254218453823 ) ) ;
#47383 = CARTESIAN_POINT ( 'NONE',  ( 7.411503528164766763, 11.79850454950093841, 1.040834085586084257E-14 ) ) ;
#47385 = CARTESIAN_POINT ( 'NONE',  ( -9.667127221743832877, 11.23706883257798772, 1.199719254218462483 ) ) ;
#47384 = DIRECTION ( 'NONE',  ( 0.000000000000000000, 0.000000000000000000, 1.000000000000000000 ) ) ;
#47386 = CARTESIAN_POINT ( 'NONE',  ( -10.10176665042269839, 1.000000000000000888, -6.279211784079198999 ) ) ;
#47387 = CARTESIAN_POINT ( 'NONE',  ( 2.830336888193147882, -0.9990820879247277464, -1.755331475833141308 ) ) ;
#47388 = CARTESIAN_POINT ( 'NONE',  ( -1.364683531249997417, 3.009375000341422801, 1.214306433183764966E-14 ) ) ;
#47389 = CARTESIAN_POINT ( 'NONE',  ( 2.523789150438203510, 6.096171108819874007, 0.7998128361456462443 ) ) ;
#47390 = CARTESIAN_POINT ( 'NONE',  ( 3.409602121571019051, -0.4253414365745535886, 2.119164713334599881 ) ) ;
#47391 = CARTESIAN_POINT ( 'NONE',  ( 6.851666526859736983, 9.086973262793417661, -1.599625672291269396 ) ) ;
#47393 = DIRECTION ( 'NONE',  ( 0.6507913734559640506, -0.7592566023653003482, 0.000000000000000000 ) ) ;
#47392 = CARTESIAN_POINT ( 'NONE',  ( 7.354371980770088690, 7.544798497178720531, 0.000000000000000000 ) ) ;
#47394 = CARTESIAN_POINT ( 'NONE',  ( 10.18181017373857600, 10.98112607889092907, 0.7216878364870438212 ) ) ;
#47396 = DIRECTION ( 'NONE',  ( 1.000000000000000000, -0.000000000000000000, -0.000000000000000000 ) ) ;
#47395 = CARTESIAN_POINT ( 'NONE',  ( 0.6960477194701603088, -1.535568182542995208, -1.535184517522319769 ) ) ;
#47397 = CARTESIAN_POINT ( 'NONE',  ( -5.585596099150182958, 8.499983968108443477, -1.082531754730544860 ) ) ;
#47398 = AXIS2_PLACEMENT_3D ( 'NONE', #116048, #169001, #182036 ) ;
#47399 = CARTESIAN_POINT ( 'NONE',  ( -1.364683531250012516, 0.5302083336747518416, 0.7879004041258379498 ) ) ;
#47400 = CARTESIAN_POINT ( 'NONE',  ( 2.613028500285840661, -0.2118117899099076218, 2.181281865515646068 ) ) ;
#47401 = CARTESIAN_POINT ( 'NONE',  ( -0.006800380015323652903, 7.009756401597622144, 1.999988438675414759 ) ) ;
#47402 = CARTESIAN_POINT ( 'NONE',  ( 2.993345543732395697, 1.941157005910049138, -1.162047774482692697 ) ) ;
#47403 = CARTESIAN_POINT ( 'NONE',  ( -8.019811557683421910, 9.315200557840817908, 1.199719254218462483 ) ) ;
#47404 = CARTESIAN_POINT ( 'NONE',  ( -3.077337680177623103, 6.534051693608437184, 0.7216878364870317197 ) ) ;
#47405 = CARTESIAN_POINT ( 'NONE',  ( 1.364683531249988535, 2.926041667008082658, 0.7879004041258500513 ) ) ;
#47406 = CARTESIAN_POINT ( 'NONE',  ( 5.054560120293923653, 7.862967615930308796, 1.113740650586869219 ) ) ;
#47407 = CARTESIAN_POINT ( 'NONE',  ( -1.500000000000015099, 11.22916666666666963, -0.8660254037844309360 ) ) ;
#47408 = CARTESIAN_POINT ( 'NONE',  ( 7.051649292883499953, 7.399548061218447437, -0.7216878364870317197 ) ) ;
#47409 = CARTESIAN_POINT ( 'NONE',  ( 2.864225066854100277, -1.223476834174407779, 1.278924851658661099 ) ) ;
#47410 = CARTESIAN_POINT ( 'NONE',  ( 7.750457368506414646, 12.19395069656619945, 0.7998128361456462443 ) ) ;
#47411 = CARTESIAN_POINT ( 'NONE',  ( 5.895608061265788180, 1.667329832391790667, 1.445732890734657161 ) ) ;
#47412 = CARTESIAN_POINT ( 'NONE',  ( -1.364683531250010295, 8.880208333674731946, 0.7879004041258445001 ) ) ;
#47413 = CARTESIAN_POINT ( 'NONE',  ( -4.111865726694519552, 8.019203457777400956, 0.000000000000000000 ) ) ;
#47414 = CARTESIAN_POINT ( 'NONE',  ( 5.343375128634678006, 0.3905785925618041610, -1.978055652833633271 ) ) ;
#47415 = ORIENTED_EDGE ( 'NONE', *, *, #93584, .F. ) ;
#47416 = CARTESIAN_POINT ( 'NONE',  ( 3.889402362484274622, 1.354500474538382626, 1.290456140434749654 ) ) ;
#47417 = CARTESIAN_POINT ( 'NONE',  ( 2.975506508543226847, -0.2074491501150333705, 2.059866449969804503 ) ) ;
#47418 = CARTESIAN_POINT ( 'NONE',  ( -6.685579144870156476, 9.853573864773576219, 1.082531754730549967 ) ) ;
#47419 = DIRECTION ( 'NONE',  ( -1.276756478318932585E-15, 1.000000000000000000, -1.665334536937738262E-16 ) ) ;
#47420 = AXIS2_PLACEMENT_3D ( 'NONE', #214002, #96057, #46234 ) ;
#47421 = CARTESIAN_POINT ( 'NONE',  ( -2.926243505372967280E-18, -4.140708350189166609, -0.9999999999999991118 ) ) ;
#47422 = CARTESIAN_POINT ( 'NONE',  ( -4.175548912258498113, 7.500701962048164972, 0.7682608395963886894 ) ) ;
#47423 = CARTESIAN_POINT ( 'NONE',  ( 1.364683531249990311, 3.696875000341416584, 1.214306433183764966E-14 ) ) ;
#47424 = CARTESIAN_POINT ( 'NONE',  ( 1.265713261412576562, 0.5522810963098608861, -1.830935845731461953 ) ) ;
#47425 = CARTESIAN_POINT ( 'NONE',  ( 3.226955236329264398, -1.811681696138227160, -0.7532884077038404236 ) ) ;
#47426 = CARTESIAN_POINT ( 'NONE',  ( 1.335314297916901927, -1.281167425915705316, 1.556668322744148014 ) ) ;
#47427 = ADVANCED_FACE ( 'NONE', ( #51418 ), #50346, .F. ) ;
#47428 = CARTESIAN_POINT ( 'NONE',  ( -4.014095998097799267, 6.840806543492835345, -1.199719254218450271 ) ) ;
#47430 =( LENGTH_UNIT ( ) NAMED_UNIT ( * ) SI_UNIT ( .MILLI., .METRE. ) );
#47429 = CARTESIAN_POINT ( 'NONE',  ( 7.476431642932036326, 10.80992178580769014, 1.199719254218460707 ) ) ;
#47431 = CARTESIAN_POINT ( 'NONE',  ( 6.397732417105159719, -0.6663202349154914161, 1.855440513692607540 ) ) ;
#47432 = CARTESIAN_POINT ( 'NONE',  ( 1.364683531249990311, 3.134375000341423245, 1.214306433183764966E-14 ) ) ;
#47433 = CARTESIAN_POINT ( 'NONE',  ( 2.373293634344127767, -1.753592693251155632, -0.9887173157705446691 ) ) ;
#47435 = CARTESIAN_POINT ( 'NONE',  ( 2.144302737913783119, 0.9084621246772636161, 1.912570996397492618 ) ) ;
#47434 = CARTESIAN_POINT ( 'NONE',  ( -6.073689629242151611, 10.02979563418376685, -0.7216878364870278340 ) ) ;
#47436 = DIRECTION ( 'NONE',  ( 5.551115123125765446E-17, 0.000000000000000000, -1.000000000000000000 ) ) ;
#47437 = CARTESIAN_POINT ( 'NONE',  ( 3.367693471486675083, -0.4065805204805824635, 2.029877954327436118 ) ) ;
#47438 = CARTESIAN_POINT ( 'NONE',  ( 3.576318658954677598, 7.394398545414291313, 0.7998128361456281477 ) ) ;
#47440 = CARTESIAN_POINT ( 'NONE',  ( 2.679707916995359263, 6.278076336469897711, -0.7998128361456291469 ) ) ;
#47439 = CARTESIAN_POINT ( 'NONE',  ( 5.648407305961395508, -1.648567506571393615, 1.285558710341473621 ) ) ;
#47442 = ORIENTED_EDGE ( 'NONE', *, *, #53608, .F. ) ;
#47441 = CARTESIAN_POINT ( 'NONE',  ( 4.629811725094972630, -1.123643258228578024, -1.438734611599351565 ) ) ;
#47443 = CARTESIAN_POINT ( 'NONE',  ( 9.459838494033030898, 12.05956421450382088, 1.599625672291281386 ) ) ;
#47444 = CARTESIAN_POINT ( 'NONE',  ( 10.48924606301532592, 11.88481095883722283, -6.433727461572112283 ) ) ;
#47445 = CARTESIAN_POINT ( 'NONE',  ( 6.598651186688741177, -0.5821561243712966016, -2.128545807824663960 ) ) ;
#47446 = CARTESIAN_POINT ( 'NONE',  ( -1.364683531250000748, 10.17187500034139802, 0.000000000000000000 ) ) ;
#47447 = EDGE_LOOP ( 'NONE', ( #103654, #66947, #27231, #5380, #54859 ) ) ;
#47448 = CARTESIAN_POINT ( 'NONE',  ( 5.531871257421491883, -1.864710570029969317, 0.4231498525801706823 ) ) ;
#47450 = CARTESIAN_POINT ( 'NONE',  ( -2.137381772448751605, 5.645362501165475777, -0.7998128361456281477 ) ) ;
#47449 = MECHANICAL_DESIGN_GEOMETRIC_PRESENTATION_REPRESENTATION (  '', ( #71682 ), #89047 ) ;
#47451 = CARTESIAN_POINT ( 'NONE',  ( 6.988338112840064120, 10.24047933403371502, 1.199719254218460707 ) ) ;
#47452 = CARTESIAN_POINT ( 'NONE',  ( -0.6801582343750282034, 1.963541667008045222, 1.178068619123803451 ) ) ;
#47453 = CARTESIAN_POINT ( 'NONE',  ( 3.131570294632282092, 5.636953862837537521, -1.082531754730543971 ) ) ;
#47454 = CYLINDRICAL_SURFACE ( 'NONE', #117065, 0.3999999999999997446 ) ;
#47455 = CARTESIAN_POINT ( 'NONE',  ( -6.328953403633620134, 6.883256856249502675, 0.7255120703185078401 ) ) ;
#47456 = CARTESIAN_POINT ( 'NONE',  ( 0.3097736896383457839, 1.270387085892955792, -1.333027339516623888 ) ) ;
#47457 = ORIENTED_EDGE ( 'NONE', *, *, #39783, .T. ) ;
#47458 = AXIS2_PLACEMENT_3D ( 'NONE', #212185, #48654, #134191 ) ;
#47459 = CARTESIAN_POINT ( 'NONE',  ( -7.747558435566414659, 8.003516027774422170, -0.7998128361456362523 ) ) ;
#47460 = CARTESIAN_POINT ( 'NONE',  ( 5.132044594934622062, 0.9627672477196843603, -1.603626212978970900 ) ) ;
#47461 = CARTESIAN_POINT ( 'NONE',  ( -0.02299388927988129522, 0.2517100516001030686, -1.946460665317284011 ) ) ;
#47462 = CARTESIAN_POINT ( 'NONE',  ( 7.693325821111733021, 7.940244644243982464, -0.7998128361456341429 ) ) ;
#47463 = CARTESIAN_POINT ( 'NONE',  ( -1.420000000000021911, 6.200000000000045475, 2.900000000000013678 ) ) ;
#47464 = CARTESIAN_POINT ( 'NONE',  ( -5.200254360346833415, 7.740598053885397789, 1.191768289972208628 ) ) ;
#47465 = CARTESIAN_POINT ( 'NONE',  ( -6.412643469583822586, 6.583764924043652655, 1.040834085586084257E-14 ) ) ;
#47466 = CARTESIAN_POINT ( 'NONE',  ( 4.039439701867726384, 6.800097854565950506, 1.199719254218462483 ) ) ;
#47467 = CARTESIAN_POINT ( 'NONE',  ( 1.393335261261628988, -1.782783755681414117, 0.8371470673369950655 ) ) ;
#47468 = CARTESIAN_POINT ( 'NONE',  ( 2.741814726283864800, 2.006445297011373974, -0.2004551355171620974 ) ) ;
#47469 = CARTESIAN_POINT ( 'NONE',  ( -9.508345801885592863, 9.987491611821676329, 0.7998128361456462443 ) ) ;
#47470 = CARTESIAN_POINT ( 'NONE',  ( 4.529305835417093640, 7.441884687032027657, -1.199719254218450271 ) ) ;
#47472 = EDGE_CURVE ( 'NONE', #206426, #63064, #107738, .T. ) ;
#47471 = DIRECTION ( 'NONE',  ( 0.000000000000000000, 0.000000000000000000, -1.000000000000000000 ) ) ;
#47473 = VECTOR ( 'NONE', #179905, 1000.000000000000000 ) ;
#47474 = CARTESIAN_POINT ( 'NONE',  ( 2.976726284633357533, -0.1618151936485581754, -2.185533650236513914 ) ) ;
#47475 = CARTESIAN_POINT ( 'NONE',  ( 2.993041990875914493, 6.420974562437304911, 0.3677586026352899218 ) ) ;
#47476 = CARTESIAN_POINT ( 'NONE',  ( -8.839026081105473054, 12.39961529701003684, -1.199719254218446718 ) ) ;
#47477 = CARTESIAN_POINT ( 'NONE',  ( 6.825078400183584471, 2.055285645424239416, 2.261848697290469445 ) ) ;
#47478 = CARTESIAN_POINT ( 'NONE',  ( 8.326672684688675286E-17, 6.999999999999999112, -1.500000000000005107 ) ) ;
#47479 = EDGE_CURVE ( 'NONE', #111140, #113025, #194086, .T. ) ;
#47480 = CARTESIAN_POINT ( 'NONE',  ( -10.37923916842784422, 4.890109552615133026, -5.358306740738790097 ) ) ;
#47481 = CARTESIAN_POINT ( 'NONE',  ( 9.206149998879153529, 10.69926207256923689, 1.199719254218453823 ) ) ;
#47482 = CARTESIAN_POINT ( 'NONE',  ( 5.636439174979242850, 7.598931675607687453, -1.599625672291262513 ) ) ;
#47483 = CARTESIAN_POINT ( 'NONE',  ( -4.596923820214036560, 8.483565078729160547, 0.2266403168418751335 ) ) ;
#47484 = CARTESIAN_POINT ( 'NONE',  ( 5.722950238744198614, 8.730506807626655430, 1.082531754730549967 ) ) ;
#47485 = ORIENTED_EDGE ( 'NONE', *, *, #79889, .F. ) ;
#47487 = CARTESIAN_POINT ( 'NONE',  ( 1.629542719884415680, -0.2443838731654828789, 1.998128341252780604 ) ) ;
#47486 = CARTESIAN_POINT ( 'NONE',  ( 5.038538826285253514, -1.576363729006284187, 0.9512496309353533075 ) ) ;
#47488 = CARTESIAN_POINT ( 'NONE',  ( 2.777091360721035240, -2.273647235919952880, 0.3355521655935486125 ) ) ;
#47490 = CARTESIAN_POINT ( 'NONE',  ( 2.307254945994464457, -1.491077236629720248, -1.113220461199310618 ) ) ;
#47489 = CARTESIAN_POINT ( 'NONE',  ( -0.1290005225502675879, 2.860092606084875033, -2.662085506130333457 ) ) ;
#47491 = CARTESIAN_POINT ( 'NONE',  ( 0.000000000000000000, -2.996874999522043392, -3.793834371823813001 ) ) ;
#47492 = PLANE ( 'NONE',  #160813 ) ;
#47493 = CARTESIAN_POINT ( 'NONE',  ( 5.818603510220927255, -0.6945032022064903110, -1.782003016414166474 ) ) ;
#47494 = CARTESIAN_POINT ( 'NONE',  ( -9.671043645249580933, 10.17730576241299900, 0.7998128361456462443 ) ) ;
#47495 = CARTESIAN_POINT ( 'NONE',  ( -6.631346530859867805, 6.909194838857525944, 0.000000000000000000 ) ) ;
#47497 = CARTESIAN_POINT ( 'NONE',  ( 3.414787578387419309, 1.690673485743508619, 0.8009127983473337542 ) ) ;
#47496 = CARTESIAN_POINT ( 'NONE',  ( 4.739831270385728601, 2.085251124590303373, 0.1521322122139453781 ) ) ;
#47498 = CARTESIAN_POINT ( 'NONE',  ( 6.426201623197458801, 9.480690412830290015, -1.082531754730537088 ) ) ;
#47499 = CARTESIAN_POINT ( 'NONE',  ( 6.409700764581637067, -0.8744420883355051854, -1.620376909479949390 ) ) ;
#47500 = CARTESIAN_POINT ( 'NONE',  ( 2.686486993802192913, 6.285985259411197568, 0.7998128361456362523 ) ) ;
#47502 = CARTESIAN_POINT ( 'NONE',  ( 5.840865249388943248, 5.708764300575555062, 0.7998128361456341429 ) ) ;
#47501 = DIRECTION ( 'NONE',  ( 0.8656921114426504582, -0.5005768354468328463, -3.032296636007458012E-15 ) ) ;
#47503 = CARTESIAN_POINT ( 'NONE',  ( 5.531808922564334097, -1.099089406413750414, -1.329375763670269883 ) ) ;
#47504 = CARTESIAN_POINT ( 'NONE',  ( -7.386494761346872551, 7.511998731193139989, -0.7998128361456291469 ) ) ;
#47505 = CARTESIAN_POINT ( 'NONE',  ( 0.4395775532227184090, -1.463650450414313520, -0.9296597220836488873 ) ) ;
#47506 = DIRECTION ( 'NONE',  ( -5.551115123125782702E-17, 0.000000000000000000, 1.000000000000000000 ) ) ;
#47507 = CARTESIAN_POINT ( 'NONE',  ( 4.311506836774354312, -1.801752502381037457, -1.211023186257336404 ) ) ;
#47508 = CARTESIAN_POINT ( 'NONE',  ( 3.861776535121093090, 1.811678901967550326, -0.2252020330209548171 ) ) ;
#47509 = CARTESIAN_POINT ( 'NONE',  ( 1.463640819124707004, -0.4818986642843925972, 1.901505326443528876 ) ) ;
#47510 = CARTESIAN_POINT ( 'NONE',  ( 5.911343334927605220, -1.992878553188395463, 0.7155076844978009998 ) ) ;
#47512 = CARTESIAN_POINT ( 'NONE',  ( -1.364683531249997417, 3.821875000341416584, 1.214306433183764966E-14 ) ) ;
#47511 = CARTESIAN_POINT ( 'NONE',  ( 5.372717881723642286, -0.05365108595901035143, -2.291914610307096201 ) ) ;
#47513 = CARTESIAN_POINT ( 'NONE',  ( 2.060660350337685465, 8.500464906089362671, 2.499999999999998668 ) ) ;
#47514 = CARTESIAN_POINT ( 'NONE',  ( 8.565000355531088516, 11.01558638625153286, -1.599625672291257406 ) ) ;
#47515 = CARTESIAN_POINT ( 'NONE',  ( 2.086737175084628859, -1.302296122868449535, 1.673399772156684895 ) ) ;
#47516 = CARTESIAN_POINT ( 'NONE',  ( -4.663641653420935285, 5.503632019488245319, 1.082531754730560403 ) ) ;
#47517 = CARTESIAN_POINT ( 'NONE',  ( 5.602074566136501232, 5.729665287594564838, 0.6253354971682704155 ) ) ;
#47518 = CARTESIAN_POINT ( 'NONE',  ( -3.755245360860925086, 6.364574773437617239, -1.082531754730548412 ) ) ;
#47519 = CARTESIAN_POINT ( 'NONE',  ( 6.578989008465588206, 2.022637127319019790, 0.7894149679951308896 ) ) ;
#47521 = CARTESIAN_POINT ( 'NONE',  ( -6.009258394948636914E-15, 14.46875000068279249, -1.732050807568875195 ) ) ;
#47520 = CARTESIAN_POINT ( 'NONE',  ( 6.983263157960366563, 3.694515354052980260, 2.467960814016751936 ) ) ;
#47523 = ORIENTED_EDGE ( 'NONE', *, *, #131672, .F. ) ;
#47522 = CARTESIAN_POINT ( 'NONE',  ( 2.860263265526213683, 0.7972832613293324711, -2.073463298260522780 ) ) ;
#47524 = CARTESIAN_POINT ( 'NONE',  ( 0.1242335807666505171, 0.4018034787525020524, 2.263199520926823638 ) ) ;
#47526 = CARTESIAN_POINT ( 'NONE',  ( 5.577030875653865571, 1.903616248300431746, 0.7944661687919268855 ) ) ;
#47525 = CARTESIAN_POINT ( 'NONE',  ( 2.347533153460546806, 5.890539112345938300, 0.000000000000000000 ) ) ;
#47528 = CARTESIAN_POINT ( 'NONE',  ( -3.474999999999998312, -1.370833333333331350, 2.006292185433951047 ) ) ;
#47527 = CARTESIAN_POINT ( 'NONE',  ( 4.016958651398847557, 7.908478536599129249, -0.7998128361456362523 ) ) ;
#47529 = CARTESIAN_POINT ( 'NONE',  ( 4.227110032410640095, 8.153655147779589996, 0.7998128361456271485 ) ) ;
#47530 = CARTESIAN_POINT ( 'NONE',  ( 1.642778471875000035, -0.2260416661887081069, -2.845375778867859751 ) ) ;
#47531 = CARTESIAN_POINT ( 'NONE',  ( 0.2331563151865486683, 0.2490001740663889407, -1.980811336351681273 ) ) ;
#47532 = CARTESIAN_POINT ( 'NONE',  ( 5.003375819710620398, -1.831856422778654681, 0.1858995714831001289 ) ) ;
#47534 = VERTEX_POINT ( 'NONE', #122912 ) ;
#47533 = CARTESIAN_POINT ( 'NONE',  ( 4.976006071415387311, 5.764094157194782575, 1.199719254218462483 ) ) ;
#47535 = CARTESIAN_POINT ( 'NONE',  ( 1.570901180570225542, 0.1317378181442031559, -1.719804994506502149 ) ) ;
#47536 = CARTESIAN_POINT ( 'NONE',  ( 1.516814941429758701, 0.2024661778830244008, 2.006371303556075958 ) ) ;
#47537 =( BOUNDED_SURFACE ( )  B_SPLINE_SURFACE ( 3, 3, ( 
 ( #81072, #146102, #93081, #63750, #26976, #10724, #159123, #126707, #95213, #195894 ),
 ( #208915, #128833, #113644, #31269, #145046, #96281, #147158, #161262, #76794, #142915 ),
 ( #192669, #160191, #44322, #211048, #97344, #194815, #163401, #64813, #62674, #213183 ),
 ( #127790, #47531, #45391, #14976, #162331, #130959, #46451, #94151, #112573, #13916 ),
 ( #79997, #209979, #110444, #176446, #12849, #212113, #28058, #196949, #111507, #109384 ),
 ( #177513, #11791, #143988, #61621, #164456, #66915, #4056, #48589, #17111, #85337 ),
 ( #133056, #83188, #148220, #136239, #152476, #16043, #184949, #50703, #201195, #118971 ) ),
 .UNSPECIFIED., .T., .F., .T. ) 
 B_SPLINE_SURFACE_WITH_KNOTS ( ( 4, 3, 4 ),
 ( 4, 1, 1, 1, 1, 1, 1, 4 ),
 ( 0.000000000000000000, 0.5000000000000000000, 1.000000000000000000 ),
 ( 0.000000000000000000, 0.09599525230796020214, 0.1893027314675523320, 0.2592390727089966540, 0.3619855251144610819, 0.5211967264240887632, 0.7336899926499302893, 1.000000000000000000 ),
 .UNSPECIFIED. ) 
 GEOMETRIC_REPRESENTATION_ITEM ( )  RATIONAL_B_SPLINE_SURFACE ( (
 ( 1.000000000000000222, 1.000000000000000222, 0.9999999999999997780, 1.000000000000000444, 1.000000000000000222, 1.000000000000000222, 1.000000000000000222, 1.000000000000000222, 1.000000000000000222, 1.000000000000000222),
 ( 0.3333333333333334259, 0.3333333333333334259, 0.3333333333333333148, 0.3333333333333335369, 0.3333333333333334259, 0.3333333333333333703, 0.3333333333333334259, 0.3333333333333333703, 0.3333333333333334259, 0.3333333333333334259),
 ( 0.3333333333333334259, 0.3333333333333334259, 0.3333333333333333148, 0.3333333333333335369, 0.3333333333333334259, 0.3333333333333333703, 0.3333333333333334259, 0.3333333333333333703, 0.3333333333333334259, 0.3333333333333334259),
 ( 1.000000000000000222, 1.000000000000000222, 0.9999999999999997780, 1.000000000000000444, 1.000000000000000222, 1.000000000000000222, 1.000000000000000222, 1.000000000000000222, 1.000000000000000222, 1.000000000000000222),
 ( 0.3333333333333334259, 0.3333333333333334259, 0.3333333333333333148, 0.3333333333333335369, 0.3333333333333334259, 0.3333333333333333703, 0.3333333333333334259, 0.3333333333333333703, 0.3333333333333334259, 0.3333333333333334259),
 ( 0.3333333333333334259, 0.3333333333333334259, 0.3333333333333333148, 0.3333333333333335369, 0.3333333333333334259, 0.3333333333333333703, 0.3333333333333334259, 0.3333333333333333703, 0.3333333333333334259, 0.3333333333333334259),
 ( 1.000000000000000222, 1.000000000000000222, 0.9999999999999997780, 1.000000000000000444, 1.000000000000000222, 1.000000000000000222, 1.000000000000000222, 1.000000000000000222, 1.000000000000000222, 1.000000000000000222) ) ) 
 REPRESENTATION_ITEM ( '' )  SURFACE ( )  );
#47538 = CARTESIAN_POINT ( 'NONE',  ( 1.811588643561705680, 1.319210623403826110, -1.882327697243087350 ) ) ;
#47539 = CARTESIAN_POINT ( 'NONE',  ( -1.364683531250012516, 3.592708333674750509, 0.7879004041258379498 ) ) ;
#47540 = CARTESIAN_POINT ( 'NONE',  ( 2.618781011676008852, 1.479506999046651838, -1.711640912222348376 ) ) ;
#47541 = CARTESIAN_POINT ( 'NONE',  ( 4.160836958300685673, -1.560740793797481318, 1.414261741400888006 ) ) ;
#47542 = CARTESIAN_POINT ( 'NONE',  ( -6.116136693540540570, 10.14959355252370266, 0.000000000000000000 ) ) ;
#47543 = CARTESIAN_POINT ( 'NONE',  ( 2.161070758698178107, 0.3078950573750063313, -1.742579939182072657 ) ) ;
#47544 = CIRCLE ( 'NONE', #9329, 6.200000000000000178 ) ;
#47545 = CARTESIAN_POINT ( 'NONE',  ( 6.043183783389218355, 8.073467052085995022, 1.599625672291267398 ) ) ;
#47546 = CARTESIAN_POINT ( 'NONE',  ( 4.028181036591620412, 7.713645286083276709, -0.7216878364870338292 ) ) ;
#47547 = CARTESIAN_POINT ( 'NONE',  ( -3.425406365747000859, 7.148057860013469877, 1.040834085586084257E-14 ) ) ;
#47548 = UNCERTAINTY_MEASURE_WITH_UNIT (LENGTH_MEASURE( 1.000000000000000082E-05 ), #4115, 'distance_accuracy_value', 'NONE');
#47549 = CARTESIAN_POINT ( 'NONE',  ( 4.948362878863507675, 8.716914425408678113, -0.7216878364870267237 ) ) ;
#47550 = CARTESIAN_POINT ( 'NONE',  ( -1.499999999999997780, 2.650000000000020339, 1.214306433183764966E-14 ) ) ;
#47551 = CARTESIAN_POINT ( 'NONE',  ( 5.994412725124051100, -1.189069957525538124, 1.876188141934010956 ) ) ;
#47552 = CARTESIAN_POINT ( 'NONE',  ( 2.941561714372803671, 0.7881326131919093037, -2.044999658057600644 ) ) ;
#47553 = CARTESIAN_POINT ( 'NONE',  ( -4.894657149733403045, 5.669187081899118574, -1.199719254218446718 ) ) ;
#47554 = CARTESIAN_POINT ( 'NONE',  ( 0.4933182949324292355, 7.812106778932951023, -1.990607459109241972 ) ) ;
#47555 = CARTESIAN_POINT ( 'NONE',  ( 6.516280388114967792, -2.120036885061008292, 0.05137064186952475936 ) ) ;
#47556 = CARTESIAN_POINT ( 'NONE',  ( -1.364683531249997417, 3.759375000341423689, 1.214306433183764966E-14 ) ) ;
#47557 = EDGE_CURVE ( 'NONE', #186824, #171443, #181433, .T. ) ;
#47558 = CARTESIAN_POINT ( 'NONE',  ( -8.012344526598182026E-15, 9.296875000341398021, -1.575800808251669460 ) ) ;
#47559 = CARTESIAN_POINT ( 'NONE',  ( -4.663641653420935285, 5.503632019488245319, 1.082531754730560403 ) ) ;
#47560 = CARTESIAN_POINT ( 'NONE',  ( 6.064709079624690524, 0.6667526090060638122, 2.013086243192941716 ) ) ;
#47561 = CARTESIAN_POINT ( 'NONE',  ( -4.651856103264620401, 8.441266197201775512, 0.000000000000000000 ) ) ;
#47562 = ORIENTED_EDGE ( 'NONE', *, *, #105381, .T. ) ;
#47563 = CARTESIAN_POINT ( 'NONE',  ( -5.045042558060949034, 6.018876084893449274, 1.082531754730549078 ) ) ;
#47564 = CARTESIAN_POINT ( 'NONE',  ( 4.493637847925535667, 7.329995691633395261, -1.199719254218452047 ) ) ;
#47565 = CARTESIAN_POINT ( 'NONE',  ( 6.497600353373155002, -1.840680978339729545, 0.05264081064878384231 ) ) ;
#47566 = CARTESIAN_POINT ( 'NONE',  ( -4.168895032367330167, 3.976329666238523242, -0.6109567437776577403 ) ) ;
#47567 = CARTESIAN_POINT ( 'NONE',  ( 0.4856440469271376958, 6.671526543591629554, -3.376304580250021559 ) ) ;
#47568 = CARTESIAN_POINT ( 'NONE',  ( -1.364683531249997417, 4.071875000341417028, 1.214306433183764966E-14 ) ) ;
#47569 = CARTESIAN_POINT ( 'NONE',  ( 2.489492129562159484, -1.735903792773977772, -0.1261859363600649764 ) ) ;
#47570 = CARTESIAN_POINT ( 'NONE',  ( -4.357933079043927016, 8.048364350591832306, -0.3271847907353189200 ) ) ;
#47571 = CARTESIAN_POINT ( 'NONE',  ( -1.115562610750309283E-14, 10.84375000068279604, 1.500000000000001554 ) ) ;
#47572 = CARTESIAN_POINT ( 'NONE',  ( 0.6823417656249882723, -0.09479166632524876901, 1.181850606188755259 ) ) ;
#47573 = FACE_OUTER_BOUND ( 'NONE', #24940, .T. ) ;
#47574 = CARTESIAN_POINT ( 'NONE',  ( -8.109748439268576803, 12.61312361245537517, 0.7998128361456481317 ) ) ;
#47575 = CARTESIAN_POINT ( 'NONE',  ( -5.653386866774179786, 8.579073197003079798, 1.082531754730548412 ) ) ;
#47576 = AXIS2_PLACEMENT_3D ( 'NONE', #3987, #182755, #200066 ) ;
#47577 = CARTESIAN_POINT ( 'NONE',  ( 5.524359596833869013, 1.291058806671550485, -1.733668313432787933 ) ) ;
#47579 = ORIENTED_EDGE ( 'NONE', *, *, #67226, .T. ) ;
#47578 = DIRECTION ( 'NONE',  ( -1.000000000000000000, 5.578564026256504688E-16, 0.000000000000000000 ) ) ;
#47580 = CARTESIAN_POINT ( 'NONE',  ( -1.364683531250012516, 3.738541667008087099, -0.7879004041258300672 ) ) ;
#47581 = CARTESIAN_POINT ( 'NONE',  ( 6.098895391831223201, 1.613120528903468243, -1.132937624142603905 ) ) ;
#47582 = CARTESIAN_POINT ( 'NONE',  ( 5.132092517088904238, 0.1681052705169924777, -1.725677682095213994 ) ) ;
#47584 = CARTESIAN_POINT ( 'NONE',  ( 1.909981697816802049, -1.036543071415759298, -1.930953618257096993 ) ) ;
#47583 = CARTESIAN_POINT ( 'NONE',  ( -5.558564015327489343E-14, -0.4218749996585599571, -1.570758158831802254 ) ) ;
#47585 = CARTESIAN_POINT ( 'NONE',  ( 3.136059509142240742, -1.548504943098116593, -1.711042559064612334 ) ) ;
#47586 = CARTESIAN_POINT ( 'NONE',  ( 6.450472299244985663, 0.6421947732520795205, 1.958257120725328315 ) ) ;
#47587 = CARTESIAN_POINT ( 'NONE',  ( 0.9373250018651816395, 0.7876268737729983371, -1.775224631529322306 ) ) ;
#47588 = CARTESIAN_POINT ( 'NONE',  ( -5.626270559546828309, 7.587068290936515247, 1.443375672974064550 ) ) ;
#47589 = CARTESIAN_POINT ( 'NONE',  ( -5.652823702255029836, 5.559658838911111900, -0.7998128361456362523 ) ) ;
#47590 = CARTESIAN_POINT ( 'NONE',  ( -5.606283457547605487, 5.690634927916947916, -0.2483668091577979076 ) ) ;
#47591 = CARTESIAN_POINT ( 'NONE',  ( 3.674183785563363447, 2.104178206457421485, -0.2630699042918820396 ) ) ;
#47592 = CARTESIAN_POINT ( 'NONE',  ( 2.901017702322743919, -0.9963018188003970321, -1.753030416019534021 ) ) ;
#47593 = CARTESIAN_POINT ( 'NONE',  ( -5.056828107772848746, 8.843457192469559303, -0.7216878364870207285 ) ) ;
#47594 = ADVANCED_FACE ( 'NONE', ( #107698 ), #77701, .T. ) ;
#47595 = CARTESIAN_POINT ( 'NONE',  ( 5.069440727656137291, 0.2206807655098403653, -2.195719112144229879 ) ) ;
#47596 = CARTESIAN_POINT ( 'NONE',  ( -4.688236331909272359, 5.260680481867119340, 1.129709447323426152 ) ) ;
#47597 = DIRECTION ( 'NONE',  ( 1.276756478318932585E-15, -1.000000000000000000, 1.665334536937738262E-16 ) ) ;
#47598 = CARTESIAN_POINT ( 'NONE',  ( 0.06470675514189982991, -1.629034059718449834, -0.8243793580787887043 ) ) ;
#47599 = CARTESIAN_POINT ( 'NONE',  ( -7.611976899429754084, 7.845337568948314022, 0.7998128361456341429 ) ) ;
#47601 = DIRECTION ( 'NONE',  ( -0.009157509157509154465, 0.000000000000000000, -0.9999580691339163829 ) ) ;
#47600 = CARTESIAN_POINT ( 'NONE',  ( -5.823544721894389653, 7.314923355733134791, 1.295626528688619272 ) ) ;
#47602 = CARTESIAN_POINT ( 'NONE',  ( 0.03686668447251651576, 7.053483931691109099, 3.954540522192132812 ) ) ;
#47603 = EDGE_LOOP ( 'NONE', ( #201635, #170356, #8161, #79922 ) ) ;
#47604 = CARTESIAN_POINT ( 'NONE',  ( 4.329017481302106063, 0.09909362218092979124, 2.058626247020868494 ) ) ;
#47605 = CARTESIAN_POINT ( 'NONE',  ( -6.577113915960828727, 9.727031097712693253, -1.082531754730549967 ) ) ;
#47606 = CARTESIAN_POINT ( 'NONE',  ( 11.33772463945036790, 13.40000000000000036, -3.600000000000002309 ) ) ;
#47607 = CARTESIAN_POINT ( 'NONE',  ( -3.581325132304157943, 7.329963087663487364, -0.7998128361456281477 ) ) ;
#47608 = CARTESIAN_POINT ( 'NONE',  ( -5.991777542596674166, 5.955104985976372944, 0.000000000000000000 ) ) ;
#47609 = CARTESIAN_POINT ( 'NONE',  ( 3.914717006531149401, -0.6357662484684013515, -1.917053231858157236 ) ) ;
#47610 = CARTESIAN_POINT ( 'NONE',  ( -1.500000000000001332, 1.150000000000019007, 0.000000000000000000 ) ) ;
#47611 = CARTESIAN_POINT ( 'NONE',  ( 8.581948047770334043, 12.95609712246668899, 0.000000000000000000 ) ) ;
#47612 = CARTESIAN_POINT ( 'NONE',  ( 7.657657833620182153, 7.828355648845348291, -0.7998128361456281477 ) ) ;
#47613 = CARTESIAN_POINT ( 'NONE',  ( 2.993097573648812126, 1.768379194316849423, -1.058085006197813538 ) ) ;
#47614 = DIRECTION ( 'NONE',  ( 0.000000000000000000, 0.000000000000000000, 1.000000000000000000 ) ) ;
#47615 = CARTESIAN_POINT ( 'NONE',  ( 5.087333953625774008, 6.958308917361963886, 1.599625672291267398 ) ) ;
#47617 = CARTESIAN_POINT ( 'NONE',  ( 3.204314817619222211, 1.275555974797081049, -1.561881975048397209 ) ) ;
#47616 = COLOUR_RGB ( '', 0.09019608, 0.27058824, 0.51372549) ;
#47618 = CARTESIAN_POINT ( 'NONE',  ( -0.2411972340276022364, 0.7381021182278154624, -1.984382818515282532 ) ) ;
#47619 = CARTESIAN_POINT ( 'NONE',  ( 1.851249556194194179, 1.836288347861175785, -0.1344999175661651392 ) ) ;
#47620 = CARTESIAN_POINT ( 'NONE',  ( 0.04808971849027363077, -1.788275647358487985, -1.458162290246179715 ) ) ;
#47621 = CARTESIAN_POINT ( 'NONE',  ( 3.562760505341037831, 7.378580699531681830, -1.734723475976807094E-15 ) ) ;
#47622 = CARTESIAN_POINT ( 'NONE',  ( 2.864712396292764751, -1.492883925411473856, 1.563474562115530375 ) ) ;
#47623 = CARTESIAN_POINT ( 'NONE',  ( -5.111060722671894929, 5.065251719313053513, 0.000000000000000000 ) ) ;
#47624 = CARTESIAN_POINT ( 'NONE',  ( 1.762908039156896978, -0.1037823317905466058, -2.014007988105172231 ) ) ;
#47626 = EDGE_CURVE ( 'NONE', #92893, #126082, #135899, .T. ) ;
#47625 =( GEOMETRIC_REPRESENTATION_CONTEXT ( 3 ) GLOBAL_UNCERTAINTY_ASSIGNED_CONTEXT ( ( #174404 ) ) GLOBAL_UNIT_ASSIGNED_CONTEXT ( ( #188796, #206102, #56671 ) ) REPRESENTATION_CONTEXT ( 'NONE', 'WORKASPACE' ) );
#47627 = CARTESIAN_POINT ( 'NONE',  ( 2.654040013917441598, -0.3913916837698909745, -2.264681309554557043 ) ) ;
#47628 = CARTESIAN_POINT ( 'NONE',  ( -11.86686399458719343, 11.10928729775337054, -1.056461745586973811 ) ) ;
#47629 = CARTESIAN_POINT ( 'NONE',  ( -0.5158641071528082822, 6.759906959843508645, 3.511243559023642824 ) ) ;
#47630 = CARTESIAN_POINT ( 'NONE',  ( 4.118015666179648093, -1.012585719757435498, -1.691412322542594326 ) ) ;
#47631 = CARTESIAN_POINT ( 'NONE',  ( 4.716029918043215474, 1.032482702726954527, -1.731993998903176957 ) ) ;
#47633 = CARTESIAN_POINT ( 'NONE',  ( 10.01911233037458260, 10.79131192829960462, 0.7216878364870438212 ) ) ;
#47632 = CARTESIAN_POINT ( 'NONE',  ( 0.6823417656249899377, 3.176041667008085323, -1.181850606188754593 ) ) ;
#47635 = CARTESIAN_POINT ( 'NONE',  ( 5.883451020920152708, 1.946514763749309429, -0.8046133670899023871 ) ) ;
#47634 = CARTESIAN_POINT ( 'NONE',  ( -7.711890448074853133, 7.891627032375787998, -0.7998128361456291469 ) ) ;
#47636 = CARTESIAN_POINT ( 'NONE',  ( 6.391088794356012848, 0.1989163192229244648, 2.060770550043041993 ) ) ;
#47637 = CARTESIAN_POINT ( 'NONE',  ( 7.156006149914539982, 7.243095351188763686, 1.040834085586084257E-14 ) ) ;
#47638 = CARTESIAN_POINT ( 'NONE',  ( -7.400052914960538963, 7.527816577075747695, 1.040834085586084257E-14 ) ) ;
#47639 = AXIS2_PLACEMENT_3D ( 'NONE', #210041, #75798, #80057 ) ;
#47640 = CARTESIAN_POINT ( 'NONE',  ( 6.539320575229290000, 0.004092658091040673150, 2.003502637948690879 ) ) ;
#47641 = CARTESIAN_POINT ( 'NONE',  ( 4.328955620115590541, 0.09577655398496780215, 1.969249263103334702 ) ) ;
#47642 = CARTESIAN_POINT ( 'NONE',  ( -0.1577409392781377873, -1.310076727147227560, -1.668215054097483385 ) ) ;
#47643 = CARTESIAN_POINT ( 'NONE',  ( 1.499999999999989120, 0.8062500006828163812, 0.000000000000000000 ) ) ;
#47644 = CARTESIAN_POINT ( 'NONE',  ( 4.407023800010228420, 1.785630936674869274, -1.461832730142158088 ) ) ;
#47645 = CARTESIAN_POINT ( 'NONE',  ( 1.604420861476773208, 2.060019368494928838, 0.1054051996416793119 ) ) ;
#47646 = CARTESIAN_POINT ( 'NONE',  ( 6.141480397310468575, 10.10888486359680982, 1.040834085586084257E-14 ) ) ;
#47647 = ADVANCED_FACE ( 'NONE', ( #23147 ), #174790, .T. ) ;
#47648 = CARTESIAN_POINT ( 'NONE',  ( 4.206772801990143584, 8.129928378955675328, 0.7998128361456271485 ) ) ;
#47649 = CARTESIAN_POINT ( 'NONE',  ( 5.923986774528332333, 5.876015756563318426, -0.7998128361456481317 ) ) ;
#47650 = CARTESIAN_POINT ( 'NONE',  ( -1.364683531250000748, 1.571875000341421691, 0.000000000000000000 ) ) ;
#47651 = CARTESIAN_POINT ( 'NONE',  ( 4.848976215542928792, 5.686169002002086970, 1.199719254218452047 ) ) ;
#47652 = CARTESIAN_POINT ( 'NONE',  ( 5.938108092661121162, 9.871617174839238729, 1.040834085586084257E-14 ) ) ;
#47653 = CARTESIAN_POINT ( 'NONE',  ( 3.772083221923136609, -2.139637338432040181, 0.3678540365955537128 ) ) ;
#47654 = CARTESIAN_POINT ( 'NONE',  ( -3.129460678718345878, 6.444905630999884671, -0.7687999843507524744 ) ) ;
#47656 = CARTESIAN_POINT ( 'NONE',  ( 3.350949008998193257, 0.4442310927498266948, -1.786741727165648497 ) ) ;
#47655 = CARTESIAN_POINT ( 'NONE',  ( -3.795919822146289313, 5.451659097302528068, -1.443375672974053447 ) ) ;
#47657 = CARTESIAN_POINT ( 'NONE',  ( 0.6823417656249917140, 5.342708333674749177, 1.181850606188765695 ) ) ;
#47658 = CARTESIAN_POINT ( 'NONE',  ( 5.864808805604324604, 0.1626094438406736342, -2.185560445749204828 ) ) ;
#47659 = CARTESIAN_POINT ( 'NONE',  ( 8.210118869120222485, 14.14525406291519261, 8.752433360441910892 ) ) ;
#47660 = CARTESIAN_POINT ( 'NONE',  ( 5.735331106285326719, -2.048134886816056266, 0.9616036564972543221 ) ) ;
#47661 = CARTESIAN_POINT ( 'NONE',  ( -4.957984823605727343, 6.829280066411827832, -1.450623857674667283 ) ) ;
#47662 = CARTESIAN_POINT ( 'NONE',  ( 4.609415035364720303, 8.472105597856021575, 0.2450749143364742144 ) ) ;
#47663 = CARTESIAN_POINT ( 'NONE',  ( -5.194182247366913252, 7.153241603385088965, 1.443375672974058777 ) ) ;
#47664 = CARTESIAN_POINT ( 'NONE',  ( 4.760321332173959696, 4.726332107057286791, 0.000000000000000000 ) ) ;
#47665 = CARTESIAN_POINT ( 'NONE',  ( 6.802016525601501051, -1.769270574432443510, 0.04669485764256275928 ) ) ;
#47666 = CARTESIAN_POINT ( 'NONE',  ( 1.364683531249997417, 11.98437500034139980, 2.602085213965210642E-15 ) ) ;
#47667 = CARTESIAN_POINT ( 'NONE',  ( 3.774091158939500978, 1.997611739970482692, -0.2487840229714877727 ) ) ;
#47668 = CARTESIAN_POINT ( 'NONE',  ( 5.361359679200154105, 8.342337828120466980, 1.199719254218462483 ) ) ;
#47669 = CARTESIAN_POINT ( 'NONE',  ( 2.643703295229280936, -1.559600718570711031, -1.415347570850413739 ) ) ;
#47670 = CARTESIAN_POINT ( 'NONE',  ( 2.267068109148970834, 1.750504415394140922, -0.7784415599910772254 ) ) ;
#47671 = CARTESIAN_POINT ( 'NONE',  ( 5.196852952739813070, 4.957416621151553571, -0.7998128361456221525 ) ) ;
#47672 = CARTESIAN_POINT ( 'NONE',  ( 2.822656803168353434, -1.360269829074612469, 1.424587346448534353 ) ) ;
#47673 = CARTESIAN_POINT ( 'NONE',  ( 1.252583056964752029, -1.476889893665521925, 1.148006582770304096 ) ) ;
#47674 = CARTESIAN_POINT ( 'NONE',  ( 1.627322669196319849, 0.1476378700930695564, -1.956383933670035713 ) ) ;
#47677 = VERTEX_POINT ( 'NONE', #39424 ) ;
#47676 = CARTESIAN_POINT ( 'NONE',  ( 0.3164790345465406385, -0.6463921985436006379, -1.799943259716822341 ) ) ;
#47675 = CARTESIAN_POINT ( 'NONE',  ( 3.721100771531059781, -0.1247040890464539975, 1.720429258078775669 ) ) ;
#47679 = CARTESIAN_POINT ( 'NONE',  ( 5.124618876285529367, 7.962177208099690873, -1.082531754730549078 ) ) ;
#47678 = CARTESIAN_POINT ( 'NONE',  ( 1.120068590173186163, -2.152398693614396397, 0.4866647226241942459 ) ) ;
#47680 = CARTESIAN_POINT ( 'NONE',  ( -0.6823417656250003738, 1.030208333674752286, -1.181850606188749264 ) ) ;
#47681 = CARTESIAN_POINT ( 'NONE',  ( 1.419999999999987272, 2.244000000000016648, 2.508000000000020435 ) ) ;
#47682 = CARTESIAN_POINT ( 'NONE',  ( 0.2082862990473907383, 7.047992147687566877, -4.030656196916692302 ) ) ;
#47683 = DIRECTION ( 'NONE',  ( 0.000000000000000000, 1.000000000000000000, 0.000000000000000000 ) ) ;
#47684 = CARTESIAN_POINT ( 'NONE',  ( 6.649288540346695697, 1.804226486660088558, -1.015068834323729297 ) ) ;
#47685 = CARTESIAN_POINT ( 'NONE',  ( 1.117730493923989599, 0.4056601665377962407, -2.030061024271647252 ) ) ;
#47686 = CARTESIAN_POINT ( 'NONE',  ( -0.7500000000000006661, 1.608333333333357373, -1.299038105676652011 ) ) ;
#47687 = CARTESIAN_POINT ( 'NONE',  ( 5.425234023762710578, 9.481190127698507553, -0.7998128361456291469 ) ) ;
#47688 = CARTESIAN_POINT ( 'NONE',  ( -7.446452682403657874, 9.710614100936176385, -1.599625672291263179 ) ) ;
#47689 = CARTESIAN_POINT ( 'NONE',  ( 5.554000203453580475, 6.508696987897830688, -1.199719254218452047 ) ) ;
#47690 = CARTESIAN_POINT ( 'NONE',  ( 5.531924462405465981, -2.068776410037334479, 0.4646945096876684556 ) ) ;
#47691 = CARTESIAN_POINT ( 'NONE',  ( 5.096939404094710468, 4.911127157724081371, 0.000000000000000000 ) ) ;
#47692 = CARTESIAN_POINT ( 'NONE',  ( -1.364683531250000748, 1.759375000341421913, 0.000000000000000000 ) ) ;
#47693 = CARTESIAN_POINT ( 'NONE',  ( -1.201851678989727383E-14, 1.962500000000020783, 1.732050807568877637 ) ) ;
#47695 = CARTESIAN_POINT ( 'NONE',  ( 8.581948047770334043, 12.95609712246668899, 0.000000000000000000 ) ) ;
#47694 = CARTESIAN_POINT ( 'NONE',  ( 6.232861002365865488, -1.862453515449840724, -0.6167318247369477646 ) ) ;
#47696 = CARTESIAN_POINT ( 'NONE',  ( 3.761092154037175117, -2.013677596940225190, -0.1017350580494805479 ) ) ;
#47697 = ADVANCED_FACE ( 'NONE', ( #105518 ), #135360, .T. ) ;
#47698 = CARTESIAN_POINT ( 'NONE',  ( 4.153473468168114913, 1.856699357379907989, -0.4712526737844865976 ) ) ;
#47699 =( NAMED_UNIT ( * ) PLANE_ANGLE_UNIT ( ) SI_UNIT ( $, .RADIAN. ) );
#47700 = CARTESIAN_POINT ( 'NONE',  ( 1.435386855117400717, -1.590506285900999295, -1.507976327226906443 ) ) ;
#47701 = DIRECTION ( 'NONE',  ( -0.9982742078614211811, 0.000000000000000000, 0.05872483221476467591 ) ) ;
#47702 = CARTESIAN_POINT ( 'NONE',  ( 4.288257209584379837, -1.849852534125648207, -0.2767368629695772797 ) ) ;
#47703 = CARTESIAN_POINT ( 'NONE',  ( -0.7500000000000249800, 0.2229166673494847872, 1.299038105676659116 ) ) ;
#47704 = CARTESIAN_POINT ( 'NONE',  ( -5.693534442735004752, 8.729875052244421951, 1.199719254218452047 ) ) ;
#47706 = CARTESIAN_POINT ( 'NONE',  ( 5.431313658478175377, -1.669672585088026517, -1.301796502452344129 ) ) ;
#47705 = CARTESIAN_POINT ( 'NONE',  ( -5.287316719649550301, 5.270883715786984780, 0.7216878364870317197 ) ) ;
#47707 = CARTESIAN_POINT ( 'NONE',  ( 1.364683531250000303, 8.567708333674730170, -0.7879004041258355073 ) ) ;
#47709 = DIRECTION ( 'NONE',  ( -1.000000000000000000, 0.000000000000000000, 0.000000000000000000 ) ) ;
#47708 = CARTESIAN_POINT ( 'NONE',  ( 2.278955919255227336, 1.910372346673551602, -0.8499720230255493059 ) ) ;
#47711 = ORIENTED_EDGE ( 'NONE', *, *, #104171, .T. ) ;
#47710 = CARTESIAN_POINT ( 'NONE',  ( 0.7446035987349702845, -1.482829294443729351, 0.8806902949074472131 ) ) ;
#47712 = CARTESIAN_POINT ( 'NONE',  ( 7.461064606222022277, 7.598996883547496139, 1.040834085586084257E-14 ) ) ;
#47713 = CARTESIAN_POINT ( 'NONE',  ( -5.608757509019071996, 5.629766575911039794, 0.4613631940431175416 ) ) ;
#47714 = DIRECTION ( 'NONE',  ( 1.000000000000000000, 0.000000000000000000, 0.000000000000000000 ) ) ;
#47715 = CARTESIAN_POINT ( 'NONE',  ( 6.661184053807540195, -7.645781813054109755, -6.773376336901701045 ) ) ;
#47717 = CARTESIAN_POINT ( 'NONE',  ( 9.381879110532285182, 10.04787317181692075, 0.000000000000000000 ) ) ;
#47716 = CARTESIAN_POINT ( 'NONE',  ( 5.635385404774530649, 9.726366738878972740, 0.7998128361456462443 ) ) ;
#47718 = ORIENTED_EDGE ( 'NONE', *, *, #160495, .T. ) ;
#47719 = CARTESIAN_POINT ( 'NONE',  ( -1.874158809982179319, 3.299964346911585356, 0.3999999999999993006 ) ) ;
#47720 = VERTEX_POINT ( 'NONE', #65254 ) ;
#47722 = CARTESIAN_POINT ( 'NONE',  ( 1.594102673003819248, -0.9688845198280521265, 1.530366366333405281 ) ) ;
#47721 = CARTESIAN_POINT ( 'NONE',  ( 6.852720297064418986, 6.959538199522133262, 0.7998128361456331437 ) ) ;
#47723 = CARTESIAN_POINT ( 'NONE',  ( -7.854251061018346469, 8.057714414143200443, -0.7998128361456291469 ) ) ;
#47724 = VECTOR ( 'NONE', #1342, 1000.000000000000000 ) ;
#47725 = CARTESIAN_POINT ( 'NONE',  ( 5.515469562660962666, 5.329135999392899947, 0.7998128361456341429 ) ) ;
#47726 = CARTESIAN_POINT ( 'NONE',  ( 5.363132282657546490, 8.414682208812571673, -1.199719254218452047 ) ) ;
#47727 = CARTESIAN_POINT ( 'NONE',  ( 6.639320575229254118, 4.698690022235154196, 2.459427960261594492 ) ) ;
#47728 = CARTESIAN_POINT ( 'NONE',  ( 4.707534831891463156, 6.823246043637223757, 1.233988984638714426 ) ) ;
#47729 = CARTESIAN_POINT ( 'NONE',  ( 8.270110514656016321, 12.59228666716665401, 0.7216878364870438212 ) ) ;
#47730 = ORIENTED_EDGE ( 'NONE', *, *, #96602, .T. ) ;
#47731 = CARTESIAN_POINT ( 'NONE',  ( 3.297144150320669542, -1.642529969829407577, 0.8749454559845524226 ) ) ;
#47732 = CARTESIAN_POINT ( 'NONE',  ( 0.9486861286592045417, -1.732399544687371229, -0.8177760133930843667 ) ) ;
#47733 = CARTESIAN_POINT ( 'NONE',  ( 6.581085459773934332, -0.09550846514571986745, -1.924131155975503216 ) ) ;
#47734 = FACE_OUTER_BOUND ( 'NONE', #39583, .T. ) ;
#47735 = CYLINDRICAL_SURFACE ( 'NONE', #26116, 1.250000000000000000 ) ;
#47737 = AXIS2_PLACEMENT_3D ( 'NONE', #174060, #175117, #112297 ) ;
#47736 = CIRCLE ( 'NONE', #199977, 0.08000000000000012657 ) ;
#47738 = CARTESIAN_POINT ( 'NONE',  ( 4.629651883607522223, 8.329987488807731211, -0.3686744245932921937 ) ) ;
#47739 = CARTESIAN_POINT ( 'NONE',  ( -2.550000000000001155, -7.105553651663779391, -1.849324200890690717 ) ) ;
#47740 = CARTESIAN_POINT ( 'NONE',  ( -4.473827502829599290, 4.321812962830357208, 0.7216878364870317197 ) ) ;
#47741 = CARTESIAN_POINT ( 'NONE',  ( 6.616015773788773480, 10.66250946948817813, -0.7216878364870267237 ) ) ;
#47742 = CARTESIAN_POINT ( 'NONE',  ( 4.100420354389649802, 1.959567862165834562, 0.1972540966053982214 ) ) ;
#47743 = CARTESIAN_POINT ( 'NONE',  ( 1.770341816056511863, 2.114587264445011883, -0.1591180397043714667 ) ) ;
#47744 = CARTESIAN_POINT ( 'NONE',  ( -5.555090253297260361, 7.504024600312024340, 1.599625672291269396 ) ) ;
#47745 = PLANE ( 'NONE',  #73268 ) ;
#47747 = ADVANCED_FACE ( 'NONE', ( #49043 ), #211513, .F. ) ;
#47746 = CYLINDRICAL_SURFACE ( 'NONE', #139260, 1.500000000000000222 ) ;
#47748 = CARTESIAN_POINT ( 'NONE',  ( 5.542994302928621053, -1.725804593724251657, -1.350479894307685447 ) ) ;
#47749 = CARTESIAN_POINT ( 'NONE',  ( 4.752910067621118451, -1.547527511699481106, 1.147055677608086466 ) ) ;
#47750 = CARTESIAN_POINT ( 'NONE',  ( -5.343885102080728977, 9.386283052402845328, 0.7998128361456481317 ) ) ;
#47751 = CARTESIAN_POINT ( 'NONE',  ( 0.5338675855391886715, 0.9430634504648884864, -1.562995807167219642 ) ) ;
#47752 = CARTESIAN_POINT ( 'NONE',  ( 1.436444770134176485, 1.085300811998829662, -1.921501399296850821 ) ) ;
#47753 = CARTESIAN_POINT ( 'NONE',  ( -6.024748404907106725, 7.078120102419984683, 1.049236913528932780 ) ) ;
#47754 = CARTESIAN_POINT ( 'NONE',  ( 0.000000000000000000, -3.517800438942085606, 3.000000000000000000 ) ) ;
#47755 = EDGE_CURVE ( 'NONE', #199511, #152913, #55867, .T. ) ;
#47756 = VERTEX_POINT ( 'NONE', #14374 ) ;
#47757 = CARTESIAN_POINT ( 'NONE',  ( 3.092668437693027794, 6.622213920701574885, -0.7216878364870338292 ) ) ;
#47758 = VERTEX_POINT ( 'NONE', #181157 ) ;
#47759 = CARTESIAN_POINT ( 'NONE',  ( 6.772316245210458163, -0.9252316606085030370, -1.738535334629727647 ) ) ;
#47760 = CARTESIAN_POINT ( 'NONE',  ( 1.013109794239855699, -1.894405189233986597, 0.4268842903399574507 ) ) ;
#47761 = CARTESIAN_POINT ( 'NONE',  ( 0.9134352171796227271, 0.5825640498151598567, 1.930122961472901855 ) ) ;
#47763 = CARTESIAN_POINT ( 'NONE',  ( 5.436322145542998641, -1.035505548906799023, 1.546008503351968821 ) ) ;
#47762 = CARTESIAN_POINT ( 'NONE',  ( -5.764151584465413869, 6.753873599078290546, -1.199719254218453823 ) ) ;
#47764 = CARTESIAN_POINT ( 'NONE',  ( 4.715203562502613188, 8.723097599553565118, 0.7998128361456341429 ) ) ;
#47766 = ADVANCED_FACE ( 'NONE', ( #210448 ), #159579, .T. ) ;
#47765 = CARTESIAN_POINT ( 'NONE',  ( 0.7500000000000006661, 11.33333333333333393, 1.299038105676657340 ) ) ;
#47767 = CARTESIAN_POINT ( 'NONE',  ( 1.836970198721030181E-16, 13.49999999999999822, 1.500000000000000222 ) ) ;
#47768 = CARTESIAN_POINT ( 'NONE',  ( -4.720210035852093533, 8.658662141802762946, -0.7998128361456281477 ) ) ;
#47769 = CARTESIAN_POINT ( 'NONE',  ( -6.936931872047518155, 8.122117267924091166, 1.199719254218452047 ) ) ;
#47770 = CARTESIAN_POINT ( 'NONE',  ( 1.136565065649897344, 0.4323997850379875385, 2.148315308122191514 ) ) ;
#47771 = CARTESIAN_POINT ( 'NONE',  ( 2.887523530030648988, 6.312601851770308414, 0.000000000000000000 ) ) ;
#47772 = CARTESIAN_POINT ( 'NONE',  ( 0.000000000000000000, -0.6185895741317448682, 0.000000000000000000 ) ) ;
#47773 = DIRECTION ( 'NONE',  ( -0.6507913734559640506, 0.7592566023653005702, 0.000000000000000000 ) ) ;
#47774 = CARTESIAN_POINT ( 'NONE',  ( 1.137010146156680834, -1.651496384925277283, 0.7785749969668461778 ) ) ;
#47775 = CARTESIAN_POINT ( 'NONE',  ( -2.123823618835070537, 5.629544655282869847, 1.040834085586084257E-14 ) ) ;
#47776 = CIRCLE ( 'NONE', #58098, 0.09999999999999982514 ) ;
#47777 = CARTESIAN_POINT ( 'NONE',  ( -0.2880152382563990754, 3.298359159248693828, -1.980637607101966235 ) ) ;
#47778 = CARTESIAN_POINT ( 'NONE',  ( 6.609000000000047947, 7.629137130509099585, 2.499999999999994227 ) ) ;
#47779 = CARTESIAN_POINT ( 'NONE',  ( 8.890396042259068210, 11.39521468743417998, -1.599625672291257406 ) ) ;
#47780 = CARTESIAN_POINT ( 'NONE',  ( 6.375623774462673587, 1.745513195383348926, -0.5351242734627087438 ) ) ;
#47781 = CARTESIAN_POINT ( 'NONE',  ( 4.487127722112081329, 0.09209952633786909482, 1.959694304038139379 ) ) ;
#47782 = AXIS2_PLACEMENT_3D ( 'NONE', #53280, #102033, #205918 ) ;
#47783 = CARTESIAN_POINT ( 'NONE',  ( -8.040148788103921973, 9.338927326664741457, 1.199719254218462483 ) ) ;
#47784 = CARTESIAN_POINT ( 'NONE',  ( 4.638861114170084399, 8.563755066507100722, 0.7998128361456462443 ) ) ;
#47785 = CARTESIAN_POINT ( 'NONE',  ( 4.230150181147958044, 2.149441460308566754, 0.4267382380854707336 ) ) ;
#47786 = ADVANCED_FACE ( 'NONE', ( #12246 ), #110894, .F. ) ;
#47787 = CARTESIAN_POINT ( 'NONE',  ( -0.7500000000000179856, 9.822916667349467446, 1.299038105676658228 ) ) ;
#47788 = CARTESIAN_POINT ( 'NONE',  ( 3.942288228968212849, -1.024710522258945655, 1.798826465557185506 ) ) ;
#47789 = CARTESIAN_POINT ( 'NONE',  ( -0.6823417656250003738, 1.030208333674752286, -1.181850606188749264 ) ) ;
#47790 = ORIENTED_EDGE ( 'NONE', *, *, #90996, .T. ) ;
#47791 = CARTESIAN_POINT ( 'NONE',  ( 4.096513536321761073, -0.3929280286100769182, 2.264727396410810556 ) ) ;
#47792 = CARTESIAN_POINT ( 'NONE',  ( 8.161645285746708112, 9.584636257201740506, -1.082531754730543083 ) ) ;
#47794 = CARTESIAN_POINT ( 'NONE',  ( -3.285556943750000514, -0.8385416661887076240, -1.896917185911906500 ) ) ;
#47793 = CARTESIAN_POINT ( 'NONE',  ( 6.536439455564168277, 6.798469917679251573, 0.7216878364870328300 ) ) ;
#47795 = CARTESIAN_POINT ( 'NONE',  ( -0.4019237886467001974, 8.332585450998168497, 1.500000000000001998 ) ) ;
#47796 = CARTESIAN_POINT ( 'NONE',  ( -10.28236465222290441, 4.804674082874877072, -6.107148855343119465 ) ) ;
#47797 = B_SPLINE_CURVE_WITH_KNOTS ( 'NONE', 3,
 ( #202783, #36029, #52295, #203849, #5634, #154069 ),
 .UNSPECIFIED., .F., .F.,
 ( 4, 2, 4 ),
 ( 0.001251957608719239451, 0.001565178843344208238, 0.001878400077969176810 ),
 .UNSPECIFIED. ) ;
#47798 = CARTESIAN_POINT ( 'NONE',  ( 4.048723784538146298, -1.615201170136868924, -1.077811959465636571 ) ) ;
#47799 = ORIENTED_EDGE ( 'NONE', *, *, #188668, .T. ) ;
#47800 = CARTESIAN_POINT ( 'NONE',  ( 8.527715432871318058, 12.89282573841782664, -0.7216878364870338292 ) ) ;
#47801 = CARTESIAN_POINT ( 'NONE',  ( 3.832203377193269755, -0.9874410831685247469, -1.637625244210038300 ) ) ;
#47802 = CARTESIAN_POINT ( 'NONE',  ( 4.763909876611899463, 5.178992836847385206, -0.8608806284969447997 ) ) ;
#47803 = CARTESIAN_POINT ( 'NONE',  ( 5.754863291335100328, -1.356889945763246841, 1.064653683861387812 ) ) ;
#47804 = CARTESIAN_POINT ( 'NONE',  ( 4.135954056172497673, 2.015980767636461835, -0.05432360925018697717 ) ) ;
#47805 = CARTESIAN_POINT ( 'NONE',  ( 5.379591378607442742, -0.5557209876673010474, -2.230391596181950042 ) ) ;
#47806 = CARTESIAN_POINT ( 'NONE',  ( 11.55950211276791251, 12.21999999999998288, 3.221476510067110777 ) ) ;
#47807 = CARTESIAN_POINT ( 'NONE',  ( 0.3115100037339203487, 1.922317768103290803, 1.083863418116323807 ) ) ;
#47809 = CARTESIAN_POINT ( 'NONE',  ( -5.492461627311929995, 5.580495784718250363, 0.000000000000000000 ) ) ;
#47808 = CARTESIAN_POINT ( 'NONE',  ( -8.618179199781044630, 13.20629283305325963, 0.7998128361456341429 ) ) ;
#47810 = CARTESIAN_POINT ( 'NONE',  ( 5.589024195967314590, 1.560314836579352438, -0.8350092274562578298 ) ) ;
#47812 = CARTESIAN_POINT ( 'NONE',  ( 1.799181239640806007, 1.907565883177517740, 1.270813247315852879 ) ) ;
#47811 = CARTESIAN_POINT ( 'NONE',  ( 5.580062740476173566, 8.667767742934335828, 1.199719254218451159 ) ) ;
#47813 = CARTESIAN_POINT ( 'NONE',  ( 1.341335103225870240, 1.738211624227633978, 0.08822054626196448868 ) ) ;
#47814 = VECTOR ( 'NONE', #158028, 1000.000000000000000 ) ;
#47815 = CARTESIAN_POINT ( 'NONE',  ( 0.000000000000000000, 2.800000000000024691, 1.214306433183764966E-14 ) ) ;
#47816 = CARTESIAN_POINT ( 'NONE',  ( 0.8778075154764168886, -0.2618308253583972456, 1.713820766736633194 ) ) ;
#47817 = CARTESIAN_POINT ( 'NONE',  ( 1.360316468749957597, 0.7760416670081098367, 0.7853790794158520550 ) ) ;
#47818 = MECHANICAL_DESIGN_GEOMETRIC_PRESENTATION_REPRESENTATION (  '', ( #213810 ), #41433 ) ;
#47819 = CARTESIAN_POINT ( 'NONE',  ( -11.55950211276791251, 12.29999999999998472, 3.221476510067111665 ) ) ;
#47820 = CARTESIAN_POINT ( 'NONE',  ( 0.9245737983274513461, 1.070221580302813891, 1.888989948743382552 ) ) ;
#47821 = CARTESIAN_POINT ( 'NONE',  ( 2.325407997918966796, -1.497503195670712328, -1.350734289967000512 ) ) ;
#47822 = CARTESIAN_POINT ( 'NONE',  ( 1.499999999999987121, 0.5354166673494816786, 0.8660254037844524744 ) ) ;
#47823 = CARTESIAN_POINT ( 'NONE',  ( 0.2879446430137333479, -0.9113367411649232475, 1.697199823463049428 ) ) ;
#47824 = CARTESIAN_POINT ( 'NONE',  ( -8.012344526598182026E-15, 12.54687500034139624, -1.575800808251669460 ) ) ;
#47825 = CARTESIAN_POINT ( 'NONE',  ( 1.969254952099579459, -1.713688747078499830, 1.413451004025434665 ) ) ;
#47826 = ORIENTED_EDGE ( 'NONE', *, *, #159504, .F. ) ;
#47827 = CARTESIAN_POINT ( 'NONE',  ( -9.579253414572390213, -9.994362535427860905, 0.1002978391578569772 ) ) ;
#47828 = CARTESIAN_POINT ( 'NONE',  ( -0.7500000000000006661, -0.3916666666666443475, -1.299038105676652011 ) ) ;
#47829 = CARTESIAN_POINT ( 'NONE',  ( 9.589694723567584234, 10.08239868711733855, -0.7998128361456281477 ) ) ;
#47830 =( NAMED_UNIT ( * ) SI_UNIT ( $, .STERADIAN. ) SOLID_ANGLE_UNIT ( ) );
#47831 = CARTESIAN_POINT ( 'NONE',  ( -15.75000000000000000, 10.19999999999999929, -1.800000000000001155 ) ) ;
#47832 = PRESENTATION_LAYER_ASSIGNMENT (  '', '', ( #206887 ) ) ;
#47833 = CARTESIAN_POINT ( 'NONE',  ( 5.477983384163819025, -1.699738153848131983, -0.3734572171999461232 ) ) ;
#47834 = CARTESIAN_POINT ( 'NONE',  ( 3.086327779807009009, 1.092107249913790712, -1.629585102321646328 ) ) ;
#47836 = CARTESIAN_POINT ( 'NONE',  ( -6.046573322014817897, 9.998159942418544333, 0.7216878364870458196 ) ) ;
#47835 = CARTESIAN_POINT ( 'NONE',  ( 9.571693261567954636, 12.19006144329456731, 1.443375672974076540 ) ) ;
#47837 = CARTESIAN_POINT ( 'NONE',  ( -1.493932498646918017, 4.331812005461956439, -0.1507059531854464673 ) ) ;
#47838 = CARTESIAN_POINT ( 'NONE',  ( 4.569752015286022484, 2.196007708051894269, -0.5437172964835658151 ) ) ;
#47839 = CARTESIAN_POINT ( 'NONE',  ( 1.557159421845564218, 1.687539990290163772, -1.185865425756290392 ) ) ;
#47840 = CARTESIAN_POINT ( 'NONE',  ( -6.693975156845199059, 8.832723654451292816, 1.599625672291283607 ) ) ;
#47841 = CARTESIAN_POINT ( 'NONE',  ( 2.008995473212730865, 1.676182761729711590, -1.519857458481475909 ) ) ;
#47842 = ORIENTED_EDGE ( 'NONE', *, *, #73745, .F. ) ;
#47843 = CARTESIAN_POINT ( 'NONE',  ( 0.7499999999999902300, 1.764583334016148086, 1.299038105676657340 ) ) ;
#47844 = CARTESIAN_POINT ( 'NONE',  ( 2.600682448077856090, 1.504852936121018558, -1.110837741034584436 ) ) ;
#47845 = CARTESIAN_POINT ( 'NONE',  ( 1.828352651294574249, 0.6632370903016276964, -1.602517542597500455 ) ) ;
#47846 = CARTESIAN_POINT ( 'NONE',  ( 5.126606437771586755, 0.1607948393855564151, 2.185736094377451089 ) ) ;
#47847 = CARTESIAN_POINT ( 'NONE',  ( 6.581126798121099242, -0.1039769691308822797, -2.305377512668804751 ) ) ;
#47848 = CARTESIAN_POINT ( 'NONE',  ( 4.381803836707322652, 1.409801062080328959, 1.638821348427916602 ) ) ;
#47849 = CARTESIAN_POINT ( 'NONE',  ( 4.224509699451983735, 0.09670237001900212903, 1.939662488567380993 ) ) ;
#47850 = CARTESIAN_POINT ( 'NONE',  ( -9.022061154889962964, 12.61315621642528129, -1.199719254218446718 ) ) ;
#47851 = CARTESIAN_POINT ( 'NONE',  ( 6.503191328365395485, 1.555263205862934983, 1.038959965768880389 ) ) ;
#47852 = CARTESIAN_POINT ( 'NONE',  ( 1.750000000000001332, 1.008799782768345906E-13, 2.052068128417951165 ) ) ;
#47853 = CARTESIAN_POINT ( 'NONE',  ( 4.171261675657679469, 7.370687464442305270, 0.7961138118306176903 ) ) ;
#47854 = CARTESIAN_POINT ( 'NONE',  ( 6.717278222822382183, -7.473374494058216300, -6.830415307812249814 ) ) ;
#47855 = CARTESIAN_POINT ( 'NONE',  ( 3.851925040058331806, 5.587274861525073355, -1.443375672974066548 ) ) ;
#47856 = CARTESIAN_POINT ( 'NONE',  ( -0.6801582343750091075, 2.848958333674732391, -1.178068619123848526 ) ) ;
#47857 = CARTESIAN_POINT ( 'NONE',  ( 5.572888750952301073, -0.9041123360693378297, 1.802415994888312722 ) ) ;
#47858 = CARTESIAN_POINT ( 'NONE',  ( -9.642873567817536795, 12.27310513391906532, 1.599625672291281386 ) ) ;
#47859 = CARTESIAN_POINT ( 'NONE',  ( 8.015895134177609904, 10.37496362800581018, 1.599625672291281386 ) ) ;
#47860 =( REPRESENTATION_RELATIONSHIP ('NONE','NONE', #84563, #149737 ) REPRESENTATION_RELATIONSHIP_WITH_TRANSFORMATION ( #76314 )SHAPE_REPRESENTATION_RELATIONSHIP( ) );
#47861 = CARTESIAN_POINT ( 'NONE',  ( 11.94105721237523277, 12.69999999999999929, 1.187919463087244720 ) ) ;
#47863 = FILL_AREA_STYLE ('',( #133378 ) ) ;
#47862 = CARTESIAN_POINT ( 'NONE',  ( 2.736711336054332921, 0.2235625380298221498, 1.811883384933578256 ) ) ;
#47864 = CARTESIAN_POINT ( 'NONE',  ( -6.446420058208179427, -6.527411821100059797, -7.058808231563611812 ) ) ;
#47865 = ORIENTED_EDGE ( 'NONE', *, *, #2982, .F. ) ;
#47866 = CARTESIAN_POINT ( 'NONE',  ( -4.624739795592936353, 7.449261290616792763, -1.082531754730549967 ) ) ;
#47867 = CARTESIAN_POINT ( 'NONE',  ( -3.285556943749998737, -3.317708332855375808, 1.896917185911908499 ) ) ;
#47868 = CARTESIAN_POINT ( 'NONE',  ( -9.429859533504656000, 10.96025652963230534, -1.199719254218441611 ) ) ;
#47869 = CARTESIAN_POINT ( 'NONE',  ( 0.08815677907929740653, 1.166467155405017442, 1.648690671293622012 ) ) ;
#47870 = CARTESIAN_POINT ( 'NONE',  ( 0.9090200710941964690, -0.5189423241485704441, -2.055877189782874481 ) ) ;
#47871 = EDGE_LOOP ( 'NONE', ( #181428, #31962, #206862, #88402 ) ) ;
#47872 = CARTESIAN_POINT ( 'NONE',  ( -4.664887371553763096, 7.600063145858131364, -1.199719254218453823 ) ) ;
#47873 = CARTESIAN_POINT ( 'NONE',  ( 3.785751206713845018, 5.439795712631356750, 1.599625672291267398 ) ) ;
#47874 = CARTESIAN_POINT ( 'NONE',  ( 0.1808504484964272296, -2.097240537080494516, -0.5235256853268267507 ) ) ;
#47875 = CARTESIAN_POINT ( 'NONE',  ( -11.33772463945037146, 13.39999999999998259, 3.679999999999999272 ) ) ;
#47876 = ORIENTED_EDGE ( 'NONE', *, *, #156690, .T. ) ;
#47877 = CARTESIAN_POINT ( 'NONE',  ( -9.755255220232635693, 11.33988483081495957, -1.199719254218441611 ) ) ;
#47878 = CARTESIAN_POINT ( 'NONE',  ( -11.41381675112453387, 12.69999999999998153, 3.704697986577180746 ) ) ;
#47879 = AXIS2_PLACEMENT_3D ( 'NONE', #103704, #149238, #20292 ) ;
#47882 = ORIENTED_EDGE ( 'NONE', *, *, #167677, .F. ) ;
#47881 = CARTESIAN_POINT ( 'NONE',  ( -6.343551558972095883, 6.506286488053499184, 2.499999999999999556 ) ) ;
#47880 = CARTESIAN_POINT ( 'NONE',  ( -6.317173229324657413, 6.334733287159020954, 0.000000000000000000 ) ) ;
#47883 = CARTESIAN_POINT ( 'NONE',  ( 5.420206975164616026, 7.644856803259713729, 1.330009527941821368 ) ) ;
#47884 = CARTESIAN_POINT ( 'NONE',  ( 5.764999918528635803, -2.016288307888712161, -0.002809016773450134351 ) ) ;
#47885 = CARTESIAN_POINT ( 'NONE',  ( 5.033073903806924321, -1.304366766181121573, -1.299653785596634137 ) ) ;
#47886 = FACE_OUTER_BOUND ( 'NONE', #30266, .T. ) ;
#47887 = CARTESIAN_POINT ( 'NONE',  ( 3.176728247877279365, -1.374524503021319344, 1.853549100471873823 ) ) ;
#47889 = CARTESIAN_POINT ( 'NONE',  ( 6.364626766972446781, 6.390095747748157251, 0.7998128361456352531 ) ) ;
#47888 = B_SPLINE_CURVE_WITH_KNOTS ( 'NONE', 3,
 ( #18382, #65002, #166788, #84460, #113852, #67118, #132192, #50903, #130109, #213379, #196102, #181950, #16240, #49835, #33579, #81275 ),
 .UNSPECIFIED., .F., .F.,
 ( 4, 3, 3, 3, 3, 4 ),
 ( 0.000000000000000000, 3.083448363908645134E-05, 6.173412828017592617E-05, 9.147751612222092168E-05, 0.0001189036761826360979, 0.0001300740652511593359 ),
 .UNSPECIFIED. ) ;
#47890 = CARTESIAN_POINT ( 'NONE',  ( 6.292270065666691892, -2.150519007954437622, -0.2187886337903441336 ) ) ;
#47891 = CARTESIAN_POINT ( 'NONE',  ( 7.121056995675668411, 9.330985799753529264, -1.599625672291262513 ) ) ;
#47892 = CARTESIAN_POINT ( 'NONE',  ( 1.276788482218065734, 1.793752796627584578, -0.7448022267775021854 ) ) ;
#47893 = CARTESIAN_POINT ( 'NONE',  ( -2.923754682041362241, 6.562797562356882608, 0.7998128361456341429 ) ) ;
#47894 = ORIENTED_EDGE ( 'NONE', *, *, #87324, .F. ) ;
#47895 = EDGE_CURVE ( 'NONE', #177149, #104840, #194208, .T. ) ;
#47896 = CARTESIAN_POINT ( 'NONE',  ( 4.991759546967353245, 2.197549137908102246, 0.6733019004761026105 ) ) ;
#47897 = FACE_OUTER_BOUND ( 'NONE', #110527, .T. ) ;
#47898 = CARTESIAN_POINT ( 'NONE',  ( -5.113360211009450040, 5.994616996712990975, -1.199719254218453823 ) ) ;
#47899 = CARTESIAN_POINT ( 'NONE',  ( 4.276139911362797363, -1.077190196239918851, 1.529178877381555335 ) ) ;
#47901 = AXIS2_PLACEMENT_3D ( 'NONE', #207208, #126047, #139036 ) ;
#47900 = AXIS2_PLACEMENT_3D ( 'NONE', #140772, #207850, #125633 ) ;
#47904 = CARTESIAN_POINT ( 'NONE',  ( -6.123442655227560927, 7.173046514967467147, 1.199719254218452047 ) ) ;
#47903 = CARTESIAN_POINT ( 'NONE',  ( -0.7500000000000006661, -0.3604166659838467512, -1.299038105676652011 ) ) ;
#47902 = CARTESIAN_POINT ( 'NONE',  ( 1.529408426332915960, -0.2309274165002393187, 1.898302859121250297 ) ) ;
#47905 = CARTESIAN_POINT ( 'NONE',  ( 2.280145854635793334, 1.358931147977986420, 1.738775483816151768 ) ) ;
#47906 = CARTESIAN_POINT ( 'NONE',  ( -1.536019160937945438, 8.701056780447583350, -2.509677374736781985 ) ) ;
#47907 = CARTESIAN_POINT ( 'NONE',  ( 5.138177029454882749, 5.096887410559832965, 0.7216878364870096263 ) ) ;
#47908 = CARTESIAN_POINT ( 'NONE',  ( 7.010974831598141499, 7.352094523052197239, -0.7216878364870317197 ) ) ;
#47909 = CARTESIAN_POINT ( 'NONE',  ( -2.625475302540713152, 6.214804952939456228, -0.7998128361456281477 ) ) ;
#47910 = CARTESIAN_POINT ( 'NONE',  ( -6.197485614778184271, 9.284131412999601096, 1.082531754730549967 ) ) ;
#47911 = CARTESIAN_POINT ( 'NONE',  ( 2.091034261367350933, 1.717025232345986252, -0.9683794122406997884 ) ) ;
#47912 = CARTESIAN_POINT ( 'NONE',  ( 1.694772972888843210, -2.296637362782745218, -0.2246623637925919403 ) ) ;
#47913 = CARTESIAN_POINT ( 'NONE',  ( 0.8538673084422104820, -0.7095216264049221122, 1.829241926910141203 ) ) ;
#47914 = CARTESIAN_POINT ( 'NONE',  ( 5.401261053844283566, -1.771754184838408630, 1.055722541708886020 ) ) ;
#47915 = CARTESIAN_POINT ( 'NONE',  ( 4.907688418466886304, 5.788353245375237321, -1.082531754730548412 ) ) ;
#47916 = CARTESIAN_POINT ( 'NONE',  ( 5.367048706163317640, 7.354919138647580290, -1.599625672291281386 ) ) ;
#47917 = ORIENTED_EDGE ( 'NONE', *, *, #139916, .F. ) ;
#47918 = CARTESIAN_POINT ( 'NONE',  ( 1.500000000000001332, 10.12500000000000178, 0.000000000000000000 ) ) ;
#47919 = CARTESIAN_POINT ( 'NONE',  ( -4.926979960302503514, 4.882856496153904935, 0.5425924526549028570 ) ) ;
#47920 = CARTESIAN_POINT ( 'NONE',  ( 3.836594282542914236, 5.499112634431936542, 1.443375672974062551 ) ) ;
#47921 = CARTESIAN_POINT ( 'NONE',  ( 0.3566018059198462486, -2.170557273582163216, -0.05455199461934338162 ) ) ;
#47923 = CARTESIAN_POINT ( 'NONE',  ( 5.794452930745782382, 1.501506822132542718, -1.065412412061928160 ) ) ;
#47922 = CARTESIAN_POINT ( 'NONE',  ( -0.04536292375657846598, -10.00000000000003908, -10.91964218157423083 ) ) ;
#47924 = DIRECTION ( 'NONE',  ( -0.7592566023652990159, 0.6507913734559659380, 0.000000000000000000 ) ) ;
#47925 = CARTESIAN_POINT ( 'NONE',  ( -5.311662079954674986, 4.760874550186750653, -2.500000000000000444 ) ) ;
#47926 = CARTESIAN_POINT ( 'NONE',  ( 1.545950201917587696, 1.868165254341861647, 0.09716206808172561660 ) ) ;
#47927 = CARTESIAN_POINT ( 'NONE',  ( 5.729794944320468097, -1.366427417996706417, -1.674954217032841974 ) ) ;
#47928 = CARTESIAN_POINT ( 'NONE',  ( -5.544970132138452357, 6.385306161890050625, 1.248999107086716798 ) ) ;
#47929 = CARTESIAN_POINT ( 'NONE',  ( -0.02244404828160087226, 1.323617703852699057, -2.440988974267483957 ) ) ;
#47930 = CARTESIAN_POINT ( 'NONE',  ( -0.6823417656250003738, -0.7822916663252423852, -1.181850606188749264 ) ) ;
#47931 = CARTESIAN_POINT ( 'NONE',  ( 1.945825403448407487, -1.250168254263404277, -1.447093241409423081 ) ) ;
#47932 = CARTESIAN_POINT ( 'NONE',  ( 3.063107849133941851, 0.2611542325122416797, -1.750338901227658894 ) ) ;
#47933 = CARTESIAN_POINT ( 'NONE',  ( 1.154776974461441341, 0.3738248154092556064, 1.875208037630435864 ) ) ;
#47935 = CARTESIAN_POINT ( 'NONE',  ( 5.431221565750523617, -1.512988070448300970, -1.174818341023081913 ) ) ;
#47934 = LINE ( 'NONE', #84659, #83837 ) ;
#47936 = CARTESIAN_POINT ( 'NONE',  ( 6.725064210944283971, -1.800211566667491825, -0.7994317546313032263 ) ) ;
#47937 = CARTESIAN_POINT ( 'NONE',  ( 0.7499999999999902300, 5.066666666666684193, -1.299038105676658228 ) ) ;
#47938 = CARTESIAN_POINT ( 'NONE',  ( 1.107859837811319581, 1.609452232531217275, 1.380942675281403353 ) ) ;
#47939 = CARTESIAN_POINT ( 'NONE',  ( 3.188928480291412626, 8.980740528189164351, -2.451733079074510435 ) ) ;
#47940 = CARTESIAN_POINT ( 'NONE',  ( 4.996879044411707937, 1.554903924810165705, -1.039696167511289238 ) ) ;
#47942 = ORIENTED_EDGE ( 'NONE', *, *, #201935, .F. ) ;
#47941 = CARTESIAN_POINT ( 'NONE',  ( 0.2756506080626683342, 1.048234779247591453, 1.494575289200591239 ) ) ;
#47944 = CARTESIAN_POINT ( 'NONE',  ( -1.499999999999982903, 4.379166666666687746, -0.8660254037844477004 ) ) ;
#47943 = CARTESIAN_POINT ( 'NONE',  ( 4.477303810882872881, 0.001702072213635372200, -2.207063162522747479 ) ) ;
#47945 = CARTESIAN_POINT ( 'NONE',  ( -0.6823417656250212460, 5.613541667008087543, 1.181850606188767472 ) ) ;
#47946 = CARTESIAN_POINT ( 'NONE',  ( 2.225118093709726352, -1.884898904786440177, -0.8381453960227978062 ) ) ;
#47947 = CARTESIAN_POINT ( 'NONE',  ( 6.636879889089462026, 7.701780277814560982, -1.199719254218446718 ) ) ;
#47948 = CARTESIAN_POINT ( 'NONE',  ( -9.365985188942097750, 9.821404230054264772, 0.7998128361456462443 ) ) ;
#47949 =( NAMED_UNIT ( * ) SI_UNIT ( $, .STERADIAN. ) SOLID_ANGLE_UNIT ( ) );
#47950 = CARTESIAN_POINT ( 'NONE',  ( 10.37606763316019531, 10.99983374830873650, 0.7998128361456462443 ) ) ;
#47951 = CARTESIAN_POINT ( 'NONE',  ( -3.427975237612759241, -0.01905636783647302046, -0.4136213213207836636 ) ) ;
#47952 = CARTESIAN_POINT ( 'NONE',  ( 6.535912570239620578, 9.782925877658371405, 1.199719254218452047 ) ) ;
#47953 = ORIENTED_EDGE ( 'NONE', *, *, #71672, .T. ) ;
#47954 = CARTESIAN_POINT ( 'NONE',  ( 4.650872726564402981, -0.4503784926754761386, -2.020631409805350387 ) ) ;
#47955 = CARTESIAN_POINT ( 'NONE',  ( 0.7499999999999920064, 5.733333333333353821, 1.299038105676669330 ) ) ;
#47956 = CARTESIAN_POINT ( 'NONE',  ( 1.124558466181435179, 1.288545020775376804, -1.735378439385642180 ) ) ;
#47957 = CARTESIAN_POINT ( 'NONE',  ( -5.163927922758308142, 7.774463771048841565, -1.174891720174384480 ) ) ;
#47958 = CARTESIAN_POINT ( 'NONE',  ( 2.402995385916364857, -0.3474029756719719808, -1.989407454614970261 ) ) ;
#47959 = VERTEX_POINT ( 'NONE', #163863 ) ;
#47960 = ORIENTED_EDGE ( 'NONE', *, *, #69586, .F. ) ;
#47962 = CARTESIAN_POINT ( 'NONE',  ( 8.595506201384020883, 9.130438111143927671, 0.7216878364870438212 ) ) ;
#47961 = CARTESIAN_POINT ( 'NONE',  ( 1.737499999999999378, -2.566666666666668650, -3.009438278150925683 ) ) ;
#47963 = CARTESIAN_POINT ( 'NONE',  ( 0.06005734137062448269, 14.50235776792163023, 11.99783618803943064 ) ) ;
#47964 = CARTESIAN_POINT ( 'NONE',  ( -4.624739795592943459, 6.488892076315448065, -1.443375672974066548 ) ) ;
#47965 = CARTESIAN_POINT ( 'NONE',  ( 0.2863426850727782136, -0.6839425765656822476, -1.897108587135355684 ) ) ;
#47966 = CARTESIAN_POINT ( 'NONE',  ( 5.196902890030515643, 1.791362914573800369, 1.262263373074036688 ) ) ;
#47967 = CARTESIAN_POINT ( 'NONE',  ( -1.500000000000011324, 4.660416667349484676, -0.8660254037844313801 ) ) ;
#47968 = CARTESIAN_POINT ( 'NONE',  ( 5.133030909251353968, 1.769313487831367437, 0.7262901588861517821 ) ) ;
#47969 = CARTESIAN_POINT ( 'NONE',  ( -4.711622075948912247, 5.455646162483875017, -1.199719254218446718 ) ) ;
#47970 = CARTESIAN_POINT ( 'NONE',  ( 4.785665035499516051, 8.527100274817353665, -0.7216878364870207285 ) ) ;
#47972 = CARTESIAN_POINT ( 'NONE',  ( 2.126577575561945821, 0.4445254776237593242, 1.966640697269490312 ) ) ;
#47971 = CARTESIAN_POINT ( 'NONE',  ( -11.89942855770813956, 9.719999999999998863, -0.7000000000000009548 ) ) ;
#47973 = CARTESIAN_POINT ( 'NONE',  ( -1.364683531250014514, 12.40104166700806054, -0.7879004041258335089 ) ) ;
#47975 = CARTESIAN_POINT ( 'NONE',  ( -5.679940009482361774, 5.591294530676332641, 0.7998128361456281477 ) ) ;
#47974 = CARTESIAN_POINT ( 'NONE',  ( 0.7500711518760843077, 2.289381476473162369, -0.1197363719210968458 ) ) ;
#47976 = CARTESIAN_POINT ( 'NONE',  ( 4.524228514566789983, 1.059873738895898310, -1.360581713153318884 ) ) ;
#47977 = CARTESIAN_POINT ( 'NONE',  ( -0.1399997263889836974, 2.022132088033218533, -2.415689637818136948 ) ) ;
#47978 = CARTESIAN_POINT ( 'NONE',  ( 4.844340958784499662, 4.546152628203684820, 0.7998128361456341429 ) ) ;
#47979 = CARTESIAN_POINT ( 'NONE',  ( 0.1399997263886003374, 0.002789056014650820314, -1.999853399661279063 ) ) ;
#47980 =( BOUNDED_CURVE ( )  B_SPLINE_CURVE ( 3, ( #160124, #78856, #190476, #27990 ),
 .UNSPECIFIED., .F., .T. ) 
 B_SPLINE_CURVE_WITH_KNOTS ( ( 4, 4 ),
 ( 3.705870088530767159, 4.712388980384695003 ),
 .UNSPECIFIED. ) 
 CURVE ( )  GEOMETRIC_REPRESENTATION_ITEM ( )  RATIONAL_B_SPLINE_CURVE ( ( 1.000000000000000000, 0.9173434942194453878, 0.9173434942194453878, 1.000000000000000000 ) ) 
 REPRESENTATION_ITEM ( '' )  );
#47981 = ORIENTED_EDGE ( 'NONE', *, *, #69925, .F. ) ;
#47982 = CARTESIAN_POINT ( 'NONE',  ( 0.4794554595633391259, -0.1051018081165492196, 2.067734805981166435 ) ) ;
#47983 = VERTEX_POINT ( 'NONE', #213629 ) ;
#47984 = CARTESIAN_POINT ( 'NONE',  ( 5.426340414154960712, -0.8198882401838718526, -1.615393417293700784 ) ) ;
#47985 = EDGE_LOOP ( 'NONE', ( #116901, #64046, #50117, #65842 ) ) ;
#47986 = CARTESIAN_POINT ( 'NONE',  ( 4.420840606507738357, 7.315341919971147355, 1.199719254218451159 ) ) ;
#47987 = FACE_OUTER_BOUND ( 'NONE', #203360, .T. ) ;
#47988 = CARTESIAN_POINT ( 'NONE',  ( 5.883446949022190786, 0.1262479900229801499, -1.807133042791621458 ) ) ;
#47989 = CARTESIAN_POINT ( 'NONE',  ( 5.953438849732186178, 8.999410187112612647, -1.082531754730548412 ) ) ;
#47990 = CIRCLE ( 'NONE', #148307, 0.09999999999999982514 ) ;
#47991 = CYLINDRICAL_SURFACE ( 'NONE', #34932, 0.08000000000000004330 ) ;
#47992 = CARTESIAN_POINT ( 'NONE',  ( 2.941561714372803227, 0.7881326131919093037, -2.044999658057600644 ) ) ;
#47994 = CARTESIAN_POINT ( 'NONE',  ( 8.809047120577066181, 11.30030761213851953, 1.599625672291281386 ) ) ;
#47993 = CARTESIAN_POINT ( 'NONE',  ( 5.775803124993572624, -1.815561990025884143, 0.4082129570420859888 ) ) ;
#47995 = CARTESIAN_POINT ( 'NONE',  ( 3.532743792504475788, -1.564076696776861120, 1.105682177958314583 ) ) ;
#47996 = PLANE ( 'NONE',  #8444 ) ;
#47997 = CARTESIAN_POINT ( 'NONE',  ( -0.6823417656250246877, 0.3010416670080895418, 1.181850606188755259 ) ) ;
#47998 = CARTESIAN_POINT ( 'NONE',  ( 5.992340707560163793, 6.093411701682730275, 0.7216878364870317197 ) ) ;
#47999 = CARTESIAN_POINT ( 'NONE',  ( -9.490344339885977476, 11.13478515369756217, -1.082531754730539753 ) ) ;
#48000 = CARTESIAN_POINT ( 'NONE',  ( 2.430746436576446179, 2.096607243605509208, 0.5259719050795114148 ) ) ;
#48001 = CARTESIAN_POINT ( 'NONE',  ( -4.936050443827081580, 7.916420063510339666, 1.199719254218452935 ) ) ;
#48002 = CARTESIAN_POINT ( 'NONE',  ( 5.578253857379852576, 5.472660686556754861, -0.7998128361456481317 ) ) ;
#48003 = CARTESIAN_POINT ( 'NONE',  ( 2.080808903162992607, -0.08653491207171599975, -1.823647505904809174 ) ) ;
#48004 = CARTESIAN_POINT ( 'NONE',  ( -3.079673448598517549, 6.744702790006905424, 1.040834085586084257E-14 ) ) ;
#48005 = CARTESIAN_POINT ( 'NONE',  ( 3.891465932158610030, 1.322013910284997262, 1.259209046625270556 ) ) ;
#48006 = CARTESIAN_POINT ( 'NONE',  ( 9.936380849164404339, 11.28055779531969272, 8.367445120465268005 ) ) ;
#48007 = CARTESIAN_POINT ( 'NONE',  ( 2.812653035604309348, -0.5591599321941118639, -1.828790038765286452 ) ) ;
#48008 = VERTEX_POINT ( 'NONE', #96747 ) ;
#48009 = CARTESIAN_POINT ( 'NONE',  ( 3.877371502699510142, -0.1471681016796568819, 1.964127982587125398 ) ) ;
#48010 = ORIENTED_EDGE ( 'NONE', *, *, #203843, .F. ) ;
#48011 = CARTESIAN_POINT ( 'NONE',  ( 5.372584366608633921, -0.05174306282297027465, -1.941541108160367513 ) ) ;
#48012 = ORIENTED_EDGE ( 'NONE', *, *, #76439, .F. ) ;
#48013 = CARTESIAN_POINT ( 'NONE',  ( -5.088052786878465739, 9.158088361325352977, 0.000000000000000000 ) ) ;
#48015 = CARTESIAN_POINT ( 'NONE',  ( 5.115537534566190203, 1.735013203181461350, 1.219038288318145646 ) ) ;
#48014 = CARTESIAN_POINT ( 'NONE',  ( 6.424584688029230328, 8.588711117491191871, 1.599625672291268286 ) ) ;
#48017 = ADVANCED_FACE ( 'NONE', ( #77254 ), #128637, .T. ) ;
#48016 = CARTESIAN_POINT ( 'NONE',  ( -0.07933194018405020920, -7.215568602689852007, 9.499668754397001535 ) ) ;
#48018 = CARTESIAN_POINT ( 'NONE',  ( 2.912652942483742180, -0.5572119909246497915, -1.829279355302193544 ) ) ;
#48019 = CARTESIAN_POINT ( 'NONE',  ( 5.603691946294323323, 6.350013490765915591, -1.172630952486140243 ) ) ;
#48020 = DIRECTION ( 'NONE',  ( -5.329070518200751394E-15, 0.000000000000000000, 1.000000000000000000 ) ) ;
#48021 = VERTEX_POINT ( 'NONE', #61012 ) ;
#48022 = CARTESIAN_POINT ( 'NONE',  ( 4.390861645979372341, 6.216034235099629157, -1.599625672291269396 ) ) ;
#48023 = CARTESIAN_POINT ( 'NONE',  ( 3.826817946245956392, 1.422007987377239546, -1.425180056034919041 ) ) ;
#48024 = CARTESIAN_POINT ( 'NONE',  ( -11.89835103415199313, 11.32893085832464308, 1.561208891256346876 ) ) ;
#48025 = CARTESIAN_POINT ( 'NONE',  ( 5.496661139185262002, -0.4475443406098400523, -1.769863040007889410 ) ) ;
#48026 = CARTESIAN_POINT ( 'NONE',  ( 1.135311898753359472, -0.04898221611688948623, -2.069941200615910581 ) ) ;
#48027 = CARTESIAN_POINT ( 'NONE',  ( -7.754900677336769022, 9.110100880723427608, 1.082531754730558626 ) ) ;
#48028 =( BOUNDED_CURVE ( )  B_SPLINE_CURVE ( 2, ( #61660, #46488, #12887, #10757, #28091 ),
 .UNSPECIFIED., .F., .T. ) 
 B_SPLINE_CURVE_WITH_KNOTS ( ( 3, 2, 3 ),
 ( 0.2236210349743807946, 0.2250000000000000056, 0.2267133053327668735 ),
 .UNSPECIFIED. ) 
 CURVE ( )  GEOMETRIC_REPRESENTATION_ITEM ( )  RATIONAL_B_SPLINE_CURVE ( ( 0.9629979416702594275, 0.9778304460996741776, 1.000000000000000000, 0.9724552731818310036, 0.9562367529269841793 ) ) 
 REPRESENTATION_ITEM ( '' )  );
#48029 = AXIS2_PLACEMENT_3D ( 'NONE', #163124, #27777, #178312 ) ;
#48030 = CARTESIAN_POINT ( 'NONE',  ( -5.987767821832088444, 7.191367801968548079, 1.216456708157914512 ) ) ;
#48031 = CARTESIAN_POINT ( 'NONE',  ( -1.347971487989957070E-14, -3.018749999044084475, 3.475000000000000089 ) ) ;
#48032 = CARTESIAN_POINT ( 'NONE',  ( 5.576977133510579776, -0.04717937999037385977, -1.870219006134994588 ) ) ;
#48033 = CARTESIAN_POINT ( 'NONE',  ( 5.991813822235618758, 9.077867661661846554, 1.199719254218462483 ) ) ;
#48034 = CARTESIAN_POINT ( 'NONE',  ( 2.896029359114099755, 6.600727695600251188, 0.2594116555042840777 ) ) ;
#48035 = CARTESIAN_POINT ( 'NONE',  ( 3.541704441667858472, 5.155074486744371853, -1.599625672291262513 ) ) ;
#48036 = CARTESIAN_POINT ( 'NONE',  ( -1.364683531250000748, 9.921875000341398021, 0.000000000000000000 ) ) ;
#48037 = CARTESIAN_POINT ( 'NONE',  ( -4.466521540698216164, 7.298359999868178960, -1.199719254218452047 ) ) ;
#48039 = CARTESIAN_POINT ( 'NONE',  ( -7.930593509350902792, 8.217056947189661287, -0.7998128361456362523 ) ) ;
#48038 = CARTESIAN_POINT ( 'NONE',  ( 7.257245574617835260, -6.363025497629767990, -6.640718169119574910 ) ) ;
#48040 = CARTESIAN_POINT ( 'NONE',  ( -4.554649539187067830, 7.401175998105142817, 1.199719254218464037 ) ) ;
#48041 = AXIS2_PLACEMENT_3D ( 'NONE', #169645, #203190, #199995 ) ;
#48042 = CARTESIAN_POINT ( 'NONE',  ( 0.8837443060279138729, -1.967007789996034095, 0.6459356165888497925 ) ) ;
#48043 = ADVANCED_FACE ( 'NONE', ( #127170 ), #203551, .T. ) ;
#48044 = CARTESIAN_POINT ( 'NONE',  ( 1.898220681748989280, -1.001352587523595128, -1.865485677531570685 ) ) ;
#48045 = CARTESIAN_POINT ( 'NONE',  ( 7.892817981449907982, 12.36003807833360391, 0.7998128361456462443 ) ) ;
#48046 = CARTESIAN_POINT ( 'NONE',  ( -1.500000000000043299, 3.452083334016150751, 0.8660254037844216102 ) ) ;
#48047 = CARTESIAN_POINT ( 'NONE',  ( 0.2390023523631857882, -0.1431304410692470219, -1.937466148627289719 ) ) ;
#48048 = CARTESIAN_POINT ( 'NONE',  ( 4.314144046604536875, 7.442532859859907646, 1.092782195075291396 ) ) ;
#48049 = CARTESIAN_POINT ( 'NONE',  ( 5.016153647376205171, 6.875265226737464985, 1.443375672974062551 ) ) ;
#48051 = PLANE ( 'NONE',  #188096 ) ;
#48050 = CARTESIAN_POINT ( 'NONE',  ( -1.737499999999997824, -3.441666666666665986, 3.009438278150925683 ) ) ;
#48052 = CARTESIAN_POINT ( 'NONE',  ( 2.379227630831231011, 2.094957926495308875, -0.9307781363587577239 ) ) ;
#48053 = CARTESIAN_POINT ( 'NONE',  ( 0.8557438351849017133, 1.823752217391808150, -0.08689656109241165882 ) ) ;
#48054 = CARTESIAN_POINT ( 'NONE',  ( 2.584119536544440265, 1.026460374567798484, 1.613398670029235538 ) ) ;
#48055 = ORIENTED_EDGE ( 'NONE', *, *, #83136, .F. ) ;
#48056 = CARTESIAN_POINT ( 'NONE',  ( 6.426201622753093368, 10.44105962661321563, 1.040834085586084257E-14 ) ) ;
#48057 = CARTESIAN_POINT ( 'NONE',  ( 1.336190909427417139, -1.121870850062630653, -1.671457199112064806 ) ) ;
#48058 = CARTESIAN_POINT ( 'NONE',  ( 0.9714493606215730548, -0.2934177832072166758, 1.939591667560663035 ) ) ;
#48059 = CARTESIAN_POINT ( 'NONE',  ( -8.727698198895085469, 11.20540053684285553, -1.599625672291263179 ) ) ;
#48060 = CARTESIAN_POINT ( 'NONE',  ( -6.340409392685171674, 10.54889472477470846, 0.7998128361456481317 ) ) ;
#48061 = CARTESIAN_POINT ( 'NONE',  ( -10.94892327452127034, 5.391491584528539605, 4.806427459653232148 ) ) ;
#48064 = B_SPLINE_CURVE_WITH_KNOTS ( 'NONE', 3,
 ( #139223, #204169, #74221, #191145 ),
 .UNSPECIFIED., .F., .F.,
 ( 4, 4 ),
 ( 0.000000000000000000, 7.241384396099075972E-05 ),
 .UNSPECIFIED. ) ;
#48063 = CARTESIAN_POINT ( 'NONE',  ( 2.043481384864866524, 0.6806142739823103360, -1.633949198972502570 ) ) ;
#48062 = CARTESIAN_POINT ( 'NONE',  ( 3.363305035154311007, 2.039577031997115597, -0.4584567826917042010 ) ) ;
#48065 = CARTESIAN_POINT ( 'NONE',  ( -10.85277107007939001, 3.956598013261175772, 3.932872935640539414 ) ) ;
#48067 = CARTESIAN_POINT ( 'NONE',  ( 5.560555354427807906, -2.070165260436385601, -0.9845844755148360772 ) ) ;
#48066 = CARTESIAN_POINT ( 'NONE',  ( -11.01500063815905328, 5.353715452092881577, 4.767907905931622281 ) ) ;
#48068 = CARTESIAN_POINT ( 'NONE',  ( 4.277133665768851678, 1.139379310349198260, 1.315593229251702523 ) ) ;
#48069 = CARTESIAN_POINT ( 'NONE',  ( 10.05067194643221207, 10.62020544712608938, 0.7998128361456462443 ) ) ;
#48070 = CARTESIAN_POINT ( 'NONE',  ( -0.1104750535120248289, 7.629137130509052511, -2.703481013110929254 ) ) ;
#48071 = CARTESIAN_POINT ( 'NONE',  ( 4.270605845326081784, -1.729236537505800086, 0.1267691526786636214 ) ) ;
#48072 = CARTESIAN_POINT ( 'NONE',  ( 4.299414767360295819, -1.890980460948383790, 1.066717558251949471 ) ) ;
#48073 = CARTESIAN_POINT ( 'NONE',  ( 3.551346171775753735, 6.230655402791975384, 1.199719254218462483 ) ) ;
#48074 = CARTESIAN_POINT ( 'NONE',  ( 6.192592252150040721, 1.490973663936447258, -1.357864438797616868 ) ) ;
#48075 = CARTESIAN_POINT ( 'NONE',  ( 0.8125000000000005551, 1.451031289061154306, 1.451031289061088136 ) ) ;
#48076 = CARTESIAN_POINT ( 'NONE',  ( 0.7499999999999902300, 4.847916667349482012, -1.299038105676658228 ) ) ;
#48077 = CARTESIAN_POINT ( 'NONE',  ( 3.188414472400236566, -1.897621675979482614, -0.3308535721826404985 ) ) ;
#48078 = CARTESIAN_POINT ( 'NONE',  ( 0.7500000000000006661, 9.697916667349467446, -1.299038105676657340 ) ) ;
#48079 = CARTESIAN_POINT ( 'NONE',  ( 5.765950734523942245, 0.6451602502356535984, -2.125694943049365904 ) ) ;
#48080 = VERTEX_POINT ( 'NONE', #63149 ) ;
#48081 = CARTESIAN_POINT ( 'NONE',  ( 6.883263157960402445, -0.003972766660574957552, 2.046037087719229319 ) ) ;
#48082 = CARTESIAN_POINT ( 'NONE',  ( 1.499999999999987121, 3.545833333333356041, -0.8660254037844262731 ) ) ;
#48083 = CARTESIAN_POINT ( 'NONE',  ( 5.769158057814842699, 6.689438141327490150, 1.199719254218462483 ) ) ;
#48084 = CARTESIAN_POINT ( 'NONE',  ( 1.436510670779034937, -1.237796341723711002, -1.844280071174006164 ) ) ;
#48085 = CARTESIAN_POINT ( 'NONE',  ( -0.9311234436981514762, -1.078119629485602804, -3.474999999999999645 ) ) ;
#48086 = CARTESIAN_POINT ( 'NONE',  ( 8.459924665247367415, 8.972259652317825740, -0.7216878364870267237 ) ) ;
#48087 = AXIS2_PLACEMENT_3D ( 'NONE', #153132, #9008, #136893 ) ;
#48088 = CARTESIAN_POINT ( 'NONE',  ( -8.459924664802993988, 12.81373650900478189, 1.040834085586084257E-14 ) ) ;
#48089 = CARTESIAN_POINT ( 'NONE',  ( 5.063044020060520900, 4.871582543017558109, 0.7998128361456352531 ) ) ;
#48090 = CARTESIAN_POINT ( 'NONE',  ( -4.258669648468323743, 6.061810238003387141, 1.443375672974065660 ) ) ;
#48092 = CARTESIAN_POINT ( 'NONE',  ( 4.562968466866096584, 1.596587869669671145, -1.305994239470360974 ) ) ;
#48091 = DIRECTION ( 'NONE',  ( 1.000000000000000000, -0.000000000000000000, -0.000000000000000000 ) ) ;
#48093 = CARTESIAN_POINT ( 'NONE',  ( -3.632695093457760649, 6.325562478087638496, -1.199719254218452047 ) ) ;
#48094 = CARTESIAN_POINT ( 'NONE',  ( -1.499999999999997780, 4.681250000682819490, 1.214306433183764966E-14 ) ) ;
#48095 = CARTESIAN_POINT ( 'NONE',  ( 0.6823417656249882723, -0.4072916663252490466, 1.181850606188755259 ) ) ;
#48096 = CARTESIAN_POINT ( 'NONE',  ( 6.503191328365395485, 1.555263205862934983, 1.038959965768880389 ) ) ;
#48097 = CARTESIAN_POINT ( 'NONE',  ( 5.326719796100753967, 0.6952390240965979906, -1.588890972402807966 ) ) ;
#48098 = CARTESIAN_POINT ( 'NONE',  ( 4.686888010602763721, 1.293897920562389947, 1.164242640570410714 ) ) ;
#48099 = CARTESIAN_POINT ( 'NONE',  ( 3.928111819657337911, 5.605883094398769195, 1.599625672291267398 ) ) ;
#48100 = CARTESIAN_POINT ( 'NONE',  ( 2.824086921994493071, 1.271197760638997254, -1.907441589200240983 ) ) ;
#48101 = CARTESIAN_POINT ( 'NONE',  ( 0.6823417656249917140, 4.905208333674755394, 1.181850606188765695 ) ) ;
#48102 = CARTESIAN_POINT ( 'NONE',  ( 1.007454599746326895, -0.8259622865525710900, -1.645551850779983116 ) ) ;
#48103 = LINE ( 'NONE', #114215, #18947 ) ;
#48104 = CARTESIAN_POINT ( 'NONE',  ( 1.588595499965880675, -0.2641367610144580991, -1.806243275932853498 ) ) ;
#48105 = CARTESIAN_POINT ( 'NONE',  ( 3.199842427594956185, 1.824118962040650604, 0.8596310190432245868 ) ) ;
#48106 = CARTESIAN_POINT ( 'NONE',  ( 0.8674257402763450031, 2.111068143204323455, -0.5878430487569612506 ) ) ;
#48107 = CARTESIAN_POINT ( 'NONE',  ( 9.243053468019274632, 13.75123835987339760, -6.856199898420598515 ) ) ;
#48108 = CARTESIAN_POINT ( 'NONE',  ( 4.085071245346539648, -0.2040513417298230325, -2.096037468315871788 ) ) ;
#48109 = CARTESIAN_POINT ( 'NONE',  ( -5.554036483092550824, 9.631459663583308739, -0.7998128361456231517 ) ) ;
#48110 = CARTESIAN_POINT ( 'NONE',  ( 8.651451850166534285, 13.72329050238413117, 9.384217411227872674 ) ) ;
#48111 = CARTESIAN_POINT ( 'NONE',  ( 1.697802635435996743, -1.498143435978617877, -1.429203828351800487 ) ) ;
#48112 = CARTESIAN_POINT ( 'NONE',  ( 5.867981556616276073, 5.740399992340775803, -0.7998128361456281477 ) ) ;
#48113 = CARTESIAN_POINT ( 'NONE',  ( 1.360316468749992236, 2.765625000341414896, -4.683753385137379155E-14 ) ) ;
#48114 = CARTESIAN_POINT ( 'NONE',  ( 3.246849895443252532, 2.069243461727567013, 0.4626693848822636124 ) ) ;
#48115 = CARTESIAN_POINT ( 'NONE',  ( -1.364683531250014514, 0.7385416670080887647, -0.7879004041258289570 ) ) ;
#48116 = CARTESIAN_POINT ( 'NONE',  ( 6.551389018236878137, -1.469694460105780642, -1.082916835497591324 ) ) ;
#48117 = ORIENTED_EDGE ( 'NONE', *, *, #125035, .T. ) ;
#48118 = CARTESIAN_POINT ( 'NONE',  ( -4.847922445338252118, 7.813604065273374921, -1.199719254218453823 ) ) ;
#48119 = CARTESIAN_POINT ( 'NONE',  ( 10.08456733046637765, 10.65975006183261087, 0.000000000000000000 ) ) ;
#48120 = CARTESIAN_POINT ( 'NONE',  ( 6.821160681006788629, 8.091013894996997635, 1.082531754730549967 ) ) ;
#48121 = CARTESIAN_POINT ( 'NONE',  ( -3.475000000000000533, -2.435416665710753215, -2.006292185433948827 ) ) ;
#48122 = CARTESIAN_POINT ( 'NONE',  ( -6.205881626753225966, 8.263281202677319470, 1.599625672291283607 ) ) ;
#48123 = CARTESIAN_POINT ( 'NONE',  ( 3.269790213696788683, 0.4867576797993823368, -1.960144559866239700 ) ) ;
#48124 = CARTESIAN_POINT ( 'NONE',  ( 0.8683613728089655259, 1.037855563948440363, 1.832367646046024534 ) ) ;
#48125 = CARTESIAN_POINT ( 'NONE',  ( -5.607179047703544583, 8.699403434699558346, 1.199719254218454489 ) ) ;
#48126 = CARTESIAN_POINT ( 'NONE',  ( 8.402302512167096893, 10.82577223566020841, -1.599625672291268286 ) ) ;
#48127 = CARTESIAN_POINT ( 'NONE',  ( 5.700015841690603935, 0.7557596558054953118, -1.700775360669419145 ) ) ;
#48128 = CARTESIAN_POINT ( 'NONE',  ( 8.426556166093362776, 9.789735934319136135, -1.199719254218446718 ) ) ;
#48129 = CARTESIAN_POINT ( 'NONE',  ( 0.4288785890452541105, 3.049942316455306113, 0.4196807566830256797 ) ) ;
#48130 = CARTESIAN_POINT ( 'NONE',  ( -10.00555417720528872, 10.77549408293541866, 0.7216878364870438212 ) ) ;
#48131 = CARTESIAN_POINT ( 'NONE',  ( -7.531718027591449705, 8.745758106066849891, 1.199719254218462483 ) ) ;
#48132 = CARTESIAN_POINT ( 'NONE',  ( 6.666874348205719336, -1.883165374045802087, -0.8376701409097894180 ) ) ;
#48134 = CARTESIAN_POINT ( 'NONE',  ( -4.313069242314466756, 7.435226253386592710, 1.131090909019900614 ) ) ;
#48133 = CARTESIAN_POINT ( 'NONE',  ( -4.586401103172829785, 8.572828063668767484, 0.7998128361456281477 ) ) ;
#48135 = CARTESIAN_POINT ( 'NONE',  ( -0.6823417656250246877, 0.3010416670080895418, 1.181850606188755259 ) ) ;
#48136 = CARTESIAN_POINT ( 'NONE',  ( 2.670900524536640841, -0.6599870735717223713, -1.603529595030905641 ) ) ;
#48137 = CARTESIAN_POINT ( 'NONE',  ( 0.9369944060461411484, 0.7087284392868421490, -1.589666227069729265 ) ) ;
#48138 = AXIS2_PLACEMENT_3D ( 'NONE', #119440, #185427, #37046 ) ;
#48140 = CARTESIAN_POINT ( 'NONE',  ( 8.297226821883377568, 8.782445501726501291, -0.7216878364870267237 ) ) ;
#48139 = CARTESIAN_POINT ( 'NONE',  ( 6.340458270854060885, 2.281561288062480486, 0.3456012654466412704 ) ) ;
#48141 = CARTESIAN_POINT ( 'NONE',  ( -12.40260256363088942, 6.580881934270854217, 3.466095386915876819 ) ) ;
#48142 = CARTESIAN_POINT ( 'NONE',  ( 2.266935757080061897, -1.882882732336080167, -0.8380483592859179209 ) ) ;
#48143 = ADVANCED_FACE ( 'NONE', ( #195289, #46921 ), #114111, .T. ) ;
#48144 = CARTESIAN_POINT ( 'NONE',  ( 1.036482258494644038, 1.943774389176852857, -0.5350038931242264706 ) ) ;
#48145 = CARTESIAN_POINT ( 'NONE',  ( 6.925078400183531713, 7.629137130509035636, 2.644348168701659674 ) ) ;
#48146 = CARTESIAN_POINT ( 'NONE',  ( -5.367048706163331850, 7.354919138647580290, -1.599625672291271394 ) ) ;
#48147 = CARTESIAN_POINT ( 'NONE',  ( 0.6902270635062581761, -1.956280663680696197, -0.2437950987402882630 ) ) ;
#48149 = CARTESIAN_POINT ( 'NONE',  ( -7.756673280794142755, 8.222076047114187602, -0.7216878364870338292 ) ) ;
#48148 = CARTESIAN_POINT ( 'NONE',  ( 4.254103502353132171, 0.8128351696983120434, -1.731171583500931366 ) ) ;
#48150 = CARTESIAN_POINT ( 'NONE',  ( 5.777994779145079640, 1.311685685134782231, 1.774619457157788904 ) ) ;
#48151 = CARTESIAN_POINT ( 'NONE',  ( -5.085717018457573957, 8.947437264926888290, 0.7216878364870267237 ) ) ;
#48152 = CARTESIAN_POINT ( 'NONE',  ( 7.700104897918568447, 7.948153567185284096, 0.000000000000000000 ) ) ;
#48153 = ADVANCED_FACE ( 'NONE', ( #212583 ), #169962, .T. ) ;
#48154 = CARTESIAN_POINT ( 'NONE',  ( -6.933015448541747006, 9.181880338089085214, 1.599625672291269396 ) ) ;
#48155 = CARTESIAN_POINT ( 'NONE',  ( 0.5221358870723510348, -2.009748826802790322, 0.2000887155638417791 ) ) ;
#48156 = DIRECTION ( 'NONE',  ( -0.7071067811865489050, 0.000000000000000000, -0.7071067811865462405 ) ) ;
#48157 = CARTESIAN_POINT ( 'NONE',  ( 4.647712500454345808, -1.780663920513593013, -1.467712336591691313 ) ) ;
#48158 = CARTESIAN_POINT ( 'NONE',  ( 5.424254290899477304, 0.9654600744411747648, 1.707767180430696641 ) ) ;
#48159 = CARTESIAN_POINT ( 'NONE',  ( 1.516376426791886445, 0.7900930292849810410, 1.795789229542772647 ) ) ;
#48160 = CARTESIAN_POINT ( 'NONE',  ( 10.72180055030867329, 11.40318881831530540, 0.7998128361456341429 ) ) ;
#48161 = CARTESIAN_POINT ( 'NONE',  ( -0.1224325501351306023, -0.4448023855274513272, -1.973852191825019364 ) ) ;
#48162 = ORIENTED_EDGE ( 'NONE', *, *, #179732, .T. ) ;
#48163 = CARTESIAN_POINT ( 'NONE',  ( 6.350795928397162449, -1.845624747684541989, -0.8128223418941012968 ) ) ;
#48165 = CARTESIAN_POINT ( 'NONE',  ( -6.347188469492005325, 10.55680364771601809, -0.7998128361456291469 ) ) ;
#48164 = CARTESIAN_POINT ( 'NONE',  ( -3.815730167242251003, 6.539103397502874948, -1.199719254218452047 ) ) ;
#48166 = CARTESIAN_POINT ( 'NONE',  ( 0.7261896124251127072, 0.1329856088156805560, 1.836402230816103209 ) ) ;
#48167 = ORIENTED_EDGE ( 'NONE', *, *, #145607, .F. ) ;
#48168 = CARTESIAN_POINT ( 'NONE',  ( 3.801787986034934619, -1.640574847700679628, -1.422045332411596474 ) ) ;
#48169 = CARTESIAN_POINT ( 'NONE',  ( 11.99956672297294880, 7.640688894226271621, 0.4526725690500942312 ) ) ;
#48170 = CARTESIAN_POINT ( 'NONE',  ( 1.529697670087664108, -0.2543295609688834835, 2.105205558366497698 ) ) ;
#48171 = CARTESIAN_POINT ( 'NONE',  ( -1.500000000000013101, 3.160416667349486008, -0.8660254037844313801 ) ) ;
#48172 = CARTESIAN_POINT ( 'NONE',  ( 8.914649696185335870, 10.35917838609310593, -1.199719254218446718 ) ) ;
#48173 = CARTESIAN_POINT ( 'NONE',  ( -1.840093022230759878, 2.503055443996555329, -2.494806138668435036 ) ) ;
#48174 = CARTESIAN_POINT ( 'NONE',  ( 2.970052003254409545, 1.099468894914462647, 1.742775920482849905 ) ) ;
#48176 = CARTESIAN_POINT ( 'NONE',  ( 0.04610459085982108324, -1.479553692838073475, 1.095721268101347734 ) ) ;
#48175 = CARTESIAN_POINT ( 'NONE',  ( -8.690940161559884913, 10.09818392903003748, 1.199719254218462483 ) ) ;
#48177 = CARTESIAN_POINT ( 'NONE',  ( -0.6823417656250212460, 3.301041667008085323, 1.181850606188767472 ) ) ;
#48178 = DIRECTION ( 'NONE',  ( -0.000000000000000000, -1.000000000000000000, -0.000000000000000000 ) ) ;
#48179 = CARTESIAN_POINT ( 'NONE',  ( 1.315333408008315441, 4.153791529306043451, 0.4024190470832924582 ) ) ;
#48180 =( GEOMETRIC_REPRESENTATION_CONTEXT ( 3 ) GLOBAL_UNCERTAINTY_ASSIGNED_CONTEXT ( ( #167689 ) ) GLOBAL_UNIT_ASSIGNED_CONTEXT ( ( #213440, #161538, #179911 ) ) REPRESENTATION_CONTEXT ( 'NONE', 'WORKASPACE' ) );
#48181 = CARTESIAN_POINT ( 'NONE',  ( 0.2412292383832773390, 0.3817025157030576321, 2.173470055567463088 ) ) ;
#48182 = CARTESIAN_POINT ( 'NONE',  ( 1.529016648559086811, 2.180303969971490563, 0.6036265194416541302 ) ) ;
#48183 = CARTESIAN_POINT ( 'NONE',  ( -9.653042183249972652, 10.36423008998754192, -0.7216878364870267237 ) ) ;
#48185 = EDGE_CURVE ( 'NONE', #144530, #160528, #155801, .T. ) ;
#48184 = CARTESIAN_POINT ( 'NONE',  ( 1.529274006537587161, -0.2194501901080987971, 1.798134050542072870 ) ) ;
#48186 = CARTESIAN_POINT ( 'NONE',  ( 2.360426208626884570, -1.834515764125169257, -0.5519355525325749801 ) ) ;
#48187 = CARTESIAN_POINT ( 'NONE',  ( 2.699741690289765295, -1.532448122638006671, -1.392287113214360827 ) ) ;
#48188 = CARTESIAN_POINT ( 'NONE',  ( 0.6823417656249882723, 1.738541667008083991, -1.181850606188749264 ) ) ;
#48189 = CARTESIAN_POINT ( 'NONE',  ( 1.252734725572089536, -1.555569235904795011, 1.211063379650168415 ) ) ;
#48190 = CARTESIAN_POINT ( 'NONE',  ( 5.813098442667213206, 1.700071987003290763, 0.9061822306820240813 ) ) ;
#48192 = CARTESIAN_POINT ( 'NONE',  ( 6.348694402744908594, 6.841026321354189754, -0.6301123915167846645 ) ) ;
#48191 = CARTESIAN_POINT ( 'NONE',  ( 1.366329765314050482, 2.272867617333930390, -0.3986118548820920537 ) ) ;
#48193 = CARTESIAN_POINT ( 'NONE',  ( 1.364683531249986537, 2.655208333674754062, -0.7879004041258239610 ) ) ;
#48194 = CARTESIAN_POINT ( 'NONE',  ( 5.336407798562197158, -1.148744492729685707, 1.713005319730724008 ) ) ;
#48195 = CARTESIAN_POINT ( 'NONE',  ( -5.599681137644054729, 6.491715067794862293, 1.199719254218450271 ) ) ;
#48196 = CARTESIAN_POINT ( 'NONE',  ( -1.445243771768972785, 3.563465185575238614, -0.4166150551214558573 ) ) ;
#48197 = CARTESIAN_POINT ( 'NONE',  ( 6.071333362910682041, 0.1583771919418910934, -2.100070647415654079 ) ) ;
#48198 = EDGE_CURVE ( 'NONE', #192556, #6976, #17801, .T. ) ;
#48199 = CARTESIAN_POINT ( 'NONE',  ( -1.364683531250000748, 2.071875000341422357, 1.214306433183764966E-14 ) ) ;
#48200 = CARTESIAN_POINT ( 'NONE',  ( 5.114612887932482366, 1.494710344919391476, -1.561737693111686642 ) ) ;
#48201 = CARTESIAN_POINT ( 'NONE',  ( 4.986975786537023225, -1.902434985030461156, -0.6785184294546533490 ) ) ;
#48202 = DIRECTION ( 'NONE',  ( 0.000000000000000000, 0.000000000000000000, -1.000000000000000000 ) ) ;
#48203 = CARTESIAN_POINT ( 'NONE',  ( -4.446711195602239819, 8.131654128270509929, -0.7216878364870267237 ) ) ;
#48204 = ADVANCED_FACE ( 'NONE', ( #152927 ), #144181, .T. ) ;
#48207 = CARTESIAN_POINT ( 'NONE',  ( 4.690757960648224589, 6.495636925554817864, 1.443375672974062551 ) ) ;
#48206 = CARTESIAN_POINT ( 'NONE',  ( -1.642778471874998480, -2.151041666188707957, 2.845375778867863303 ) ) ;
#48205 = CARTESIAN_POINT ( 'NONE',  ( -7.788274451701516554, 14.55185945186256724, -9.081450335369259719 ) ) ;
#48208 = CARTESIAN_POINT ( 'NONE',  ( -3.806807270387036368, 7.663301925418665839, 0.000000000000000000 ) ) ;
#48209 = CARTESIAN_POINT ( 'NONE',  ( 3.186732694495420848, 1.586669336078951664, -1.244385354607212335 ) ) ;
#48210 = CARTESIAN_POINT ( 'NONE',  ( -7.069687034522070590, 10.33538640932937724, -1.199719254218440723 ) ) ;
#48212 = CARTESIAN_POINT ( 'NONE',  ( -7.065207446052809814, 9.336104335185325453, -1.443375672974066548 ) ) ;
#48211 = CARTESIAN_POINT ( 'NONE',  ( -10.49364770729726359, 11.34493653470939023, 0.7216878364870438212 ) ) ;
#48213 = CARTESIAN_POINT ( 'NONE',  ( 0.6823417656249899377, 5.676041667008087543, -1.181850606188754593 ) ) ;
#48215 = CARTESIAN_POINT ( 'NONE',  ( -0.6823417656250003738, 8.901041667008065872, 1.181850606188754593 ) ) ;
#48214 = CARTESIAN_POINT ( 'NONE',  ( 5.295850518597075229, -0.7817450549502875656, 2.015575934489414411 ) ) ;
#48216 = CARTESIAN_POINT ( 'NONE',  ( 1.734723475976807094E-15, 0.2401923788623739342, 10.89999999999920810 ) ) ;
#48217 = CARTESIAN_POINT ( 'NONE',  ( -11.95736795583652778, 7.932031143568775811, -1.043616941178784785 ) ) ;
#48219 = CARTESIAN_POINT ( 'NONE',  ( 5.413685477598253470, -1.281375732037979942, -1.556898226837098331 ) ) ;
#48218 = CARTESIAN_POINT ( 'NONE',  ( -6.114364089638801403, 8.156510742710487705, 1.443375672974078761 ) ) ;
#48220 = CARTESIAN_POINT ( 'NONE',  ( -0.6823417656250246877, -1.136458332991911790, 1.181850606188755259 ) ) ;
#48221 = CARTESIAN_POINT ( 'NONE',  ( 1.330204427372463138, 1.661418051098985327, 0.4633224975721556005 ) ) ;
#48222 = CARTESIAN_POINT ( 'NONE',  ( 4.115782150200256950, 6.959440387612411349, 1.199719254218452047 ) ) ;
#48224 = CARTESIAN_POINT ( 'NONE',  ( 7.126746022638799971, 8.343567110280638133, 1.199719254218452047 ) ) ;
#48223 = CARTESIAN_POINT ( 'NONE',  ( 7.809133291791403586, 8.213003049952529722, -0.7216878364870257245 ) ) ;
#48225 = AXIS2_PLACEMENT_3D ( 'NONE', #62012, #44711, #13249 ) ;
#48226 = CARTESIAN_POINT ( 'NONE',  ( -11.32370062957175172, 7.703969811881795415, -3.978908248158274930 ) ) ;
#48227 = CARTESIAN_POINT ( 'NONE',  ( 6.925078400183548588, 0.0006614011395407459748, 1.855452278108092656 ) ) ;
#48228 = CARTESIAN_POINT ( 'NONE',  ( 1.330727748098162078, 1.350296381755649922, -1.493239990923441951 ) ) ;
#48229 = CARTESIAN_POINT ( 'NONE',  ( -0.4170821662629279336, 3.033599471985628959, -0.4170821662629279336 ) ) ;
#48230 = CARTESIAN_POINT ( 'NONE',  ( 3.346891443098894303, 0.5343612633194516626, 2.140983517310310891 ) ) ;
#48231 = CARTESIAN_POINT ( 'NONE',  ( 5.752828983992735346, -0.5200050086436918129, -2.107789999013423454 ) ) ;
#48232 = ORIENTED_EDGE ( 'NONE', *, *, #65201, .F. ) ;
#48234 = CARTESIAN_POINT ( 'NONE',  ( 1.704704067347760699, 1.882482151684254923, 0.7231221989368596947 ) ) ;
#48233 = CARTESIAN_POINT ( 'NONE',  ( 2.033984416766075665, -2.056095976692096094, 0.5180656111221926263 ) ) ;
#48235 = CARTESIAN_POINT ( 'NONE',  ( 1.968756957844201239, -1.398423508019512651, 1.151565528817798834 ) ) ;
#48236 = CARTESIAN_POINT ( 'NONE',  ( 6.363572996767764778, 8.517530811019446091, -1.599625672291283607 ) ) ;
#48237 = EDGE_LOOP ( 'NONE', ( #101022, #137261, #5655, #123710, #153540 ) ) ;
#48238 = VECTOR ( 'NONE', #94832, 1000.000000000000000 ) ;
#48239 = CARTESIAN_POINT ( 'NONE',  ( 5.276094334012385367, 9.307193822989793475, 1.040834085586084257E-14 ) ) ;
#48241 = CARTESIAN_POINT ( 'NONE',  ( 0.07520289192196588646, 1.421326540713454323, 1.284674935297628773 ) ) ;
#48240 = CARTESIAN_POINT ( 'NONE',  ( -4.172158584703340445, 5.890604320285754980, -1.599625672291256295 ) ) ;
#48242 = DIRECTION ( 'NONE',  ( -1.000000000000000000, 0.000000000000000000, 0.000000000000000000 ) ) ;
#48243 = CARTESIAN_POINT ( 'NONE',  ( 9.609441814500813805, -6.583711573986998467, -0.3689019803512830764 ) ) ;
#48244 = CARTESIAN_POINT ( 'NONE',  ( 5.788968402910812827, 6.816513227226497662, 1.082531754730558626 ) ) ;
#48245 = CARTESIAN_POINT ( 'NONE',  ( 1.364683531249988757, 0.4468750003414206917, 0.000000000000000000 ) ) ;
#48246 = CARTESIAN_POINT ( 'NONE',  ( 0.000000000000000000, -0.4330127018922214077, 0.000000000000000000 ) ) ;
#48247 = CARTESIAN_POINT ( 'NONE',  ( -9.321394304595349567, 10.83371376257142416, 1.199719254218462483 ) ) ;
#48248 = CARTESIAN_POINT ( 'NONE',  ( 4.715790015261832835, -2.120648752638915724, 0.4184459369844309440 ) ) ;
#48249 = CARTESIAN_POINT ( 'NONE',  ( -5.885648082108231982, 7.959951743916638733, 1.443375672974058777 ) ) ;
#48250 = CARTESIAN_POINT ( 'NONE',  ( 6.238160076063542725, 6.450477308261824305, -0.7216878364870458196 ) ) ;
#48251 = CARTESIAN_POINT ( 'NONE',  ( 2.144932638433934002, 2.058100890041581810, 0.5106320605416380110 ) ) ;
#48252 = CARTESIAN_POINT ( 'NONE',  ( -0.3282377607281349308, 2.448664549684623104, -1.225000000000029177 ) ) ;
#48253 = CARTESIAN_POINT ( 'NONE',  ( 3.409407428336236556, -0.3879349331968630077, 1.932650128172111126 ) ) ;
#48254 = CARTESIAN_POINT ( 'NONE',  ( 5.256085721135645095, 0.7693902824621422498, -1.750971482026221437 ) ) ;
#48255 = ORIENTED_EDGE ( 'NONE', *, *, #66268, .T. ) ;
#48256 = CARTESIAN_POINT ( 'NONE',  ( 1.499999999999990896, 4.525000000000021672, 1.214306433183764966E-14 ) ) ;
#48257 = CARTESIAN_POINT ( 'NONE',  ( 0.9595327444568906294, 1.691550050060253829, 1.193477315110213599 ) ) ;
#48258 = CARTESIAN_POINT ( 'NONE',  ( 1.570153368812776229, -1.843976851262040029, -0.6092462720258711162 ) ) ;
#48259 = ORIENTED_EDGE ( 'NONE', *, *, #11231, .F. ) ;
#48260 = CYLINDRICAL_SURFACE ( 'NONE', #99114, 1.250000000000000000 ) ;
#48262 = CARTESIAN_POINT ( 'NONE',  ( 6.230854113932139171, 9.427024345299638952, 1.199719254218452047 ) ) ;
#48261 = CARTESIAN_POINT ( 'NONE',  ( -5.587368702607575344, 8.572328348800551723, 1.082531754730550855 ) ) ;
#48264 = CARTESIAN_POINT ( 'NONE',  ( 6.283314124929436417, 9.417951348137970413, -1.199719254218440723 ) ) ;
#48263 = CARTESIAN_POINT ( 'NONE',  ( 2.326223132658828963, 2.028069097222063188, 0.5071170776438630456 ) ) ;
#48267 = EDGE_CURVE ( 'NONE', #98321, #75836, #38556, .T. ) ;
#48266 = CARTESIAN_POINT ( 'NONE',  ( 5.438229012412886476, 7.437962829272074750, -1.443375672974078761 ) ) ;
#48265 = CARTESIAN_POINT ( 'NONE',  ( 6.608709811657416999, 9.797579649320619311, -1.199719254218440723 ) ) ;
#48269 = EDGE_LOOP ( 'NONE', ( #34584, #62627, #52058, #114449, #140160, #198144, #31716, #133505, #160013, #141663, #63975, #91937, #209362 ) ) ;
#48268 = CARTESIAN_POINT ( 'NONE',  ( 6.111958284735683478, -0.6397702040911549259, 1.802229686255519603 ) ) ;
#48270 = CARTESIAN_POINT ( 'NONE',  ( 4.090592613104036879, -2.182713160620152859, -0.3248913242878055385 ) ) ;
#48271 = CARTESIAN_POINT ( 'NONE',  ( 1.729795059504362076, -2.077734391967264838, 0.7439406459070622146 ) ) ;
#48272 = CARTESIAN_POINT ( 'NONE',  ( -11.88156762547254175, 12.22000008454030073, 1.686557021358693342 ) ) ;
#48273 = CARTESIAN_POINT ( 'NONE',  ( 2.121601645288184290, -0.4173985973947492711, 1.866012167355892704 ) ) ;
#48274 = CARTESIAN_POINT ( 'NONE',  ( -10.50000000000000000, 13.40000000000000036, -3.600000000000002309 ) ) ;
#48275 = CARTESIAN_POINT ( 'NONE',  ( 0.000000000000000000, 12.29999999999998295, 0.000000000000000000 ) ) ;
#48276 = CARTESIAN_POINT ( 'NONE',  ( 4.211429588753928144, -1.719575573843845850, -1.152724658989822348 ) ) ;
#48278 = CARTESIAN_POINT ( 'NONE',  ( 2.096749907087645415, -0.5762017740289016032, -2.083436276955972222 ) ) ;
#48277 = CARTESIAN_POINT ( 'NONE',  ( -4.451154503988200339, 4.087435097607984957, 1.214306433183764966E-14 ) ) ;
#48279 = CARTESIAN_POINT ( 'NONE',  ( 3.878626735558046157, -0.2160506499642600997, -2.180900317982924275 ) ) ;
#48280 = DIRECTION ( 'NONE',  ( 1.276756478318932585E-15, -1.000000000000000000, 1.665334536937738262E-16 ) ) ;
#48281 = DIRECTION ( 'NONE',  ( -0.9990890794760040050, 5.454924750823445190E-15, 0.04267330865764876885 ) ) ;
#48282 = CARTESIAN_POINT ( 'NONE',  ( -0.5500358407890207912, 7.827628757559874195, 1.923053904898951005 ) ) ;
#48283 = CARTESIAN_POINT ( 'NONE',  ( 0.6823417656249934904, 14.75520833367473195, 1.181850606188764807 ) ) ;
#48284 = EDGE_CURVE ( 'NONE', #134461, #13120, #99850, .T. ) ;
#48285 = CARTESIAN_POINT ( 'NONE',  ( -5.517242166118370150, 5.401480380085008193, 0.7998128361456281477 ) ) ;
#48286 = CARTESIAN_POINT ( 'NONE',  ( 6.574911468446097196, -0.7340051069854407473, 1.570379515389648040 ) ) ;
#48287 = CARTESIAN_POINT ( 'NONE',  ( -9.164948653157990677, 11.71552606681625619, -1.443375672974059665 ) ) ;
#48288 = CARTESIAN_POINT ( 'NONE',  ( 4.381733404717279790, -1.982624999272282862, 0.5960583376443123749 ) ) ;
#48289 = CARTESIAN_POINT ( 'NONE',  ( 3.070836455255634423, -1.780209531678895729, -0.7368423699729318432 ) ) ;
#48290 = CARTESIAN_POINT ( 'NONE',  ( 5.325823331840044084, 0.8572517883133590200, -1.936080889991494747 ) ) ;
#48291 = CARTESIAN_POINT ( 'NONE',  ( 6.010342169559767633, 5.906487374108181143, -0.7998128361456281477 ) ) ;
#48292 = CARTESIAN_POINT ( 'NONE',  ( -1.201851678989727383E-14, 5.446875000341422357, -1.575800808251660134 ) ) ;
#48293 = CARTESIAN_POINT ( 'NONE',  ( 4.082825143736307005, 1.868653194780546922, 0.6220825103698603975 ) ) ;
#48294 = CARTESIAN_POINT ( 'NONE',  ( 6.492113699461491194, -0.6046859696737926226, -2.211003196133090931 ) ) ;
#48295 = CARTESIAN_POINT ( 'NONE',  ( 3.949673224339702138, 0.6133576713117369072, -1.719707012317383210 ) ) ;
#48296 = EDGE_CURVE ( 'NONE', #194999, #68165, #66195, .T. ) ;
#48297 = CARTESIAN_POINT ( 'NONE',  ( 4.472210567661338843, 6.310941310395290493, 1.599625672291261402 ) ) ;
#48298 = CARTESIAN_POINT ( 'NONE',  ( 5.788968402910816380, 5.856144012925152076, 0.7216878364870317197 ) ) ;
#48299 = CARTESIAN_POINT ( 'NONE',  ( -7.632314129850253259, 7.869064337772231355, 0.7998128361456341429 ) ) ;
#48300 = CARTESIAN_POINT ( 'NONE',  ( 5.855142236255289845, 7.924361590421551860, -1.599625672291281386 ) ) ;
#48301 = VERTEX_POINT ( 'NONE', #186485 ) ;
#48302 = CARTESIAN_POINT ( 'NONE',  ( 4.781498422495529255, 0.1932255103699429266, -2.003883580701450562 ) ) ;
#48303 = CARTESIAN_POINT ( 'NONE',  ( 0.1580921841808444750, -0.5169658338281759580, -2.248806653996893168 ) ) ;
#48304 = CARTESIAN_POINT ( 'NONE',  ( 4.205873059901494848, 0.6649649114027419428, -1.845726756006949909 ) ) ;
#48305 = CARTESIAN_POINT ( 'NONE',  ( -6.663996196316808174, 7.733415969579778171, -1.199719254218446718 ) ) ;
#48306 = CARTESIAN_POINT ( 'NONE',  ( -4.517891501851816649, 6.293959390292322986, -1.599625672291256295 ) ) ;
#48307 = CARTESIAN_POINT ( 'NONE',  ( -1.499999999999930278, -6.071532165918824830E-15, -10.99818166789402518 ) ) ;
#48308 = CARTESIAN_POINT ( 'NONE',  ( -4.613517410400161722, 8.604463755433990002, -0.7998128361456362523 ) ) ;
#48310 = CARTESIAN_POINT ( 'NONE',  ( 6.209784286858486269, -1.755916252942066436, 0.2208807251847556830 ) ) ;
#48309 = CARTESIAN_POINT ( 'NONE',  ( 0.7321124197560413549, 2.060462595713075995, 0.3535659584654736731 ) ) ;
#48311 = CARTESIAN_POINT ( 'NONE',  ( -0.3423093779010097926, 2.999999999999995559, 0.3999999999999906408 ) ) ;
#48312 = CARTESIAN_POINT ( 'NONE',  ( 6.210880146794990786, -0.2354563166601444379, 1.927560789186753665 ) ) ;
#48313 = FACE_OUTER_BOUND ( 'NONE', #166850, .T. ) ;
#48314 = CARTESIAN_POINT ( 'NONE',  ( 1.223704041615133464, 1.677047869609141983, 0.4652235607782040372 ) ) ;
#48315 = CARTESIAN_POINT ( 'NONE',  ( 6.257251587906815793, 7.258880593101466161, 1.199719254218462483 ) ) ;
#48316 = CARTESIAN_POINT ( 'NONE',  ( 0.2333690889706959148, 4.088440985731725874, -2.608190362703251441 ) ) ;
#48317 = CARTESIAN_POINT ( 'NONE',  ( 2.156509779666794024, -1.334175267976490664, 1.093223185313265899 ) ) ;
#48318 = CARTESIAN_POINT ( 'NONE',  ( 1.734175692058033347, 2.168326105380265378, 0.3173973903456903112 ) ) ;
#48319 = CARTESIAN_POINT ( 'NONE',  ( 3.616033620774202983, -2.174319932014677548, 0.3768175846284789743 ) ) ;
#48320 = MECHANICAL_DESIGN_GEOMETRIC_PRESENTATION_REPRESENTATION (  '', ( #58663 ), #34528 ) ;
#48321 = CARTESIAN_POINT ( 'NONE',  ( 1.323347942641838415, -1.961697495959934479, -0.9305402519725998189 ) ) ;
#48322 = CARTESIAN_POINT ( 'NONE',  ( 4.161989969715272686, 4.726297878971393196, 2.420000000000010587 ) ) ;
#48323 = CARTESIAN_POINT ( 'NONE',  ( 2.747379667311528273, 0.3059357446031922834, -2.094990568135519649 ) ) ;
#48324 = CARTESIAN_POINT ( 'NONE',  ( 6.717748655459607754, -7.246166700180828535, -6.717748655459624629 ) ) ;
#48325 = EDGE_CURVE ( 'NONE', #197280, #148930, #187280, .T. ) ;
#48326 = EDGE_LOOP ( 'NONE', ( #190846, #144179, #91428, #94946 ) ) ;
#48328 = CARTESIAN_POINT ( 'NONE',  ( -1.364683531250000748, -0.4281249996585800854, 0.000000000000000000 ) ) ;
#48327 = CARTESIAN_POINT ( 'NONE',  ( 2.771321709476880280, 2.175846111983824382, -0.7217205603756542409 ) ) ;
#48329 = CARTESIAN_POINT ( 'NONE',  ( -11.84668730067608600, 12.69999999999999929, -1.400000000000001910 ) ) ;
#48330 = CARTESIAN_POINT ( 'NONE',  ( 5.542585869888291938, 5.360771691158120689, -0.7998128361456211532 ) ) ;
#48331 = CARTESIAN_POINT ( 'NONE',  ( 4.758541215226599341, 2.215266761731282674, 0.1642064029221591559 ) ) ;
#48332 = CARTESIAN_POINT ( 'NONE',  ( -7.104109303880803417, 8.350844278358124484, 1.082531754730549967 ) ) ;
#48333 = EDGE_CURVE ( 'NONE', #159860, #123335, #93941, .T. ) ;
#48334 = CARTESIAN_POINT ( 'NONE',  ( -6.520158902582610772, 5.290451655907115303, -2.438235897557448961 ) ) ;
#48335 = CARTESIAN_POINT ( 'NONE',  ( 4.772106882330221289, 6.590544000850479200, -1.443375672974051449 ) ) ;
#48336 = CARTESIAN_POINT ( 'NONE',  ( -7.090551149822745813, 9.295395646258437949, 1.443375672974078761 ) ) ;
#48337 = CARTESIAN_POINT ( 'NONE',  ( 4.340018570150304456, 6.156717313299049366, -1.443375672974068769 ) ) ;
#48338 = ORIENTED_EDGE ( 'NONE', *, *, #138645, .F. ) ;
#48339 = CARTESIAN_POINT ( 'NONE',  ( 2.707657903872981553, 1.899618770239443366, 0.6767133375917554483 ) ) ;
#48341 = CARTESIAN_POINT ( 'NONE',  ( 2.711848548736516040, 0.5542824208455496837, -1.986605816314121808 ) ) ;
#48340 = CARTESIAN_POINT ( 'NONE',  ( 7.786460292950004636, 7.978625184730144149, 1.040834085586084257E-14 ) ) ;
#48342 = DIRECTION ( 'NONE',  ( -0.9510565162951500895, 0.000000000000000000, 0.3090169943749582759 ) ) ;
#48343 = CARTESIAN_POINT ( 'NONE',  ( 4.814553946184248368, 7.670711132973337065, -1.082531754730548412 ) ) ;
#48344 = CARTESIAN_POINT ( 'NONE',  ( -4.609409038966246541, 6.400729850259146758, -1.443375672974053892 ) ) ;
#48345 = CARTESIAN_POINT ( 'NONE',  ( 0.6823417656249917140, 4.092708333674755394, 1.181850606188765695 ) ) ;
#48346 = CARTESIAN_POINT ( 'NONE',  ( 4.892620165872568094, 1.823077252308364482, -1.215776859382920794 ) ) ;
#48347 = CARTESIAN_POINT ( 'NONE',  ( 2.215470409936692420, 1.956561601830292485, 0.4872017847364697452 ) ) ;
#48348 = CARTESIAN_POINT ( 'NONE',  ( 0.9953642579336658969, -1.841430844361633845, 2.783310008858119066E-05 ) ) ;
#48349 = CARTESIAN_POINT ( 'NONE',  ( 7.283754839039659146, 9.520799950344851936, -1.599625672291262513 ) ) ;
#48350 = FILL_AREA_STYLE_COLOUR ( '', #152055 ) ;
#48351 = CARTESIAN_POINT ( 'NONE',  ( 4.893472065931465664, 1.353474861756031267, 1.225258530246610134 ) ) ;
#48352 = CARTESIAN_POINT ( 'NONE',  ( 6.152970239395502361, 1.038990588714868490, 1.728003889287746286 ) ) ;
#48353 = CARTESIAN_POINT ( 'NONE',  ( -7.853197290813634268, 10.18514947741448573, 1.599625672291295375 ) ) ;
#48355 = CARTESIAN_POINT ( 'NONE',  ( -7.130662446144611977, 7.283804040115648526, 0.000000000000000000 ) ) ;
#48354 = CARTESIAN_POINT ( 'NONE',  ( 4.627936124501790260, -1.388401915515205198, -1.786361659577795136 ) ) ;
#48356 = CARTESIAN_POINT ( 'NONE',  ( 0.3816453311432427831, 1.964265557344764712, -0.7602060659359122230 ) ) ;
#48357 = CARTESIAN_POINT ( 'NONE',  ( -6.749980374757255319, 8.968339418673846097, 1.599625672291269396 ) ) ;
#48358 = CARTESIAN_POINT ( 'NONE',  ( 4.879381568908511824, -0.1049739508458477355, 2.067839077007492143 ) ) ;
#48359 = CARTESIAN_POINT ( 'NONE',  ( 9.023114925094663619, 10.48572115315399245, 1.199719254218453823 ) ) ;
#48360 = CARTESIAN_POINT ( 'NONE',  ( -1.360316468750013108, 2.921875000341411788, -1.734723475976807094E-14 ) ) ;
#48361 = CARTESIAN_POINT ( 'NONE',  ( -7.720478407978036195, 11.09464301169468037, -1.199719254218446718 ) ) ;
#48362 = B_SPLINE_CURVE_WITH_KNOTS ( 'NONE', 3,
 ( #39102, #190658, #22818, #26030, #6571, #90000 ),
 .UNSPECIFIED., .F., .F.,
 ( 4, 2, 4 ),
 ( 0.000000000000000000, 0.0003258677429877276867, 0.0006517354859754553734 ),
 .UNSPECIFIED. ) ;
#48363 = DIRECTION ( 'NONE',  ( 8.659560562354941486E-17, -0.7071067811865469066, 0.7071067811865482389 ) ) ;
#48364 = CARTESIAN_POINT ( 'NONE',  ( 6.068156270568149324, 9.237210194708310951, 1.199719254218452047 ) ) ;
#48365 = CARTESIAN_POINT ( 'NONE',  ( 4.809732914444119878, 6.735689552132856583, -1.248430568442916888 ) ) ;
#48366 = CARTESIAN_POINT ( 'NONE',  ( -8.500599126088349777, 12.86119004717103209, 1.040834085586084257E-14 ) ) ;
#48368 = CARTESIAN_POINT ( 'NONE',  ( 1.775925898354186572, 0.3739997881802308299, -2.189552662180799913 ) ) ;
#48367 = CARTESIAN_POINT ( 'NONE',  ( 1.863691559860299884, -1.706161385809309650, -1.259181899442491037 ) ) ;
#48369 = CARTESIAN_POINT ( 'NONE',  ( 4.936581118797800372, 8.100871430792054184, -1.059671831818540966 ) ) ;
#48371 = CIRCLE ( 'NONE', #127924, 11.95586200173889146 ) ;
#48370 = CARTESIAN_POINT ( 'NONE',  ( -5.237192476628793614, 9.332084666034067055, 0.7998128361456291469 ) ) ;
#48372 = CARTESIAN_POINT ( 'NONE',  ( 6.972971076130050072, 7.029554431773520129, 1.040834085586084257E-14 ) ) ;
#48373 = CARTESIAN_POINT ( 'NONE',  ( 3.771884902471400292, -1.933230903833718539, 0.3329965046865584477 ) ) ;
#48374 = CARTESIAN_POINT ( 'NONE',  ( 5.473741331615251227, 7.409117525016355010, -1.599625672291262513 ) ) ;
#48375 = CARTESIAN_POINT ( 'NONE',  ( -4.099290701344459720, 7.507401141727952698, 0.5799236987427489609 ) ) ;
#48376 = CARTESIAN_POINT ( 'NONE',  ( 3.871016551901614200, 4.474939717762034697, -1.199719254218446718 ) ) ;
#48377 = CARTESIAN_POINT ( 'NONE',  ( -5.722950238744243023, 7.770137593325314285, 1.443375672974058777 ) ) ;
#48378 = CARTESIAN_POINT ( 'NONE',  ( -6.887178846062116833, 9.058127958537705027, -1.443375672974059665 ) ) ;
#48379 = CARTESIAN_POINT ( 'NONE',  ( 2.197662576721173266, 1.936918166296027977, -0.8637449004969055544 ) ) ;
#48380 = CARTESIAN_POINT ( 'NONE',  ( -6.947627372360122955, 7.070263120700404968, 0.000000000000000000 ) ) ;
#48381 = CARTESIAN_POINT ( 'NONE',  ( 5.635196431686764207, -0.04651148872366302894, -1.961470878453225763 ) ) ;
#48382 = CARTESIAN_POINT ( 'NONE',  ( 3.309602206082487008, -0.4233974974612622066, 2.119663826602156131 ) ) ;
#48383 = CARTESIAN_POINT ( 'NONE',  ( 2.841158510722852970, 0.6603703904487292498, -1.718939526767604420 ) ) ;
#48384 = CARTESIAN_POINT ( 'NONE',  ( -5.296940370067747317, 6.395615756200102808, 1.134431874056667233 ) ) ;
#48385 = CARTESIAN_POINT ( 'NONE',  ( -1.364683531250000748, -0.4281249996585800854, 0.000000000000000000 ) ) ;
#48386 = ADVANCED_FACE ( 'NONE', ( #118359 ), #83539, .F. ) ;
#48387 = CARTESIAN_POINT ( 'NONE',  ( 4.611116368171574109, -1.705915267380184286, 0.3434222965797654181 ) ) ;
#48388 = CARTESIAN_POINT ( 'NONE',  ( 6.727182134110209155, 1.290711256955964448, 1.927001067762003972 ) ) ;
#48389 = CARTESIAN_POINT ( 'NONE',  ( 3.660338286009610975, 6.253849852777763729, -1.082531754730543083 ) ) ;
#48390 =( LENGTH_UNIT ( ) NAMED_UNIT ( * ) SI_UNIT ( .MILLI., .METRE. ) );
#48391 = CARTESIAN_POINT ( 'NONE',  ( 2.536181837661064087, 1.019768383293401248, -1.906060392209196763 ) ) ;
#48392 = AXIS2_PLACEMENT_3D ( 'NONE', #41702, #155423, #58992 ) ;
#48393 = CARTESIAN_POINT ( 'NONE',  ( 4.639999869408336863, 0.002810260262744306969, -2.016288307263448321 ) ) ;
#48394 = CARTESIAN_POINT ( 'NONE',  ( -9.178506806327330736, 10.77097469787910455, 1.082531754730558626 ) ) ;
#48395 = CARTESIAN_POINT ( 'NONE',  ( 1.850665834824256173, 0.6780317805383448970, 2.052694239800388676 ) ) ;
#48396 = CARTESIAN_POINT ( 'NONE',  ( 2.952367129307902793, 0.6606739728568145065, 1.857499748845674370 ) ) ;
#48397 = DIRECTION ( 'NONE',  ( -0.000000000000000000, -8.546850786086437571E-32, -1.000000000000000000 ) ) ;
#48398 = CARTESIAN_POINT ( 'NONE',  ( 3.210425159823264707, 1.756831471361683494, 0.8279855452232912638 ) ) ;
#48399 = B_SPLINE_CURVE_WITH_KNOTS ( 'NONE', 3,
 ( #77257, #94607, #92479, #207253, #158520, #125036, #127172 ),
 .UNSPECIFIED., .F., .F.,
 ( 4, 3, 4 ),
 ( 0.000000000000000000, 0.0008000000000004422844, 0.002977368225425623249 ),
 .UNSPECIFIED. ) ;
#48402 = ORIENTED_EDGE ( 'NONE', *, *, #180391, .F. ) ;
#48401 = CARTESIAN_POINT ( 'NONE',  ( 9.950255243072246565E-16, 7.999999999999992895, -7.750000000000000888 ) ) ;
#48400 = CARTESIAN_POINT ( 'NONE',  ( -8.310784975052669665, 12.63974020429606249, -0.7216878364870267237 ) ) ;
#48403 = CARTESIAN_POINT ( 'NONE',  ( -8.120407659942227241, 8.438506789546210030, 0.7998128361456341429 ) ) ;
#48404 = CARTESIAN_POINT ( 'NONE',  ( 2.898410978271408922, 6.603506251283770112, -0.7998128361456362523 ) ) ;
#48405 = EDGE_CURVE ( 'NONE', #24930, #51151, #88673, .T. ) ;
#48407 = ORIENTED_EDGE ( 'NONE', *, *, #102049, .F. ) ;
#48406 = CARTESIAN_POINT ( 'NONE',  ( -4.796552484184649856, 8.818004674849227342, -0.7998128361456362523 ) ) ;
#48408 = CARTESIAN_POINT ( 'NONE',  ( -8.527715432871366019, 10.01171809551380143, 1.082531754730558626 ) ) ;
#48409 = CARTESIAN_POINT ( 'NONE',  ( 1.466163881440044836, 2.173982691173735216, -0.3780781022180225159 ) ) ;
#48410 = CARTESIAN_POINT ( 'NONE',  ( 1.642778471875001811, -2.442708332855377140, 2.845375778867859751 ) ) ;
#48411 = CARTESIAN_POINT ( 'NONE',  ( 5.700043108275813175, 0.7984002208856562088, -1.792138013221859394 ) ) ;
#48412 = CARTESIAN_POINT ( 'NONE',  ( -0.6823417656250212460, 5.363541667008087543, 1.181850606188767472 ) ) ;
#48413 = CARTESIAN_POINT ( 'NONE',  ( -0.7500000000000215383, 2.972916667349487341, 1.299038105676671107 ) ) ;
#48414 = CARTESIAN_POINT ( 'NONE',  ( 0.1745949693968875116, 2.894395776691494060, -2.244452406707102110 ) ) ;
#48415 = CARTESIAN_POINT ( 'NONE',  ( 4.699059028873219468, -0.4882365319774860102, 1.775153104902137624 ) ) ;
#48416 = ORIENTED_EDGE ( 'NONE', *, *, #193200, .F. ) ;
#48417 = CARTESIAN_POINT ( 'NONE',  ( -6.561256274009600986, 9.742217188731485678, -1.199719254218440723 ) ) ;
#48418 = CARTESIAN_POINT ( 'NONE',  ( 1.347111479062088405E-15, 6.999999999999999112, 11.00000000000000000 ) ) ;
#48419 = CARTESIAN_POINT ( 'NONE',  ( 4.834296457332984076, -1.136628438424293508, -1.790084250976264002 ) ) ;
#48420 = CARTESIAN_POINT ( 'NONE',  ( -5.524540912749783317, 5.975067110676214988, -0.9400251737342411040 ) ) ;
#48421 = CARTESIAN_POINT ( 'NONE',  ( 6.986529229743720926, 7.045372277656132276, -0.7998128361456281477 ) ) ;
#48422 = CARTESIAN_POINT ( 'NONE',  ( 6.731718603199120743, -1.342629487124985532, -1.563498854789405534 ) ) ;
#48425 = CARTESIAN_POINT ( 'NONE',  ( 3.473999211503727036, -1.775402473473717935, -0.4878004006634574230 ) ) ;
#48424 = CARTESIAN_POINT ( 'NONE',  ( 0.5900176457281476328, 0.9615612750370464701, -1.593262740414502776 ) ) ;
#48423 = CARTESIAN_POINT ( 'NONE',  ( -4.168895032367330167, 3.976329666238523242, -0.6109567437776577403 ) ) ;
#48426 = CARTESIAN_POINT ( 'NONE',  ( 7.639129486296027061, 10.99973593639901814, 1.199719254218460707 ) ) ;
#48427 = CARTESIAN_POINT ( 'NONE',  ( -6.959052028702998882, 5.167241622962444936, 1.214306433183764966E-14 ) ) ;
#48428 = CARTESIAN_POINT ( 'NONE',  ( -7.228432174741334038, 8.462200954400218578, -1.199719254218452047 ) ) ;
#48429 = CARTESIAN_POINT ( 'NONE',  ( 4.638229190868996987, 5.411267389347211854, 2.420000000000010587 ) ) ;
#48430 = CARTESIAN_POINT ( 'NONE',  ( 3.158999515626020216, -1.670948785577108797, 1.441709373268922123 ) ) ;
#48431 = CARTESIAN_POINT ( 'NONE',  ( 5.378307924748570557, -1.263187946576078247, 1.876752126472463367 ) ) ;
#48432 = CARTESIAN_POINT ( 'NONE',  ( -6.561783159334137139, 8.678499657355050800, -1.443375672974059665 ) ) ;
#48433 = CARTESIAN_POINT ( 'NONE',  ( 5.361500737056818622, -1.433101695931580100, -1.108104203189824277 ) ) ;
#48434 = CARTESIAN_POINT ( 'NONE',  ( 5.014804717692854297, 0.1473437859633792701, 1.910143238840347868 ) ) ;
#48435 = CARTESIAN_POINT ( 'NONE',  ( 1.364683531249988535, 4.967708333674756283, -0.7879004041258300672 ) ) ;
#48436 = AXIS2_PLACEMENT_3D ( 'NONE', #155352, #70866, #212621 ) ;
#48437 = CARTESIAN_POINT ( 'NONE',  ( 6.315307248462690204, -0.2269180964024133385, 1.856785020699961875 ) ) ;
#48438 = CARTESIAN_POINT ( 'NONE',  ( 6.180112001919068732, -1.034620502799053599, -1.546732508075428392 ) ) ;
#48439 = CARTESIAN_POINT ( 'NONE',  ( -5.883875478206491927, 5.966868934103426447, 0.000000000000000000 ) ) ;
#48440 = CARTESIAN_POINT ( 'NONE',  ( 6.385617153790816403, 1.223975321695195184, 1.278628327690333411 ) ) ;
#48441 = CARTESIAN_POINT ( 'NONE',  ( 1.130092623156966347, 2.014433208573155110, 0.09411304420373775570 ) ) ;
#48443 = CARTESIAN_POINT ( 'NONE',  ( 2.983145545965359080, -0.1552688264333592638, -2.100405815202969873 ) ) ;
#48442 = CARTESIAN_POINT ( 'NONE',  ( -8.696665468161981494, 12.23352791524263239, -1.199719254218446718 ) ) ;
#48444 = EDGE_CURVE ( 'NONE', #123444, #162756, #111300, .T. ) ;
#48445 = CARTESIAN_POINT ( 'NONE',  ( 7.248805684800777804, 11.60869039890961218, 1.040834085586084257E-14 ) ) ;
#48447 = CARTESIAN_POINT ( 'NONE',  ( -8.992082194361570302, 11.51384853155376220, 1.599625672291269396 ) ) ;
#48446 = DIRECTION ( 'NONE',  ( -0.000000000000000000, 1.000000000000000000, -0.000000000000000000 ) ) ;
#48448 = CARTESIAN_POINT ( 'NONE',  ( 1.499999999999989120, 6.280000000000042881, -2.579999999999995630 ) ) ;
#48449 = CARTESIAN_POINT ( 'NONE',  ( 2.197526642425628118, 1.844980167888200961, -0.8223984085018556378 ) ) ;
#48450 = CARTESIAN_POINT ( 'NONE',  ( -1.201851678989727383E-14, 2.571875000341417472, 1.575800808251672791 ) ) ;
#48451 = EDGE_CURVE ( 'NONE', #106888, #5398, #40254, .T. ) ;
#48452 = CARTESIAN_POINT ( 'NONE',  ( 4.546061579283848353, 4.198160018786257552, -0.7998128361456211532 ) ) ;
#48453 = CARTESIAN_POINT ( 'NONE',  ( 3.743588348364734752, -1.634107004491680115, -1.415051943026650161 ) ) ;
#48454 = CARTESIAN_POINT ( 'NONE',  ( 6.890000000000006786, 1.992106636881568305, 2.580154195607385237 ) ) ;
#48457 = DIRECTION ( 'NONE',  ( 0.7592566023653005702, -0.6507913734559640506, 0.000000000000000000 ) ) ;
#48456 = CARTESIAN_POINT ( 'NONE',  ( -4.222669843016471525, 3.519858668466405494, -2.499999999999995559 ) ) ;
#48455 = CARTESIAN_POINT ( 'NONE',  ( 5.598591087800349086, 5.496387455380669529, -0.7998128361456481317 ) ) ;
#48458 = CARTESIAN_POINT ( 'NONE',  ( 8.215877899756996783, 12.52901528311778989, 1.040834085586084257E-14 ) ) ;
#48459 = CARTESIAN_POINT ( 'NONE',  ( -7.700668062882078502, 9.046829497192987901, -1.082531754730543971 ) ) ;
#48460 = CARTESIAN_POINT ( 'NONE',  ( 0.6823417656249882723, 0.3427083336747516196, 1.181850606188755259 ) ) ;
#48461 = CARTESIAN_POINT ( 'NONE',  ( 1.540847765565691585, -1.849059859674206496, 1.176127931831471907 ) ) ;
#48462 = CARTESIAN_POINT ( 'NONE',  ( 0.5473748313345295768, 7.493086169160064536, 1.923660786605030149 ) ) ;
#48463 = CARTESIAN_POINT ( 'NONE',  ( 2.202381998968961696, -2.261980054776930427, 0.05578962468580014183 ) ) ;
#48464 = CARTESIAN_POINT ( 'NONE',  ( -8.518600588087975822, 8.832788862391110385, 1.040834085586084257E-14 ) ) ;
#48465 = CARTESIAN_POINT ( 'NONE',  ( -3.592547517496935683, 6.174760622846296343, -1.082531754730548412 ) ) ;
#48466 = CARTESIAN_POINT ( 'NONE',  ( -1.201851678989727383E-14, 2.884375000341418804, 1.575800808251672791 ) ) ;
#48467 = LINE ( 'NONE', #98271, #203056 ) ;
#48468 = CARTESIAN_POINT ( 'NONE',  ( -1.500000000000008216, 10.74999999999999645, 3.469446951953614189E-15 ) ) ;
#48469 = CARTESIAN_POINT ( 'NONE',  ( 7.241463443474815520, 8.581367117876336437, -1.082531754730548412 ) ) ;
#48470 = CARTESIAN_POINT ( 'NONE',  ( 3.567426164108201903, 1.727176351593662007, -0.3850055527321315507 ) ) ;
#48471 = CARTESIAN_POINT ( 'NONE',  ( 0.1476710321905516377, -1.628112296142746995, -1.335496995165935674 ) ) ;
#48472 = CARTESIAN_POINT ( 'NONE',  ( 1.364683531249996529, 9.213541667008062319, 0.7879004041258405033 ) ) ;
#48473 = VERTEX_POINT ( 'NONE', #137763 ) ;
#48474 = CARTESIAN_POINT ( 'NONE',  ( -6.459533842268148973, 6.500820668926428958, 0.000000000000000000 ) ) ;
#48475 = CARTESIAN_POINT ( 'NONE',  ( 4.622672832840883039, 0.3474877929729481840, 1.986098205159859909 ) ) ;
#48476 = EDGE_LOOP ( 'NONE', ( #95415, #122101, #169640, #2791 ) ) ;
#48477 = CARTESIAN_POINT ( 'NONE',  ( 2.113927203836548419, -0.8795192785214582809, -1.650985937663045577 ) ) ;
#48478 = CARTESIAN_POINT ( 'NONE',  ( 3.784089331405198653, -1.229265877060268242, -1.665672133652921660 ) ) ;
#48479 = CARTESIAN_POINT ( 'NONE',  ( -7.553300976144794454, 7.984808358356614733, -0.7216878364870338292 ) ) ;
#48480 = CARTESIAN_POINT ( 'NONE',  ( 2.004032382285144021, -0.8144628449315849394, 1.730399521388835460 ) ) ;
#48481 = CARTESIAN_POINT ( 'NONE',  ( -0.3982008013781589417, -4.205834154662571933, -0.9999999999999991118 ) ) ;
#48482 = CARTESIAN_POINT ( 'NONE',  ( -4.995253251992230581, 4.792493313604505367, 0.000000000000000000 ) ) ;
#48483 = CARTESIAN_POINT ( 'NONE',  ( -1.364683531250012516, 4.301041667008089320, -0.7879004041258300672 ) ) ;
#48484 = CARTESIAN_POINT ( 'NONE',  ( 1.564566645345835338, 0.6029492335615972420, 1.814891859350221459 ) ) ;
#48485 = CARTESIAN_POINT ( 'NONE',  ( 2.277722772326017608, -1.903703133612335119, 0.4737097981617058862 ) ) ;
#48486 = CARTESIAN_POINT ( 'NONE',  ( 0.5091384654962345380, 2.010518347751136137, 0.1511200514899835312 ) ) ;
#48487 = CARTESIAN_POINT ( 'NONE',  ( -3.610214042988883598, 7.433943160120816351, 0.7998128361456352531 ) ) ;
#48489 = DIRECTION ( 'NONE',  ( 0.000000000000000000, 0.000000000000000000, 1.000000000000000000 ) ) ;
#48488 = CARTESIAN_POINT ( 'NONE',  ( 8.609591239877852686, 10.00327685373437347, -1.199719254218445830 ) ) ;
#48490 = CARTESIAN_POINT ( 'NONE',  ( 6.380149230842863339, -1.056690401097816867, 1.664064485322758635 ) ) ;
#48491 = CARTESIAN_POINT ( 'NONE',  ( -0.6823417656250212460, 2.801041667008084879, 1.181850606188767472 ) ) ;
#48492 = CARTESIAN_POINT ( 'NONE',  ( 2.443610342004947533, -1.876944004186463566, 0.7284700530331960078 ) ) ;
#48494 = CARTESIAN_POINT ( 'NONE',  ( 2.443091204979094044, -1.843612287508783920, -1.040880819149572201 ) ) ;
#48493 = CARTESIAN_POINT ( 'NONE',  ( -6.046573322014817897, 9.998159942418544333, 0.7216878364870458196 ) ) ;
#48495 = CARTESIAN_POINT ( 'NONE',  ( 4.176279081494421952, -1.061646348645030713, -1.777293304589353085 ) ) ;
#48496 = CARTESIAN_POINT ( 'NONE',  ( 4.224247379109608680, 7.085983154673295203, -1.199719254218452047 ) ) ;
#48498 = CARTESIAN_POINT ( 'NONE',  ( 5.366329872910639232, 5.155139694684188534, 1.040834085586084257E-14 ) ) ;
#48497 = CARTESIAN_POINT ( 'NONE',  ( 5.296857843117306786, 1.708683220140273740, 1.204356289764816568 ) ) ;
#48500 = ORIENTED_EDGE ( 'NONE', *, *, #72198, .F. ) ;
#48499 = CARTESIAN_POINT ( 'NONE',  ( 3.803562306130504389, -0.5304149723801485639, 1.746809896627635084 ) ) ;
#48501 = CARTESIAN_POINT ( 'NONE',  ( 9.511208455186636712, 11.05516360492796935, 1.199719254218453823 ) ) ;
#48502 = CARTESIAN_POINT ( 'NONE',  ( -1.249999999999964695, 8.500000000000000000, -10.97907099895069294 ) ) ;
#48503 = CARTESIAN_POINT ( 'NONE',  ( 10.78205070141670774, 8.191904004416022289, 2.765601532466400947 ) ) ;
#48504 = CARTESIAN_POINT ( 'NONE',  ( -10.44369227015510404, 5.112964020592959180, 5.232143560358712087 ) ) ;
#48505 = CARTESIAN_POINT ( 'NONE',  ( 1.364683531249997417, 11.29687500034139802, 2.602085213965210642E-15 ) ) ;
#48506 = ORIENTED_EDGE ( 'NONE', *, *, #80530, .F. ) ;
#48507 = CARTESIAN_POINT ( 'NONE',  ( 4.740819843082155316, 1.831016553098392619, 0.5515768964349797576 ) ) ;
#48508 = CARTESIAN_POINT ( 'NONE',  ( -3.297657676621885692, 4.870353260857385180, 1.599625672291267398 ) ) ;
#48509 = CARTESIAN_POINT ( 'NONE',  ( 6.662942426112080874, 9.860851032851066122, 1.199719254218460707 ) ) ;
#48510 = CARTESIAN_POINT ( 'NONE',  ( 0.6801582343749674742, 1.755208333674734833, 1.178068619123803451 ) ) ;
#48511 = CARTESIAN_POINT ( 'NONE',  ( 3.497640442201256139, 7.024404915969360452, 1.040834085586084257E-14 ) ) ;
#48512 = DIRECTION ( 'NONE',  ( 1.039099362110107450E-15, 1.000000000000000000, -4.583713267641621330E-32 ) ) ;
#48513 = CARTESIAN_POINT ( 'NONE',  ( 0.000000000000000000, 13.79999999999999893, 0.000000000000000000 ) ) ;
#48514 = CARTESIAN_POINT ( 'NONE',  ( 0.3625324912872700533, 0.1813134127766780901, -1.832273687604975665 ) ) ;
#48515 = ORIENTED_EDGE ( 'NONE', *, *, #6025, .F. ) ;
#48516 = CARTESIAN_POINT ( 'NONE',  ( -7.937372586157736443, 8.224965870130965584, 0.7998128361456341429 ) ) ;
#48517 = CARTESIAN_POINT ( 'NONE',  ( 5.079306140367803479, 1.745876537259077432, -0.6719496041647440299 ) ) ;
#48518 = CARTESIAN_POINT ( 'NONE',  ( -2.788906526875773208E-15, 8.687500000000000000, -1.499999999999998446 ) ) ;
#48519 = CARTESIAN_POINT ( 'NONE',  ( 7.289443866002793371, 8.533381260871966134, 1.199719254218452047 ) ) ;
#48520 = CARTESIAN_POINT ( 'NONE',  ( 0.000000000000000000, 13.49999999999999822, 0.000000000000000000 ) ) ;
#48521 =( BOUNDED_CURVE ( )  B_SPLINE_CURVE ( 2, ( #111441, #31200, #13850, #193678, #61553 ),
 .UNSPECIFIED., .F., .T. ) 
 B_SPLINE_CURVE_WITH_KNOTS ( ( 3, 2, 3 ),
 ( 0.2461390157910678111, 0.2500000000000000000, 0.2545216234105981967 ),
 .UNSPECIFIED. ) 
 CURVE ( )  GEOMETRIC_REPRESENTATION_ITEM ( )  RATIONAL_B_SPLINE_CURVE ( ( 0.9333732439868740460, 0.9379271439536381871, 1.000000000000000000, 0.9273060795191534478, 0.9334988468753528945 ) ) 
 REPRESENTATION_ITEM ( '' )  );
#48522 = CARTESIAN_POINT ( 'NONE',  ( -7.266807147244793263, 8.540658428949452485, 1.082531754730549967 ) ) ;
#48523 = CARTESIAN_POINT ( 'NONE',  ( 4.660252114795294887, 6.460046772059735432, -1.599625672291256295 ) ) ;
#48524 = CARTESIAN_POINT ( 'NONE',  ( 0.9011414689646871645, -1.692011168669171672, 1.007586202480597048 ) ) ;
#48525 = CARTESIAN_POINT ( 'NONE',  ( 2.319935610374638468, 0.9480221781073931986, -1.779637559903464394 ) ) ;
#48526 = CARTESIAN_POINT ( 'NONE',  ( -7.483210719738908168, 10.81783070874899799, 1.199719254218453823 ) ) ;
#48527 = CARTESIAN_POINT ( 'NONE',  ( 4.505052181490820651, 8.477920988373101707, -0.7998128361456381397 ) ) ;
#48528 = CARTESIAN_POINT ( 'NONE',  ( 6.776370306708059843, -7.161464053357565973, 6.781144757626057284 ) ) ;
#48529 = CARTESIAN_POINT ( 'NONE',  ( 2.062683196291382082, -2.004346222996217897, -0.8864330828558324438 ) ) ;
#48530 = CARTESIAN_POINT ( 'NONE',  ( -2.173285075505815599E-15, -8.011313137147263674, 11.00000000000000178 ) ) ;
#48531 = CARTESIAN_POINT ( 'NONE',  ( -10.45741655484220267, 11.09474082360439873, -0.7998128361456221525 ) ) ;
#48532 = CARTESIAN_POINT ( 'NONE',  ( 6.825078400183548055, 3.702925343214446663, 2.370119418288775925 ) ) ;
#48533 = CARTESIAN_POINT ( 'NONE',  ( 10.40709887848268167, 1.794419290072776896, -5.561702625701125946 ) ) ;
#48534 = EDGE_CURVE ( 'NONE', #72912, #31219, #138922, .T. ) ;
#48535 = CARTESIAN_POINT ( 'NONE',  ( 4.340018570150304456, 6.156717313299049366, -1.443375672974068769 ) ) ;
#48536 = CARTESIAN_POINT ( 'NONE',  ( 7.801827329660018684, 11.18955008699033726, 1.199719254218460707 ) ) ;
#48537 = DIRECTION ( 'NONE',  ( -0.8079921913829680724, -5.171644362755859381E-12, -0.5891931929886402575 ) ) ;
#48538 = CARTESIAN_POINT ( 'NONE',  ( 7.526184669361807522, 7.953172667109813077, 0.000000000000000000 ) ) ;
#48539 = ORIENTED_EDGE ( 'NONE', *, *, #111774, .F. ) ;
#48541 = CARTESIAN_POINT ( 'NONE',  ( 1.822903811843211264, 1.490285103888006280, -1.353523025221949450 ) ) ;
#48540 = CARTESIAN_POINT ( 'NONE',  ( 4.634224865634020141, 0.3196297827482602050, 1.813140464320086132 ) ) ;
#48542 = ORIENTED_EDGE ( 'NONE', *, *, #116473, .T. ) ;
#48543 = CARTESIAN_POINT ( 'NONE',  ( 3.550466583917981200, 2.079229874635016184, -0.9797032261932754338 ) ) ;
#48545 = CARTESIAN_POINT ( 'NONE',  ( 1.533807339325540475, 1.103149047995868104, 1.498595216881804859 ) ) ;
#48544 = CARTESIAN_POINT ( 'NONE',  ( -0.1290005225502641184, 1.996213967822700663, -2.587563282167547385 ) ) ;
#48546 = CARTESIAN_POINT ( 'NONE',  ( 1.642778471875000035, -1.626041666188710044, -2.845375778867859751 ) ) ;
#48547 = CARTESIAN_POINT ( 'NONE',  ( -4.038971567461725698, 3.986455684509185193, -0.5169845646830102392 ) ) ;
#48548 = CARTESIAN_POINT ( 'NONE',  ( 5.906500813101932756, -1.903809282439900219, -0.1807861040028224398 ) ) ;
#48549 = CARTESIAN_POINT ( 'NONE',  ( -7.700141177557535244, 11.07091624287075859, -1.199719254218446718 ) ) ;
#48550 = CARTESIAN_POINT ( 'NONE',  ( -5.302647476720585118, 9.200522799567075083, 0.000000000000000000 ) ) ;
#48552 = CARTESIAN_POINT ( 'NONE',  ( 3.221420234344949840, -1.803205065257794004, 0.4975683872451354683 ) ) ;
#48551 = CARTESIAN_POINT ( 'NONE',  ( 4.722262070665103728, 2.001137821747037915, 0.6055792653000735548 ) ) ;
#48553 = CARTESIAN_POINT ( 'NONE',  ( 7.998947442382716488, 9.394822106610419610, -1.082531754730543083 ) ) ;
#48554 = CARTESIAN_POINT ( 'NONE',  ( 5.460457653299121361, -1.667157065227730106, -0.7818181906407914994 ) ) ;
#48555 = CARTESIAN_POINT ( 'NONE',  ( 4.467575310902914154, 5.170924936596891008, 1.199719254218464037 ) ) ;
#48556 = FACE_BOUND ( 'NONE', #152390, .T. ) ;
#48557 = CARTESIAN_POINT ( 'NONE',  ( 4.600069218058569831, -1.724633479392148949, -0.03822871362766516734 ) ) ;
#48558 = CARTESIAN_POINT ( 'NONE',  ( -5.716734326456539783, 9.821273814174633188, -0.7998128361456231517 ) ) ;
#48559 = FILL_AREA_STYLE_COLOUR ( '', #44015 ) ;
#48560 = CARTESIAN_POINT ( 'NONE',  ( 1.886017674307056691, 3.298060805577443411, 0.4014564593430875461 ) ) ;
#48561 = CARTESIAN_POINT ( 'NONE',  ( 9.578446392664460518, -9.953004327042588528, -0.1519871474491476526 ) ) ;
#48562 = CARTESIAN_POINT ( 'NONE',  ( 5.260662464746663325, -0.7247129924745611129, -2.046699161452083526 ) ) ;
#48563 = CARTESIAN_POINT ( 'NONE',  ( 3.580510235063854019, -1.759844519496515325, -0.4856381957471164745 ) ) ;
#48564 = CARTESIAN_POINT ( 'NONE',  ( 0.6901946996495964548, 1.013433542811643440, -1.679602092450118711 ) ) ;
#48565 = CARTESIAN_POINT ( 'NONE',  ( 6.210183267806027807, 1.217293573752244784, -1.732272713164469735 ) ) ;
#48566 = ADVANCED_FACE ( 'NONE', ( #73808 ), #87929, .F. ) ;
#48568 = CARTESIAN_POINT ( 'NONE',  ( 1.364683531249988535, 3.967708333674751842, -0.7879004041258239610 ) ) ;
#48567 = CARTESIAN_POINT ( 'NONE',  ( 5.829661053323575537, 1.133102282163217955, -1.992656795126966252 ) ) ;
#48569 = CARTESIAN_POINT ( 'NONE',  ( 4.957044826792370351, 6.512741263613364140, 2.499999999999778399 ) ) ;
#48570 = CARTESIAN_POINT ( 'NONE',  ( 7.865701674222579598, 12.32840238656838139, -0.7998128361456352531 ) ) ;
#48571 = TOROIDAL_SURFACE ( 'NONE', #34790, 10.92000000000000171, 0.08000000000000000167 ) ;
#48572 = CARTESIAN_POINT ( 'NONE',  ( 1.243013918421622455, 2.044566944090483229, 0.5621290157047582614 ) ) ;
#48573 = CARTESIAN_POINT ( 'NONE',  ( -2.643476764984671767, 6.027880625883323518, 1.040834085586084257E-14 ) ) ;
#48574 = ADVANCED_FACE ( 'NONE', ( #105267 ), #205933, .T. ) ;
#48575 = DIRECTION ( 'NONE',  ( 0.000000000000000000, 0.000000000000000000, 1.000000000000000000 ) ) ;
#48576 = CARTESIAN_POINT ( 'NONE',  ( -3.863710589770277259, 6.491117540498504646, 1.082531754730560403 ) ) ;
#48577 = CARTESIAN_POINT ( 'NONE',  ( 6.649308703871936288, 1.893188687436907047, -1.062577851937399620 ) ) ;
#48579 = CARTESIAN_POINT ( 'NONE',  ( -1.402160292154681736E-14, 12.34375000068279782, 1.732050807568881190 ) ) ;
#48578 = CARTESIAN_POINT ( 'NONE',  ( 6.983263157960363898, 3.684327263089666182, 2.667753665259400275 ) ) ;
#48581 = ORIENTED_EDGE ( 'NONE', *, *, #71920, .T. ) ;
#48580 = CARTESIAN_POINT ( 'NONE',  ( 2.702056655550812980, 1.572631313784816687, 1.569006521454456848 ) ) ;
#48582 = CARTESIAN_POINT ( 'NONE',  ( 5.977185442992979603, -2.006959616289708315, -0.1948445219252663840 ) ) ;
#48584 = CARTESIAN_POINT ( 'NONE',  ( 5.067260671706765862, 1.791893645760339826, 1.021364248522889762 ) ) ;
#48583 = CARTESIAN_POINT ( 'NONE',  ( 3.323720213644492993, 7.029424015893889433, 1.040834085586084257E-14 ) ) ;
#48586 = CARTESIAN_POINT ( 'NONE',  ( 1.737500000000001155, -3.383333333333331971, 3.009438278150922130 ) ) ;
#48585 = CARTESIAN_POINT ( 'NONE',  ( 5.692444392891300886, 7.734547439830227411, -1.599625672291281386 ) ) ;
#48587 = CARTESIAN_POINT ( 'NONE',  ( 6.900173834712277632, 7.014900660111269559, -0.7998128361456341429 ) ) ;
#48588 = CARTESIAN_POINT ( 'NONE',  ( -3.285556943750000514, -2.676041666188707424, -1.896917185911906500 ) ) ;
#48589 = CARTESIAN_POINT ( 'NONE',  ( 0.1329588055935214119, 5.724880713053031478, -2.439996743105294907 ) ) ;
#48590 = CARTESIAN_POINT ( 'NONE',  ( 4.985823801847525161, -1.827980399782932697, -0.2200341325891697619 ) ) ;
#48591 = CARTESIAN_POINT ( 'NONE',  ( 4.547870462380197765, 7.393267075163835855, 1.199719254218462483 ) ) ;
#48592 = CARTESIAN_POINT ( 'NONE',  ( 1.395042272690392604, 1.302445673786157831, 1.130794771346554928 ) ) ;
#48593 = CARTESIAN_POINT ( 'NONE',  ( 0.2160302486270138655, 1.032475520995678853, -1.731998313101141163 ) ) ;
#48594 = CARTESIAN_POINT ( 'NONE',  ( 1.899501351379283554, -1.088314401552924249, -2.024763765589305820 ) ) ;
#48595 = CARTESIAN_POINT ( 'NONE',  ( 0.6823417656249917140, 4.405208333674755394, 1.181850606188765695 ) ) ;
#48596 = CARTESIAN_POINT ( 'NONE',  ( 1.318052817733056825, -2.207296558944459974, 0.4957021660386366491 ) ) ;
#48597 = CARTESIAN_POINT ( 'NONE',  ( 4.635441201516187881, -1.925843587088198916, 0.8528682856967207959 ) ) ;
#48598 = CARTESIAN_POINT ( 'NONE',  ( -3.797165540279144214, 6.587721009371067638, 1.199719254218452935 ) ) ;
#48599 = CARTESIAN_POINT ( 'NONE',  ( 2.495042215028328236, 1.364832443287033570, 1.126547774882515673 ) ) ;
#48600 = CARTESIAN_POINT ( 'NONE',  ( 7.070740804726770357, 8.207951346058097286, 1.199719254218462483 ) ) ;
#48601 = CARTESIAN_POINT ( 'NONE',  ( 4.950135482320912494, 6.868520377498098739, -1.443375672974068769 ) ) ;
#48602 = CARTESIAN_POINT ( 'NONE',  ( -6.087774667736030487, 7.061157519568837415, 1.199719254218450271 ) ) ;
#48603 = CARTESIAN_POINT ( 'NONE',  ( -1.500000000000011324, 2.670833333333352044, 0.8660254037844403729 ) ) ;
#48604 = CARTESIAN_POINT ( 'NONE',  ( 6.416288448142412726, -2.220950948806613034, 0.05311210701240512422 ) ) ;
#48605 = CARTESIAN_POINT ( 'NONE',  ( 3.380998015235132215, 1.981133383611884735, -0.9370748116589098231 ) ) ;
#48606 = CARTESIAN_POINT ( 'NONE',  ( -5.111587607552082524, 5.922272616020886282, 1.199719254218450271 ) ) ;
#48607 = CARTESIAN_POINT ( 'NONE',  ( 0.004619473214107315887, 7.151453204069587066, -1.999995854215781410 ) ) ;
#48608 = CARTESIAN_POINT ( 'NONE',  ( 6.393239817247728496, -0.1034752114322245314, -2.118097640427937911 ) ) ;
#48609 =( BOUNDED_CURVE ( )  B_SPLINE_CURVE ( 2, ( #198, #146526, #130325, #66267, #198417, #183247, #50061 ),
 .UNSPECIFIED., .F., .T. ) 
 B_SPLINE_CURVE_WITH_KNOTS ( ( 3, 2, 2, 3 ),
 ( 0.2375000000000003775, 0.2416666666666668351, 0.2458333333333332926, 0.2499999999999997502 ),
 .UNSPECIFIED. ) 
 CURVE ( )  GEOMETRIC_REPRESENTATION_ITEM ( )  RATIONAL_B_SPLINE_CURVE ( ( 0.9999999999999874545, 0.8660254037844512531, 1.000000000000000000, 0.8660254037844387076, 1.000000000000000000, 0.8660254037844467012, 0.9999999999999920064 ) ) 
 REPRESENTATION_ITEM ( '' )  );
#48610 = COLOUR_RGB ( '', 0.40784314, 0.44705882, 0.49803922) ;
#48611 = CARTESIAN_POINT ( 'NONE',  ( 1.364683531249990311, 2.884375000341422801, 1.214306433183764966E-14 ) ) ;
#48612 = CARTESIAN_POINT ( 'NONE',  ( -1.364683531250010295, 9.630208333674735499, 0.7879004041258445001 ) ) ;
#48613 = CARTESIAN_POINT ( 'NONE',  ( -5.260200412422220140, 5.239248024021764039, -0.7216878364870207285 ) ) ;
#48614 = CARTESIAN_POINT ( 'NONE',  ( 5.871359616481898414, -1.819694913365289768, -1.088597390283413402 ) ) ;
#48615 = CARTESIAN_POINT ( 'NONE',  ( -5.912764389335557702, 8.951956649983198844, 1.082531754730550855 ) ) ;
#48616 = EDGE_LOOP ( 'NONE', ( #3313, #189788, #13039, #74092 ) ) ;
#48618 = CARTESIAN_POINT ( 'NONE',  ( 4.318982125183886467, 7.080239525325785266, 1.240331472013181058 ) ) ;
#48617 = CARTESIAN_POINT ( 'NONE',  ( -4.001064729808656573, 7.682009594836471500, 1.214306433183764966E-14 ) ) ;
#48619 = CARTESIAN_POINT ( 'NONE',  ( 4.306686350635271054, 8.176217842383143974, -0.7998128361456221525 ) ) ;
#48620 = CARTESIAN_POINT ( 'NONE',  ( 6.286648950733226826, 1.598451336667701339, -0.9137711784916457969 ) ) ;
#48621 = FACE_OUTER_BOUND ( 'NONE', #52117, .T. ) ;
#48622 = CARTESIAN_POINT ( 'NONE',  ( -1.364683531250010295, 4.092708333674751842, 0.7879004041258379498 ) ) ;
#48623 = CARTESIAN_POINT ( 'NONE',  ( 1.962089020239773163, -1.591546648218734816, -0.7047476087739585893 ) ) ;
#48624 = CARTESIAN_POINT ( 'NONE',  ( 3.979481780810941949, 4.601482484822914998, 1.199719254218464037 ) ) ;
#48625 = CARTESIAN_POINT ( 'NONE',  ( -1.402160292154681736E-14, -0.4906249996585810846, -1.575800808251665908 ) ) ;
#48626 = CARTESIAN_POINT ( 'NONE',  ( -0.4516138619288407874, 3.070015318549076166, -0.4124855346667993805 ) ) ;
#48627 = CARTESIAN_POINT ( 'NONE',  ( 6.069229152942410721, 0.1638285306290178100, -2.155560115052157055 ) ) ;
#48628 = CARTESIAN_POINT ( 'NONE',  ( -2.788173145904702555, 6.404619103530779789, -0.7998128361456281477 ) ) ;
#48629 = CARTESIAN_POINT ( 'NONE',  ( -7.199016378732087773, 7.501199984716642177, 0.7216878364870317197 ) ) ;
#48630 = CARTESIAN_POINT ( 'NONE',  ( 5.489210439962995736, 1.908424935776025455, -1.015307555102950010 ) ) ;
#48632 = EDGE_LOOP ( 'NONE', ( #92468, #51733 ) ) ;
#48631 = CARTESIAN_POINT ( 'NONE',  ( -7.720982897393583677, -9.999999999999994671, 7.834948825496934610 ) ) ;
#48633 = CARTESIAN_POINT ( 'NONE',  ( -1.364683531250012516, 2.780208333674754506, 0.7879004041258379498 ) ) ;
#48634 = CARTESIAN_POINT ( 'NONE',  ( 5.589129042188730523, 1.739749244469630529, -0.9270521019464451618 ) ) ;
#48635 = CARTESIAN_POINT ( 'NONE',  ( 4.727759377455642564, -1.549208768551156190, -0.7787371415562751586 ) ) ;
#48637 = CARTESIAN_POINT ( 'NONE',  ( 1.417800074541092137, -1.221294057239637576, -1.819523406426680090 ) ) ;
#48636 = CARTESIAN_POINT ( 'NONE',  ( -0.6801582343750213200, -1.067708332991926135, 1.178068619123832983 ) ) ;
#48638 = CARTESIAN_POINT ( 'NONE',  ( 2.907580275951544113, 1.948851909871853749, 1.235431545971882095 ) ) ;
#48639 = CARTESIAN_POINT ( 'NONE',  ( 4.956353021003493176, 0.7848952607251434843, 1.905660951107574608 ) ) ;
#48640 = CARTESIAN_POINT ( 'NONE',  ( 0.7439598490389126573, 0.5628818913385369438, 1.858577368155549525 ) ) ;
#48641 = CARTESIAN_POINT ( 'NONE',  ( -6.277061933002790362, 8.346324893301817482, 1.443375672974078761 ) ) ;
#48642 = CARTESIAN_POINT ( 'NONE',  ( -5.666381855868691808, 5.575476684793721383, 0.000000000000000000 ) ) ;
#48643 = CARTESIAN_POINT ( 'NONE',  ( -0.4644097342743139234, -8.233137084989849086, -9.488641820551089623 ) ) ;
#48644 = EDGE_CURVE ( 'NONE', #80951, #80427, #148123, .T. ) ;
#48645 = CARTESIAN_POINT ( 'NONE',  ( 4.324552338190708056, -0.9094542848507057853, -1.915842285305848769 ) ) ;
#48646 = CYLINDRICAL_SURFACE ( 'NONE', #139951, 11.00000000000000000 ) ;
#48647 = CARTESIAN_POINT ( 'NONE',  ( 1.494767762416524093, -2.000856930885573259, 0.2496086726550551249 ) ) ;
#48648 = CARTESIAN_POINT ( 'NONE',  ( -5.043269954159181445, 8.827639346586952485, 1.214306433183764966E-14 ) ) ;
#48649 = CARTESIAN_POINT ( 'NONE',  ( 4.612475435721691497, -0.9401552641563456492, -1.996616816212187340 ) ) ;
#48650 = CARTESIAN_POINT ( 'NONE',  ( 3.285556943749998737, -0.6927083328553748087, -1.896917185911906500 ) ) ;
#48651 = CARTESIAN_POINT ( 'NONE',  ( -11.80248046418316044, 12.29999999999998295, 1.695421849633139466 ) ) ;
#48652 = CARTESIAN_POINT ( 'NONE',  ( -5.576146316970437944, 9.727530813099326323, 0.000000000000000000 ) ) ;
#48653 = CARTESIAN_POINT ( 'NONE',  ( -5.492869780704572769, 7.580512000422499952, -1.348893862496753249 ) ) ;
#48654 = DIRECTION ( 'NONE',  ( 0.000000000000000000, -1.000000000000000000, 0.000000000000000000 ) ) ;
#48655 = ORIENTED_EDGE ( 'NONE', *, *, #7876, .F. ) ;
#48656 = CARTESIAN_POINT ( 'NONE',  ( 4.205972405791720270, -2.055509729078345948, 0.1495927064073861168 ) ) ;
#48657 = DIRECTION ( 'NONE',  ( 1.000000000000000000, 0.000000000000000000, 0.000000000000000000 ) ) ;
#48658 = UNCERTAINTY_MEASURE_WITH_UNIT (LENGTH_MEASURE( 1.000000000000000082E-05 ), #131175, 'distance_accuracy_value', 'NONE');
#48659 = DIRECTION ( 'NONE',  ( 0.000000000000000000, 1.000000000000000000, 0.000000000000000000 ) ) ;
#48660 = CARTESIAN_POINT ( 'NONE',  ( -4.554649539187067830, 7.401175998105142817, 1.199719254218464037 ) ) ;
#48661 = CARTESIAN_POINT ( 'NONE',  ( 2.965494806321045562, -1.652366046825021417, -1.161084516292823832 ) ) ;
#48662 = CARTESIAN_POINT ( 'NONE',  ( -0.7500000000000249800, -0.05833333333331303105, 1.299038105676659116 ) ) ;
#48663 = CARTESIAN_POINT ( 'NONE',  ( 10.41229878561526512, 11.25002945941372623, -0.7216878364870257245 ) ) ;
#48664 = CARTESIAN_POINT ( 'NONE',  ( 6.259060471003163428, 10.45398764947904624, -0.7998128361456291469 ) ) ;
#48665 = CARTESIAN_POINT ( 'NONE',  ( 3.327077596220921141, 0.04893577929474152155, 2.060475874978876298 ) ) ;
#48666 = EDGE_CURVE ( 'NONE', #34325, #4753, #112780, .T. ) ;
#48667 = CARTESIAN_POINT ( 'NONE',  ( 5.789495288235341874, 6.713164910151406595, 1.199719254218462483 ) ) ;
#48668 = CARTESIAN_POINT ( 'NONE',  ( -0.1408020194050146334, 2.009929383927198998, -2.515281701100045009 ) ) ;
#48669 = CARTESIAN_POINT ( 'NONE',  ( 0.9020086522944226193, 1.395640307904035593, -1.200911154268270664 ) ) ;
#48670 = CARTESIAN_POINT ( 'NONE',  ( 0.1007806894988797913, -2.307328790448114120, -0.04970016441883937791 ) ) ;
#48671 = CARTESIAN_POINT ( 'NONE',  ( 4.715203562502613188, 8.723097599553565118, 0.7998128361456341429 ) ) ;
#48672 = CARTESIAN_POINT ( 'NONE',  ( 2.829541668879275829, -2.018026287816252040, 0.7751260729957698548 ) ) ;
#48673 = CARTESIAN_POINT ( 'NONE',  ( -2.982430605326328532, 5.462957558647244305, -1.082531754730543971 ) ) ;
#48674 = B_SPLINE_CURVE_WITH_KNOTS ( 'NONE', 3,
 ( #76508, #42980, #138329, #8307, #60261, #157783, #171884, #57070, #172968, #74391, #88514, #142619, #204345, #25620, #22405, #89588, #9381, #191312, #140492, #41910, #206503, #158839, #75452 ),
 .UNSPECIFIED., .F., .F.,
 ( 4, 2, 2, 2, 2, 2, 2, 2, 2, 1, 2, 4 ),
 ( 0.2533959729413839401, 0.2675222111384283896, 0.2816484493354728391, 0.2957746875325172331, 0.3099009257295616826, 0.3240271639266061321, 0.3381534021236505816, 0.3452165212221727786, 0.3469823009968033278, 0.3487480807714339326, 0.3522796403206950311, 0.3664058785177394806 ),
 .UNSPECIFIED. ) ;
#48675 = CARTESIAN_POINT ( 'NONE',  ( 1.973842561262352469, -0.8578407463649927456, 1.825077436249371354 ) ) ;
#48676 = CARTESIAN_POINT ( 'NONE',  ( 2.566106820329843163, 1.847058390165011721, -1.367687711909180148 ) ) ;
#48677 = CARTESIAN_POINT ( 'NONE',  ( 0.3399812269560758549, 3.243416237969932503, -2.042960595231173571 ) ) ;
#48678 = CARTESIAN_POINT ( 'NONE',  ( 0.5845639792326964290, -0.2246964894469481722, -1.857040431621145959 ) ) ;
#48679 = CIRCLE ( 'NONE', #31517, 0.07999999999999975187 ) ;
#48680 = CARTESIAN_POINT ( 'NONE',  ( 4.979350729014382360, 1.839849877434216241, -0.7087157093622028503 ) ) ;
#48681 = CARTESIAN_POINT ( 'NONE',  ( 4.346888830327386266, -1.803415170841724979, -0.9023466997552240798 ) ) ;
#48683 = CARTESIAN_POINT ( 'NONE',  ( 9.693716643646590470, 12.33242205571964512, 1.443375672974076540 ) ) ;
#48682 = CARTESIAN_POINT ( 'NONE',  ( -1.364683531250000748, 2.009375000341421913, 1.214306433183764966E-14 ) ) ;
#48685 = CARTESIAN_POINT ( 'NONE',  ( 6.182269030498733997, -1.128069697684991546, 1.778281062836915449 ) ) ;
#48684 = CARTESIAN_POINT ( 'NONE',  ( -5.876569516519495551, 8.943415971659659292, 1.199719254218452047 ) ) ;
#48686 = EDGE_CURVE ( 'NONE', #79641, #111999, #7610, .T. ) ;
#48687 = CARTESIAN_POINT ( 'NONE',  ( 6.021949436824264978, 2.040384406434097464, -0.3501103912618847014 ) ) ;
#48688 = CARTESIAN_POINT ( 'NONE',  ( 4.971035877704902184, 8.951292290631053916, 1.040834085586084257E-14 ) ) ;
#48689 = CARTESIAN_POINT ( 'NONE',  ( -5.391338639728555648, 9.441645512991978961, -0.7998128361456231517 ) ) ;
#48690 = CARTESIAN_POINT ( 'NONE',  ( 6.539320575229236709, 1.252639605590207150, 2.218328189723097754 ) ) ;
#48691 = CARTESIAN_POINT ( 'NONE',  ( -0.05226516427493665962, -1.936187138999283297, 0.8653993394739032397 ) ) ;
#48692 = CARTESIAN_POINT ( 'NONE',  ( -1.402160292154681736E-14, -0.006249999317184824418, 1.732050807568877637 ) ) ;
#48693 = CARTESIAN_POINT ( 'NONE',  ( 3.791899867668945490, 1.670594791088287678, 1.592266751676748582 ) ) ;
#48694 = EDGE_CURVE ( 'NONE', #85130, #60185, #84656, .T. ) ;
#48695 = CARTESIAN_POINT ( 'NONE',  ( 2.395447240195498484, -1.844268472375994339, 0.9235843863054800096 ) ) ;
#48696 = CARTESIAN_POINT ( 'NONE',  ( 7.944714827928050838, 9.331550723079971021, 1.082531754730558626 ) ) ;
#48697 = CARTESIAN_POINT ( 'NONE',  ( 7.018280793729500644, 8.217024343219755167, -1.199719254218452047 ) ) ;
#48698 = CARTESIAN_POINT ( 'NONE',  ( 6.873057527484919937, 6.983264968346048818, 0.7998128361456352531 ) ) ;
#48699 = CARTESIAN_POINT ( 'NONE',  ( -1.402160292154681736E-14, 0.3843750003414230232, 1.575800808251672791 ) ) ;
#48700 = CARTESIAN_POINT ( 'NONE',  ( 3.379725431556547477, 7.165039780116438273, -1.734723475976807094E-15 ) ) ;
#48701 = CARTESIAN_POINT ( 'NONE',  ( 5.612712405933139692, 9.491988873656591608, 1.040834085586084257E-14 ) ) ;
#48702 = CARTESIAN_POINT ( 'NONE',  ( 4.598189031992506948, 0.9324077545292840385, -1.960920063828344384 ) ) ;
#48703 = CARTESIAN_POINT ( 'NONE',  ( 0.2999999999999860556, 4.000000000000010658, 1.007084189318397938 ) ) ;
#48705 = CARTESIAN_POINT ( 'NONE',  ( 3.368544699895597461, 0.04196216268675251326, -1.840931771443871101 ) ) ;
#48704 = CARTESIAN_POINT ( 'NONE',  ( -4.663641653420935285, 5.503632019488245319, 1.082531754730560403 ) ) ;
#48706 = CARTESIAN_POINT ( 'NONE',  ( -1.201851678989727383E-14, 4.446875000341417916, -1.575800808251660134 ) ) ;
#48707 = CARTESIAN_POINT ( 'NONE',  ( 4.370767597569780172, -0.0006098066561242150270, -2.191739723162715592 ) ) ;
#48708 = CARTESIAN_POINT ( 'NONE',  ( 8.776224899084642317, 13.27471476138782691, 8.184001253707560153 ) ) ;
#48709 = CARTESIAN_POINT ( 'NONE',  ( 5.524405971769074775, 1.352560167130362867, -1.813582142078016712 ) ) ;
#48710 = CARTESIAN_POINT ( 'NONE',  ( -5.927203485463973465, 6.129067544638190590, -0.8144944673919730649 ) ) ;
#48711 = CARTESIAN_POINT ( 'NONE',  ( 5.420206975164616026, 7.644856803259713729, 1.330009527941821368 ) ) ;
#48712 = VECTOR ( 'NONE', #27700, 1000.000000000000000 ) ;
#48713 = CARTESIAN_POINT ( 'NONE',  ( -4.624739795592931912, 8.409630504918133909, -0.7216878364870338292 ) ) ;
#48714 = CARTESIAN_POINT ( 'NONE',  ( 4.068855497876973537, 7.761098824249525130, -0.7216878364870338292 ) ) ;
#48715 = CARTESIAN_POINT ( 'NONE',  ( 6.626229037604012717, 1.016508351997437165, -1.448449474740549858 ) ) ;
#48716 = CARTESIAN_POINT ( 'NONE',  ( 3.738934858379244552, 1.912307379442554689, 0.6292302551485791096 ) ) ;
#48717 = CARTESIAN_POINT ( 'NONE',  ( 6.958359152311676787, 9.141171649162195934, -1.599625672291262513 ) ) ;
#48718 = CARTESIAN_POINT ( 'NONE',  ( 2.907361098931018795, 1.778370309693329210, 1.127733957892971484 ) ) ;
#48719 = CARTESIAN_POINT ( 'NONE',  ( 2.636237813805066388, 0.6479696587880221514, 1.802806680411846774 ) ) ;
#48720 = CARTESIAN_POINT ( 'NONE',  ( 3.225950485047770933, 5.851027101609320269, 1.199719254218450271 ) ) ;
#48721 = CARTESIAN_POINT ( 'NONE',  ( 3.525798893484650254, 1.922080780809858114, -0.4290687576708405726 ) ) ;
#48722 = CARTESIAN_POINT ( 'NONE',  ( 4.957288421310242832, -1.730244549199685400, 1.041802906739682566 ) ) ;
#48723 = CARTESIAN_POINT ( 'NONE',  ( 0.4966798268824790252, 1.557709316500059726, -1.035497600327957235 ) ) ;
#48724 = CARTESIAN_POINT ( 'NONE',  ( 1.521847698614446687, 1.933392594956625521, -0.3320675068423510345 ) ) ;
#48726 = EDGE_LOOP ( 'NONE', ( #100794, #43159, #173613, #134539, #53544 ) ) ;
#48725 = CARTESIAN_POINT ( 'NONE',  ( 0.4395310841842986482, -1.815173276516975243, 0.6020934215927520317 ) ) ;
#48727 = CARTESIAN_POINT ( 'NONE',  ( 4.202664430556241726, 7.846932902383524144, 0.7216878364870298324 ) ) ;
#48728 = VECTOR ( 'NONE', #166049, 1000.000000000000000 ) ;
#48729 = CARTESIAN_POINT ( 'NONE',  ( 0.6823417656249882723, 0.1552083336747514530, 1.181850606188755259 ) ) ;
#48730 = CARTESIAN_POINT ( 'NONE',  ( 6.649288223980675205, -1.503899034092891940, -1.112267350887645945 ) ) ;
#48731 = CARTESIAN_POINT ( 'NONE',  ( 4.376584659113025744, 4.000436945253625254, 0.7998128361456341429 ) ) ;
#48732 = DIRECTION ( 'NONE',  ( 0.000000000000000000, 1.000000000000000000, 0.000000000000000000 ) ) ;
#48733 = CARTESIAN_POINT ( 'NONE',  ( 6.455931442665615805, -0.7031469350025701948, 1.947301169641938223 ) ) ;
#48734 = CARTESIAN_POINT ( 'NONE',  ( 0.7499999999999902300, 3.764583334016149863, 1.299038105676669330 ) ) ;
#48735 = CARTESIAN_POINT ( 'NONE',  ( 0.9419464005683108043, 1.389173191389100337, 1.535309223701806447 ) ) ;
#48736 = CARTESIAN_POINT ( 'NONE',  ( 0.7499999999999902300, 1.233333333333357151, 1.299038105676657340 ) ) ;
#48737 = CARTESIAN_POINT ( 'NONE',  ( 7.019370843573166319, 9.212351955633947043, 1.599625672291281386 ) ) ;
#48738 = CARTESIAN_POINT ( 'NONE',  ( -7.340850106795412167, 10.65174332698158643, 1.199719254218453823 ) ) ;
#48739 = CARTESIAN_POINT ( 'NONE',  ( 5.876533236880477240, 5.820653295974182129, 0.7998128361456352531 ) ) ;
#48740 = CARTESIAN_POINT ( 'NONE',  ( 5.215537505735290402, 1.733765862324820439, 1.220609238144418240 ) ) ;
#48741 = CARTESIAN_POINT ( 'NONE',  ( 4.411198876399872404, 6.239761003923544713, -1.599625672291273171 ) ) ;
#48742 = CARTESIAN_POINT ( 'NONE',  ( -1.364683531250000748, 0.7593750003414210248, 0.000000000000000000 ) ) ;
#48743 = EDGE_LOOP ( 'NONE', ( #180060, #21988, #85250 ) ) ;
#48744 = CARTESIAN_POINT ( 'NONE',  ( -1.500000000000013101, 1.920833333333356263, 0.8660254037844403729 ) ) ;
#48746 = CARTESIAN_POINT ( 'NONE',  ( 4.684505768721569652, 5.424010470718658716, -1.199719254218452047 ) ) ;
#48745 = CARTESIAN_POINT ( 'NONE',  ( 6.039501783790233169, 1.813256598412491982, -0.7494862575098264479 ) ) ;
#48747 = CARTESIAN_POINT ( 'NONE',  ( 4.464220131058834085, 1.617570847575640736, 1.203168917025834839 ) ) ;
#48748 = CARTESIAN_POINT ( 'NONE',  ( 3.292102688380782460, -0.7811219226253396375, -1.749442990535796438 ) ) ;
#48749 = DIRECTION ( 'NONE',  ( 0.000000000000000000, 1.000000000000000000, 0.000000000000000000 ) ) ;
#48750 = CARTESIAN_POINT ( 'NONE',  ( 1.470551405592795957, -2.082434148983134392, -0.6831980896230758216 ) ) ;
#48751 = SPHERICAL_SURFACE ( 'NONE', #83893, 0.08000000000000000167 ) ;
#48752 = CARTESIAN_POINT ( 'NONE',  ( 3.180766902908559235, -0.1340872481324743570, -1.865776598943262199 ) ) ;
#48753 = CARTESIAN_POINT ( 'NONE',  ( -1.500000000000015099, -1.089583332650509773, -0.8660254037844383745 ) ) ;
#48754 = CARTESIAN_POINT ( 'NONE',  ( -5.357443255694392725, 9.402100898285455699, 0.000000000000000000 ) ) ;
#48756 = CARTESIAN_POINT ( 'NONE',  ( 5.150072296613558365, 1.044590698784592542, 1.841551053096659230 ) ) ;
#48755 = CARTESIAN_POINT ( 'NONE',  ( -4.500943810056945438, 5.313817868896925312, 1.082531754730560403 ) ) ;
#48757 = CARTESIAN_POINT ( 'NONE',  ( 1.364683531249996529, 8.776041667008067648, 0.7879004041258405033 ) ) ;
#48758 = B_SPLINE_CURVE_WITH_KNOTS ( 'NONE', 3,
 ( #173917, #96669, #65177, #64143, #212502, #208492 ),
 .UNSPECIFIED., .F., .F.,
 ( 4, 2, 4 ),
 ( 0.000000000000000000, 0.0003767643964918267023, 0.0007535287929836531878 ),
 .UNSPECIFIED. ) ;
#48760 = CARTESIAN_POINT ( 'NONE',  ( -7.767895665986912057, 8.027242796598338614, -0.7998128361456362523 ) ) ;
#48759 = CARTESIAN_POINT ( 'NONE',  ( 1.821934285652214935, 1.201201420651318630, -1.711045060523497030 ) ) ;
#48762 = ORIENTED_EDGE ( 'NONE', *, *, #86749, .F. ) ;
#48761 = CARTESIAN_POINT ( 'NONE',  ( 0.3930057192131968802, 1.272852841813755687, 1.164116782529129868 ) ) ;
#48763 = CARTESIAN_POINT ( 'NONE',  ( 6.612626235163189925, 8.737816579155630592, -1.599625672291262513 ) ) ;
#48764 = CARTESIAN_POINT ( 'NONE',  ( 0.09263630470259102967, -10.00000000000047251, 9.579493439010624556 ) ) ;
#48765 = CARTESIAN_POINT ( 'NONE',  ( -0.3602790413719305640, -9.063128419003716019, 9.630430012830167641 ) ) ;
#48767 = CARTESIAN_POINT ( 'NONE',  ( 10.01911233037458260, 10.79131192829960462, 0.7216878364870438212 ) ) ;
#48766 = CARTESIAN_POINT ( 'NONE',  ( 6.440286661691305703, 7.472421512516709718, 1.199719254218462483 ) ) ;
#48768 = CARTESIAN_POINT ( 'NONE',  ( -1.500000000000039524, 7.000000000000000000, -10.89724735885167739 ) ) ;
#48770 = CARTESIAN_POINT ( 'NONE',  ( 1.224954274949443978, 1.597400116765529843, 0.8541874478597778486 ) ) ;
#48769 = CARTESIAN_POINT ( 'NONE',  ( 5.448397627845284141, 7.449826213943242514, 1.599625672291268286 ) ) ;
#48771 = CARTESIAN_POINT ( 'NONE',  ( -7.531718027591449705, 8.745758106066849891, 1.199719254218462483 ) ) ;
#48772 = AXIS2_PLACEMENT_3D ( 'NONE', #155761, #107063, #90775 ) ;
#48773 = CARTESIAN_POINT ( 'NONE',  ( 3.655894977179307226, 7.416961240017848844, -0.7998128361456291469 ) ) ;
#48774 = CARTESIAN_POINT ( 'NONE',  ( 4.362691568547328202, 8.311833606605697256, -0.7998128361456381397 ) ) ;
#48775 = CARTESIAN_POINT ( 'NONE',  ( 6.539320575229254473, 0.5926322452488984593, 1.950287522085321301 ) ) ;
#48776 = AXIS2_PLACEMENT_3D ( 'NONE', #148240, #29148, #132021 ) ;
#48777 = CARTESIAN_POINT ( 'NONE',  ( 4.055251984284337752, 7.519160923078652026, -0.4935718261673445184 ) ) ;
#48778 = CARTESIAN_POINT ( 'NONE',  ( 9.300530189294644146, 10.91333531134101165, -1.082531754730543083 ) ) ;
#48779 = EDGE_LOOP ( 'NONE', ( #11059, #29459, #135432, #213429 ) ) ;
#48780 = CARTESIAN_POINT ( 'NONE',  ( 3.367479257110431945, -0.3654178573793941398, 1.824635806631241808 ) ) ;
#48781 = CARTESIAN_POINT ( 'NONE',  ( 0.2455189486357247652, 1.894654674652377135, -0.2817335493821241932 ) ) ;
#48782 = CARTESIAN_POINT ( 'NONE',  ( 6.458035534591947346, 1.921153000004784284, -0.1426463852419664891 ) ) ;
#48783 = CARTESIAN_POINT ( 'NONE',  ( 6.795378861676105053, -1.851214886592133846, 0.9271815693319698237 ) ) ;
#48784 = CARTESIAN_POINT ( 'NONE',  ( -7.334597915313094241, 9.580116872663850813, 1.040834085586084257E-14 ) ) ;
#48785 = CARTESIAN_POINT ( 'NONE',  ( 4.771497086726927073, 8.161215468402982509, 0.7801120568680236511 ) ) ;
#48786 = CARTESIAN_POINT ( 'NONE',  ( 11.48243876534946217, 9.719999999999998863, -3.200000000000001510 ) ) ;
#48787 = CARTESIAN_POINT ( 'NONE',  ( 8.107412671292031803, 11.44210330227398487, 1.082531754730557072 ) ) ;
#48788 = CARTESIAN_POINT ( 'NONE',  ( 4.504722179138310523, 0.5213129852876841053, 1.899149332505256638 ) ) ;
#48789 = CARTESIAN_POINT ( 'NONE',  ( 1.559403367407938390, -1.789607135292633266, 1.137164086494051096 ) ) ;
#48790 = CARTESIAN_POINT ( 'NONE',  ( -4.232116505760120440, 8.089219690028791376, -0.7998128361456281477 ) ) ;
#48791 = CARTESIAN_POINT ( 'NONE',  ( -10.79708633470181134, 6.390220175058726859, -5.149361723773914434 ) ) ;
#48792 = CARTESIAN_POINT ( 'NONE',  ( 5.560252395380215873, 6.619954228432645138, 1.082531754730549078 ) ) ;
#48793 = CARTESIAN_POINT ( 'NONE',  ( 6.263654578238285531, 1.123272483274835087, 1.881548979392036802 ) ) ;
#48794 = LINE ( 'NONE', #114911, #174693 ) ;
#48795 = CARTESIAN_POINT ( 'NONE',  ( 4.172816426537079515, -1.797186248846779133, -0.6940461778226751921 ) ) ;
#48796 = CARTESIAN_POINT ( 'NONE',  ( -6.938021921891187382, 9.117444880338284818, -1.599625672291263179 ) ) ;
#48797 = CARTESIAN_POINT ( 'NONE',  ( 0.9267433102794274680, 1.311770220233858586, -1.774563083084364834 ) ) ;
#48798 = DIRECTION ( 'NONE',  ( 0.7592566023653010143, -0.6507913734559633845, -5.900213523162838665E-32 ) ) ;
#48799 = CARTESIAN_POINT ( 'NONE',  ( 0.2285749388857594433, 1.317234250586714284, -1.386657971642536014 ) ) ;
#48800 =( BOUNDED_SURFACE ( )  B_SPLINE_SURFACE ( 3, 2, ( 
 ( #186430, #168066, #85743 ),
 ( #5521, #87880, #151827 ),
 ( #23926, #38069, #153953 ),
 ( #71601, #152878, #137710 ),
 ( #203732, #122609, #121533 ),
 ( #187503, #19666, #135575 ),
 ( #105215, #171253, #6602 ),
 ( #72683, #52183, #138778 ) ),
 .UNSPECIFIED., .F., .F., .T. ) 
 B_SPLINE_SURFACE_WITH_KNOTS ( ( 4, 2, 2, 4 ),
 ( 3, 3 ),
 ( 0.000000000000000000, 0.0002568729646053923097, 0.0005137459292107846194, 0.001027491858421569239 ),
 ( 0.000000000000000000, 1.000000000000000000 ),
 .UNSPECIFIED. ) 
 GEOMETRIC_REPRESENTATION_ITEM ( )  RATIONAL_B_SPLINE_SURFACE ( (
 ( 1.000000000000000000, 0.3826834323651035485, 1.000000000000000000),
 ( 1.000000000000000000, 0.3847114443836440745, 1.000000000000000000),
 ( 1.000000000000000000, 0.4039255759072567509, 1.000000000000000000),
 ( 1.000000000000000000, 0.4557194474498202919, 1.000000000000000000),
 ( 1.000000000000000000, 0.4874388927522833037, 1.000000000000000000),
 ( 1.000000000000000000, 0.5833547384518390500, 1.000000000000000000),
 ( 1.000000000000000000, 0.6470545345835431172, 1.000000000000000000),
 ( 1.000000000000000000, 0.7045118851637689472, 1.000000000000000000) ) ) 
 REPRESENTATION_ITEM ( '' )  SURFACE ( )  );
#48801 = ORIENTED_EDGE ( 'NONE', *, *, #211272, .T. ) ;
#48802 = ORIENTED_EDGE ( 'NONE', *, *, #155697, .F. ) ;
#48803 = CARTESIAN_POINT ( 'NONE',  ( 6.034039001082764919, 1.170257472284089717, 1.583912470002272199 ) ) ;
#48804 = CARTESIAN_POINT ( 'NONE',  ( 1.241630701082994559, 1.939900434848752964, 0.09377332689292780521 ) ) ;
#48805 = CARTESIAN_POINT ( 'NONE',  ( 6.626320313634256109, 0.4032262605214493312, -2.262638539848499164 ) ) ;
#48807 = CARTESIAN_POINT ( 'NONE',  ( 5.647250314520869452, 1.642094101250504146, -0.8754911610409812361 ) ) ;
#48806 = CARTESIAN_POINT ( 'NONE',  ( -5.420227550413282636, 9.545625585449309725, 0.7998128361456291469 ) ) ;
#48808 = CARTESIAN_POINT ( 'NONE',  ( 5.956828388357757298, 8.042995434541133193, 1.599625672291269396 ) ) ;
#48809 = SURFACE_STYLE_USAGE ( .BOTH. , #114926 ) ;
#48810 = LINE ( 'NONE', #47767, #8420 ) ;
#48811 = CARTESIAN_POINT ( 'NONE',  ( -6.878064000834399394, 6.918829510595249310, -0.7998128361456291469 ) ) ;
#48812 = CARTESIAN_POINT ( 'NONE',  ( -3.197123283245616676, -0.9841229182759280159, 1.361626862150112860 ) ) ;
#48813 = CARTESIAN_POINT ( 'NONE',  ( 1.558417602779540889, -1.546676288433556756, 1.552911753681482487 ) ) ;
#48814 = CARTESIAN_POINT ( 'NONE',  ( 4.202664430556247055, 6.886563688082179446, 1.082531754730558626 ) ) ;
#48815 = EDGE_CURVE ( 'NONE', #145242, #67222, #202157, .T. ) ;
#48816 = CARTESIAN_POINT ( 'NONE',  ( 10.86152993230179220, -6.808378554901793223, -0.3183146091066044736 ) ) ;
#48817 = DIRECTION ( 'NONE',  ( 1.000000000000000000, 0.000000000000000000, 0.000000000000000000 ) ) ;
#48818 = CARTESIAN_POINT ( 'NONE',  ( 1.453431991042982041, 0.5316948868413253759, -1.746555546766684675 ) ) ;
#48819 = CARTESIAN_POINT ( 'NONE',  ( 1.408489644581676137, 7.311701683604759694, 4.382268911472973372 ) ) ;
#48820 = CARTESIAN_POINT ( 'NONE',  ( -0.1054627972275563597, 3.385846599571565640, -2.076146368081344118 ) ) ;
#48821 = CARTESIAN_POINT ( 'NONE',  ( 6.609000000000005315, 2.959011640422835487, 2.552823073452652913 ) ) ;
#48822 = CARTESIAN_POINT ( 'NONE',  ( 9.836604141914616406, 11.43479190611061647, 1.199719254218452047 ) ) ;
#48823 = CARTESIAN_POINT ( 'NONE',  ( 6.340460056601358474, 1.806591233369018834, 0.2625940548972791611 ) ) ;
#48824 = CARTESIAN_POINT ( 'NONE',  ( 4.399235598239510381, -1.708881994454291675, 0.9632455365647660805 ) ) ;
#48825 = ADVANCED_FACE ( 'NONE', ( #14112 ), #78070, .F. ) ;
#48826 = CARTESIAN_POINT ( 'NONE',  ( -8.853638004923878313, 10.28799807962136548, 1.199719254218462483 ) ) ;
#48827 = CARTESIAN_POINT ( 'NONE',  ( 5.178324605415663306, 8.128796908705222535, 1.199719254218462483 ) ) ;
#48828 = CARTESIAN_POINT ( 'NONE',  ( 4.899148033862871898, -0.2601683324335196668, -2.104413843559429065 ) ) ;
#48829 = CARTESIAN_POINT ( 'NONE',  ( 3.632539538618652752, 0.3231117836275976818, 2.167502126216628522 ) ) ;
#48830 = EDGE_CURVE ( 'NONE', #191645, #138616, #21354, .T. ) ;
#48831 = CARTESIAN_POINT ( 'NONE',  ( 3.811813743736467419, 7.598866467667865443, 1.040834085586084257E-14 ) ) ;
#48832 = CARTESIAN_POINT ( 'NONE',  ( 3.168866831888625946, 1.502704456927813403, -1.424286459396295390 ) ) ;
#48834 = CARTESIAN_POINT ( 'NONE',  ( -0.6823417656250246877, -0.1364583329919108468, 1.181850606188755259 ) ) ;
#48833 = LINE ( 'NONE', #147401, #96268 ) ;
#48835 = EDGE_LOOP ( 'NONE', ( #177561, #123838 ) ) ;
#48836 = CARTESIAN_POINT ( 'NONE',  ( 3.164923336591000336, 1.459680849325554197, 1.775737417650694816 ) ) ;
#48837 = CARTESIAN_POINT ( 'NONE',  ( 8.270110514656026979, 10.67154823856396817, 1.443375672974076540 ) ) ;
#48839 = CARTESIAN_POINT ( 'NONE',  ( 0.000000000000000000, -1.246874999522042948, -3.793834371823813001 ) ) ;
#48838 = CARTESIAN_POINT ( 'NONE',  ( 6.753369913382843315, 8.011924666102361314, -1.082531754730548412 ) ) ;
#48840 = CARTESIAN_POINT ( 'NONE',  ( 6.720655732516647163, 0.005566325962592238996, 1.826293863978686982 ) ) ;
#48841 = CARTESIAN_POINT ( 'NONE',  ( -10.41369770442025633, 5.038847794253626944, -5.873885783557990514 ) ) ;
#48842 = CARTESIAN_POINT ( 'NONE',  ( 3.257691520677992614, 0.8739490649069777684, 1.734254922796226506 ) ) ;
#48843 = VERTEX_POINT ( 'NONE', #13056 ) ;
#48844 = LINE ( 'NONE', #160453, #198090 ) ;
#48845 = EDGE_CURVE ( 'NONE', #197321, #118044, #160773, .T. ) ;
#48846 = CARTESIAN_POINT ( 'NONE',  ( 4.341997288149157086, -1.180789491531178292, -1.504210074635865757 ) ) ;
#48847 = FACE_OUTER_BOUND ( 'NONE', #160446, .T. ) ;
#48848 = CARTESIAN_POINT ( 'NONE',  ( 5.385687109042746279, 1.161108558237003985, 1.275598767315838211 ) ) ;
#48849 = CARTESIAN_POINT ( 'NONE',  ( 3.274625289317079524, -0.3981104328964027994, -1.976669913042613747 ) ) ;
#48850 = CARTESIAN_POINT ( 'NONE',  ( 5.344470762249110329, 0.4509167475243852086, -2.253899259558800772 ) ) ;
#48851 = CARTESIAN_POINT ( 'NONE',  ( -0.4577034257980932552, -0.8887487162305418575, -3.253519940713586855 ) ) ;
#48852 = CARTESIAN_POINT ( 'NONE',  ( 0.9970219447392356660, -0.5395372827587068265, -2.139793933917451874 ) ) ;
#48853 = CARTESIAN_POINT ( 'NONE',  ( -3.987506576194992824, 7.666191748953863794, 0.7216878364870338292 ) ) ;
#48854 = CARTESIAN_POINT ( 'NONE',  ( 5.800005483916761406, -1.769921774263127912, 0.001416880316495658159 ) ) ;
#48856 = CARTESIAN_POINT ( 'NONE',  ( 1.904612379804408118, 1.696638126304336858, -1.541566781129146912 ) ) ;
#48855 = CARTESIAN_POINT ( 'NONE',  ( 5.845500506147374153, 6.848780674373954547, 1.199719254218453823 ) ) ;
#48857 = CARTESIAN_POINT ( 'NONE',  ( 0.7084657485305994040, -0.2594935844701939387, 1.720731466566546519 ) ) ;
#48858 = CARTESIAN_POINT ( 'NONE',  ( 0.4839601414735513196, 4.104060063207238152, -0.4353502767700700438 ) ) ;
#48859 = STYLED_ITEM ( 'NONE', ( #18886 ), #171225 ) ;
#48860 = CARTESIAN_POINT ( 'NONE',  ( -7.075376061485238566, 9.347967719856493218, 1.599625672291269396 ) ) ;
#48861 = CARTESIAN_POINT ( 'NONE',  ( -0.6801582343750334214, 0.3802083336747336118, -1.178068619123869398 ) ) ;
#48862 = CARTESIAN_POINT ( 'NONE',  ( 1.016456843292303031E-15, 0.2000000000000057288, -8.300000000000000711 ) ) ;
#48863 = CARTESIAN_POINT ( 'NONE',  ( 1.364001086256797945, -0.5279541034660294452, 2.105878793243611824 ) ) ;
#48864 = CARTESIAN_POINT ( 'NONE',  ( 2.413296319342159713, -1.879803466158457059, 0.7303082167480907660 ) ) ;
#48865 = CARTESIAN_POINT ( 'NONE',  ( -1.500000000000013101, 0.7020833340161545255, 0.8660254037844403729 ) ) ;
#48866 = CARTESIAN_POINT ( 'NONE',  ( 5.637312448503878137, -1.740617781635974248, 0.8259078106758013238 ) ) ;
#48867 = CARTESIAN_POINT ( 'NONE',  ( -1.364683531250010295, 12.88020833367473372, 0.7879004041258445001 ) ) ;
#48868 = CARTESIAN_POINT ( 'NONE',  ( 2.602056794214495650, 1.574129494629309622, 1.567664267292529612 ) ) ;
#48869 = ORIENTED_EDGE ( 'NONE', *, *, #1922, .F. ) ;
#48870 = CARTESIAN_POINT ( 'NONE',  ( -2.353140975214501829, 2.704741401632028808, 2.456000212125921678 ) ) ;
#48871 = CARTESIAN_POINT ( 'NONE',  ( 9.185812768458653466, 10.67553530374532045, 1.199719254218453823 ) ) ;
#48872 = SURFACE_SIDE_STYLE ('',( #164743 ) ) ;
#48873 = CARTESIAN_POINT ( 'NONE',  ( 5.407646374456077432, -0.7895141955979433357, -1.551160667784831748 ) ) ;
#48875 = CARTESIAN_POINT ( 'NONE',  ( 3.103904542773823660, 0.7086415210641981988, -1.829580771271981154 ) ) ;
#48874 = CIRCLE ( 'NONE', #114636, 1.914481421317578258 ) ;
#48877 = CARTESIAN_POINT ( 'NONE',  ( -5.883875478650828050, 9.808345791827219884, 0.7216878364870458196 ) ) ;
#48876 = CARTESIAN_POINT ( 'NONE',  ( 5.495132332240461714, 5.305409230568988832, 0.7998128361456341429 ) ) ;
#48878 = CARTESIAN_POINT ( 'NONE',  ( -5.910622443071302357, 6.001017179288033354, 0.07212419881679615896 ) ) ;
#48879 = CARTESIAN_POINT ( 'NONE',  ( 4.481858567196604248, 1.473221693029845181, 1.717120190082993103 ) ) ;
#48880 = CARTESIAN_POINT ( 'NONE',  ( 0.8188879582939897483, -1.495318261269963589, 1.421039783695568604 ) ) ;
#48881 = CARTESIAN_POINT ( 'NONE',  ( -6.008234629150358330, 10.16135750065076060, 0.000000000000000000 ) ) ;
#48882 = CARTESIAN_POINT ( 'NONE',  ( -4.406036734316900905, 5.203092947200234519, -1.082531754730543971 ) ) ;
#48883 = CARTESIAN_POINT ( 'NONE',  ( 2.219920553356643289, -2.194584817558010936, 0.5498286310916412623 ) ) ;
#48884 = ORIENTED_EDGE ( 'NONE', *, *, #213665, .T. ) ;
#48885 = CARTESIAN_POINT ( 'NONE',  ( 0.7499999999999902300, 1.264583334016147642, 1.299038105676657340 ) ) ;
#48886 = CARTESIAN_POINT ( 'NONE',  ( 2.583089905966722277, 1.711919019956799737, -0.7542334906679578621 ) ) ;
#48887 = CARTESIAN_POINT ( 'NONE',  ( 1.195528834012358210, 1.529115512818737699, 0.8178816217611245554 ) ) ;
#48888 = CARTESIAN_POINT ( 'NONE',  ( 4.880524338131243312, -0.2681524694418158661, -2.175044001020635331 ) ) ;
#48889 = CARTESIAN_POINT ( 'NONE',  ( 6.387736634265912983, 1.584785628913528699, 1.677562689604541468 ) ) ;
#48890 = CARTESIAN_POINT ( 'NONE',  ( 1.674756777405971064, -1.956562173829911044, -0.6475767382677873885 ) ) ;
#48891 = CARTESIAN_POINT ( 'NONE',  ( 4.593657693847520207, -1.941558278569108120, -0.04622955632663238584 ) ) ;
#48892 = CARTESIAN_POINT ( 'NONE',  ( -3.212919216314315207, 5.731860938133201522, 1.082531754730560403 ) ) ;
#48893 = CARTESIAN_POINT ( 'NONE',  ( 6.415307259278708152, -0.2288938695442776505, 1.856442058181500654 ) ) ;
#48894 = CARTESIAN_POINT ( 'NONE',  ( 1.062500000000000888, -1.451031289061164742, -1.451031289061077922 ) ) ;
#48895 = CARTESIAN_POINT ( 'NONE',  ( 4.071134731106788252, 7.497899514862828241, -0.5496474101556632075 ) ) ;
#48896 = CARTESIAN_POINT ( 'NONE',  ( 6.257185446134499784, -2.006139278912861368, -0.2004013049526700285 ) ) ;
#48897 = EDGE_CURVE ( 'NONE', #37159, #112702, #26446, .T. ) ;
#48898 = CARTESIAN_POINT ( 'NONE',  ( 1.528150327639969719, -3.232243495192087757, 2.908546201585544999 ) ) ;
#48899 = CARTESIAN_POINT ( 'NONE',  ( -1.360316468750032870, 0.6614583336747411613, 0.7853790794158620470 ) ) ;
#48900 = CARTESIAN_POINT ( 'NONE',  ( 5.836564609439236939, 0.5826586670559866787, -1.930416874340326938 ) ) ;
#48901 = CARTESIAN_POINT ( 'NONE',  ( -4.406036734316906234, 4.242723732898890709, -0.7216878364870207285 ) ) ;
#48902 = CARTESIAN_POINT ( 'NONE',  ( 6.448874621594486989, 10.67543749183559143, 0.7998128361456462443 ) ) ;
#48903 = CARTESIAN_POINT ( 'NONE',  ( 5.090160327287878594, 4.903218234782778850, -0.7998128361456481317 ) ) ;
#48905 = DIRECTION ( 'NONE',  ( 0.000000000000000000, 0.000000000000000000, 1.000000000000000000 ) ) ;
#48904 = CARTESIAN_POINT ( 'NONE',  ( 2.051128252772801641, -1.465761996925791122, -1.088229512710245261 ) ) ;
#48906 = DIRECTION ( 'NONE',  ( 0.000000000000000000, 0.000000000000000000, -1.000000000000000000 ) ) ;
#48907 = CARTESIAN_POINT ( 'NONE',  ( -9.645001968711920171, 4.042125922905831281, 6.587946042608958663 ) ) ;
#48908 = VERTEX_POINT ( 'NONE', #212317 ) ;
#48909 = CARTESIAN_POINT ( 'NONE',  ( -3.621436428181653788, 7.239109909604962922, 0.7216878364870338292 ) ) ;
#48910 = CARTESIAN_POINT ( 'NONE',  ( 2.960183528328370173, -4.197067547847380453, -1.425551791145183156 ) ) ;
#48911 = CARTESIAN_POINT ( 'NONE',  ( -9.508345801885592863, 9.987491611821676329, 0.7998128361456462443 ) ) ;
#48912 = CARTESIAN_POINT ( 'NONE',  ( -0.1579319072057436268, -1.246015270063109748, -1.590120154594099278 ) ) ;
#48913 = CARTESIAN_POINT ( 'NONE',  ( 0.3113914200543760336, 1.760583737686383321, -1.181573663439141830 ) ) ;
#48914 = ORIENTED_EDGE ( 'NONE', *, *, #199415, .F. ) ;
#48915 = CARTESIAN_POINT ( 'NONE',  ( -5.088052786878465739, 9.158088361325352977, 0.000000000000000000 ) ) ;
#48916 = CARTESIAN_POINT ( 'NONE',  ( 4.005544317833563461, 6.760553239859419250, -1.199719254218452047 ) ) ;
#48917 = CARTESIAN_POINT ( 'NONE',  ( 6.192271402255323132, -2.050732637037344208, -0.2044092671329711397 ) ) ;
#48918 = CARTESIAN_POINT ( 'NONE',  ( 5.397111353752316987, -0.9091427841607623295, -1.799923777076550824 ) ) ;
#48919 = ORIENTED_EDGE ( 'NONE', *, *, #190705, .F. ) ;
#48920 = ORIENTED_EDGE ( 'NONE', *, *, #212049, .T. ) ;
#48921 = ORIENTED_EDGE ( 'NONE', *, *, #53808, .F. ) ;
#48922 = CARTESIAN_POINT ( 'NONE',  ( -9.484092147959342967, 11.02352791316275216, 1.199719254218462483 ) ) ;
#48923 = CARTESIAN_POINT ( 'NONE',  ( -1.225000000000028066, 0.3125000006828221322, -4.336808689942017736E-14 ) ) ;
#48924 = CIRCLE ( 'NONE', #197636, 1.500000000000000222 ) ;
#48927 = ORIENTED_EDGE ( 'NONE', *, *, #43966, .F. ) ;
#48926 = CARTESIAN_POINT ( 'NONE',  ( 4.650083499807220910, 5.295740330745369207, -2.420000000000000373 ) ) ;
#48925 = CARTESIAN_POINT ( 'NONE',  ( -6.493429226302317225, 6.540365283632955773, 0.7998128361456341429 ) ) ;
#48928 = CARTESIAN_POINT ( 'NONE',  ( 5.950060389077887812, 7.221515259811701171, 1.225279837341096689 ) ) ;
#48929 = CARTESIAN_POINT ( 'NONE',  ( 4.710314442360476583, -1.556670644073439913, -1.281164596596932936 ) ) ;
#48930 = CARTESIAN_POINT ( 'NONE',  ( 4.822110771479974467, 1.762745816080556915, 0.5315184756640098929 ) ) ;
#48931 = AXIS2_PLACEMENT_3D ( 'NONE', #88179, #36207, #185657 ) ;
#48932 = CARTESIAN_POINT ( 'NONE',  ( 0.07661050522433668353, 0.008287133257128471639, -1.710863442170395432 ) ) ;
#48933 = CARTESIAN_POINT ( 'NONE',  ( 3.071242857908276669, -2.132312958082840826, -0.8828933859421483898 ) ) ;
#48934 = CARTESIAN_POINT ( 'NONE',  ( 5.481239241674765950, 9.616805891921051952, -0.7998128361456481317 ) ) ;
#48935 = CARTESIAN_POINT ( 'NONE',  ( 6.309879873373573922, -2.146112031266556919, 0.2576265230809087758 ) ) ;
#48936 = CARTESIAN_POINT ( 'NONE',  ( 8.281332899848809603, 8.555976559445431562, 0.7998128361456481317 ) ) ;
#48937 = CARTESIAN_POINT ( 'NONE',  ( 1.311946287462633309, 1.302956792059128066, -1.440285294924074311 ) ) ;
#48938 = CARTESIAN_POINT ( 'NONE',  ( -3.113568832632681360, 6.784247404713427798, -0.7998128361456281477 ) ) ;
#48939 = ORIENTED_EDGE ( 'NONE', *, *, #197116, .F. ) ;
#48940 = CARTESIAN_POINT ( 'NONE',  ( 4.253462032731039066, -2.272626950162641268, -0.3425954598320450906 ) ) ;
#48941 = CARTESIAN_POINT ( 'NONE',  ( -9.351007409486083333, 15.43944876071892125, -7.441777623099242511 ) ) ;
#48942 = CARTESIAN_POINT ( 'NONE',  ( -4.329849954717889915, 6.144853928627882489, 1.599625672291270506 ) ) ;
#48943 = CARTESIAN_POINT ( 'NONE',  ( 3.115926070338378207, -0.9207206926411042325, -1.628290677324291780 ) ) ;
#48946 = CARTESIAN_POINT ( 'NONE',  ( -6.231907884136888676, 7.299589282028351001, -1.199719254218453823 ) ) ;
#48945 = CARTESIAN_POINT ( 'NONE',  ( -0.7500000000000006661, 0.6395833340161540814, -1.299038105676652011 ) ) ;
#48944 = CARTESIAN_POINT ( 'NONE',  ( 0.8262462788446511830, -0.8622288892402606431, -1.707089296137359158 ) ) ;
#48947 = B_SPLINE_CURVE_WITH_KNOTS ( 'NONE', 3,
 ( #17397, #149563, #68281, #19544, #151709, #69345, #20603, #105096, #157043, #74712 ),
 .UNSPECIFIED., .F., .F.,
 ( 4, 3, 3, 4 ),
 ( 7.433113292862203613E-18, 0.0001748236543164608252, 0.0003403917518363700173, 0.0005070588120444130585 ),
 .UNSPECIFIED. ) ;
#48948 = CARTESIAN_POINT ( 'NONE',  ( 2.385638622766753425, 2.017150886971270651, -0.8956362484653990208 ) ) ;
#48949 = EDGE_CURVE ( 'NONE', #73128, #31261, #26490, .T. ) ;
#48950 = CARTESIAN_POINT ( 'NONE',  ( 6.983263157960372780, 7.052928845687945980, 2.444341994195888379 ) ) ;
#48951 = CARTESIAN_POINT ( 'NONE',  ( 4.390142812726693045, 4.016254791136236513, 1.214306433183764966E-14 ) ) ;
#48952 = CARTESIAN_POINT ( 'NONE',  ( 6.983858524370782028, 8.280828045588322084, 1.082531754730549967 ) ) ;
#48953 = CARTESIAN_POINT ( 'NONE',  ( -4.406563619641430840, 5.099744630125142564, -1.199719254218446718 ) ) ;
#48954 = CARTESIAN_POINT ( 'NONE',  ( -7.566859129758459979, 8.000626204239226880, 0.000000000000000000 ) ) ;
#48955 = CARTESIAN_POINT ( 'NONE',  ( 0.6496080044469240145, 0.6224236735355732630, -1.870565628188630702 ) ) ;
#48956 = CARTESIAN_POINT ( 'NONE',  ( 1.114821240386947965, -1.040235440384199794, -2.059874970276051265 ) ) ;
#48957 = CARTESIAN_POINT ( 'NONE',  ( 1.574581288703358339, 1.320057194528483135, -1.451483715152704246 ) ) ;
#48958 = CARTESIAN_POINT ( 'NONE',  ( 4.996965725392733759, 0.3474287616172208604, 2.032942699294958633 ) ) ;
#48959 = CARTESIAN_POINT ( 'NONE',  ( 4.311129659465574804, 7.013106455143060636, -1.082531754730548412 ) ) ;
#48960 = CARTESIAN_POINT ( 'NONE',  ( 6.150558962454855561, 7.204682206732687000, 1.199719254218452047 ) ) ;
#48961 = ORIENTED_EDGE ( 'NONE', *, *, #102136, .T. ) ;
#48962 = CARTESIAN_POINT ( 'NONE',  ( -1.364683531250010295, 4.342708333674753618, 0.7879004041258379498 ) ) ;
#48963 = CARTESIAN_POINT ( 'NONE',  ( -4.944262139963866431, 4.884656545040805042, 0.5135224484073761531 ) ) ;
#48964 = CARTESIAN_POINT ( 'NONE',  ( 3.511198595814926993, 6.079853547550633230, 1.082531754730558626 ) ) ;
#48965 = CARTESIAN_POINT ( 'NONE',  ( 0.9718041211803396529, -0.3205511010368928271, 2.147183668106082521 ) ) ;
#48967 = CARTESIAN_POINT ( 'NONE',  ( 6.304252605626877504, 1.359535501544101077, -1.241908024382516240 ) ) ;
#48966 = CARTESIAN_POINT ( 'NONE',  ( 9.490381562237910629, -9.037089468803353398, -0.4325416218483115194 ) ) ;
#48968 = ADVANCED_FACE ( 'NONE', ( #47734 ), #180494, .T. ) ;
#48969 = CARTESIAN_POINT ( 'NONE',  ( 11.35569630219380777, 11.11268439291370314, -3.554478010595023107 ) ) ;
#48970 = CARTESIAN_POINT ( 'NONE',  ( -7.458876248283173638, -7.605490376493679427, 6.801849632071883534 ) ) ;
#48971 = CARTESIAN_POINT ( 'NONE',  ( 1.458040028222376439, 0.7530789129696242590, 1.712431740859089668 ) ) ;
#48972 = CARTESIAN_POINT ( 'NONE',  ( 5.202478051755599964, -0.7228594145181690411, -2.037298988101433839 ) ) ;
#48973 = CARTESIAN_POINT ( 'NONE',  ( -6.063230027062802563, 6.042581475280591086, 0.5001817740485012820 ) ) ;
#48974 = CARTESIAN_POINT ( 'NONE',  ( -0.02244404828160087226, 1.995160441984781041, -2.602654351998904492 ) ) ;
#48975 = CARTESIAN_POINT ( 'NONE',  ( -0.6823417656250246877, -0.6989583329919113464, 1.181850606188755259 ) ) ;
#48976 = CARTESIAN_POINT ( 'NONE',  ( 1.682132150489405564, 0.9841149911452107268, 1.639481845682550398 ) ) ;
#48977 = CARTESIAN_POINT ( 'NONE',  ( 3.397073482672040345, 1.394525624090914961, 1.089649698571172776 ) ) ;
#48978 = CARTESIAN_POINT ( 'NONE',  ( 0.9086806230526077721, -0.4651930584498394916, -1.854694524013176693 ) ) ;
#48980 = CARTESIAN_POINT ( 'NONE',  ( 5.308173953863717820, 1.137349973717050267, -1.541276042019421810 ) ) ;
#48979 = CARTESIAN_POINT ( 'NONE',  ( 2.540449947701581390, -3.218732648277128572, 2.112750016026112565 ) ) ;
#48981 = CARTESIAN_POINT ( 'NONE',  ( 1.499999999999987121, -0.9958333333333134751, 0.8660254037844524744 ) ) ;
#48982 = CARTESIAN_POINT ( 'NONE',  ( 6.162556002056702731, -0.7074686763054702787, -1.838295890583282022 ) ) ;
#48983 = CARTESIAN_POINT ( 'NONE',  ( -0.7499999999999972244, 4.858333333333353821, -1.299038105676652011 ) ) ;
#48984 = CARTESIAN_POINT ( 'NONE',  ( 0.7738737444688469358, 0.4079195088417563730, -2.080830740624163955 ) ) ;
#48985 = CARTESIAN_POINT ( 'NONE',  ( 0.000000000000000000, 0.5000000000000004441, 0.000000000000000000 ) ) ;
#48986 = CARTESIAN_POINT ( 'NONE',  ( 4.293723057671197552, -0.7160966649314598476, 1.728361679364013748 ) ) ;
#48988 = EDGE_LOOP ( 'NONE', ( #38058, #170107, #159666, #66722, #70005, #21953 ) ) ;
#48987 = CARTESIAN_POINT ( 'NONE',  ( 0.6096330727367264002, -1.817201089070449971, 0.1759225495863714350 ) ) ;
#48990 = CARTESIAN_POINT ( 'NONE',  ( -1.499999999999997780, 4.400000000000021672, 1.214306433183764966E-14 ) ) ;
#48989 = CARTESIAN_POINT ( 'NONE',  ( 4.547634279845023109, -1.704780727694398479, -1.401453192282381188 ) ) ;
#48991 = CARTESIAN_POINT ( 'NONE',  ( -1.201851678989727383E-14, 5.259375000341421469, -1.575800808251660134 ) ) ;
#48992 = CARTESIAN_POINT ( 'NONE',  ( 1.609910828531309956, 0.6006481715085715267, -1.973267531027416810 ) ) ;
#48993 = CARTESIAN_POINT ( 'NONE',  ( 6.124532705071213279, 8.168374127381657246, -1.599625672291262513 ) ) ;
#48994 = CARTESIAN_POINT ( 'NONE',  ( -8.877891658850122880, 9.251961778280284321, 0.7998128361456462443 ) ) ;
#48995 = CARTESIAN_POINT ( 'NONE',  ( -3.459886018179104017, -0.007765290029630126691, -0.2323671850544757334 ) ) ;
#48997 = EDGE_CURVE ( 'NONE', #59844, #161718, #170121, .T. ) ;
#48996 = VECTOR ( 'NONE', #4914, 1000.000000000000000 ) ;
#48998 = CARTESIAN_POINT ( 'NONE',  ( 6.994027139803230320, 9.253060644560830994, -1.599625672291267398 ) ) ;
#48999 = ORIENTED_EDGE ( 'NONE', *, *, #98822, .F. ) ;
#49000 = CARTESIAN_POINT ( 'NONE',  ( 4.141125838365485201, -0.1998502692034490602, -2.060677327190631569 ) ) ;
#49001 = CARTESIAN_POINT ( 'NONE',  ( 0.7499999999999920064, 5.233333333333353821, 1.299038105676669330 ) ) ;
#49002 = CARTESIAN_POINT ( 'NONE',  ( 1.229993901927586286, -1.370328181169593096, -1.671761099108048265 ) ) ;
#49003 = CARTESIAN_POINT ( 'NONE',  ( -5.670379370357061077, 7.341873695786736320, -1.227147999111227294 ) ) ;
#49004 = CARTESIAN_POINT ( 'NONE',  ( 1.699873857359509799, 1.394438142870989772, 1.461265194366095033 ) ) ;
#49005 = CARTESIAN_POINT ( 'NONE',  ( -3.283337425626721373, -0.1112512837626866702, -0.1207467602163218856 ) ) ;
#49006 = ORIENTED_EDGE ( 'NONE', *, *, #123570, .T. ) ;
#49008 = CARTESIAN_POINT ( 'NONE',  ( 8.934460041725669655, 9.525884258209195821, 1.040834085586084257E-14 ) ) ;
#49007 = CARTESIAN_POINT ( 'NONE',  ( -3.475000000000000533, -3.499999999999999556, 0.000000000000000000 ) ) ;
#49009 = CARTESIAN_POINT ( 'NONE',  ( 6.883263157960391787, 1.253787318140922480, 2.167784446185747171 ) ) ;
#49010 = CARTESIAN_POINT ( 'NONE',  ( 0.4269707148552639997, -1.727061408318403712, 1.040797348915108111 ) ) ;
#49011 = CARTESIAN_POINT ( 'NONE',  ( 4.687173145698103838, 1.624054394666199830, 1.471728111018810070 ) ) ;
#49012 = CARTESIAN_POINT ( 'NONE',  ( -1.201851678989727383E-14, 3.368750000682815049, -1.732050807568863648 ) ) ;
#49013 = CARTESIAN_POINT ( 'NONE',  ( 3.673993457511486760, 1.897360377298975331, -0.2389773157873422149 ) ) ;
#49014 = CARTESIAN_POINT ( 'NONE',  ( -4.115063316947640715, 4.759660943649018705, 1.199719254218462483 ) ) ;
#49015 = CARTESIAN_POINT ( 'NONE',  ( 7.117667457050084856, 7.406292909420979953, -0.7216878364870257245 ) ) ;
#49017 = CARTESIAN_POINT ( 'NONE',  ( 1.862907868837269998, -0.1017702599966328891, -2.013986063733465226 ) ) ;
#49016 = CARTESIAN_POINT ( 'NONE',  ( -8.446366511189330240, 12.79791866312216442, 0.7216878364870317197 ) ) ;
#49018 = CARTESIAN_POINT ( 'NONE',  ( -1.364683531250014514, 12.90104166700806232, -0.7879004041258335089 ) ) ;
#49020 = CARTESIAN_POINT ( 'NONE',  ( -2.993318053567081360, 6.714231172462041819, 0.000000000000000000 ) ) ;
#49019 = CARTESIAN_POINT ( 'NONE',  ( 0.6797070353673840826, 1.544897314466355143, 1.693757226825955753 ) ) ;
#49021 = CARTESIAN_POINT ( 'NONE',  ( 3.926516724862822993, 1.637815149125703584, 0.5408920155725772672 ) ) ;
#49022 = CARTESIAN_POINT ( 'NONE',  ( 1.250000000000037526, 8.500000000000000000, 10.97907099895068583 ) ) ;
#49023 = CARTESIAN_POINT ( 'NONE',  ( 3.225950485047770933, 5.851027101609320269, 1.199719254218450271 ) ) ;
#49024 = VECTOR ( 'NONE', #119671, 1000.000000000000000 ) ;
#49025 = DIRECTION ( 'NONE',  ( 3.451266460341927524E-31, -0.6000000000000035305, -0.7999999999999974909 ) ) ;
#49026 = CARTESIAN_POINT ( 'NONE',  ( 5.027376032568989572, 4.759693547618927489, 0.7998128361456341429 ) ) ;
#49027 = CARTESIAN_POINT ( 'NONE',  ( 0.1751657365761704888, 2.870293503558702497, -2.532510806204853804 ) ) ;
#49028 = VERTEX_POINT ( 'NONE', #88480 ) ;
#49029 =( NAMED_UNIT ( * ) PLANE_ANGLE_UNIT ( ) SI_UNIT ( $, .RADIAN. ) );
#49030 = ORIENTED_EDGE ( 'NONE', *, *, #84368, .F. ) ;
#49031 = CARTESIAN_POINT ( 'NONE',  ( 5.127533414443554705, -0.2600442617171055404, 1.792572003776324197 ) ) ;
#49032 = ORIENTED_EDGE ( 'NONE', *, *, #8819, .F. ) ;
#49033 = CARTESIAN_POINT ( 'NONE',  ( 6.554440917563797875, 6.611545590104705994, -0.7998128361456481317 ) ) ;
#49034 = CARTESIAN_POINT ( 'NONE',  ( 6.937452841262695458, -7.242250812743807664, -6.937452841262718550 ) ) ;
#49035 = CARTESIAN_POINT ( 'NONE',  ( 5.602179418825736334, -0.8085942178241835032, 1.621059995222628780 ) ) ;
#49036 = CARTESIAN_POINT ( 'NONE',  ( 6.997416677984476863, 7.336276677169590421, 0.000000000000000000 ) ) ;
#49037 = CARTESIAN_POINT ( 'NONE',  ( 7.755938900619410603, -5.581885079358431589, -7.800371912476627756 ) ) ;
#49038 = CARTESIAN_POINT ( 'NONE',  ( 2.765787700092982693, 1.173089151190203294, 1.850848517565194751 ) ) ;
#49039 = CIRCLE ( 'NONE', #7406, 1.000000000000000000 ) ;
#49041 = CARTESIAN_POINT ( 'NONE',  ( 7.553864141108259211, 11.96459193126834464, 1.040834085586084257E-14 ) ) ;
#49040 = CARTESIAN_POINT ( 'NONE',  ( 6.496546432963370421, 1.840999872533972903, 0.2716635292502044829 ) ) ;
#49042 = CARTESIAN_POINT ( 'NONE',  ( 4.130425774021486696, 0.5146700378890654015, 1.845081245478853216 ) ) ;
#49043 = FACE_OUTER_BOUND ( 'NONE', #204304, .T. ) ;
#49044 = PRESENTATION_STYLE_ASSIGNMENT (( #115164 ) ) ;
#49045 = CARTESIAN_POINT ( 'NONE',  ( 1.364683531249988757, -0.1156249996585798079, 0.000000000000000000 ) ) ;
#49046 = CARTESIAN_POINT ( 'NONE',  ( 4.826339496784873617, 8.574553812983598533, -0.7216878364870257245 ) ) ;
#49048 = CARTESIAN_POINT ( 'NONE',  ( 6.104719058799578768, 1.976458628850938704, 0.7599229572291065216 ) ) ;
#49047 = CARTESIAN_POINT ( 'NONE',  ( -10.31739171031960822, 11.13930453823545186, 1.040834085586084257E-14 ) ) ;
#49049 = CARTESIAN_POINT ( 'NONE',  ( 1.288190726105652217, -0.9714702286227733241, 1.931199087792371261 ) ) ;
#49050 = CARTESIAN_POINT ( 'NONE',  ( -6.147696309153835692, 6.137010213626392208, 0.7998128361456281477 ) ) ;
#49051 = CARTESIAN_POINT ( 'NONE',  ( 5.174371902270911150, 6.065797303184739420, 1.199719254218452047 ) ) ;
#49052 = CARTESIAN_POINT ( 'NONE',  ( 1.008509592878764183, 1.385430265305506170, -1.188947219173806413 ) ) ;
#49053 = CARTESIAN_POINT ( 'NONE',  ( -5.115504031057831469, 4.862509545855891346, 0.7998128361456341429 ) ) ;
#49054 = CARTESIAN_POINT ( 'NONE',  ( 3.803562306130504389, -0.5304149723801485639, 1.746809896627635084 ) ) ;
#49055 = CARTESIAN_POINT ( 'NONE',  ( 8.484127223451739752, 12.60054268945961198, 8.443863754375202646 ) ) ;
#49056 = CARTESIAN_POINT ( 'NONE',  ( 2.584119536544440265, 1.026460374567798484, 1.613398670029235538 ) ) ;
#49057 = ORIENTED_EDGE ( 'NONE', *, *, #36946, .T. ) ;
#49058 = CARTESIAN_POINT ( 'NONE',  ( 2.611712457634679296, 0.5281755657932221126, -1.897318813625125777 ) ) ;
#49059 = ORIENTED_EDGE ( 'NONE', *, *, #159020, .T. ) ;
#49060 = CARTESIAN_POINT ( 'NONE',  ( 4.423342042002774477, -1.197376356234590933, -1.528922412636232631 ) ) ;
#49061 = CARTESIAN_POINT ( 'NONE',  ( -4.248501033035892327, 6.049946853332221153, -1.599625672291271394 ) ) ;
#49063 = CARTESIAN_POINT ( 'NONE',  ( 5.836213162209912930, -1.179542664122106510, -1.762073437084572314 ) ) ;
#49062 = CARTESIAN_POINT ( 'NONE',  ( 7.042534447655770080, 7.180988041878682004, -0.7998128361456341429 ) ) ;
#49064 = CARTESIAN_POINT ( 'NONE',  ( -0.07933194154488883154, -7.246166700194011767, 9.499668754385636404 ) ) ;
#49065 = CARTESIAN_POINT ( 'NONE',  ( 3.176317266091326807, 0.8619891151622931513, 1.707069686517001195 ) ) ;
#49066 = CARTESIAN_POINT ( 'NONE',  ( 5.841900715481964212, 6.189949835993628469, -0.9061318016433889122 ) ) ;
#49067 = CARTESIAN_POINT ( 'NONE',  ( -1.123270288250315163, 3.047697346350006331, -0.7749999999993613109 ) ) ;
#49068 = ORIENTED_EDGE ( 'NONE', *, *, #76833, .F. ) ;
#49069 = CARTESIAN_POINT ( 'NONE',  ( 4.095444919779759552, 6.935713618788495793, 1.199719254218451159 ) ) ;
#49070 = CARTESIAN_POINT ( 'NONE',  ( 5.495132332240461714, 5.305409230568988832, 0.7998128361456341429 ) ) ;
#49071 = CARTESIAN_POINT ( 'NONE',  ( 4.055341430421886884, -1.750343679372264205, 0.9943053665309193878 ) ) ;
#49072 = CARTESIAN_POINT ( 'NONE',  ( 11.07790593930098311, 12.30000000000000071, -0.7000000000000009548 ) ) ;
#49073 = CARTESIAN_POINT ( 'NONE',  ( 4.828627627824715773, 1.747987318788373656, 0.5269492854979712648 ) ) ;
#49074 = CARTESIAN_POINT ( 'NONE',  ( 0.5200892513525963157, 2.048054262204841880, -0.3022008342252607838 ) ) ;
#49075 = CARTESIAN_POINT ( 'NONE',  ( -8.432808358020034589, 10.86136238915529084, 1.443375672974064550 ) ) ;
#49076 = CARTESIAN_POINT ( 'NONE',  ( -6.486107617800834113, 6.842887492708185526, 0.6303255377333163434 ) ) ;
#49077 = DIRECTION ( 'NONE',  ( 0.000000000000000000, 1.000000000000000000, 0.000000000000000000 ) ) ;
#49078 = CARTESIAN_POINT ( 'NONE',  ( 5.612129163471575310, -0.8422657237196762292, -1.670366365510121742 ) ) ;
#49079 = CARTESIAN_POINT ( 'NONE',  ( 6.962275575817444384, 8.081408578997208991, -1.199719254218446718 ) ) ;
#49080 = CIRCLE ( 'NONE', #76721, 0.7500000000000006661 ) ;
#49081 = CARTESIAN_POINT ( 'NONE',  ( -3.750802052474980108, 7.527686161196117887, 1.040834085586084257E-14 ) ) ;
#49082 = EDGE_CURVE ( 'NONE', #185972, #210868, #98594, .T. ) ;
#49083 = CARTESIAN_POINT ( 'NONE',  ( 1.364683531249997417, 10.04687500034139802, 2.602085213965210642E-15 ) ) ;
#49084 = CARTESIAN_POINT ( 'NONE',  ( -4.415151579544611238, 8.302760609444034046, -0.7998128361456281477 ) ) ;
#49085 = CARTESIAN_POINT ( 'NONE',  ( 4.546061579283848353, 4.198160018786257552, -0.7998128361456211532 ) ) ;
#49086 = CARTESIAN_POINT ( 'NONE',  ( -6.583366107887490770, 9.838288338247510367, 1.199719254218452935 ) ) ;
#49087 = CARTESIAN_POINT ( 'NONE',  ( -4.543954038874438162, 8.453030145328826350, 1.040834085586084257E-14 ) ) ;
#49088 = CARTESIAN_POINT ( 'NONE',  ( 0.8485890540621650047, -2.054197865963180547, -0.2570499307305574299 ) ) ;
#49089 = CARTESIAN_POINT ( 'NONE',  ( 2.390374844762462203, -0.8132668539616545456, -1.954994498336021458 ) ) ;
#49090 = CARTESIAN_POINT ( 'NONE',  ( 9.725276259704228821, 10.24057714594344048, 0.7998128361456462443 ) ) ;
#49091 = CARTESIAN_POINT ( 'NONE',  ( -0.1263102688159843945, 6.363441598446243574, 3.117922131261606999 ) ) ;
#49092 = CARTESIAN_POINT ( 'NONE',  ( 6.561392567526037389, 1.717850402480676664, 1.155108059606273052 ) ) ;
#49093 = CARTESIAN_POINT ( 'NONE',  ( 4.715454802112915011, 7.044561259014620269, 1.385117731104364536 ) ) ;
#49094 = CARTESIAN_POINT ( 'NONE',  ( 4.175548123328908900, 7.815297210618305179, -0.7216878364870197293 ) ) ;
#49096 = FACE_OUTER_BOUND ( 'NONE', #42677, .T. ) ;
#49095 = CARTESIAN_POINT ( 'NONE',  ( 3.475000000000000533, -3.295833333333334725, -2.006292185433951047 ) ) ;
#49097 = CARTESIAN_POINT ( 'NONE',  ( 2.115536061532933942, -2.222870945405757137, 0.5592890022133433225 ) ) ;
#49099 = CARTESIAN_POINT ( 'NONE',  ( -4.517335436343488553, 8.499999999999996447, -0.7750000000000013545 ) ) ;
#49098 = CARTESIAN_POINT ( 'NONE',  ( -6.343417644169881520, 6.506394916555812813, 2.500000000000000444 ) ) ;
#49100 = CARTESIAN_POINT ( 'NONE',  ( 2.214975196874233720, 1.533708969217022933, -1.142120075431733994 ) ) ;
#49101 = ORIENTED_EDGE ( 'NONE', *, *, #79457, .T. ) ;
#49102 = CARTESIAN_POINT ( 'NONE',  ( 6.263503779389103521, 10.25124547602188763, 1.040834085586084257E-14 ) ) ;
#49103 = EDGE_CURVE ( 'NONE', #30003, #35846, #65223, .T. ) ;
#49104 = CARTESIAN_POINT ( 'NONE',  ( 0.4748584900105623507, -1.455329053371579695, 1.391259960792426975 ) ) ;
#49105 = CARTESIAN_POINT ( 'NONE',  ( 1.252704021237858401, -0.4712815170893420724, -1.904206577484176321 ) ) ;
#49106 = CARTESIAN_POINT ( 'NONE',  ( -10.29471871147821282, 10.90492667301307605, -0.7998128361456291469 ) ) ;
#49107 = APPLICATION_CONTEXT ( 'automotive_design' ) ;
#49108 = CARTESIAN_POINT ( 'NONE',  ( -7.202405917357668663, 9.425892875049191488, 1.599625672291295375 ) ) ;
#49109 = CARTESIAN_POINT ( 'NONE',  ( -11.95500822865703761, 8.101291463845146978, -0.2602123231208265941 ) ) ;
#49111 = CARTESIAN_POINT ( 'NONE',  ( 2.359889027365429826, 0.7540158325645224258, 1.601324458166239806 ) ) ;
#49110 = CARTESIAN_POINT ( 'NONE',  ( 3.662131271747073757, -1.403999256393541284, 1.549221476816674548 ) ) ;
#49112 = CARTESIAN_POINT ( 'NONE',  ( 0.000000000000000000, 18.91999999999999815, 11.18000000000000149 ) ) ;
#49114 = CARTESIAN_POINT ( 'NONE',  ( 4.787240309336779909, 1.696446081987776022, 1.541789747812449818 ) ) ;
#49113 = CARTESIAN_POINT ( 'NONE',  ( -11.57271903506312150, 7.021589676523640300, -3.181598541533452895 ) ) ;
#49115 = CARTESIAN_POINT ( 'NONE',  ( 4.241972025877470465, 0.4673694910880517583, 1.676319072879989047 ) ) ;
#49116 = B_SPLINE_CURVE_WITH_KNOTS ( 'NONE', 3,
 ( #25438, #43861, #61150, #171691, #109976, #187932, #12383, #65122, #131279, #199386 ),
 .UNSPECIFIED., .F., .F.,
 ( 4, 3, 3, 4 ),
 ( 0.000000000000000000, 4.084796759526023937E-05, 5.706657677113307714E-05, 5.895014842486881381E-05 ),
 .UNSPECIFIED. ) ;
#49117 = CARTESIAN_POINT ( 'NONE',  ( 7.944187942603509356, 11.35563746875774882, 1.199719254218460707 ) ) ;
#49118 = VECTOR ( 'NONE', #132168, 1000.000000000000000 ) ;
#49119 = CARTESIAN_POINT ( 'NONE',  ( 4.199993725183333915, 8.122019456014369254, -0.7998128361456361413 ) ) ;
#49120 = CARTESIAN_POINT ( 'NONE',  ( 4.042145929572971141, 1.632826047920731050, -0.5835893337435077433 ) ) ;
#49121 = CARTESIAN_POINT ( 'NONE',  ( 5.002462566363424123, 2.165002515946230499, 0.1647018997421762776 ) ) ;
#49122 = CARTESIAN_POINT ( 'NONE',  ( 4.708759422647839976, 4.387974169377582001, -0.7998128361456211532 ) ) ;
#49123 = CARTESIAN_POINT ( 'NONE',  ( 6.051970301643104122, 1.040788372175960541, 1.727066800951609249 ) ) ;
#49124 = CARTESIAN_POINT ( 'NONE',  ( 6.625000595499368039, -2.052053476427456502, 3.646059517245236328E-13 ) ) ;
#49125 = CARTESIAN_POINT ( 'NONE',  ( 1.499999999999989120, 4.035416667349482012, 0.8660254037844524744 ) ) ;
#49126 = CARTESIAN_POINT ( 'NONE',  ( 2.098540742119249458, -0.5114569845777928725, -1.857200404858405207 ) ) ;
#49127 = CARTESIAN_POINT ( 'NONE',  ( 0.7500000000000006661, 9.364583334016129967, 1.299038105676657340 ) ) ;
#49128 = CARTESIAN_POINT ( 'NONE',  ( 5.572587854402127228, 0.9002147710611071441, 2.031021293335387501 ) ) ;
#49129 = EDGE_LOOP ( 'NONE', ( #210367, #46278, #97091, #158149 ) ) ;
#49130 = CARTESIAN_POINT ( 'NONE',  ( 6.983263157960370116, 2.036707217602062414, 2.350489458799970066 ) ) ;
#49131 = CARTESIAN_POINT ( 'NONE',  ( -0.7500000000000215383, 2.691666666666689522, 1.299038105676671107 ) ) ;
#49132 = CARTESIAN_POINT ( 'NONE',  ( 7.284808609244363353, 7.393364887073558656, 0.7998128361456341429 ) ) ;
#49133 = CARTESIAN_POINT ( 'NONE',  ( 1.805654246593148660, 1.930672025830199479, -1.098395813934008425 ) ) ;
#49134 = CARTESIAN_POINT ( 'NONE',  ( 6.637165056451467038, -0.09505199798197358496, -1.959668910398344233 ) ) ;
#49135 = CARTESIAN_POINT ( 'NONE',  ( 8.107412671292035355, 10.48173408797264194, 1.443375672974076540 ) ) ;
#49136 = CARTESIAN_POINT ( 'NONE',  ( 0.006768871532346317291, 8.210909518262139883, 2.038649385027042626 ) ) ;
#49137 = MECHANICAL_DESIGN_GEOMETRIC_PRESENTATION_REPRESENTATION (  '', ( #24999 ), #63045 ) ;
#49138 = CARTESIAN_POINT ( 'NONE',  ( 4.146814880933355596, 5.931313009212638931, 1.599625672291261402 ) ) ;
#49139 = CARTESIAN_POINT ( 'NONE',  ( -0.1341500063891595818, -0.1486117279969369209, -1.983907055413631992 ) ) ;
#49141 = CARTESIAN_POINT ( 'NONE',  ( 4.686014676054621297, -1.266354490919174403, -1.628128356427221313 ) ) ;
#49140 = LINE ( 'NONE', #196448, #40213 ) ;
#49142 = CARTESIAN_POINT ( 'NONE',  ( -3.405069135326500351, 7.124331091189553433, 1.040834085586084257E-14 ) ) ;
#49143 = CARTESIAN_POINT ( 'NONE',  ( 1.499999999999989120, 5.327083334016152527, -0.8660254037844323793 ) ) ;
#49144 = CARTESIAN_POINT ( 'NONE',  ( 0.6823417656249882723, -0.1572916663252488245, 1.181850606188755259 ) ) ;
#49145 = CARTESIAN_POINT ( 'NONE',  ( 5.835183367072669824, -1.691281831231405963, 0.7993005984755219284 ) ) ;
#49146 = CARTESIAN_POINT ( 'NONE',  ( 5.045445647265833777, -1.250780835746621245, 1.201444140469201782 ) ) ;
#49147 = CARTESIAN_POINT ( 'NONE',  ( 4.036439982160089812, -1.511860617216064684, 0.8620873645008280128 ) ) ;
#49148 = CARTESIAN_POINT ( 'NONE',  ( 3.337278367258157630, 7.045241861776501580, 0.7998128361456341429 ) ) ;
#49149 = CARTESIAN_POINT ( 'NONE',  ( 2.349550187768103093, 0.6076851952682017499, -2.210314646808369421 ) ) ;
#49150 = CARTESIAN_POINT ( 'NONE',  ( 1.364683531249984538, -1.094791666325247936, -0.7879004041258309554 ) ) ;
#49151 = CARTESIAN_POINT ( 'NONE',  ( 6.040588761503070003, -1.765850204961866954, 1.119074740713212002 ) ) ;
#49152 = CARTESIAN_POINT ( 'NONE',  ( 0.7261896124251127072, 0.1329856088156805560, 1.836402230816103209 ) ) ;
#49153 = CARTESIAN_POINT ( 'NONE',  ( 4.264541082807580707, 7.493297298796540495, 1.068285269651513936 ) ) ;
#49154 =( LENGTH_UNIT ( ) NAMED_UNIT ( * ) SI_UNIT ( .MILLI., .METRE. ) );
#49155 = CARTESIAN_POINT ( 'NONE',  ( 2.285779929129946098, 1.617817622347239803, -1.203354541732377658 ) ) ;
#49156 = CARTESIAN_POINT ( 'NONE',  ( 1.570551226722196381, -2.081687204081467346, -0.6850663153453034893 ) ) ;
#49157 = CARTESIAN_POINT ( 'NONE',  ( 9.254012853841652841, 13.68113304516277573, -6.839690896908458662 ) ) ;
#49158 = CARTESIAN_POINT ( 'NONE',  ( -8.213542131780492639, 8.476887330032372603, 1.040834085586084257E-14 ) ) ;
#49159 = CARTESIAN_POINT ( 'NONE',  ( 1.557173632797459684, 1.693725193156172315, -1.190412882225246438 ) ) ;
#49160 = CARTESIAN_POINT ( 'NONE',  ( 5.678167406024951624, 5.518950149984223508, 0.7998128361456341429 ) ) ;
#49161 = CARTESIAN_POINT ( 'NONE',  ( -1.360316468749997565, 2.890625000341401574, 1.734723475976807094E-15 ) ) ;
#49162 = CARTESIAN_POINT ( 'NONE',  ( 4.037823014030429647, -2.028772383530423884, 0.6168223452112444605 ) ) ;
#49163 = CARTESIAN_POINT ( 'NONE',  ( 1.364683531249984538, -1.094791666325247936, -0.7879004041258309554 ) ) ;
#49164 = CARTESIAN_POINT ( 'NONE',  ( 6.322862864304120478, 1.705426906915354035, 0.6521430802832667295 ) ) ;
#49165 = ORIENTED_EDGE ( 'NONE', *, *, #147708, .T. ) ;
#49166 = CARTESIAN_POINT ( 'NONE',  ( -5.764151584465413869, 6.753873599078290546, -1.199719254218453823 ) ) ;
#49167 = CARTESIAN_POINT ( 'NONE',  ( 8.387690588348714726, 12.93738945304888333, 1.040834085586084257E-14 ) ) ;
#49168 = CARTESIAN_POINT ( 'NONE',  ( 7.499068361690118145, 7.921536974826172361, -0.7216878364870317197 ) ) ;
#49169 = CARTESIAN_POINT ( 'NONE',  ( 1.001543065824772753E-15, -2.318749999044082966, 4.012584370867899430 ) ) ;
#49170 = CARTESIAN_POINT ( 'NONE',  ( -4.693093728624763372, 8.627026450037540428, 0.7998128361456481317 ) ) ;
#49171 = CARTESIAN_POINT ( 'NONE',  ( 3.076430314242516229, 0.9118049750012310328, 1.802366903320629765 ) ) ;
#49172 = CARTESIAN_POINT ( 'NONE',  ( 1.272647984039422697, -1.336331724779236119, 1.627640044824183674 ) ) ;
#49174 = CARTESIAN_POINT ( 'NONE',  ( -6.363572996767778100, 8.517530811019446091, -1.599625672291271394 ) ) ;
#49173 = CIRCLE ( 'NONE', #111387, 2.150000000000000799 ) ;
#49175 = CARTESIAN_POINT ( 'NONE',  ( 7.716561984472250835, 12.15440608185967086, 1.040834085586084257E-14 ) ) ;
#49176 = CARTESIAN_POINT ( 'NONE',  ( 5.260548175522302472, -0.6249328720258572334, -1.753037815340392935 ) ) ;
#49177 = CARTESIAN_POINT ( 'NONE',  ( 9.088043039861931405, 9.497138389460751284, 1.040834085586084257E-14 ) ) ;
#49178 = CARTESIAN_POINT ( 'NONE',  ( 11.80251051724185807, 13.79999999999999893, -1.695257889419042874 ) ) ;
#49179 = CARTESIAN_POINT ( 'NONE',  ( -3.093231602212184850, 6.760520635889515795, -0.7998128361456281477 ) ) ;
#49180 = CARTESIAN_POINT ( 'NONE',  ( -7.854251061018346469, 8.057714414143200443, -0.7998128361456291469 ) ) ;
#49181 = CARTESIAN_POINT ( 'NONE',  ( 0.1456854043008250221, -1.672057201651616642, -1.369741535119282982 ) ) ;
#49183 = CARTESIAN_POINT ( 'NONE',  ( -5.301779071304492774, 6.560601962741976045, 1.383466813282836716 ) ) ;
#49182 = CARTESIAN_POINT ( 'NONE',  ( -5.101610940492132151, 9.173906207207963348, -0.7998128361456362523 ) ) ;
#49184 = CARTESIAN_POINT ( 'NONE',  ( -1.364683531250014514, -0.01145833299191483488, -0.7879004041258359514 ) ) ;
#49185 = CARTESIAN_POINT ( 'NONE',  ( 1.879855919261735675, -0.2174549385326445539, 1.720076089969482469 ) ) ;
#49186 = CARTESIAN_POINT ( 'NONE',  ( 0.9897393536978270623, -0.4193350815317981040, -1.688907716811594240 ) ) ;
#49188 = CARTESIAN_POINT ( 'NONE',  ( 5.965224400332808763, 9.903252867122883885, -0.7216878364870267237 ) ) ;
#49187 = CARTESIAN_POINT ( 'NONE',  ( 6.445943507803128192, 0.8898977879068777908, -2.129411633396756098 ) ) ;
#49189 = CARTESIAN_POINT ( 'NONE',  ( -10.71026998871754721, 6.055660674263378951, 4.667787751035539223 ) ) ;
#49190 = CARTESIAN_POINT ( 'NONE',  ( 2.442714938195661212, 0.4483736453565168589, 2.011251146304892767 ) ) ;
#49191 = CARTESIAN_POINT ( 'NONE',  ( 1.141953626738337890, -0.04666616626641807014, -2.015725262716171695 ) ) ;
#49192 = CARTESIAN_POINT ( 'NONE',  ( 6.925078400183513949, 3.679108800414055302, 2.758152782261179325 ) ) ;
#49193 = CARTESIAN_POINT ( 'NONE',  ( -4.274563570058511175, 8.209017608368725405, 0.000000000000000000 ) ) ;
#49194 = CARTESIAN_POINT ( 'NONE',  ( 0.2507688454781953902, -1.584965806562924628, 1.172240258958085146 ) ) ;
#49195 = ADVANCED_FACE ( 'NONE', ( #199554 ), #154033, .T. ) ;
#49197 = CARTESIAN_POINT ( 'NONE',  ( -6.563555762791521531, 9.711213252348503744, 1.082531754730549967 ) ) ;
#49196 = CARTESIAN_POINT ( 'NONE',  ( 4.201352949932454450, 1.705870964349815333, -0.8646410313453978258 ) ) ;
#49198 = CARTESIAN_POINT ( 'NONE',  ( 6.041676539500916654, -1.595688354349385607, -1.524751901930617715 ) ) ;
#49199 = CARTESIAN_POINT ( 'NONE',  ( -5.275531169048895741, 9.168887107283438809, -0.7216878364870338292 ) ) ;
#49200 = CARTESIAN_POINT ( 'NONE',  ( 8.039058738260216330, 8.343599714250547805, -0.7998128361456341429 ) ) ;
#49201 = CARTESIAN_POINT ( 'NONE',  ( -2.997761361953021009, 6.511488999004883205, -0.7216878364870458196 ) ) ;
#49202 = CARTESIAN_POINT ( 'NONE',  ( 0.5572930201490761126, -1.731111387009228952, 1.040124062761533352 ) ) ;
#49203 = VERTEX_POINT ( 'NONE', #116254 ) ;
#49204 = CARTESIAN_POINT ( 'NONE',  ( -0.4019237886466933696, 12.83258545099817027, 1.500000000000005995 ) ) ;
#49205 = CARTESIAN_POINT ( 'NONE',  ( 4.630063564305310742, -1.415688044924306555, -1.822237510073132949 ) ) ;
#49206 = CARTESIAN_POINT ( 'NONE',  ( 5.248475795274027078, -1.946838731704622072, -0.2419367024937419397 ) ) ;
#49207 = CARTESIAN_POINT ( 'NONE',  ( 1.481223165768187355, -0.05357505548480785695, 1.961209554040027170 ) ) ;
#49208 = CARTESIAN_POINT ( 'NONE',  ( 10.42352117080803708, 11.05519620889787724, -0.7998128361456281477 ) ) ;
#49209 = CARTESIAN_POINT ( 'NONE',  ( -0.1048463755018592264, -0.8645036352170620830, -1.819965476435807306 ) ) ;
#49210 = ORIENTED_EDGE ( 'NONE', *, *, #50663, .T. ) ;
#49211 = CARTESIAN_POINT ( 'NONE',  ( 0.2338150414605598693, 0.6575980258751003005, -2.012739700429423628 ) ) ;
#49213 = CARTESIAN_POINT ( 'NONE',  ( -7.296259222448620463, 11.66405285949874759, 0.7998128361456481317 ) ) ;
#49212 = CARTESIAN_POINT ( 'NONE',  ( -5.057354993097396445, 5.859001232490445688, -1.199719254218446718 ) ) ;
#49214 = CARTESIAN_POINT ( 'NONE',  ( 0.4800843290509413386, -0.2225996465644273503, -1.827572303103291551 ) ) ;
#49215 = VERTEX_POINT ( 'NONE', #169205 ) ;
#49216 = CARTESIAN_POINT ( 'NONE',  ( 4.135715461124009451, 2.046248213957535089, -0.7259774245699932571 ) ) ;
#49217 = CARTESIAN_POINT ( 'NONE',  ( 9.428250952287726250, 13.54490846161957052, -7.423481931054031868 ) ) ;
#49219 = EDGE_CURVE ( 'NONE', #14088, #197822, #70595, .T. ) ;
#49218 = CARTESIAN_POINT ( 'NONE',  ( 1.828540510153942922, -1.004066958311781832, -1.867862179375394005 ) ) ;
#49220 = CARTESIAN_POINT ( 'NONE',  ( -1.201851678989727383E-14, 2.743750000682820378, 1.732050807568877637 ) ) ;
#49221 = CARTESIAN_POINT ( 'NONE',  ( 8.535021395002688749, 9.916278701380017324, 1.199719254218462483 ) ) ;
#49222 = CARTESIAN_POINT ( 'NONE',  ( 6.562153376633583335, 6.794832157118596783, -0.3727171428496069971 ) ) ;
#49223 = CARTESIAN_POINT ( 'NONE',  ( 1.757177114327221901, -1.766000478700447074, -1.061884917490847791 ) ) ;
#49224 = CARTESIAN_POINT ( 'NONE',  ( -8.962103233833181193, 10.41454084668224489, -1.199719254218446718 ) ) ;
#49225 = CARTESIAN_POINT ( 'NONE',  ( 1.364683531249990311, 3.384375000341416140, 1.214306433183764966E-14 ) ) ;
#49226 = CARTESIAN_POINT ( 'NONE',  ( -6.770610912236888268, -7.154544010627095219, -6.663994888585867749 ) ) ;
#49227 =( BOUNDED_CURVE ( )  B_SPLINE_CURVE ( 2, ( #16575, #169252, #50174, #68523, #184421, #99987, #98930, #53365, #168187, #32855, #66382, #102118, #19786, #182285, #116294, #82658, #51240, #199597, #183363, #85868, #119499, #34967, #200655, #131472, #101039, #166053, #37111, #33911, #164984, #52304, #197474, #167129, #118434, #310, #17638, #185485, #103189, #49119, #150886, #151945, #20838, #83724, #18714, #148742, #84798, #86937, #57641, #105345, #4580, #136764, #172465, #206006, #41413, #26192, #39252, #204927, #122737, #188700, #187625, #157287, #207073 ),
 .UNSPECIFIED., .F., .T. ) 
 B_SPLINE_CURVE_WITH_KNOTS ( ( 3, 2, 2, 2, 2, 2, 2, 2, 2, 2, 2, 2, 2, 2, 2, 2, 2, 2, 2, 2, 2, 2, 2, 2, 2, 2, 2, 2, 2, 2, 3 ),
 ( 0.2691230753395070785, 0.2750000000000000222, 0.2833333333333333259, 0.2916666666666666852, 0.2999999999999999889, 0.3083333333333333481, 0.3166666666666666519, 0.3250000000000000111, 0.3333333333333333148, 0.3416666666666666741, 0.3499999999999999778, 0.3583333333333333370, 0.3666666666666666408, 0.3750000000000000000, 0.3833333333333333592, 0.3916666666666666630, 0.4000000000000000222, 0.4083333333333333259, 0.4166666666666666852, 0.4249999999999999889, 0.4333333333333333481, 0.4416666666666666519, 0.4500000000000000111, 0.4583333333333333148, 0.4666666666666666741, 0.4749999999999999778, 0.4833333333333333370, 0.4916666666666666408, 0.5000000000000000000, 0.5083333333333333037, 0.5097603473456372436 ),
 .UNSPECIFIED. ) 
 CURVE ( )  GEOMETRIC_REPRESENTATION_ITEM ( )  RATIONAL_B_SPLINE_CURVE ( ( 0.9442986539893905018, 0.9055169669945422051, 1.000000000000000000, 0.8660254037844387076, 1.000000000000000000, 0.8660254037844387076, 1.000000000000000000, 0.8660254037844387076, 1.000000000000000000, 0.8660254037844387076, 1.000000000000000000, 0.8660254037844387076, 1.000000000000000000, 0.8660254037844387076, 1.000000000000000000, 0.8660254037844387076, 1.000000000000000000, 0.8660254037844387076, 1.000000000000000000, 0.8660254037844387076, 1.000000000000000000, 0.8660254037844387076, 1.000000000000000000, 0.8660254037844387076, 1.000000000000000000, 0.8660254037844387076, 1.000000000000000000, 0.8660254037844387076, 1.000000000000000000, 0.8660254037844387076, 1.000000000000000000, 0.8660254037844387076, 1.000000000000000000, 0.8660254037844387076, 1.000000000000000000, 0.8660254037844387076, 1.000000000000000000, 0.8660254037844387076, 1.000000000000000000, 0.8660254037844387076, 1.000000000000000000, 0.8660254037844387076, 1.000000000000000000, 0.8660254037844387076, 1.000000000000000000, 0.8660254037844387076, 1.000000000000000000, 0.8660254037844387076, 1.000000000000000000, 0.8660254037844387076, 1.000000000000000000, 0.8660254037844387076, 1.000000000000000000, 0.8660254037844387076, 1.000000000000000000, 0.8660254037844387076, 1.000000000000000000, 0.8660254037844387076, 1.000000000000000000, 0.9770579648689160512, 0.9619731950825103350 ) ) 
 REPRESENTATION_ITEM ( '' )  );
#49228 = CARTESIAN_POINT ( 'NONE',  ( 6.938893903907228378E-15, 10.64264068711930733, 1.214306433183764966E-14 ) ) ;
#49229 = CARTESIAN_POINT ( 'NONE',  ( 5.092401474535850348, -1.059014397921493433, 1.592059587274458510 ) ) ;
#49230 = AXIS2_PLACEMENT_3D ( 'NONE', #165850, #194072, #64090 ) ;
#49231 = CARTESIAN_POINT ( 'NONE',  ( -1.737499999999997824, -0.9916666666666684726, 3.009438278150925683 ) ) ;
#49232 = CARTESIAN_POINT ( 'NONE',  ( 2.021152898351881166, 2.110506920502265960, 0.8154138738461161884 ) ) ;
#49233 = CARTESIAN_POINT ( 'NONE',  ( -9.327646496521984076, 11.90534021740758064, -1.443375672974059665 ) ) ;
#49234 = CARTESIAN_POINT ( 'NONE',  ( 1.792921450925293536, -0.09139298786187435852, -1.809423198457478676 ) ) ;
#49235 = CARTESIAN_POINT ( 'NONE',  ( 2.237376970375870577, 0.5068087052534899772, -1.847417656071285608 ) ) ;
#49236 = CARTESIAN_POINT ( 'NONE',  ( 2.576698201331685922, 1.354182300986291887, -1.566139152919379107 ) ) ;
#49237 = CARTESIAN_POINT ( 'NONE',  ( -1.364683531250014514, 1.301041667008083325, -0.7879004041258289570 ) ) ;
#49238 = CARTESIAN_POINT ( 'NONE',  ( 1.815242386724497337, -0.2434097785052463103, 1.956328700473447979 ) ) ;
#49239 = CARTESIAN_POINT ( 'NONE',  ( 5.180268977979770817, -1.068588414017849653, 1.602784418908353548 ) ) ;
#49241 = CARTESIAN_POINT ( 'NONE',  ( 6.381672224870991172, 6.819330018336470012, -0.5576268912585117254 ) ) ;
#49240 = CARTESIAN_POINT ( 'NONE',  ( 1.049971938256549109, -1.822247386521518298, -1.415841994891045674 ) ) ;
#49242 = CARTESIAN_POINT ( 'NONE',  ( -0.6823417656250003738, 0.9677083336747521747, -1.181850606188749264 ) ) ;
#49243 = CARTESIAN_POINT ( 'NONE',  ( 5.266109189975630045, -2.053049664954803788, 0.1989083462991206031 ) ) ;
#49244 = CARTESIAN_POINT ( 'NONE',  ( -5.656776405399756236, 7.622658444431597680, -1.599625672291256295 ) ) ;
#49245 = CARTESIAN_POINT ( 'NONE',  ( 0.000000000000000000, 9.200000000000020606, -0.3999999999999941380 ) ) ;
#49246 = EDGE_CURVE ( 'NONE', #16779, #55454, #182242, .T. ) ;
#49248 = CARTESIAN_POINT ( 'NONE',  ( 1.499999999999989120, 5.504166666666685970, 0.8660254037844524744 ) ) ;
#49247 = CARTESIAN_POINT ( 'NONE',  ( 0.01252217983070766719, -0.9030397145437498718, -1.901010321977952389 ) ) ;
#49249 = CARTESIAN_POINT ( 'NONE',  ( 1.364683531249988535, 3.176041667008084435, 0.7879004041258500513 ) ) ;
#49250 = CARTESIAN_POINT ( 'NONE',  ( 4.481803774187195444, 1.408218611193782221, 1.640057829624480101 ) ) ;
#49251 = CARTESIAN_POINT ( 'NONE',  ( 5.584630649692731375, -1.279725605644935760, 1.562507038963067973 ) ) ;
#49252 = CARTESIAN_POINT ( 'NONE',  ( 0.000000000000000000, 13.88000000000000078, 0.000000000000000000 ) ) ;
#49253 = CARTESIAN_POINT ( 'NONE',  ( -4.555176424511596878, 7.297827681030051750, 1.082531754730560403 ) ) ;
#49256 = CARTESIAN_POINT ( 'NONE',  ( 3.823036129373602154, 6.443664003369091731, -1.082531754730548412 ) ) ;
#49255 = CARTESIAN_POINT ( 'NONE',  ( 0.000000000000000000, -1.596874999522041705, -3.793834371823813001 ) ) ;
#49254 = CARTESIAN_POINT ( 'NONE',  ( 7.849244587668864348, 8.122149871893999062, 0.7998128361456291469 ) ) ;
#49257 = CARTESIAN_POINT ( 'NONE',  ( -3.820365424000704557, 7.679119771301277098, -0.7998128361456481317 ) ) ;
#49258 = CARTESIAN_POINT ( 'NONE',  ( 3.766814776335784209, -0.2024620155892907503, -2.006371719556559796 ) ) ;
#49259 = CARTESIAN_POINT ( 'NONE',  ( -8.040148788103921973, 9.338927326664741457, 1.199719254218462483 ) ) ;
#49261 = CARTESIAN_POINT ( 'NONE',  ( -10.99126615174920651, -5.199999999999992184, 0.4382560683119312572 ) ) ;
#49260 = CARTESIAN_POINT ( 'NONE',  ( -3.440018289565379028, 5.036440642624797626, 1.599625672291267398 ) ) ;
#49262 = CARTESIAN_POINT ( 'NONE',  ( 1.364683531249990311, 4.863541667008084879, 0.7879004041258500513 ) ) ;
#49264 = CARTESIAN_POINT ( 'NONE',  ( -1.402160292154681736E-14, 9.421875000341398021, 1.575800808251682339 ) ) ;
#49263 = CARTESIAN_POINT ( 'NONE',  ( 4.645497774645744649, -1.668943667408796294, -1.373881373981879594 ) ) ;
#49265 = SURFACE_STYLE_USAGE ( .BOTH. , #66527 ) ;
#49266 = CARTESIAN_POINT ( 'NONE',  ( -11.63072395171695028, 7.359443703391274738, -2.774425872105819035 ) ) ;
#49268 = CARTESIAN_POINT ( 'NONE',  ( 5.607046053289695742, -0.04666138757647777385, 2.016035322322209389 ) ) ;
#49267 = CARTESIAN_POINT ( 'NONE',  ( -8.337901282280023807, 8.829899038855916871, 0.7216878364870438212 ) ) ;
#49269 = CARTESIAN_POINT ( 'NONE',  ( 0.6823417656249882723, -0.01145833299191073573, -1.181850606188749264 ) ) ;
#49270 = CARTESIAN_POINT ( 'NONE',  ( 0.7149654600043838792, -0.2576282674517544335, 1.705390864826474839 ) ) ;
#49271 = CARTESIAN_POINT ( 'NONE',  ( 3.736153849017632922, 6.516540702899320081, -1.199719254218453823 ) ) ;
#49272 = AXIS2_PLACEMENT_3D ( 'NONE', #87423, #201136, #18120 ) ;
#49274 = CARTESIAN_POINT ( 'NONE',  ( 6.692885107001518286, 7.837396042037102717, -1.199719254218452047 ) ) ;
#49273 = CARTESIAN_POINT ( 'NONE',  ( 7.782016984564054773, 10.10210578678999482, 1.443375672974076540 ) ) ;
#49275 = CARTESIAN_POINT ( 'NONE',  ( -11.75631475800592973, 8.608613766629060748, -2.422433509477694535 ) ) ;
#49276 = CARTESIAN_POINT ( 'NONE',  ( 6.731728662460410462, -1.222180481402233898, -1.416172877279207931 ) ) ;
#49277 = CARTESIAN_POINT ( 'NONE',  ( 0.4342398884448725460, -1.078799894535716231, -1.699460183843485073 ) ) ;
#49278 = DIRECTION ( 'NONE',  ( 0.000000000000000000, 1.000000000000000000, 0.000000000000000000 ) ) ;
#49279 = CARTESIAN_POINT ( 'NONE',  ( 2.968872451268290913, 5.447139712246216625, -1.082531754730543971 ) ) ;
#49280 = CARTESIAN_POINT ( 'NONE',  ( 3.118423654462946892, -1.086285162511631652, -1.920806481261853493 ) ) ;
#49281 =( BOUNDED_SURFACE ( )  B_SPLINE_SURFACE ( 3, 3, ( 
 ( #36285, #117618, #152190, #183611, #3759, #58953, #24293, #27516, #9135, #42733, #92310, #173553, #110422, #177490, #28032, #161236, #12823, #128808, #46426, #33867, #149768, #136722, #186515, #38146, #104219, #83678, #68483, #168143, #184375, #123756, #188655, #189718, #41370, #89045, #6686, #121611, #107482, #173506, #155102, #204877, #172672, #11210, #126127, #43752, #155344, #141274, #89293, #156420, #192087, #75165, #209399, #109866, #140190, #143403, #91434, #191023, #6926, #73004, #205132, #42690, #35810, #108096, #119264, #25698, #3289, #91806, #152769, #157864, #169014, #85632, #121421, #4350, #202555, #87768, #167952, #19555, #54207, #9457, #120345, #69357, #20612, #186321, #37956, #104029, #21662, #5415, #141640, #185249, #36872, #75529, #207649, #102955, #59269, #71493, #137605, #125425, #26769, #83491, #177159, #140428, #51424, #14634, #212838, #114362, #164116, #27931, #174211, #90817, #206668, #127659, #25784, #75618, #42071, #194687, #46329, #108185, #59360, #125517, #100385, #150222, #133997, #96156, #200003, #64685, #87343, #88416, #6062, #204254, #101451, #63121, #52201, #73231, #55938, #24479, #184843, #108678, #142213, #127087, #209283, #42575, #11094, #59859, #208227, #159495, #193050, #126011, #43638, #76109, #174706, #92396, #109753, #175763, #27356, #158434, #26282, #93458, #143292, #60930, #44704, #10035, #40964, #107071, #91860, #42038, #165350, #149099, #66746, #166417, #18010, #183730, #101417, #19085, #185300, #116108, #67269, #115054, #16397, #166946, #86751, #132344, #33730, #134476, #88905, #172787, #161874, #97944, #59567, #128921, #44410, #47617, #15063, #49717, #61187, #127347, #173901, #141421, #59047, #406, #59605, #173382, #192788, #91068, #111115, #201830, #31073, #29998, #96083, #45198, #195697, #175195, #164257, #197806, #170129, #3341, #70471, #85683, #202608, #87825, #135518, #53188, #119316, #38402, #103405, #169466, #65619, #178361, #186490, #41345, #44537, #73707, #166800, #32414, #50790, #149362, #85422, #180791, #82215, #33473, #116919, #133146, #944, #147246, #2008, #64902, #16131, #67009, #115853, #151506, #35596, #181838, #182920, #199146, #34535, #100606, #167744, #197039, #166682, #18274, #84356, #48675, #15071, #131050, #99547, #148309, #165611, #150446, #68074, #134210, #200220, #49724, #3075, #47624, #65938, #179742, #83274, #51871, #17200, #164546, #117992, #130001, #195991, #183985, #214307, #132087, #114791, #101674, #98480, #198097, #19343, #113736, #31359, #97434, #163489, #81163, #213273, #72357, #154701, #86492, #155770, #4143, #169867, #6284, #55065, #24679, #189326, #121215, #122291, #138460, #204479, #56132, #107075, #136325, #39889, #105999, #188248, #202343, #168804, #70213, #187184, #21458, #38811, #172020, #23611, #89721, #7354, #203412, #173098, #90785, #104897, #170936, #20410, #22535, #120134, #53995, #73433, #137394, #139536, #88644, #205561, #156848, #57201, #69146, #123361, #119053, #135267, #201281, #40967, #152556, #52922, #185038, #36663, #102749, #186111, #37745, #103820, #87566, #153634, #5207, #71280, #142754, #96122, #209826, #59328, #93993, #176294, #76640, #108153, #191447, #158971, #61462, #11636, #160034, #10565, #206635, #192513, #190381, #207708, #9513, #44165, #144891, #77709, #157918, #140623, #141695, #91863, #143830, #42041 ),
 ( #75585, #112415, #174179, #127628, #12692, #193592, #27898, #8432, #74520, #126552, #25750, #110285, #26821, #45236, #111351, #125485, #43112, #30036, #177356, #28970, #175237, #92925, #109227, #210898, #95053, #161104, #58266, #78768, #124423, #208763, #62525, #60388, #46300, #128687, #194656, #178427, #163241, #214062, #116662, #34280, #149103, #79840, #63598, #182660, #129752, #100353, #15885, #14823, #98241, #166421, #180541, #97188, #682, #164296, #65690, #99305, #162177, #113485, #81969, #198893, #148056, #80915, #32164, #197846, #49478, #131838, #115598, #181592, #150189, #196793, #147005, #66749, #18013, #114550, #84102, #165353, #31114, #195737, #213023, #179492, #64658, #33221, #199970, #130800, #16947, #1758, #48434, #83026, #132890, #13763, #145948, #50539, #67815, #133962, #211959, #183734, #51618, #117741, #35340, #47372, #89458, #39618, #21203, #19088, #72095, #3885, #68892, #153374, #69955, #103560, #204217, #168553, #52668, #105722, #86237, #53740, #85168, #151252, #136067, #7092, #171752, #101420, #88378, #202080, #185851, #36410, #118797, #201025, #73165, #2821, #135011, #152308, #154445, #87305, #189070, #6026, #119872, #186927, #54808, #169619, #184784, #37483, #4945, #138205, #104635, #38559, #71021, #102489, #137135, #20152, #203163, #120956, #170682, #23347, #22269, #55870, #122026, #187993, #155511, #139271, #205301, #56940, #123112, #167492, #43911, #126290, #11370, #8180, #176039, #94795, #93731, #77450, #128434, #172839, #191184, #90524, #208498, #27631, #76382, #75323, #111087, #210647, #106809, #142491, #141440, #125226, #190128, #110025, #9252, #157654, #159771, #60133, #62273, #91604, #207446, #158711, #143568, #209560, #192249, #58002, #127363, #41783, #59065, #61205, #26560, #40705, #160844, #92667, #193333, #44979, #177094, #28709, #78515, #107897, #12436, #144632, #24410, #173923, #140357, #25496, #10308, #42851, #156586, #74264, #206375, #124166, #108958, #174978, #83841, #149930, #180295, #81720, #145704, #147802, #30858, #47112, #426, #48186, #132637, #114297, #32972, #1499, #31918, #67565, #49235, #29783, #17751, #194401, #66498, #63339, #131590, #46043, #197591, #97996, #112164, #95867, #161922, #178167, #13513, #198643, #129498, #115354, #79585, #181345, #164054, #211703, #195479, #166163, #113229, #179233, #96935, #99048, #15633, #162985, #165103, #14566, #65439, #213820, #16694, #80662, #146753, #130551, #82780, #148853, #50291, #196543, #212771, #116410, #64407, #182400, #34029, #100103, #55617, #202908, #68639, #51360, #52422, #2568, #136881, #167240, #19900, #105466, #199714, #54552, #4692, #104379, #101154, #120699, #187741, #186674, #170426, #6841, #117484, #69708, #183475, #87048, #38301, #169366, #168303, #203970, #89206, #35082, #20951, #85984, #3630, #134763, #22013, #102232, #36153, #88123, #153121, #155259, #184530, #152060, #37233, #154193, #5761, #70767, #151000, #71841, #200771, #135812, #137949, #119618, #133708, #39369, #185602, #121772, #171499, #23091, #18828, #84912, #118548, #201835, #53480, #103304, #206124, #172582, #74004, #58819, #25243, #124972, #43660, #76134, #109776, #93478, #207193, #176839, #28452, #190933, #174732, #24163, #26304, #123914, #140097, #159517, #141184, #11116, #42597, #126032, #94546, #108703, #160584, #142237, #8996, #92418, #10057 ),
 ( #110834, #57754, #175785, #27377, #208249, #189881, #90266, #41524, #158457, #91343, #59883, #77192, #191995, #143312, #209305, #60952, #72919, #139024, #127109, #193074, #156333, #44725, #107636, #173668, #205048, #56691, #122858, #188819, #40453, #106555, #7919, #157404, #75071, #62027, #50033, #182144, #98794, #95619, #163800, #33775, #15376, #212517, #116158, #128183, #198393, #194144, #45792, #63084, #65190, #146500, #99854, #213568, #129253, #97741, #180042, #80403, #111913, #195224, #162736, #131344, #81470, #147547, #14308, #210386, #196289, #177913, #211449, #13263, #47935, #148606, #197339, #161669, #144386, #145453, #79335, #48980, #29527, #112974, #12191, #78262, #115099, #181095, #32712, #46861, #164848, #66242, #16440, #82519, #178986, #30600, #64159, #96687, #31664, #175, #114048, #130301, #132391, #121514, #17501, #201582, #200520, #35904, #100902, #20702, #134516, #68387, #86795, #185347, #187486, #2310, #118292, #69452, #152862, #4440, #36969, #184278, #101979, #166991, #153936, #202652, #38050, #149670, #135558, #83588, #18582, #70510, #3383, #203714, #136625, #84660, #137694, #150749, #53228, #120439, #104121, #54301, #1251, #67310, #186413, #133452, #170168, #19650, #52165, #168048, #21756, #85723, #151810, #87864, #119359, #103052, #169105, #165916, #117225, #5505, #71585, #55362, #39116, #199457, #51099, #183222, #34828, #206934, #107378, #93222, #139838, #172320, #158212, #59624, #57500, #125780, #108451, #188555, #138762, #156070, #122592, #40186, #8739, #143054, #90014, #174470, #159254, #7657, #123659, #106299, #105199, #88946, #173401, #23910, #73741, #155000, #126849, #189622, #205866, #124717, #41270, #10855, #43397, #24983, #22832, #75876, #91086, #72664, #157146, #74820, #140920, #207997, #58563, #56433, #109519, #190676, #42336, #6585, #204779, #26046, #76928, #175526, #171236, #92159, #9801, #141983, #191742, #27116, #209049, #60685, #192806, #144129, #31403, #48719, #179783, #63888, #132130, #44465, #162473, #210122, #80133, #62816, #130043, #14046, #11933, #177658, #65980, #196036, #212254, #112710, #61763, #12992, #194956, #97477, #47670, #113781, #46592, #28194, #146237, #78005, #29266, #45531, #163533, #180832, #15118, #193883, #176583, #95358, #127931, #81207, #111646, #145185, #16174, #110581, #147286, #213318, #64942, #161408, #131093, #98527, #197082, #114833, #94289, #160329, #178722, #79067, #32457, #164588, #82258, #211191, #148350, #214350, #128977, #30337, #96422, #68119, #133189, #55907, #166726, #100649, #122064, #6064, #156624, #34577, #150489, #101718, #188028, #204256, #72134, #987, #73204, #199189, #84401, #138242, #184022, #8214, #106847, #35639, #39658, #105766, #171791, #23386, #24450, #50837, #89498, #155552, #7132, #116964, #83318, #182962, #167789, #2048, #22306, #139310, #205339, #56977, #123151, #118036, #90563, #74299, #88418, #154485, #149405, #189108, #18318, #134255, #40741, #51913, #172878, #198139, #49770, #115896, #181881, #33518, #99590, #165656, #17243, #67052, #200262, #9289, #77485, #161958, #143604, #126325, #178204, #41820, #112198, #190166, #107933, #191221, #193370, #60168, #13548, #127398, #42885, #111125, #173958, #61241, #194437, #45015, #177128, #140395, #58038, #76413, #25531, #93765, #28745, #176072, #175011, #210681, #95905, #206414, #27670 ),
 ( #43944, #94829, #209597, #11408, #157691, #12476, #75362, #26598, #160881, #192284, #124202, #46078, #110060, #78551, #144668, #62310, #128469, #29821, #207481, #91639, #141474, #59101, #125261, #108994, #92699, #159804, #158745, #10339, #142523, #208532, #50324, #100134, #213854, #183509, #35118, #65475, #181383, #30895, #33006, #130587, #146790, #166196, #147837, #17787, #131625, #132673, #101189, #197624, #167278, #148889, #129533, #117516, #79620, #83874, #163020, #16728, #145739, #82812, #49268, #211739, #195514, #51396, #47150, #113267, #196577, #198679, #115389, #63377, #66531, #48219, #165137, #99085, #462, #179271, #114332, #15668, #116442, #182436, #34063, #81755, #96972, #149966, #14602, #64443, #80699, #1535, #67597, #133743, #212806, #180327, #31949, #98033, #199751, #164087, #119650, #205081, #84947, #22045, #104411, #187772, #185634, #39404, #88156, #102263, #52454, #69740, #36187, #168338, #136915, #56723, #3663, #154224, #72952, #135845, #37267, #19933, #18863, #2605, #87082, #86019, #152092, #68674, #40486, #103337, #201868, #38334, #53516, #6874, #171530, #153152, #151036, #204000, #169399, #200803, #70802, #20985, #4727, #121805, #202942, #184567, #23123, #54586, #120733, #134797, #118579, #186706, #139054, #89240, #170460, #5796, #71873, #137983, #55649, #105498, #155291, #122891, #188850, #106590, #159554, #176877, #93513, #192033, #45828, #172618, #76168, #57787, #208284, #190966, #43696, #142273, #140133, #91380, #194183, #27415, #109813, #125009, #42632, #173703, #160623, #209342, #44764, #156367, #59915, #24194, #25278, #77228, #10094, #210424, #11151, #157440, #144422, #9034, #126072, #127143, #110872, #143347, #90297, #74043, #193115, #206159, #28489, #26343, #75108, #108741, #94580, #174768, #107674, #60990, #92456, #175822, #12224, #7951, #123947, #158495, #78297, #62066, #141219, #128221, #189916, #41561, #207229, #58853, #114088, #99890, #146540, #179022, #164884, #180079, #165952, #212559, #30640, #16478, #66282, #64198, #132429, #115136, #195264, #145492, #162773, #129288, #46898, #15416, #149708, #96724, #181131, #17536, #14351, #130339, #113013, #111949, #95657, #31702, #80441, #196328, #161708, #133491, #47972, #97777, #131380, #163837, #83625, #50076, #81506, #29565, #82558, #147585, #79373, #213603, #65229, #197376, #211, #49017, #63124, #116197, #32752, #98834, #13300, #211487, #148645, #1288, #182184, #177951, #198430, #33811, #67346, #199494, #68425, #150786, #200556, #155038, #2349, #38089, #55398, #186452, #70547, #138798, #51138, #169144, #134553, #86833, #69488, #136666, #20738, #18620, #184315, #72703, #120479, #202691, #3422, #135596, #52204, #39154, #87901, #137735, #34864, #152897, #117261, #118330, #170208, #103087, #88985, #104160, #35939, #22869, #102019, #4476, #5541, #203754, #21792, #183260, #167025, #71622, #84699, #121552, #119397, #168087, #201617, #187523, #53266, #19687, #153974, #185386, #54341, #105236, #100938, #85765, #37005, #171277, #6624, #151845, #8774, #26086, #92202, #206970, #158252, #74857, #9840, #174511, #172358, #123696, #11969, #59661, #75916, #157179, #140959, #205904, #192844, #27156, #76968, #188593, #142019, #56469, #57538, #109561, #42377, #28232, #191781, #189657, #176620, #41308, #108487, #159294, #143095, #43437, #122631, #106336, #10893 ),
 ( #208034, #204818, #156111, #58600, #93260, #124755, #107416, #190715, #125820, #175565, #209088, #60723, #126886, #44503, #25020, #173441, #110620, #94325, #160366, #78043, #40225, #73777, #23947, #91120, #7694, #139873, #90052, #181922, #129017, #213353, #198173, #194994, #162512, #145223, #144167, #127969, #212291, #211228, #62854, #193921, #165691, #14083, #161448, #163574, #46628, #132167, #82295, #63924, #61800, #114869, #112751, #111684, #196074, #178763, #146279, #32491, #30376, #95396, #148388, #96462, #80173, #45567, #177691, #130079, #49806, #214389, #210159, #131129, #47706, #113821, #79105, #13028, #29302, #179820, #33552, #31439, #197118, #66018, #64975, #15157, #17280, #97518, #81243, #147325, #48756, #180870, #98565, #164626, #16211, #115932, #99625, #182997, #70291, #87642, #4222, #102827, #171016, #83356, #201358, #34614, #119135, #101755, #168882, #52999, #50875, #2085, #104975, #152635, #20486, #35677, #167822, #84435, #71359, #120214, #169946, #67088, #185115, #149441, #150524, #202423, #135344, #121288, #136407, #68158, #55142, #134292, #36741, #37821, #21532, #54078, #1023, #199228, #103899, #116997, #153713, #151587, #200297, #19422, #5282, #85500, #18357, #186188, #3154, #86572, #137475, #133222, #100684, #69225, #203489, #187264, #51950, #38890, #166762, #118072, #184059, #174248, #60458, #89800, #207770, #59397, #157990, #155845, #122370, #23690, #8510, #189399, #74591, #125553, #25820, #191514, #43179, #156921, #126615, #192578, #140694, #124493, #188326, #190452, #73512, #7431, #109292, #90857, #175302, #206710, #75655, #44233, #58337, #110354, #91930, #72433, #22613, #88721, #26888, #106074, #9578, #154780, #141762, #42110, #6364, #138535, #208828, #204558, #56206, #139615, #92991, #108223, #39967, #159036, #205637, #10629, #76704, #142821, #172097, #57275, #123437, #41041, #107150, #173175, #24755, #65754, #162239, #63662, #127694, #129816, #12756, #29038, #196855, #30098, #114612, #96188, #14882, #131901, #13825, #49537, #31174, #11702, #214125, #197908, #48494, #45296, #113550, #176357, #179553, #79899, #27965, #77776, #148125, #143896, #209890, #78830, #80976, #146008, #94058, #163301, #144951, #47435, #195798, #212018, #61528, #210957, #112479, #147066, #97247, #213087, #178488, #160099, #64717, #193654, #161170, #177420, #130859, #98300, #180603, #111416, #95121, #62584, #128746, #32228, #194720, #46359, #164363, #15948, #82031, #201095, #86308, #83092, #36483, #169689, #168620, #152379, #203237, #33283, #51690, #165420, #68962, #102560, #151322, #150259, #185922, #71098, #181657, #2890, #1827, #200038, #50603, #184856, #84170, #18082, #20222, #135082, #137216, #166491, #67886, #19160, #3958, #118870, #52736, #132957, #202159, #116728, #134031, #70025, #117812, #136141, #115663, #53817, #119947, #37557, #103637, #21277, #153451, #182728, #87383, #5024, #99368, #34347, #748, #100420, #101490, #183802, #167560, #17016, #149171, #66814, #35412, #198960, #85234, #190201, #188066, #154521, #55949, #40784, #7172, #106889, #25569, #58079, #91681, #75402, #189147, #158785, #10382, #172916, #156662, #6101, #8254, #105806, #122102, #141515, #123186, #207523, #24491, #107969, #76458, #90602, #142566, #124241, #104710, #92740, #54881, #59142, #138278, #206452, #121035, #41860, #74338, #187002, #170759 ),
 ( #23424, #139349, #204292, #72170, #39696, #171831, #38633, #89535, #173997, #125300, #157733, #140440, #22348, #88460, #9330, #155587, #191259, #73242, #42924, #109034, #205379, #57017, #175053, #26640, #49048, #111169, #177170, #11452, #33842, #245, #198463, #126367, #65260, #208573, #143647, #148677, #213634, #149744, #16508, #209641, #83654, #61282, #131407, #132461, #50107, #82590, #192326, #110103, #116228, #176114, #182219, #78590, #127443, #160924, #99923, #28787, #77526, #66317, #12518, #197407, #32787, #60206, #193414, #115168, #165984, #181163, #45057, #94870, #17570, #98863, #43985, #147616, #1321, #164915, #27714, #67382, #93808, #159849, #188778, #25205, #145141, #62769, #177611, #105429, #89171, #211147, #155223, #128933, #41491, #40416, #123879, #194910, #206086, #122819, #29223, #189844, #91310, #124937, #187704, #138988, #107603, #12945, #8961, #205009, #6804, #190900, #75036, #173634, #141151, #157367, #178676, #7881, #106519, #95313, #46548, #140064, #112668, #42564, #56656, #72880, #24130, #172545, #90232, #207160, #14005, #156297, #108666, #30291, #73969, #57721, #58783, #39332, #171465, #161362, #79025, #96377, #23053, #212208, #162428, #80089, #146193, #63844, #117718, #98220, #166396, #52645, #49455, #183708, #202056, #35316, #17987, #3859, #81947, #152285, #15862, #148030, #16922, #19064, #100329, #53716, #167468, #83002, #51594, #133940, #34257, #65666, #149078, #116640, #85142, #101394, #151229, #182635, #164272, #150165, #214040, #165329, #181569, #1733, #102464, #2798, #115573, #131814, #99281, #33198, #68870, #197823, #66723, #69932, #32140, #134990, #201000, #118775, #656, #184759, #20128, #36386, #168530, #180519, #132866, #198870, #86214, #50517, #84077, #136044, #67790, #199947, #141416, #123089, #105699, #157631, #21179, #91579, #169597, #87282, #170659, #172814, #39596, #207423, #106786, #22246, #205276, #73140, #187968, #4921, #88356, #55846, #24386, #189046, #56916, #122002, #103537, #89433, #153351, #104612, #120929, #155484, #41758, #40683, #54782, #37458, #38534, #203140, #90499, #70998, #5999, #9229, #185827, #156562, #8157, #74241, #137111, #140334, #173896, #206353, #57980, #119849, #186902, #171726, #154421, #139245, #124143, #7067, #72070, #190105, #75301, #138180, #107870, #204190, #23325, #25472, #128413, #27610, #176018, #194380, #78494, #14543, #110005, #11348, #177072, #46023, #62252, #144611, #76361, #145682, #208476, #159751, #210626, #93710, #29760, #80640, #211680, #112142, #178146, #95845, #161901, #96912, #126271, #13488, #79563, #63316, #192228, #158689, #60112, #44958, #77429, #111066, #129477, #195459, #47088, #113206, #193312, #162964, #146732, #28688, #160822, #10287, #12414, #143546, #43891, #179211, #127342, #30836, #94774, #59042, #125200, #191163, #42830, #108936, #174957, #26539, #92647, #142468, #209540, #61182, #16671, #17727, #182374, #180272, #131566, #19878, #67542, #83815, #165080, #82756, #213794, #200748, #35058, #84889, #196520, #34004, #64384, #65417, #117460, #50268, #36127, #199689, #197567, #184509, #49211, #116386, #167217, #150976, #51333, #130529, #114275, #18804, #31896, #2541, #66473, #115331, #148829, #68616, #402, #147778, #183453, #132614, #100078, #149908, #212750, #164032, #198621, #101129, #166140, #15607, #97973, #1475, #133684 ),
 ( #81694, #181322, #32950, #99024, #134741, #52397, #102212, #118524, #168277, #85961, #48163, #170401, #153097, #152037, #135789, #5737, #4672, #70745, #201813, #173646, #21989, #169344, #171478, #136858, #72895, #37208, #203947, #88098, #122833, #54530, #119595, #55594, #120675, #154171, #40430, #202882, #103282, #90244, #186653, #104356, #53457, #185578, #38279, #57734, #7894, #3608, #139001, #71816, #137926, #87025, #20928, #121749, #187717, #41502, #39346, #205023, #105442, #23068, #89184, #155236, #188794, #6817, #106532, #172558, #56669, #107615, #25219, #24142, #156310, #73982, #140076, #206100, #123891, #189857, #69685, #32421, #14009, #147249, #49731, #80095, #181844, #191974, #31364, #8975, #146199, #180796, #174709, #97440, #115859, #163496, #212213, #132093, #207172, #65944, #141164, #58796, #142216, #213281, #63850, #91323, #81169, #208230, #179746, #47631, #162433, #190913, #59862, #30296, #64907, #15079, #131056, #96381, #75049, #130006, #124951, #76112, #92399, #195997, #16137, #197044, #26285, #42578, #10038, #158437, #48681, #108681, #43641, #198102, #157381, #114797, #98488, #164551, #126014, #82222, #148313, #214312, #112673, #178683, #113742, #183989, #83282, #201287, #20416, #69152, #68082, #103825, #203417, #99553, #135272, #134217, #117999, #182925, #102757, #2013, #150452, #168812, #52928, #55073, #84361, #200226, #151514, #86498, #36668, #119062, #50798, #120140, #34541, #51877, #185044, #35603, #4150, #121222, #186118, #152563, #70221, #136332, #202352, #71287, #100611, #54002, #37751, #169873, #166687, #133151, #137400, #19349, #21463, #199153, #87572, #101680, #18278, #153642, #167750, #5212, #85429, #33480, #165618, #3082, #17206, #149367, #949, #67015, #116925, #59337, #56138, #124431, #208767, #190389, #173106, #10573, #88650, #158976, #22544, #154710, #23620, #25757, #107084, #60395, #174186, #89729, #58275, #140629, #40973, #72365, #155777, #123367, #91870, #42047, #108158, #189334, #170944, #156854, #6291, #172027, #188256, #8439, #109233, #157925, #122299, #104903, #106006, #39897, #9519, #138466, #73439, #76647, #38820, #75591, #141703, #207714, #204488, #125491, #26829, #191453, #43118, #187192, #7362, #24686, #139543, #206642, #175243, #74527, #205569, #92932, #142762, #57207, #90790, #161111, #210904, #61469, #195743, #95062, #28977, #47380, #145955, #81976, #177363, #78775, #30042, #113493, #129759, #211965, #143837, #213033, #127634, #12697, #63604, #144896, #97195, #148064, #64663, #179499, #31121, #163248, #14830, #164303, #193599, #80921, #147010, #130809, #45241, #11644, #111358, #112422, #62531, #178436, #196799, #48441, #114556, #180549, #46306, #15892, #32170, #98247, #214070, #128693, #77715, #194661, #96131, #162184, #13770, #126559, #192519, #44173, #110292, #79846, #176301, #27904, #94001, #160040, #209832, #19095, #116668, #132896, #86245, #133969, #3892, #199978, #118805, #21211, #51625, #153382, #166430, #2830, #197853, #117750, #152315, #149109, #68899, #87315, #135018, #183740, #103569, #181600, #37493, #115605, #33228, #182666, #184791, #35350, #65696, #52675, #34288, #151258, #85174, #101426, #165361, #100360, #1766, #36417, #201032, #102495, #67823, #49484, #167497, #99311, #50546, #66755, #168559, #202090, #20158, #689, #16954, #198900, #18021, #69964, #83035 ) ),
 .UNSPECIFIED., .T., .F., .T. ) 
 B_SPLINE_SURFACE_WITH_KNOTS ( ( 4, 3, 4 ),
 ( 4, 1, 1, 1, 1, 1, 1, 1, 1, 1, 1, 1, 1, 1, 1, 1, 1, 1, 1, 1, 1, 1, 1, 1, 1, 1, 1, 1, 1, 1, 1, 1, 1, 1, 1, 1, 1, 1, 1, 1, 1, 1, 1, 1, 1, 1, 1, 1, 1, 1, 1, 1, 1, 1, 1, 1, 1, 1, 1, 1, 1, 1, 1, 1, 1, 1, 1, 1, 1, 1, 1, 1, 1, 1, 1, 1, 1, 1, 1, 1, 1, 1, 1, 1, 1, 1, 1, 1, 1, 1, 1, 1, 1, 1, 1, 1, 1, 1, 1, 1, 1, 1, 1, 1, 1, 1, 1, 1, 1, 1, 1, 1, 1, 1, 1, 1, 1, 1, 1, 1, 1, 1, 1, 1, 1, 1, 1, 1, 1, 1, 1, 1, 1, 1, 1, 1, 1, 1, 1, 1, 1, 1, 1, 1, 1, 1, 1, 1, 1, 1, 1, 1, 1, 1, 1, 1, 1, 1, 1, 1, 1, 1, 1, 1, 1, 1, 1, 1, 1, 1, 1, 1, 1, 1, 1, 1, 1, 1, 1, 1, 1, 1, 1, 1, 1, 1, 1, 1, 1, 1, 1, 1, 1, 1, 1, 1, 1, 1, 1, 1, 1, 1, 1, 1, 1, 1, 1, 1, 1, 1, 1, 1, 1, 1, 1, 1, 1, 1, 1, 1, 1, 1, 1, 1, 1, 1, 1, 1, 1, 1, 1, 1, 1, 1, 1, 1, 1, 1, 1, 1, 1, 1, 1, 1, 1, 1, 1, 1, 1, 1, 1, 1, 1, 1, 1, 1, 1, 1, 1, 1, 1, 1, 1, 1, 1, 1, 1, 1, 1, 1, 1, 1, 1, 1, 1, 1, 1, 1, 1, 1, 1, 1, 1, 1, 1, 1, 1, 1, 1, 1, 1, 1, 1, 1, 1, 1, 1, 1, 1, 1, 1, 1, 1, 1, 1, 1, 1, 1, 1, 1, 1, 1, 1, 1, 1, 1, 1, 1, 1, 1, 1, 1, 1, 1, 1, 1, 1, 1, 1, 1, 1, 1, 1, 1, 1, 1, 1, 1, 1, 1, 1, 1, 1, 1, 1, 1, 1, 1, 1, 1, 1, 1, 1, 1, 1, 1, 1, 1, 1, 1, 1, 1, 1, 1, 1, 1, 1, 1, 1, 1, 1, 1, 1, 1, 1, 1, 1, 1, 1, 1, 1, 1, 1, 1, 4 ),
 ( 0.000000000000000000, 0.5000000000000000000, 1.000000000000000000 ),
 ( 0.000000000000000000, 0.002600034503794030130, 0.005208798665460326327, 0.007813183304800875098, 0.01041632952039499814, 0.01302078637366306003, 0.01562487905948694092, 0.01822913957756216313, 0.02083328395591756144, 0.02343739818322774712, 0.02604168118785421884, 0.02864568517727394958, 0.03125004130332968699, 0.03385401862675675722, 0.03645834363201481965, 0.03906241290072134942, 0.04166661303991354287, 0.04427083116291704451, 0.04687488238457573897, 0.04947921467585455341, 0.05208318889621989245, 0.05468754274347345512, 0.05729155431138267807, 0.05989582568988525285, 0.06249996760622017478, 0.06510408932096034551, 0.06770837349117478365, 0.07031237295078232585, 0.07291672927807971161, 0.07552070761765239393, 0.07812503204114096267, 0.08072910085791458468, 0.08333330089851145872, 0.08593751883178461781, 0.08854156980611090078, 0.09114590188302622298, 0.09374987588873062716, 0.09635422952249227124, 0.09895824087764454324, 0.1015625120427016276, 0.1041666537503683765, 0.1067707752516706410, 0.1093750592157429480, 0.1119790584643299974, 0.1145834145867499904, 0.1171873927198607973, 0.1197917169388799108, 0.1223957855539345302, 0.1249999853896588409, 0.1276042031245507580, 0.1302082538950744550, 0.1328125857752754935, 0.1354165595809520839, 0.1380209130188291833, 0.1406249241787864424, 0.1432291951479887082, 0.1458333366646657747, 0.1484374579699756502, 0.1510417417453218114, 0.1536457408005802994, 0.1562500967354857329, 0.1588540746797905134, 0.1614583987117299280, 0.1640624671426803571, 0.1666666667910262079, 0.1692708843450304312, 0.1718749349293641482, 0.1744792666302357464, 0.1770832402535473249, 0.1796875935129024493, 0.1822916044953091785, 0.1848958752860835608, 0.1875000166293293857, 0.1901041377562054102, 0.1927084213602507368, 0.1953124202398235920, 0.1979167760045740521, 0.2005207537777317084, 0.2031250776399721736, 0.2057291459044250093, 0.2083333453828807025, 0.2109375627734847158, 0.2135416131892344249, 0.2161459447281551538, 0.2187499181867580689, 0.2213542712849473904, 0.2239582821074418695, 0.2265625527372090720, 0.2291666939245756707, 0.2317708148905701926, 0.2343750983407339450, 0.2369790970622578097, 0.2395834526742069426, 0.2421874302938704648, 0.2447917540037867212, 0.2473958221193426621, 0.2500000214453905190, 0.2526042386900758108, 0.2552082889548416555, 0.2578126203491843960, 0.2604165936607292231, 0.2630209466151033904, 0.2656249572953180982, 0.2682292277814931625, 0.2708333688305272213, 0.2734374896531870935, 0.2760417729668830367, 0.2786457715479891406, 0.2812501270244852081, 0.2838541045083020076, 0.2864584280832634389, 0.2890624960675178268, 0.2916666952586349781, 0.2942709123748779576, 0.2968749625062547248, 0.2994792937733871119, 0.3020832669555192918, 0.3046876197834237909, 0.3072916303389863768, 0.3098959006989794318, 0.3125000416272227799, 0.3151041623240899980, 0.3177084455187270673, 0.3203124439770417831, 0.3229167993354283839, 0.3255207767010412923, 0.3281251001584127303, 0.3307291680289564662, 0.3333333671026155187, 0.3359375841078879321, 0.3385416341234662174, 0.3411459652807516951, 0.3437499383511121720, 0.3463542910698884647, 0.3489583015184220538, 0.3515625717696388985, 0.3541667125946290073, 0.3567708331832410984, 0.3593751162762241491, 0.3619791146293697692, 0.3645834698869864221, 0.3671874471520340522, 0.3697917705091763874, 0.3723958382835964032, 0.3750000372572658280, 0.3776042541690359799, 0.3802083040864021046, 0.3828126351512001757, 0.3854166081274262856, 0.3880209607544118922, 0.3906249711135359459, 0.3932292412733790488, 0.3958333820126498370, 0.3984375025105409418, 0.4010417855192715542, 0.4036457837848667074, 0.4062501389590495449, 0.4088541161411674008, 0.4114584394154381930, 0.4140625071113177014, 0.4166667060024629166, 0.4192709228381954478, 0.4218749726749327911, 0.4244793036646000717, 0.4270832765643259310, 0.4296876291168554296, 0.4322916394041865784, 0.4348959094900549660, 0.4375000501611374104, 0.4401041705858387276, 0.4427084535277153732, 0.4453124517233759683, 0.4479168068314584583, 0.4505207839482789911, 0.4531251071570330247, 0.4557291747919532399, 0.4583333736180368323, 0.4609375903951940523, 0.4635416401688834398, 0.4661459711007739370, 0.4687499439416310532, 0.4713542964370365795, 0.4739583066701890113, 0.4765625766994796009, 0.4791667173199026797, 0.4817708376889431876, 0.4843751205813623395, 0.4869791187247021202, 0.4895834737840155659, 0.4921874508531692838, 0.4947917740137594000, 0.4973958416052992049, 0.5000000403837819851, 0.5026042571198243714, 0.5052083068480445194, 0.5078126377395105751, 0.5104166105391289010, 0.5130209629947408700, 0.5156249731913270518, 0.5182292431814352618, 0.5208333837687260104, 0.5234375040996330775, 0.5260417869599895990, 0.5286457850686206994, 0.5312501400964950715, 0.5338541171356111503, 0.5364584402653888029, 0.5390625078311259699, 0.5416667065794673608, 0.5442709232918542250, 0.5468749729921829061, 0.5494793038605755298, 0.5520832766365837418, 0.5546876290697317913, 0.5572916392473630243, 0.5598959092156829964, 0.5625000497873680061, 0.5651041700976676685, 0.5677084529433557014, 0.5703124510348895893, 0.5729168060486536929, 0.5755207830753605869, 0.5781251061916765632, 0.5807291737491879768, 0.5833333724848467350, 0.5859375891910368894, 0.5885416388810509325, 0.5911459697437208005, 0.5937499425137473530, 0.5963542949417601768, 0.5989583051180477069, 0.6015625750819736384, 0.6041667156555785567, 0.6067708359627971282, 0.6093751188112106476, 0.6119791169032582356, 0.6145834719202413199, 0.6171874489521673723, 0.6197917720723722379, 0.6223958396392350600, 0.6250000383796699976, 0.6276042550971219214, 0.6302083047943985994, 0.6328126356686964993, 0.6354166084503697354, 0.6380209608905765828, 0.6406249710831318778, 0.6432292410600577437, 0.6458333816531092175, 0.6484375019747732338, 0.6510417848433065480, 0.6536457829534795261, 0.6562501379910111732, 0.6588541150457848383, 0.6614584381872300467, 0.6640625057810221055, 0.6666667045436925898, 0.6692709212898660942, 0.6718749710119833463, 0.6744793019152608426, 0.6770832747262099938, 0.6796876271959411131, 0.6822916374223763070, 0.6848959074296973037, 0.6875000480597228680, 0.6901041684133596421, 0.6927084513194080584, 0.6953124494653194487, 0.6979168045407300180, 0.7005207816359816375, 0.7031251048160196415, 0.7057291724543196532, 0.7083333712566866058, 0.7109375880490425015, 0.7135416378135795989, 0.7161459687631898108, 0.7187499416210458847, 0.7213542941376326345, 0.7239583044155618596, 0.7265625744706748490, 0.7291667151552034820, 0.7317708355583423252, 0.7343751185193033715, 0.7369791167185673064, 0.7395834718491895998, 0.7421874490025512916, 0.7447917722385364314, 0.7473958399389256657, 0.7500000387984516736, 0.7526042556544531026, 0.7552083054789914263, 0.7578126364922896929, 0.7604166094146853627, 0.7630209619954617661, 0.7656249723425013753, 0.7682292424628052174, 0.7708333832193684509, 0.7734375036895410060, 0.7760417867228139865, 0.7786457849930478181, 0.7812501401962168579, 0.7838541174253229604, 0.7864584407346123518, 0.7890625085146746320, 0.7916667074488250577, 0.7942709243859374935, 0.7968749742880611997, 0.7994793053824050810, 0.8020832783869765725, 0.8046876310492792062, 0.8072916414830481058, 0.8098959116859448804, 0.8125000525320774658, 0.8151041730868179291, 0.8177084562098055898, 0.8203124545686294455, 0.8229168098616829186, 0.8255207871841712119, 0.8281251105841250792, 0.8307291784614470043, 0.8333333774876906519, 0.8359375945233833427, 0.8385416445206798075, 0.8411459757134309712, 0.8437499488178175078, 0.8463543015789862789, 0.8489583121171074831, 0.8515625824200027116, 0.8541667233732427311, 0.8567708440300897399, 0.8593751272601987123, 0.8619791257252362726, 0.8645834811255164176, 0.8671874585590289009, 0.8697917820670107991, 0.8723958500591838527, 0.8750000491949933012, 0.8776042663467393812, 0.8802083164568000884, 0.8828126477653241988, 0.8854166209871692228, 0.8880209738645485906, 0.8906249845246493324, 0.8932292549449527552, 0.8958333960228427317, 0.8984375167993386979, 0.9010418001539796107, 0.9036457987428592187, 0.9062501542677121602, 0.9088541318298947180, 0.9114584554632734203, 0.9140625235878931942, 0.9166667228507454634, 0.9192709401360219523, 0.9218749903764450471, 0.9244793218181143191, 0.9270832951750564987, 0.9296876481859919217, 0.9322916589857459524, 0.9348959295408556525, 0.9375000707608250883, 0.9401041916746273319, 0.9427084751713679101, 0.9453124739016935951, 0.9479168295687272483, 0.9505208072738278169, 0.9531251310501845930, 0.9557291993520028450, 0.9583333987332913750, 0.9609376160454207172, 0.9635416666839513589, 0.9661459986354887786, 0.9687499708159389433, 0.9713543235632202677, 0.9739583390673558494, 0.9765626083347638264, 0.9791667417950460361, 0.9817708662416058107, 0.9843751381318576188, 0.9869792129215403387, 0.9895836736503123010, 0.9921868305638316121, 0.9947912020913856068, 0.9973999845648282569, 1.000000000000000000 ),
 .UNSPECIFIED. ) 
 GEOMETRIC_REPRESENTATION_ITEM ( )  RATIONAL_B_SPLINE_SURFACE ( (
 ( 1.000000000000000222, 1.000000000000000222, 1.000000000000000222, 1.000000000000000222, 0.9999999999999996669, 0.9999999999999997780, 1.000000000000000444, 1.000000000000000000, 1.000000000000000000, 1.000000000000000000, 0.9999999999999997780, 1.000000000000000000, 1.000000000000000000, 1.000000000000000000, 1.000000000000000000, 0.9999999999999997780, 1.000000000000000222, 0.9999999999999996669, 1.000000000000000000, 0.9999999999999997780, 1.000000000000000222, 1.000000000000000000, 1.000000000000000222, 0.9999999999999996669, 1.000000000000000000, 1.000000000000000222, 0.9999999999999996669, 1.000000000000000444, 1.000000000000000000, 0.9999999999999997780, 1.000000000000000222, 1.000000000000000222, 1.000000000000000222, 1.000000000000000000, 1.000000000000000000, 0.9999999999999997780, 1.000000000000000000, 1.000000000000000000, 1.000000000000000000, 1.000000000000000000, 1.000000000000000222, 1.000000000000000222, 1.000000000000000000, 1.000000000000000000, 1.000000000000000000, 0.9999999999999996669, 1.000000000000000222, 1.000000000000000000, 1.000000000000000000, 0.9999999999999997780, 0.9999999999999997780, 1.000000000000000000, 0.9999999999999996669, 1.000000000000000222, 0.9999999999999997780, 1.000000000000000222, 0.9999999999999997780, 0.9999999999999997780, 1.000000000000000222, 1.000000000000000222, 0.9999999999999997780, 1.000000000000000222, 1.000000000000000000, 1.000000000000000222, 1.000000000000000000, 0.9999999999999997780, 1.000000000000000000, 1.000000000000000000, 1.000000000000000222, 1.000000000000000222, 1.000000000000000000, 0.9999999999999997780, 1.000000000000000000, 1.000000000000000222, 0.9999999999999997780, 1.000000000000000444, 0.9999999999999996669, 1.000000000000000000, 1.000000000000000222, 0.9999999999999997780, 0.9999999999999997780, 0.9999999999999997780, 1.000000000000000000, 0.9999999999999997780, 1.000000000000000000, 0.9999999999999997780, 1.000000000000000222, 1.000000000000000000, 1.000000000000000222, 1.000000000000000000, 0.9999999999999997780, 1.000000000000000000, 1.000000000000000000, 0.9999999999999997780, 1.000000000000000222, 1.000000000000000000, 1.000000000000000000, 1.000000000000000000, 1.000000000000000222, 0.9999999999999996669, 1.000000000000000222, 1.000000000000000000, 1.000000000000000000, 0.9999999999999997780, 1.000000000000000000, 0.9999999999999997780, 1.000000000000000000, 1.000000000000000222, 1.000000000000000000, 0.9999999999999997780, 1.000000000000000222, 1.000000000000000222, 0.9999999999999996669, 1.000000000000000222, 1.000000000000000000, 1.000000000000000444, 0.9999999999999996669, 1.000000000000000000, 1.000000000000000222, 1.000000000000000222, 1.000000000000000222, 1.000000000000000222, 1.000000000000000000, 0.9999999999999997780, 1.000000000000000222, 1.000000000000000000, 1.000000000000000222, 0.9999999999999996669, 1.000000000000000000, 1.000000000000000000, 1.000000000000000222, 1.000000000000000222, 0.9999999999999997780, 1.000000000000000000, 0.9999999999999997780, 1.000000000000000222, 1.000000000000000000, 1.000000000000000222, 1.000000000000000000, 1.000000000000000444, 0.9999999999999996669, 1.000000000000000444, 0.9999999999999996669, 0.9999999999999997780, 0.9999999999999997780, 1.000000000000000222, 1.000000000000000000, 0.9999999999999997780, 1.000000000000000000, 0.9999999999999997780, 0.9999999999999996669, 1.000000000000000222, 1.000000000000000000, 0.9999999999999997780, 1.000000000000000000, 1.000000000000000000, 1.000000000000000222, 1.000000000000000000, 1.000000000000000000, 1.000000000000000444, 0.9999999999999997780, 1.000000000000000222, 1.000000000000000222, 0.9999999999999997780, 1.000000000000000444, 0.9999999999999996669, 1.000000000000000000, 0.9999999999999997780, 1.000000000000000222, 0.9999999999999997780, 1.000000000000000222, 1.000000000000000000, 1.000000000000000222, 0.9999999999999997780, 0.9999999999999997780, 1.000000000000000000, 1.000000000000000000, 0.9999999999999997780, 1.000000000000000222, 0.9999999999999997780, 1.000000000000000000, 1.000000000000000000, 1.000000000000000222, 1.000000000000000000, 0.9999999999999997780, 1.000000000000000222, 1.000000000000000444, 1.000000000000000000, 1.000000000000000000, 1.000000000000000000, 1.000000000000000000, 0.9999999999999997780, 1.000000000000000000, 1.000000000000000222, 1.000000000000000000, 1.000000000000000222, 0.9999999999999996669, 1.000000000000000000, 1.000000000000000000, 0.9999999999999994449, 1.000000000000000444, 1.000000000000000000, 1.000000000000000222, 0.9999999999999997780, 1.000000000000000000, 1.000000000000000222, 1.000000000000000000, 0.9999999999999996669, 1.000000000000000444, 0.9999999999999997780, 1.000000000000000444, 0.9999999999999996669, 1.000000000000000000, 0.9999999999999996669, 1.000000000000000444, 1.000000000000000000, 0.9999999999999997780, 1.000000000000000222, 1.000000000000000000, 0.9999999999999997780, 1.000000000000000444, 1.000000000000000222, 0.9999999999999997780, 1.000000000000000000, 1.000000000000000222, 0.9999999999999997780, 1.000000000000000222, 1.000000000000000222, 1.000000000000000000, 1.000000000000000000, 0.9999999999999996669, 1.000000000000000222, 0.9999999999999997780, 1.000000000000000000, 0.9999999999999997780, 1.000000000000000444, 1.000000000000000000, 1.000000000000000000, 0.9999999999999997780, 1.000000000000000444, 1.000000000000000000, 0.9999999999999997780, 1.000000000000000444, 0.9999999999999996669, 1.000000000000000444, 1.000000000000000000, 1.000000000000000444, 1.000000000000000222, 1.000000000000000222, 0.9999999999999997780, 1.000000000000000000, 0.9999999999999997780, 1.000000000000000444, 0.9999999999999996669, 1.000000000000000000, 1.000000000000000000, 1.000000000000000222, 1.000000000000000000, 1.000000000000000222, 1.000000000000000000, 1.000000000000000000, 0.9999999999999997780, 1.000000000000000000, 1.000000000000000000, 0.9999999999999997780, 1.000000000000000000, 1.000000000000000000, 0.9999999999999997780, 1.000000000000000000, 1.000000000000000222, 1.000000000000000000, 1.000000000000000000, 1.000000000000000000, 1.000000000000000000, 0.9999999999999996669, 1.000000000000000222, 1.000000000000000000, 0.9999999999999997780, 1.000000000000000000, 1.000000000000000222, 1.000000000000000000, 1.000000000000000222, 1.000000000000000222, 1.000000000000000000, 1.000000000000000222, 1.000000000000000000, 1.000000000000000000, 1.000000000000000000, 1.000000000000000222, 0.9999999999999996669, 1.000000000000000222, 0.9999999999999996669, 1.000000000000000222, 1.000000000000000222, 1.000000000000000222, 1.000000000000000222, 0.9999999999999996669, 1.000000000000000444, 1.000000000000000000, 1.000000000000000000, 1.000000000000000222, 1.000000000000000444, 0.9999999999999996669, 1.000000000000000444, 1.000000000000000222, 0.9999999999999996669, 1.000000000000000222, 0.9999999999999997780, 1.000000000000000000, 1.000000000000000000, 0.9999999999999997780, 1.000000000000000000, 0.9999999999999997780, 1.000000000000000000, 1.000000000000000000, 1.000000000000000444, 0.9999999999999997780, 1.000000000000000222, 0.9999999999999997780, 0.9999999999999997780, 1.000000000000000000, 1.000000000000000000, 0.9999999999999996669, 1.000000000000000000, 1.000000000000000222, 1.000000000000000222, 0.9999999999999997780, 1.000000000000000222, 0.9999999999999997780, 0.9999999999999997780, 1.000000000000000000, 1.000000000000000000, 1.000000000000000000, 1.000000000000000222, 1.000000000000000000, 1.000000000000000222, 1.000000000000000000, 0.9999999999999996669, 0.9999999999999997780, 1.000000000000000444, 0.9999999999999996669, 1.000000000000000444, 0.9999999999999997780, 0.9999999999999997780, 1.000000000000000222, 0.9999999999999997780, 1.000000000000000222, 1.000000000000000000, 1.000000000000000000, 0.9999999999999997780, 1.000000000000000222, 1.000000000000000222, 1.000000000000000000, 1.000000000000000222, 1.000000000000000000, 1.000000000000000000, 0.9999999999999997780, 1.000000000000000000, 1.000000000000000000, 0.9999999999999997780, 1.000000000000000000, 0.9999999999999996669, 1.000000000000000222, 0.9999999999999997780, 1.000000000000000222, 0.9999999999999997780, 1.000000000000000000, 0.9999999999999997780, 1.000000000000000222, 0.9999999999999997780, 1.000000000000000000, 1.000000000000000000, 1.000000000000000000, 1.000000000000000000, 0.9999999999999997780, 1.000000000000000222, 1.000000000000000000, 0.9999999999999997780, 1.000000000000000000, 1.000000000000000000, 1.000000000000000222, 1.000000000000000222, 1.000000000000000000, 1.000000000000000222, 1.000000000000000000, 1.000000000000000000, 1.000000000000000000),
 ( 0.3333333333333334259, 0.3333333333333334259, 0.3333333333333334259, 0.3333333333333333703, 0.3333333333333333148, 0.3333333333333333703, 0.3333333333333334259, 0.3333333333333333703, 0.3333333333333333703, 0.3333333333333334259, 0.3333333333333332593, 0.3333333333333334259, 0.3333333333333333703, 0.3333333333333333703, 0.3333333333333333703, 0.3333333333333333703, 0.3333333333333333703, 0.3333333333333333148, 0.3333333333333334259, 0.3333333333333333148, 0.3333333333333334259, 0.3333333333333333148, 0.3333333333333333703, 0.3333333333333333703, 0.3333333333333333148, 0.3333333333333334814, 0.3333333333333332593, 0.3333333333333334814, 0.3333333333333333148, 0.3333333333333333148, 0.3333333333333334259, 0.3333333333333333703, 0.3333333333333334814, 0.3333333333333332593, 0.3333333333333334259, 0.3333333333333333703, 0.3333333333333333703, 0.3333333333333333148, 0.3333333333333333703, 0.3333333333333333703, 0.3333333333333334814, 0.3333333333333333703, 0.3333333333333334259, 0.3333333333333333703, 0.3333333333333333148, 0.3333333333333333148, 0.3333333333333333703, 0.3333333333333334259, 0.3333333333333333703, 0.3333333333333333703, 0.3333333333333333148, 0.3333333333333333703, 0.3333333333333332593, 0.3333333333333334259, 0.3333333333333333148, 0.3333333333333333703, 0.3333333333333333703, 0.3333333333333333703, 0.3333333333333333703, 0.3333333333333335369, 0.3333333333333332593, 0.3333333333333334259, 0.3333333333333333703, 0.3333333333333334259, 0.3333333333333334259, 0.3333333333333333148, 0.3333333333333334259, 0.3333333333333334259, 0.3333333333333334259, 0.3333333333333334814, 0.3333333333333333703, 0.3333333333333333148, 0.3333333333333333148, 0.3333333333333333703, 0.3333333333333334259, 0.3333333333333333703, 0.3333333333333333703, 0.3333333333333333703, 0.3333333333333333703, 0.3333333333333333148, 0.3333333333333333703, 0.3333333333333332593, 0.3333333333333333703, 0.3333333333333333148, 0.3333333333333333148, 0.3333333333333333703, 0.3333333333333333703, 0.3333333333333333148, 0.3333333333333333703, 0.3333333333333333703, 0.3333333333333333703, 0.3333333333333333703, 0.3333333333333334259, 0.3333333333333332593, 0.3333333333333334259, 0.3333333333333333148, 0.3333333333333333703, 0.3333333333333333148, 0.3333333333333334814, 0.3333333333333332038, 0.3333333333333335369, 0.3333333333333332593, 0.3333333333333333703, 0.3333333333333333703, 0.3333333333333333148, 0.3333333333333333703, 0.3333333333333333148, 0.3333333333333334259, 0.3333333333333334259, 0.3333333333333332593, 0.3333333333333334814, 0.3333333333333333703, 0.3333333333333332593, 0.3333333333333334814, 0.3333333333333334259, 0.3333333333333334259, 0.3333333333333332593, 0.3333333333333333703, 0.3333333333333333703, 0.3333333333333334259, 0.3333333333333333703, 0.3333333333333334259, 0.3333333333333333703, 0.3333333333333333148, 0.3333333333333334814, 0.3333333333333333703, 0.3333333333333334259, 0.3333333333333333703, 0.3333333333333333703, 0.3333333333333333148, 0.3333333333333334259, 0.3333333333333334259, 0.3333333333333333703, 0.3333333333333333148, 0.3333333333333333148, 0.3333333333333334259, 0.3333333333333334814, 0.3333333333333333148, 0.3333333333333334259, 0.3333333333333334814, 0.3333333333333333148, 0.3333333333333334814, 0.3333333333333332038, 0.3333333333333333703, 0.3333333333333333148, 0.3333333333333333703, 0.3333333333333334259, 0.3333333333333332038, 0.3333333333333334259, 0.3333333333333333148, 0.3333333333333332038, 0.3333333333333334259, 0.3333333333333333148, 0.3333333333333334259, 0.3333333333333332593, 0.3333333333333334259, 0.3333333333333333703, 0.3333333333333334259, 0.3333333333333333703, 0.3333333333333334259, 0.3333333333333333703, 0.3333333333333333703, 0.3333333333333334814, 0.3333333333333333703, 0.3333333333333335369, 0.3333333333333332038, 0.3333333333333333703, 0.3333333333333333703, 0.3333333333333333703, 0.3333333333333333148, 0.3333333333333333703, 0.3333333333333333703, 0.3333333333333334259, 0.3333333333333333148, 0.3333333333333334259, 0.3333333333333333148, 0.3333333333333334814, 0.3333333333333332593, 0.3333333333333333703, 0.3333333333333334259, 0.3333333333333333148, 0.3333333333333333703, 0.3333333333333333148, 0.3333333333333334259, 0.3333333333333332593, 0.3333333333333333703, 0.3333333333333334814, 0.3333333333333333703, 0.3333333333333333703, 0.3333333333333333703, 0.3333333333333333703, 0.3333333333333333148, 0.3333333333333333703, 0.3333333333333333703, 0.3333333333333334259, 0.3333333333333333703, 0.3333333333333333703, 0.3333333333333333703, 0.3333333333333333703, 0.3333333333333332038, 0.3333333333333334814, 0.3333333333333333703, 0.3333333333333333703, 0.3333333333333333148, 0.3333333333333333148, 0.3333333333333334259, 0.3333333333333334259, 0.3333333333333332593, 0.3333333333333335369, 0.3333333333333332593, 0.3333333333333334814, 0.3333333333333332593, 0.3333333333333334259, 0.3333333333333332038, 0.3333333333333335369, 0.3333333333333333148, 0.3333333333333333703, 0.3333333333333334259, 0.3333333333333333148, 0.3333333333333333148, 0.3333333333333335369, 0.3333333333333334259, 0.3333333333333333703, 0.3333333333333333148, 0.3333333333333334259, 0.3333333333333333148, 0.3333333333333334259, 0.3333333333333334259, 0.3333333333333333703, 0.3333333333333333703, 0.3333333333333333148, 0.3333333333333333703, 0.3333333333333333703, 0.3333333333333334259, 0.3333333333333333703, 0.3333333333333335369, 0.3333333333333333148, 0.3333333333333333703, 0.3333333333333332593, 0.3333333333333335369, 0.3333333333333333148, 0.3333333333333333148, 0.3333333333333334814, 0.3333333333333332593, 0.3333333333333334814, 0.3333333333333333703, 0.3333333333333334259, 0.3333333333333334814, 0.3333333333333333703, 0.3333333333333333703, 0.3333333333333333148, 0.3333333333333332593, 0.3333333333333334814, 0.3333333333333333148, 0.3333333333333333703, 0.3333333333333333703, 0.3333333333333333703, 0.3333333333333333703, 0.3333333333333334259, 0.3333333333333333703, 0.3333333333333333703, 0.3333333333333333148, 0.3333333333333333703, 0.3333333333333334259, 0.3333333333333332593, 0.3333333333333334814, 0.3333333333333333703, 0.3333333333333333703, 0.3333333333333334259, 0.3333333333333333703, 0.3333333333333334259, 0.3333333333333333703, 0.3333333333333334259, 0.3333333333333332593, 0.3333333333333333703, 0.3333333333333334259, 0.3333333333333333148, 0.3333333333333333148, 0.3333333333333333703, 0.3333333333333334814, 0.3333333333333333148, 0.3333333333333333703, 0.3333333333333334259, 0.3333333333333333703, 0.3333333333333333703, 0.3333333333333333148, 0.3333333333333333703, 0.3333333333333333148, 0.3333333333333335369, 0.3333333333333332593, 0.3333333333333333703, 0.3333333333333333148, 0.3333333333333333703, 0.3333333333333334259, 0.3333333333333334259, 0.3333333333333333703, 0.3333333333333333148, 0.3333333333333334259, 0.3333333333333334259, 0.3333333333333333148, 0.3333333333333334259, 0.3333333333333335369, 0.3333333333333332593, 0.3333333333333333703, 0.3333333333333335369, 0.3333333333333332038, 0.3333333333333334259, 0.3333333333333333148, 0.3333333333333333703, 0.3333333333333333703, 0.3333333333333333703, 0.3333333333333333148, 0.3333333333333333703, 0.3333333333333333703, 0.3333333333333334259, 0.3333333333333334259, 0.3333333333333333148, 0.3333333333333334259, 0.3333333333333333148, 0.3333333333333333703, 0.3333333333333333148, 0.3333333333333334259, 0.3333333333333332038, 0.3333333333333333703, 0.3333333333333334259, 0.3333333333333335369, 0.3333333333333333148, 0.3333333333333333703, 0.3333333333333333703, 0.3333333333333333703, 0.3333333333333333703, 0.3333333333333333703, 0.3333333333333333703, 0.3333333333333334259, 0.3333333333333333703, 0.3333333333333333703, 0.3333333333333333703, 0.3333333333333332038, 0.3333333333333333703, 0.3333333333333335369, 0.3333333333333333148, 0.3333333333333334814, 0.3333333333333333703, 0.3333333333333332593, 0.3333333333333335369, 0.3333333333333333148, 0.3333333333333333703, 0.3333333333333333703, 0.3333333333333333148, 0.3333333333333333703, 0.3333333333333334259, 0.3333333333333334259, 0.3333333333333333703, 0.3333333333333334259, 0.3333333333333333148, 0.3333333333333333703, 0.3333333333333332593, 0.3333333333333333703, 0.3333333333333333703, 0.3333333333333333703, 0.3333333333333333703, 0.3333333333333333703, 0.3333333333333333703, 0.3333333333333333148, 0.3333333333333334259, 0.3333333333333333703, 0.3333333333333334259, 0.3333333333333333148, 0.3333333333333334259, 0.3333333333333333148, 0.3333333333333333703, 0.3333333333333334259, 0.3333333333333333703, 0.3333333333333333148, 0.3333333333333333148, 0.3333333333333334259, 0.3333333333333333703, 0.3333333333333333703, 0.3333333333333334259, 0.3333333333333333703, 0.3333333333333333148, 0.3333333333333334814, 0.3333333333333333703, 0.3333333333333334259, 0.3333333333333333703, 0.3333333333333333703, 0.3333333333333333703),
 ( 0.3333333333333334259, 0.3333333333333334259, 0.3333333333333334259, 0.3333333333333333703, 0.3333333333333333148, 0.3333333333333333703, 0.3333333333333334259, 0.3333333333333333703, 0.3333333333333333703, 0.3333333333333334259, 0.3333333333333332593, 0.3333333333333334259, 0.3333333333333333703, 0.3333333333333333703, 0.3333333333333333703, 0.3333333333333333703, 0.3333333333333333703, 0.3333333333333333148, 0.3333333333333334259, 0.3333333333333333148, 0.3333333333333334259, 0.3333333333333333148, 0.3333333333333333703, 0.3333333333333333703, 0.3333333333333333148, 0.3333333333333334814, 0.3333333333333332593, 0.3333333333333334814, 0.3333333333333333148, 0.3333333333333333148, 0.3333333333333334259, 0.3333333333333333703, 0.3333333333333334814, 0.3333333333333332593, 0.3333333333333334259, 0.3333333333333333703, 0.3333333333333333703, 0.3333333333333333148, 0.3333333333333333703, 0.3333333333333333703, 0.3333333333333334814, 0.3333333333333333703, 0.3333333333333334259, 0.3333333333333333703, 0.3333333333333333148, 0.3333333333333333148, 0.3333333333333333703, 0.3333333333333334259, 0.3333333333333333703, 0.3333333333333333703, 0.3333333333333333148, 0.3333333333333333703, 0.3333333333333332593, 0.3333333333333334259, 0.3333333333333333148, 0.3333333333333333703, 0.3333333333333333703, 0.3333333333333333703, 0.3333333333333333703, 0.3333333333333335369, 0.3333333333333332593, 0.3333333333333334259, 0.3333333333333333703, 0.3333333333333334259, 0.3333333333333334259, 0.3333333333333333148, 0.3333333333333334259, 0.3333333333333334259, 0.3333333333333334259, 0.3333333333333334814, 0.3333333333333333703, 0.3333333333333333148, 0.3333333333333333148, 0.3333333333333333703, 0.3333333333333334259, 0.3333333333333333703, 0.3333333333333333703, 0.3333333333333333703, 0.3333333333333333703, 0.3333333333333333148, 0.3333333333333333703, 0.3333333333333332593, 0.3333333333333333703, 0.3333333333333333148, 0.3333333333333333148, 0.3333333333333333703, 0.3333333333333333703, 0.3333333333333333148, 0.3333333333333333703, 0.3333333333333333703, 0.3333333333333333703, 0.3333333333333333703, 0.3333333333333334259, 0.3333333333333332593, 0.3333333333333334259, 0.3333333333333333148, 0.3333333333333333703, 0.3333333333333333148, 0.3333333333333334814, 0.3333333333333332038, 0.3333333333333335369, 0.3333333333333332593, 0.3333333333333333703, 0.3333333333333333703, 0.3333333333333333148, 0.3333333333333333703, 0.3333333333333333148, 0.3333333333333334259, 0.3333333333333334259, 0.3333333333333332593, 0.3333333333333334814, 0.3333333333333333703, 0.3333333333333332593, 0.3333333333333334814, 0.3333333333333334259, 0.3333333333333334259, 0.3333333333333332593, 0.3333333333333333703, 0.3333333333333333703, 0.3333333333333334259, 0.3333333333333333703, 0.3333333333333334259, 0.3333333333333333703, 0.3333333333333333148, 0.3333333333333334814, 0.3333333333333333703, 0.3333333333333334259, 0.3333333333333333703, 0.3333333333333333703, 0.3333333333333333148, 0.3333333333333334259, 0.3333333333333334259, 0.3333333333333333703, 0.3333333333333333148, 0.3333333333333333148, 0.3333333333333334259, 0.3333333333333334814, 0.3333333333333333148, 0.3333333333333334259, 0.3333333333333334814, 0.3333333333333333148, 0.3333333333333334814, 0.3333333333333332038, 0.3333333333333333703, 0.3333333333333333148, 0.3333333333333333703, 0.3333333333333334259, 0.3333333333333332038, 0.3333333333333334259, 0.3333333333333333148, 0.3333333333333332038, 0.3333333333333334259, 0.3333333333333333148, 0.3333333333333334259, 0.3333333333333332593, 0.3333333333333334259, 0.3333333333333333703, 0.3333333333333334259, 0.3333333333333333703, 0.3333333333333334259, 0.3333333333333333703, 0.3333333333333333703, 0.3333333333333334814, 0.3333333333333333703, 0.3333333333333335369, 0.3333333333333332038, 0.3333333333333333703, 0.3333333333333333703, 0.3333333333333333703, 0.3333333333333333148, 0.3333333333333333703, 0.3333333333333333703, 0.3333333333333334259, 0.3333333333333333148, 0.3333333333333334259, 0.3333333333333333148, 0.3333333333333334814, 0.3333333333333332593, 0.3333333333333333703, 0.3333333333333334259, 0.3333333333333333148, 0.3333333333333333703, 0.3333333333333333148, 0.3333333333333334259, 0.3333333333333332593, 0.3333333333333333703, 0.3333333333333334814, 0.3333333333333333703, 0.3333333333333333703, 0.3333333333333333703, 0.3333333333333333703, 0.3333333333333333148, 0.3333333333333333703, 0.3333333333333333703, 0.3333333333333334259, 0.3333333333333333703, 0.3333333333333333703, 0.3333333333333333703, 0.3333333333333333703, 0.3333333333333332038, 0.3333333333333334814, 0.3333333333333333703, 0.3333333333333333703, 0.3333333333333333148, 0.3333333333333333148, 0.3333333333333334259, 0.3333333333333334259, 0.3333333333333332593, 0.3333333333333335369, 0.3333333333333332593, 0.3333333333333334814, 0.3333333333333332593, 0.3333333333333334259, 0.3333333333333332038, 0.3333333333333335369, 0.3333333333333333148, 0.3333333333333333703, 0.3333333333333334259, 0.3333333333333333148, 0.3333333333333333148, 0.3333333333333335369, 0.3333333333333334259, 0.3333333333333333703, 0.3333333333333333148, 0.3333333333333334259, 0.3333333333333333148, 0.3333333333333334259, 0.3333333333333334259, 0.3333333333333333703, 0.3333333333333333703, 0.3333333333333333148, 0.3333333333333333703, 0.3333333333333333703, 0.3333333333333334259, 0.3333333333333333703, 0.3333333333333335369, 0.3333333333333333148, 0.3333333333333333703, 0.3333333333333332593, 0.3333333333333335369, 0.3333333333333333148, 0.3333333333333333148, 0.3333333333333334814, 0.3333333333333332593, 0.3333333333333334814, 0.3333333333333333703, 0.3333333333333334259, 0.3333333333333334814, 0.3333333333333333703, 0.3333333333333333703, 0.3333333333333333148, 0.3333333333333332593, 0.3333333333333334814, 0.3333333333333333148, 0.3333333333333333703, 0.3333333333333333703, 0.3333333333333333703, 0.3333333333333333703, 0.3333333333333334259, 0.3333333333333333703, 0.3333333333333333703, 0.3333333333333333148, 0.3333333333333333703, 0.3333333333333334259, 0.3333333333333332593, 0.3333333333333334814, 0.3333333333333333703, 0.3333333333333333703, 0.3333333333333334259, 0.3333333333333333703, 0.3333333333333334259, 0.3333333333333333703, 0.3333333333333334259, 0.3333333333333332593, 0.3333333333333333703, 0.3333333333333334259, 0.3333333333333333148, 0.3333333333333333148, 0.3333333333333333703, 0.3333333333333334814, 0.3333333333333333148, 0.3333333333333333703, 0.3333333333333334259, 0.3333333333333333703, 0.3333333333333333703, 0.3333333333333333148, 0.3333333333333333703, 0.3333333333333333148, 0.3333333333333335369, 0.3333333333333332593, 0.3333333333333333703, 0.3333333333333333148, 0.3333333333333333703, 0.3333333333333334259, 0.3333333333333334259, 0.3333333333333333703, 0.3333333333333333148, 0.3333333333333334259, 0.3333333333333334259, 0.3333333333333333148, 0.3333333333333334259, 0.3333333333333335369, 0.3333333333333332593, 0.3333333333333333703, 0.3333333333333335369, 0.3333333333333332038, 0.3333333333333334259, 0.3333333333333333148, 0.3333333333333333703, 0.3333333333333333703, 0.3333333333333333703, 0.3333333333333333148, 0.3333333333333333703, 0.3333333333333333703, 0.3333333333333334259, 0.3333333333333334259, 0.3333333333333333148, 0.3333333333333334259, 0.3333333333333333148, 0.3333333333333333703, 0.3333333333333333148, 0.3333333333333334259, 0.3333333333333332038, 0.3333333333333333703, 0.3333333333333334259, 0.3333333333333335369, 0.3333333333333333148, 0.3333333333333333703, 0.3333333333333333703, 0.3333333333333333703, 0.3333333333333333703, 0.3333333333333333703, 0.3333333333333333703, 0.3333333333333334259, 0.3333333333333333703, 0.3333333333333333703, 0.3333333333333333703, 0.3333333333333332038, 0.3333333333333333703, 0.3333333333333335369, 0.3333333333333333148, 0.3333333333333334814, 0.3333333333333333703, 0.3333333333333332593, 0.3333333333333335369, 0.3333333333333333148, 0.3333333333333333703, 0.3333333333333333703, 0.3333333333333333148, 0.3333333333333333703, 0.3333333333333334259, 0.3333333333333334259, 0.3333333333333333703, 0.3333333333333334259, 0.3333333333333333148, 0.3333333333333333703, 0.3333333333333332593, 0.3333333333333333703, 0.3333333333333333703, 0.3333333333333333703, 0.3333333333333333703, 0.3333333333333333703, 0.3333333333333333703, 0.3333333333333333148, 0.3333333333333334259, 0.3333333333333333703, 0.3333333333333334259, 0.3333333333333333148, 0.3333333333333334259, 0.3333333333333333148, 0.3333333333333333703, 0.3333333333333334259, 0.3333333333333333703, 0.3333333333333333148, 0.3333333333333333148, 0.3333333333333334259, 0.3333333333333333703, 0.3333333333333333703, 0.3333333333333334259, 0.3333333333333333703, 0.3333333333333333148, 0.3333333333333334814, 0.3333333333333333703, 0.3333333333333334259, 0.3333333333333333703, 0.3333333333333333703, 0.3333333333333333703),
 ( 1.000000000000000222, 1.000000000000000222, 1.000000000000000222, 1.000000000000000222, 0.9999999999999996669, 0.9999999999999997780, 1.000000000000000444, 1.000000000000000000, 1.000000000000000000, 1.000000000000000000, 0.9999999999999997780, 1.000000000000000000, 1.000000000000000000, 1.000000000000000000, 1.000000000000000000, 0.9999999999999997780, 1.000000000000000222, 0.9999999999999996669, 1.000000000000000000, 0.9999999999999997780, 1.000000000000000222, 1.000000000000000000, 1.000000000000000222, 0.9999999999999996669, 1.000000000000000000, 1.000000000000000222, 0.9999999999999996669, 1.000000000000000444, 1.000000000000000000, 0.9999999999999997780, 1.000000000000000222, 1.000000000000000222, 1.000000000000000222, 1.000000000000000000, 1.000000000000000000, 0.9999999999999997780, 1.000000000000000000, 1.000000000000000000, 1.000000000000000000, 1.000000000000000000, 1.000000000000000222, 1.000000000000000222, 1.000000000000000000, 1.000000000000000000, 1.000000000000000000, 0.9999999999999996669, 1.000000000000000222, 1.000000000000000000, 1.000000000000000000, 0.9999999999999997780, 0.9999999999999997780, 1.000000000000000000, 0.9999999999999996669, 1.000000000000000222, 0.9999999999999997780, 1.000000000000000222, 0.9999999999999997780, 0.9999999999999997780, 1.000000000000000222, 1.000000000000000222, 0.9999999999999997780, 1.000000000000000222, 1.000000000000000000, 1.000000000000000222, 1.000000000000000000, 0.9999999999999997780, 1.000000000000000000, 1.000000000000000000, 1.000000000000000222, 1.000000000000000222, 1.000000000000000000, 0.9999999999999997780, 1.000000000000000000, 1.000000000000000222, 0.9999999999999997780, 1.000000000000000444, 0.9999999999999996669, 1.000000000000000000, 1.000000000000000222, 0.9999999999999997780, 0.9999999999999997780, 0.9999999999999997780, 1.000000000000000000, 0.9999999999999997780, 1.000000000000000000, 0.9999999999999997780, 1.000000000000000222, 1.000000000000000000, 1.000000000000000222, 1.000000000000000000, 0.9999999999999997780, 1.000000000000000000, 1.000000000000000000, 0.9999999999999997780, 1.000000000000000222, 1.000000000000000000, 1.000000000000000000, 1.000000000000000000, 1.000000000000000222, 0.9999999999999996669, 1.000000000000000222, 1.000000000000000000, 1.000000000000000000, 0.9999999999999997780, 1.000000000000000000, 0.9999999999999997780, 1.000000000000000000, 1.000000000000000222, 1.000000000000000000, 0.9999999999999997780, 1.000000000000000222, 1.000000000000000222, 0.9999999999999996669, 1.000000000000000222, 1.000000000000000000, 1.000000000000000444, 0.9999999999999996669, 1.000000000000000000, 1.000000000000000222, 1.000000000000000222, 1.000000000000000222, 1.000000000000000222, 1.000000000000000000, 0.9999999999999997780, 1.000000000000000222, 1.000000000000000000, 1.000000000000000222, 0.9999999999999996669, 1.000000000000000000, 1.000000000000000000, 1.000000000000000222, 1.000000000000000222, 0.9999999999999997780, 1.000000000000000000, 0.9999999999999997780, 1.000000000000000222, 1.000000000000000000, 1.000000000000000222, 1.000000000000000000, 1.000000000000000444, 0.9999999999999996669, 1.000000000000000444, 0.9999999999999996669, 0.9999999999999997780, 0.9999999999999997780, 1.000000000000000222, 1.000000000000000000, 0.9999999999999997780, 1.000000000000000000, 0.9999999999999997780, 0.9999999999999996669, 1.000000000000000222, 1.000000000000000000, 0.9999999999999997780, 1.000000000000000000, 1.000000000000000000, 1.000000000000000222, 1.000000000000000000, 1.000000000000000000, 1.000000000000000444, 0.9999999999999997780, 1.000000000000000222, 1.000000000000000222, 0.9999999999999997780, 1.000000000000000444, 0.9999999999999996669, 1.000000000000000000, 0.9999999999999997780, 1.000000000000000222, 0.9999999999999997780, 1.000000000000000222, 1.000000000000000000, 1.000000000000000222, 0.9999999999999997780, 0.9999999999999997780, 1.000000000000000000, 1.000000000000000000, 0.9999999999999997780, 1.000000000000000222, 0.9999999999999997780, 1.000000000000000000, 1.000000000000000000, 1.000000000000000222, 1.000000000000000000, 0.9999999999999997780, 1.000000000000000222, 1.000000000000000444, 1.000000000000000000, 1.000000000000000000, 1.000000000000000000, 1.000000000000000000, 0.9999999999999997780, 1.000000000000000000, 1.000000000000000222, 1.000000000000000000, 1.000000000000000222, 0.9999999999999996669, 1.000000000000000000, 1.000000000000000000, 0.9999999999999994449, 1.000000000000000444, 1.000000000000000000, 1.000000000000000222, 0.9999999999999997780, 1.000000000000000000, 1.000000000000000222, 1.000000000000000000, 0.9999999999999996669, 1.000000000000000444, 0.9999999999999997780, 1.000000000000000444, 0.9999999999999996669, 1.000000000000000000, 0.9999999999999996669, 1.000000000000000444, 1.000000000000000000, 0.9999999999999997780, 1.000000000000000222, 1.000000000000000000, 0.9999999999999997780, 1.000000000000000444, 1.000000000000000222, 0.9999999999999997780, 1.000000000000000000, 1.000000000000000222, 0.9999999999999997780, 1.000000000000000222, 1.000000000000000222, 1.000000000000000000, 1.000000000000000000, 0.9999999999999996669, 1.000000000000000222, 0.9999999999999997780, 1.000000000000000000, 0.9999999999999997780, 1.000000000000000444, 1.000000000000000000, 1.000000000000000000, 0.9999999999999997780, 1.000000000000000444, 1.000000000000000000, 0.9999999999999997780, 1.000000000000000444, 0.9999999999999996669, 1.000000000000000444, 1.000000000000000000, 1.000000000000000444, 1.000000000000000222, 1.000000000000000222, 0.9999999999999997780, 1.000000000000000000, 0.9999999999999997780, 1.000000000000000444, 0.9999999999999996669, 1.000000000000000000, 1.000000000000000000, 1.000000000000000222, 1.000000000000000000, 1.000000000000000222, 1.000000000000000000, 1.000000000000000000, 0.9999999999999997780, 1.000000000000000000, 1.000000000000000000, 0.9999999999999997780, 1.000000000000000000, 1.000000000000000000, 0.9999999999999997780, 1.000000000000000000, 1.000000000000000222, 1.000000000000000000, 1.000000000000000000, 1.000000000000000000, 1.000000000000000000, 0.9999999999999996669, 1.000000000000000222, 1.000000000000000000, 0.9999999999999997780, 1.000000000000000000, 1.000000000000000222, 1.000000000000000000, 1.000000000000000222, 1.000000000000000222, 1.000000000000000000, 1.000000000000000222, 1.000000000000000000, 1.000000000000000000, 1.000000000000000000, 1.000000000000000222, 0.9999999999999996669, 1.000000000000000222, 0.9999999999999996669, 1.000000000000000222, 1.000000000000000222, 1.000000000000000222, 1.000000000000000222, 0.9999999999999996669, 1.000000000000000444, 1.000000000000000000, 1.000000000000000000, 1.000000000000000222, 1.000000000000000444, 0.9999999999999996669, 1.000000000000000444, 1.000000000000000222, 0.9999999999999996669, 1.000000000000000222, 0.9999999999999997780, 1.000000000000000000, 1.000000000000000000, 0.9999999999999997780, 1.000000000000000000, 0.9999999999999997780, 1.000000000000000000, 1.000000000000000000, 1.000000000000000444, 0.9999999999999997780, 1.000000000000000222, 0.9999999999999997780, 0.9999999999999997780, 1.000000000000000000, 1.000000000000000000, 0.9999999999999996669, 1.000000000000000000, 1.000000000000000222, 1.000000000000000222, 0.9999999999999997780, 1.000000000000000222, 0.9999999999999997780, 0.9999999999999997780, 1.000000000000000000, 1.000000000000000000, 1.000000000000000000, 1.000000000000000222, 1.000000000000000000, 1.000000000000000222, 1.000000000000000000, 0.9999999999999996669, 0.9999999999999997780, 1.000000000000000444, 0.9999999999999996669, 1.000000000000000444, 0.9999999999999997780, 0.9999999999999997780, 1.000000000000000222, 0.9999999999999997780, 1.000000000000000222, 1.000000000000000000, 1.000000000000000000, 0.9999999999999997780, 1.000000000000000222, 1.000000000000000222, 1.000000000000000000, 1.000000000000000222, 1.000000000000000000, 1.000000000000000000, 0.9999999999999997780, 1.000000000000000000, 1.000000000000000000, 0.9999999999999997780, 1.000000000000000000, 0.9999999999999996669, 1.000000000000000222, 0.9999999999999997780, 1.000000000000000222, 0.9999999999999997780, 1.000000000000000000, 0.9999999999999997780, 1.000000000000000222, 0.9999999999999997780, 1.000000000000000000, 1.000000000000000000, 1.000000000000000000, 1.000000000000000000, 0.9999999999999997780, 1.000000000000000222, 1.000000000000000000, 0.9999999999999997780, 1.000000000000000000, 1.000000000000000000, 1.000000000000000222, 1.000000000000000222, 1.000000000000000000, 1.000000000000000222, 1.000000000000000000, 1.000000000000000000, 1.000000000000000000),
 ( 0.3333333333333334259, 0.3333333333333334259, 0.3333333333333334259, 0.3333333333333333703, 0.3333333333333333148, 0.3333333333333333703, 0.3333333333333334259, 0.3333333333333333703, 0.3333333333333333703, 0.3333333333333334259, 0.3333333333333332593, 0.3333333333333334259, 0.3333333333333333703, 0.3333333333333333703, 0.3333333333333333703, 0.3333333333333333703, 0.3333333333333333703, 0.3333333333333333148, 0.3333333333333334259, 0.3333333333333333148, 0.3333333333333334259, 0.3333333333333333148, 0.3333333333333333703, 0.3333333333333333703, 0.3333333333333333148, 0.3333333333333334814, 0.3333333333333332593, 0.3333333333333334814, 0.3333333333333333148, 0.3333333333333333148, 0.3333333333333334259, 0.3333333333333333703, 0.3333333333333334814, 0.3333333333333332593, 0.3333333333333334259, 0.3333333333333333703, 0.3333333333333333703, 0.3333333333333333148, 0.3333333333333333703, 0.3333333333333333703, 0.3333333333333334814, 0.3333333333333333703, 0.3333333333333334259, 0.3333333333333333703, 0.3333333333333333148, 0.3333333333333333148, 0.3333333333333333703, 0.3333333333333334259, 0.3333333333333333703, 0.3333333333333333703, 0.3333333333333333148, 0.3333333333333333703, 0.3333333333333332593, 0.3333333333333334259, 0.3333333333333333148, 0.3333333333333333703, 0.3333333333333333703, 0.3333333333333333703, 0.3333333333333333703, 0.3333333333333335369, 0.3333333333333332593, 0.3333333333333334259, 0.3333333333333333703, 0.3333333333333334259, 0.3333333333333334259, 0.3333333333333333148, 0.3333333333333334259, 0.3333333333333334259, 0.3333333333333334259, 0.3333333333333334814, 0.3333333333333333703, 0.3333333333333333148, 0.3333333333333333148, 0.3333333333333333703, 0.3333333333333334259, 0.3333333333333333703, 0.3333333333333333703, 0.3333333333333333703, 0.3333333333333333703, 0.3333333333333333148, 0.3333333333333333703, 0.3333333333333332593, 0.3333333333333333703, 0.3333333333333333148, 0.3333333333333333148, 0.3333333333333333703, 0.3333333333333333703, 0.3333333333333333148, 0.3333333333333333703, 0.3333333333333333703, 0.3333333333333333703, 0.3333333333333333703, 0.3333333333333334259, 0.3333333333333332593, 0.3333333333333334259, 0.3333333333333333148, 0.3333333333333333703, 0.3333333333333333148, 0.3333333333333334814, 0.3333333333333332038, 0.3333333333333335369, 0.3333333333333332593, 0.3333333333333333703, 0.3333333333333333703, 0.3333333333333333148, 0.3333333333333333703, 0.3333333333333333148, 0.3333333333333334259, 0.3333333333333334259, 0.3333333333333332593, 0.3333333333333334814, 0.3333333333333333703, 0.3333333333333332593, 0.3333333333333334814, 0.3333333333333334259, 0.3333333333333334259, 0.3333333333333332593, 0.3333333333333333703, 0.3333333333333333703, 0.3333333333333334259, 0.3333333333333333703, 0.3333333333333334259, 0.3333333333333333703, 0.3333333333333333148, 0.3333333333333334814, 0.3333333333333333703, 0.3333333333333334259, 0.3333333333333333703, 0.3333333333333333703, 0.3333333333333333148, 0.3333333333333334259, 0.3333333333333334259, 0.3333333333333333703, 0.3333333333333333148, 0.3333333333333333148, 0.3333333333333334259, 0.3333333333333334814, 0.3333333333333333148, 0.3333333333333334259, 0.3333333333333334814, 0.3333333333333333148, 0.3333333333333334814, 0.3333333333333332038, 0.3333333333333333703, 0.3333333333333333148, 0.3333333333333333703, 0.3333333333333334259, 0.3333333333333332038, 0.3333333333333334259, 0.3333333333333333148, 0.3333333333333332038, 0.3333333333333334259, 0.3333333333333333148, 0.3333333333333334259, 0.3333333333333332593, 0.3333333333333334259, 0.3333333333333333703, 0.3333333333333334259, 0.3333333333333333703, 0.3333333333333334259, 0.3333333333333333703, 0.3333333333333333703, 0.3333333333333334814, 0.3333333333333333703, 0.3333333333333335369, 0.3333333333333332038, 0.3333333333333333703, 0.3333333333333333703, 0.3333333333333333703, 0.3333333333333333148, 0.3333333333333333703, 0.3333333333333333703, 0.3333333333333334259, 0.3333333333333333148, 0.3333333333333334259, 0.3333333333333333148, 0.3333333333333334814, 0.3333333333333332593, 0.3333333333333333703, 0.3333333333333334259, 0.3333333333333333148, 0.3333333333333333703, 0.3333333333333333148, 0.3333333333333334259, 0.3333333333333332593, 0.3333333333333333703, 0.3333333333333334814, 0.3333333333333333703, 0.3333333333333333703, 0.3333333333333333703, 0.3333333333333333703, 0.3333333333333333148, 0.3333333333333333703, 0.3333333333333333703, 0.3333333333333334259, 0.3333333333333333703, 0.3333333333333333703, 0.3333333333333333703, 0.3333333333333333703, 0.3333333333333332038, 0.3333333333333334814, 0.3333333333333333703, 0.3333333333333333703, 0.3333333333333333148, 0.3333333333333333148, 0.3333333333333334259, 0.3333333333333334259, 0.3333333333333332593, 0.3333333333333335369, 0.3333333333333332593, 0.3333333333333334814, 0.3333333333333332593, 0.3333333333333334259, 0.3333333333333332038, 0.3333333333333335369, 0.3333333333333333148, 0.3333333333333333703, 0.3333333333333334259, 0.3333333333333333148, 0.3333333333333333148, 0.3333333333333335369, 0.3333333333333334259, 0.3333333333333333703, 0.3333333333333333148, 0.3333333333333334259, 0.3333333333333333148, 0.3333333333333334259, 0.3333333333333334259, 0.3333333333333333703, 0.3333333333333333703, 0.3333333333333333148, 0.3333333333333333703, 0.3333333333333333703, 0.3333333333333334259, 0.3333333333333333703, 0.3333333333333335369, 0.3333333333333333148, 0.3333333333333333703, 0.3333333333333332593, 0.3333333333333335369, 0.3333333333333333148, 0.3333333333333333148, 0.3333333333333334814, 0.3333333333333332593, 0.3333333333333334814, 0.3333333333333333703, 0.3333333333333334259, 0.3333333333333334814, 0.3333333333333333703, 0.3333333333333333703, 0.3333333333333333148, 0.3333333333333332593, 0.3333333333333334814, 0.3333333333333333148, 0.3333333333333333703, 0.3333333333333333703, 0.3333333333333333703, 0.3333333333333333703, 0.3333333333333334259, 0.3333333333333333703, 0.3333333333333333703, 0.3333333333333333148, 0.3333333333333333703, 0.3333333333333334259, 0.3333333333333332593, 0.3333333333333334814, 0.3333333333333333703, 0.3333333333333333703, 0.3333333333333334259, 0.3333333333333333703, 0.3333333333333334259, 0.3333333333333333703, 0.3333333333333334259, 0.3333333333333332593, 0.3333333333333333703, 0.3333333333333334259, 0.3333333333333333148, 0.3333333333333333148, 0.3333333333333333703, 0.3333333333333334814, 0.3333333333333333148, 0.3333333333333333703, 0.3333333333333334259, 0.3333333333333333703, 0.3333333333333333703, 0.3333333333333333148, 0.3333333333333333703, 0.3333333333333333148, 0.3333333333333335369, 0.3333333333333332593, 0.3333333333333333703, 0.3333333333333333148, 0.3333333333333333703, 0.3333333333333334259, 0.3333333333333334259, 0.3333333333333333703, 0.3333333333333333148, 0.3333333333333334259, 0.3333333333333334259, 0.3333333333333333148, 0.3333333333333334259, 0.3333333333333335369, 0.3333333333333332593, 0.3333333333333333703, 0.3333333333333335369, 0.3333333333333332038, 0.3333333333333334259, 0.3333333333333333148, 0.3333333333333333703, 0.3333333333333333703, 0.3333333333333333703, 0.3333333333333333148, 0.3333333333333333703, 0.3333333333333333703, 0.3333333333333334259, 0.3333333333333334259, 0.3333333333333333148, 0.3333333333333334259, 0.3333333333333333148, 0.3333333333333333703, 0.3333333333333333148, 0.3333333333333334259, 0.3333333333333332038, 0.3333333333333333703, 0.3333333333333334259, 0.3333333333333335369, 0.3333333333333333148, 0.3333333333333333703, 0.3333333333333333703, 0.3333333333333333703, 0.3333333333333333703, 0.3333333333333333703, 0.3333333333333333703, 0.3333333333333334259, 0.3333333333333333703, 0.3333333333333333703, 0.3333333333333333703, 0.3333333333333332038, 0.3333333333333333703, 0.3333333333333335369, 0.3333333333333333148, 0.3333333333333334814, 0.3333333333333333703, 0.3333333333333332593, 0.3333333333333335369, 0.3333333333333333148, 0.3333333333333333703, 0.3333333333333333703, 0.3333333333333333148, 0.3333333333333333703, 0.3333333333333334259, 0.3333333333333334259, 0.3333333333333333703, 0.3333333333333334259, 0.3333333333333333148, 0.3333333333333333703, 0.3333333333333332593, 0.3333333333333333703, 0.3333333333333333703, 0.3333333333333333703, 0.3333333333333333703, 0.3333333333333333703, 0.3333333333333333703, 0.3333333333333333148, 0.3333333333333334259, 0.3333333333333333703, 0.3333333333333334259, 0.3333333333333333148, 0.3333333333333334259, 0.3333333333333333148, 0.3333333333333333703, 0.3333333333333334259, 0.3333333333333333703, 0.3333333333333333148, 0.3333333333333333148, 0.3333333333333334259, 0.3333333333333333703, 0.3333333333333333703, 0.3333333333333334259, 0.3333333333333333703, 0.3333333333333333148, 0.3333333333333334814, 0.3333333333333333703, 0.3333333333333334259, 0.3333333333333333703, 0.3333333333333333703, 0.3333333333333333703),
 ( 0.3333333333333334259, 0.3333333333333334259, 0.3333333333333334259, 0.3333333333333333703, 0.3333333333333333148, 0.3333333333333333703, 0.3333333333333334259, 0.3333333333333333703, 0.3333333333333333703, 0.3333333333333334259, 0.3333333333333332593, 0.3333333333333334259, 0.3333333333333333703, 0.3333333333333333703, 0.3333333333333333703, 0.3333333333333333703, 0.3333333333333333703, 0.3333333333333333148, 0.3333333333333334259, 0.3333333333333333148, 0.3333333333333334259, 0.3333333333333333148, 0.3333333333333333703, 0.3333333333333333703, 0.3333333333333333148, 0.3333333333333334814, 0.3333333333333332593, 0.3333333333333334814, 0.3333333333333333148, 0.3333333333333333148, 0.3333333333333334259, 0.3333333333333333703, 0.3333333333333334814, 0.3333333333333332593, 0.3333333333333334259, 0.3333333333333333703, 0.3333333333333333703, 0.3333333333333333148, 0.3333333333333333703, 0.3333333333333333703, 0.3333333333333334814, 0.3333333333333333703, 0.3333333333333334259, 0.3333333333333333703, 0.3333333333333333148, 0.3333333333333333148, 0.3333333333333333703, 0.3333333333333334259, 0.3333333333333333703, 0.3333333333333333703, 0.3333333333333333148, 0.3333333333333333703, 0.3333333333333332593, 0.3333333333333334259, 0.3333333333333333148, 0.3333333333333333703, 0.3333333333333333703, 0.3333333333333333703, 0.3333333333333333703, 0.3333333333333335369, 0.3333333333333332593, 0.3333333333333334259, 0.3333333333333333703, 0.3333333333333334259, 0.3333333333333334259, 0.3333333333333333148, 0.3333333333333334259, 0.3333333333333334259, 0.3333333333333334259, 0.3333333333333334814, 0.3333333333333333703, 0.3333333333333333148, 0.3333333333333333148, 0.3333333333333333703, 0.3333333333333334259, 0.3333333333333333703, 0.3333333333333333703, 0.3333333333333333703, 0.3333333333333333703, 0.3333333333333333148, 0.3333333333333333703, 0.3333333333333332593, 0.3333333333333333703, 0.3333333333333333148, 0.3333333333333333148, 0.3333333333333333703, 0.3333333333333333703, 0.3333333333333333148, 0.3333333333333333703, 0.3333333333333333703, 0.3333333333333333703, 0.3333333333333333703, 0.3333333333333334259, 0.3333333333333332593, 0.3333333333333334259, 0.3333333333333333148, 0.3333333333333333703, 0.3333333333333333148, 0.3333333333333334814, 0.3333333333333332038, 0.3333333333333335369, 0.3333333333333332593, 0.3333333333333333703, 0.3333333333333333703, 0.3333333333333333148, 0.3333333333333333703, 0.3333333333333333148, 0.3333333333333334259, 0.3333333333333334259, 0.3333333333333332593, 0.3333333333333334814, 0.3333333333333333703, 0.3333333333333332593, 0.3333333333333334814, 0.3333333333333334259, 0.3333333333333334259, 0.3333333333333332593, 0.3333333333333333703, 0.3333333333333333703, 0.3333333333333334259, 0.3333333333333333703, 0.3333333333333334259, 0.3333333333333333703, 0.3333333333333333148, 0.3333333333333334814, 0.3333333333333333703, 0.3333333333333334259, 0.3333333333333333703, 0.3333333333333333703, 0.3333333333333333148, 0.3333333333333334259, 0.3333333333333334259, 0.3333333333333333703, 0.3333333333333333148, 0.3333333333333333148, 0.3333333333333334259, 0.3333333333333334814, 0.3333333333333333148, 0.3333333333333334259, 0.3333333333333334814, 0.3333333333333333148, 0.3333333333333334814, 0.3333333333333332038, 0.3333333333333333703, 0.3333333333333333148, 0.3333333333333333703, 0.3333333333333334259, 0.3333333333333332038, 0.3333333333333334259, 0.3333333333333333148, 0.3333333333333332038, 0.3333333333333334259, 0.3333333333333333148, 0.3333333333333334259, 0.3333333333333332593, 0.3333333333333334259, 0.3333333333333333703, 0.3333333333333334259, 0.3333333333333333703, 0.3333333333333334259, 0.3333333333333333703, 0.3333333333333333703, 0.3333333333333334814, 0.3333333333333333703, 0.3333333333333335369, 0.3333333333333332038, 0.3333333333333333703, 0.3333333333333333703, 0.3333333333333333703, 0.3333333333333333148, 0.3333333333333333703, 0.3333333333333333703, 0.3333333333333334259, 0.3333333333333333148, 0.3333333333333334259, 0.3333333333333333148, 0.3333333333333334814, 0.3333333333333332593, 0.3333333333333333703, 0.3333333333333334259, 0.3333333333333333148, 0.3333333333333333703, 0.3333333333333333148, 0.3333333333333334259, 0.3333333333333332593, 0.3333333333333333703, 0.3333333333333334814, 0.3333333333333333703, 0.3333333333333333703, 0.3333333333333333703, 0.3333333333333333703, 0.3333333333333333148, 0.3333333333333333703, 0.3333333333333333703, 0.3333333333333334259, 0.3333333333333333703, 0.3333333333333333703, 0.3333333333333333703, 0.3333333333333333703, 0.3333333333333332038, 0.3333333333333334814, 0.3333333333333333703, 0.3333333333333333703, 0.3333333333333333148, 0.3333333333333333148, 0.3333333333333334259, 0.3333333333333334259, 0.3333333333333332593, 0.3333333333333335369, 0.3333333333333332593, 0.3333333333333334814, 0.3333333333333332593, 0.3333333333333334259, 0.3333333333333332038, 0.3333333333333335369, 0.3333333333333333148, 0.3333333333333333703, 0.3333333333333334259, 0.3333333333333333148, 0.3333333333333333148, 0.3333333333333335369, 0.3333333333333334259, 0.3333333333333333703, 0.3333333333333333148, 0.3333333333333334259, 0.3333333333333333148, 0.3333333333333334259, 0.3333333333333334259, 0.3333333333333333703, 0.3333333333333333703, 0.3333333333333333148, 0.3333333333333333703, 0.3333333333333333703, 0.3333333333333334259, 0.3333333333333333703, 0.3333333333333335369, 0.3333333333333333148, 0.3333333333333333703, 0.3333333333333332593, 0.3333333333333335369, 0.3333333333333333148, 0.3333333333333333148, 0.3333333333333334814, 0.3333333333333332593, 0.3333333333333334814, 0.3333333333333333703, 0.3333333333333334259, 0.3333333333333334814, 0.3333333333333333703, 0.3333333333333333703, 0.3333333333333333148, 0.3333333333333332593, 0.3333333333333334814, 0.3333333333333333148, 0.3333333333333333703, 0.3333333333333333703, 0.3333333333333333703, 0.3333333333333333703, 0.3333333333333334259, 0.3333333333333333703, 0.3333333333333333703, 0.3333333333333333148, 0.3333333333333333703, 0.3333333333333334259, 0.3333333333333332593, 0.3333333333333334814, 0.3333333333333333703, 0.3333333333333333703, 0.3333333333333334259, 0.3333333333333333703, 0.3333333333333334259, 0.3333333333333333703, 0.3333333333333334259, 0.3333333333333332593, 0.3333333333333333703, 0.3333333333333334259, 0.3333333333333333148, 0.3333333333333333148, 0.3333333333333333703, 0.3333333333333334814, 0.3333333333333333148, 0.3333333333333333703, 0.3333333333333334259, 0.3333333333333333703, 0.3333333333333333703, 0.3333333333333333148, 0.3333333333333333703, 0.3333333333333333148, 0.3333333333333335369, 0.3333333333333332593, 0.3333333333333333703, 0.3333333333333333148, 0.3333333333333333703, 0.3333333333333334259, 0.3333333333333334259, 0.3333333333333333703, 0.3333333333333333148, 0.3333333333333334259, 0.3333333333333334259, 0.3333333333333333148, 0.3333333333333334259, 0.3333333333333335369, 0.3333333333333332593, 0.3333333333333333703, 0.3333333333333335369, 0.3333333333333332038, 0.3333333333333334259, 0.3333333333333333148, 0.3333333333333333703, 0.3333333333333333703, 0.3333333333333333703, 0.3333333333333333148, 0.3333333333333333703, 0.3333333333333333703, 0.3333333333333334259, 0.3333333333333334259, 0.3333333333333333148, 0.3333333333333334259, 0.3333333333333333148, 0.3333333333333333703, 0.3333333333333333148, 0.3333333333333334259, 0.3333333333333332038, 0.3333333333333333703, 0.3333333333333334259, 0.3333333333333335369, 0.3333333333333333148, 0.3333333333333333703, 0.3333333333333333703, 0.3333333333333333703, 0.3333333333333333703, 0.3333333333333333703, 0.3333333333333333703, 0.3333333333333334259, 0.3333333333333333703, 0.3333333333333333703, 0.3333333333333333703, 0.3333333333333332038, 0.3333333333333333703, 0.3333333333333335369, 0.3333333333333333148, 0.3333333333333334814, 0.3333333333333333703, 0.3333333333333332593, 0.3333333333333335369, 0.3333333333333333148, 0.3333333333333333703, 0.3333333333333333703, 0.3333333333333333148, 0.3333333333333333703, 0.3333333333333334259, 0.3333333333333334259, 0.3333333333333333703, 0.3333333333333334259, 0.3333333333333333148, 0.3333333333333333703, 0.3333333333333332593, 0.3333333333333333703, 0.3333333333333333703, 0.3333333333333333703, 0.3333333333333333703, 0.3333333333333333703, 0.3333333333333333703, 0.3333333333333333148, 0.3333333333333334259, 0.3333333333333333703, 0.3333333333333334259, 0.3333333333333333148, 0.3333333333333334259, 0.3333333333333333148, 0.3333333333333333703, 0.3333333333333334259, 0.3333333333333333703, 0.3333333333333333148, 0.3333333333333333148, 0.3333333333333334259, 0.3333333333333333703, 0.3333333333333333703, 0.3333333333333334259, 0.3333333333333333703, 0.3333333333333333148, 0.3333333333333334814, 0.3333333333333333703, 0.3333333333333334259, 0.3333333333333333703, 0.3333333333333333703, 0.3333333333333333703),
 ( 1.000000000000000222, 1.000000000000000222, 1.000000000000000222, 1.000000000000000222, 0.9999999999999996669, 0.9999999999999997780, 1.000000000000000444, 1.000000000000000000, 1.000000000000000000, 1.000000000000000000, 0.9999999999999997780, 1.000000000000000000, 1.000000000000000000, 1.000000000000000000, 1.000000000000000000, 0.9999999999999997780, 1.000000000000000222, 0.9999999999999996669, 1.000000000000000000, 0.9999999999999997780, 1.000000000000000222, 1.000000000000000000, 1.000000000000000222, 0.9999999999999996669, 1.000000000000000000, 1.000000000000000222, 0.9999999999999996669, 1.000000000000000444, 1.000000000000000000, 0.9999999999999997780, 1.000000000000000222, 1.000000000000000222, 1.000000000000000222, 1.000000000000000000, 1.000000000000000000, 0.9999999999999997780, 1.000000000000000000, 1.000000000000000000, 1.000000000000000000, 1.000000000000000000, 1.000000000000000222, 1.000000000000000222, 1.000000000000000000, 1.000000000000000000, 1.000000000000000000, 0.9999999999999996669, 1.000000000000000222, 1.000000000000000000, 1.000000000000000000, 0.9999999999999997780, 0.9999999999999997780, 1.000000000000000000, 0.9999999999999996669, 1.000000000000000222, 0.9999999999999997780, 1.000000000000000222, 0.9999999999999997780, 0.9999999999999997780, 1.000000000000000222, 1.000000000000000222, 0.9999999999999997780, 1.000000000000000222, 1.000000000000000000, 1.000000000000000222, 1.000000000000000000, 0.9999999999999997780, 1.000000000000000000, 1.000000000000000000, 1.000000000000000222, 1.000000000000000222, 1.000000000000000000, 0.9999999999999997780, 1.000000000000000000, 1.000000000000000222, 0.9999999999999997780, 1.000000000000000444, 0.9999999999999996669, 1.000000000000000000, 1.000000000000000222, 0.9999999999999997780, 0.9999999999999997780, 0.9999999999999997780, 1.000000000000000000, 0.9999999999999997780, 1.000000000000000000, 0.9999999999999997780, 1.000000000000000222, 1.000000000000000000, 1.000000000000000222, 1.000000000000000000, 0.9999999999999997780, 1.000000000000000000, 1.000000000000000000, 0.9999999999999997780, 1.000000000000000222, 1.000000000000000000, 1.000000000000000000, 1.000000000000000000, 1.000000000000000222, 0.9999999999999996669, 1.000000000000000222, 1.000000000000000000, 1.000000000000000000, 0.9999999999999997780, 1.000000000000000000, 0.9999999999999997780, 1.000000000000000000, 1.000000000000000222, 1.000000000000000000, 0.9999999999999997780, 1.000000000000000222, 1.000000000000000222, 0.9999999999999996669, 1.000000000000000222, 1.000000000000000000, 1.000000000000000444, 0.9999999999999996669, 1.000000000000000000, 1.000000000000000222, 1.000000000000000222, 1.000000000000000222, 1.000000000000000222, 1.000000000000000000, 0.9999999999999997780, 1.000000000000000222, 1.000000000000000000, 1.000000000000000222, 0.9999999999999996669, 1.000000000000000000, 1.000000000000000000, 1.000000000000000222, 1.000000000000000222, 0.9999999999999997780, 1.000000000000000000, 0.9999999999999997780, 1.000000000000000222, 1.000000000000000000, 1.000000000000000222, 1.000000000000000000, 1.000000000000000444, 0.9999999999999996669, 1.000000000000000444, 0.9999999999999996669, 0.9999999999999997780, 0.9999999999999997780, 1.000000000000000222, 1.000000000000000000, 0.9999999999999997780, 1.000000000000000000, 0.9999999999999997780, 0.9999999999999996669, 1.000000000000000222, 1.000000000000000000, 0.9999999999999997780, 1.000000000000000000, 1.000000000000000000, 1.000000000000000222, 1.000000000000000000, 1.000000000000000000, 1.000000000000000444, 0.9999999999999997780, 1.000000000000000222, 1.000000000000000222, 0.9999999999999997780, 1.000000000000000444, 0.9999999999999996669, 1.000000000000000000, 0.9999999999999997780, 1.000000000000000222, 0.9999999999999997780, 1.000000000000000222, 1.000000000000000000, 1.000000000000000222, 0.9999999999999997780, 0.9999999999999997780, 1.000000000000000000, 1.000000000000000000, 0.9999999999999997780, 1.000000000000000222, 0.9999999999999997780, 1.000000000000000000, 1.000000000000000000, 1.000000000000000222, 1.000000000000000000, 0.9999999999999997780, 1.000000000000000222, 1.000000000000000444, 1.000000000000000000, 1.000000000000000000, 1.000000000000000000, 1.000000000000000000, 0.9999999999999997780, 1.000000000000000000, 1.000000000000000222, 1.000000000000000000, 1.000000000000000222, 0.9999999999999996669, 1.000000000000000000, 1.000000000000000000, 0.9999999999999994449, 1.000000000000000444, 1.000000000000000000, 1.000000000000000222, 0.9999999999999997780, 1.000000000000000000, 1.000000000000000222, 1.000000000000000000, 0.9999999999999996669, 1.000000000000000444, 0.9999999999999997780, 1.000000000000000444, 0.9999999999999996669, 1.000000000000000000, 0.9999999999999996669, 1.000000000000000444, 1.000000000000000000, 0.9999999999999997780, 1.000000000000000222, 1.000000000000000000, 0.9999999999999997780, 1.000000000000000444, 1.000000000000000222, 0.9999999999999997780, 1.000000000000000000, 1.000000000000000222, 0.9999999999999997780, 1.000000000000000222, 1.000000000000000222, 1.000000000000000000, 1.000000000000000000, 0.9999999999999996669, 1.000000000000000222, 0.9999999999999997780, 1.000000000000000000, 0.9999999999999997780, 1.000000000000000444, 1.000000000000000000, 1.000000000000000000, 0.9999999999999997780, 1.000000000000000444, 1.000000000000000000, 0.9999999999999997780, 1.000000000000000444, 0.9999999999999996669, 1.000000000000000444, 1.000000000000000000, 1.000000000000000444, 1.000000000000000222, 1.000000000000000222, 0.9999999999999997780, 1.000000000000000000, 0.9999999999999997780, 1.000000000000000444, 0.9999999999999996669, 1.000000000000000000, 1.000000000000000000, 1.000000000000000222, 1.000000000000000000, 1.000000000000000222, 1.000000000000000000, 1.000000000000000000, 0.9999999999999997780, 1.000000000000000000, 1.000000000000000000, 0.9999999999999997780, 1.000000000000000000, 1.000000000000000000, 0.9999999999999997780, 1.000000000000000000, 1.000000000000000222, 1.000000000000000000, 1.000000000000000000, 1.000000000000000000, 1.000000000000000000, 0.9999999999999996669, 1.000000000000000222, 1.000000000000000000, 0.9999999999999997780, 1.000000000000000000, 1.000000000000000222, 1.000000000000000000, 1.000000000000000222, 1.000000000000000222, 1.000000000000000000, 1.000000000000000222, 1.000000000000000000, 1.000000000000000000, 1.000000000000000000, 1.000000000000000222, 0.9999999999999996669, 1.000000000000000222, 0.9999999999999996669, 1.000000000000000222, 1.000000000000000222, 1.000000000000000222, 1.000000000000000222, 0.9999999999999996669, 1.000000000000000444, 1.000000000000000000, 1.000000000000000000, 1.000000000000000222, 1.000000000000000444, 0.9999999999999996669, 1.000000000000000444, 1.000000000000000222, 0.9999999999999996669, 1.000000000000000222, 0.9999999999999997780, 1.000000000000000000, 1.000000000000000000, 0.9999999999999997780, 1.000000000000000000, 0.9999999999999997780, 1.000000000000000000, 1.000000000000000000, 1.000000000000000444, 0.9999999999999997780, 1.000000000000000222, 0.9999999999999997780, 0.9999999999999997780, 1.000000000000000000, 1.000000000000000000, 0.9999999999999996669, 1.000000000000000000, 1.000000000000000222, 1.000000000000000222, 0.9999999999999997780, 1.000000000000000222, 0.9999999999999997780, 0.9999999999999997780, 1.000000000000000000, 1.000000000000000000, 1.000000000000000000, 1.000000000000000222, 1.000000000000000000, 1.000000000000000222, 1.000000000000000000, 0.9999999999999996669, 0.9999999999999997780, 1.000000000000000444, 0.9999999999999996669, 1.000000000000000444, 0.9999999999999997780, 0.9999999999999997780, 1.000000000000000222, 0.9999999999999997780, 1.000000000000000222, 1.000000000000000000, 1.000000000000000000, 0.9999999999999997780, 1.000000000000000222, 1.000000000000000222, 1.000000000000000000, 1.000000000000000222, 1.000000000000000000, 1.000000000000000000, 0.9999999999999997780, 1.000000000000000000, 1.000000000000000000, 0.9999999999999997780, 1.000000000000000000, 0.9999999999999996669, 1.000000000000000222, 0.9999999999999997780, 1.000000000000000222, 0.9999999999999997780, 1.000000000000000000, 0.9999999999999997780, 1.000000000000000222, 0.9999999999999997780, 1.000000000000000000, 1.000000000000000000, 1.000000000000000000, 1.000000000000000000, 0.9999999999999997780, 1.000000000000000222, 1.000000000000000000, 0.9999999999999997780, 1.000000000000000000, 1.000000000000000000, 1.000000000000000222, 1.000000000000000222, 1.000000000000000000, 1.000000000000000222, 1.000000000000000000, 1.000000000000000000, 1.000000000000000000) ) ) 
 REPRESENTATION_ITEM ( '' )  SURFACE ( )  );
#49282 = CARTESIAN_POINT ( 'NONE',  ( -5.573810548549546162, 9.516879716700865188, 0.7216878364870267237 ) ) ;
#49283 = ORIENTED_EDGE ( 'NONE', *, *, #93834, .F. ) ;
#49284 = CARTESIAN_POINT ( 'NONE',  ( 7.741342523278686549, 11.97539067722642869, 0.7216878364870438212 ) ) ;
#49285 = B_SPLINE_CURVE_WITH_KNOTS ( 'NONE', 3,
 ( #80559, #147704, #146658, #197497 ),
 .UNSPECIFIED., .F., .F.,
 ( 4, 4 ),
 ( 0.000000000000000000, 3.548791410040124229E-05 ),
 .UNSPECIFIED. ) ;
#49287 = CARTESIAN_POINT ( 'NONE',  ( 1.616814774554303780, 0.2004563524992293566, 2.006445175307514095 ) ) ;
#49286 = CARTESIAN_POINT ( 'NONE',  ( 2.016421337698256711, -2.119947128278206971, 0.05498460973795551987 ) ) ;
#49289 = ORIENTED_EDGE ( 'NONE', *, *, #7969, .F. ) ;
#49288 = CARTESIAN_POINT ( 'NONE',  ( 2.285178059325339461, 0.08539987017499665878, -1.809671756684204214 ) ) ;
#49290 = CARTESIAN_POINT ( 'NONE',  ( 6.851666526859736983, 9.086973262793417661, -1.599625672291269396 ) ) ;
#49291 = ORIENTED_EDGE ( 'NONE', *, *, #4355, .T. ) ;
#49292 = CARTESIAN_POINT ( 'NONE',  ( 4.937140493670735708, 8.911747675924535983, -0.7998128361456281477 ) ) ;
#49293 = VECTOR ( 'NONE', #92118, 1000.000000000000000 ) ;
#49295 = CARTESIAN_POINT ( 'NONE',  ( 0.3740639818887542267, -1.901581053304630675, -0.2314239742453021165 ) ) ;
#49294 = CARTESIAN_POINT ( 'NONE',  ( -6.013204822860843457, 6.974159367214481264, -1.199719254218446718 ) ) ;
#49296 = CIRCLE ( 'NONE', #201385, 2.000000000000000000 ) ;
#49297 = CARTESIAN_POINT ( 'NONE',  ( 1.845237968648437032, 8.937006183319889274, 0.7750000000000004663 ) ) ;
#49298 =( LENGTH_UNIT ( ) NAMED_UNIT ( * ) SI_UNIT ( .MILLI., .METRE. ) );
#49299 = CARTESIAN_POINT ( 'NONE',  ( 6.616015773344440021, 6.821032611764393572, 1.040834085586084257E-14 ) ) ;
#49300 = CARTESIAN_POINT ( 'NONE',  ( 1.364683531249986537, -0.3239583329919163424, 0.7879004041258500513 ) ) ;
#49301 = CARTESIAN_POINT ( 'NONE',  ( -10.47097470845587175, 11.11055866948701443, 1.040834085586084257E-14 ) ) ;
#49302 = CARTESIAN_POINT ( 'NONE',  ( 4.627887939457571598, -1.327398817707679868, -1.706084338546076662 ) ) ;
#49303 = CARTESIAN_POINT ( 'NONE',  ( -6.129694847154220305, 8.244672969803623630, -1.443375672974066548 ) ) ;
#49304 = CARTESIAN_POINT ( 'NONE',  ( 4.407809338218622308, 8.156544971314787063, 0.000000000000000000 ) ) ;
#49305 = CARTESIAN_POINT ( 'NONE',  ( 1.635180430577408028, 1.980530345366804834, 0.7584260845197099421 ) ) ;
#49306 = CARTESIAN_POINT ( 'NONE',  ( 6.651389018303578204, -1.468406013062272475, -1.084454090978362428 ) ) ;
#49307 = CARTESIAN_POINT ( 'NONE',  ( 3.198462767114045313, -0.5687421903855809369, -1.887558129442780341 ) ) ;
#49308 = VERTEX_POINT ( 'NONE', #149769 ) ;
#49309 = CARTESIAN_POINT ( 'NONE',  ( 5.793399386127640049, -1.781339898235247077, 0.8404781526112365952 ) ) ;
#49310 = CARTESIAN_POINT ( 'NONE',  ( 1.974458820771322953, -0.09541523299517583323, -1.939727210137192737 ) ) ;
#49311 = ORIENTED_EDGE ( 'NONE', *, *, #20338, .F. ) ;
#49312 = CARTESIAN_POINT ( 'NONE',  ( -3.447516199624892419, 7.244129009529488350, 0.7998128361456352531 ) ) ;
#49314 = CARTESIAN_POINT ( 'NONE',  ( 1.865311119267500040, 2.483290406177208975, -2.476007760152826531 ) ) ;
#49313 = CARTESIAN_POINT ( 'NONE',  ( -5.641601317062239218, 8.635599732330991429, -1.082531754730549967 ) ) ;
#49316 = CARTESIAN_POINT ( 'NONE',  ( 7.416473721875251890, 8.611306416064660851, 1.199719254218462483 ) ) ;
#49315 = CARTESIAN_POINT ( 'NONE',  ( 2.994169869935947137, -0.6075897704641713970, -2.000389221998987832 ) ) ;
#49318 = CARTESIAN_POINT ( 'NONE',  ( 4.868786560638889149, 6.773613302202437403, 1.443375672974065660 ) ) ;
#49317 = CARTESIAN_POINT ( 'NONE',  ( 6.337546739384100292, 9.481222731668410120, 1.199719254218460707 ) ) ;
#49320 = ORIENTED_EDGE ( 'NONE', *, *, #48185, .F. ) ;
#49319 = CARTESIAN_POINT ( 'NONE',  ( 6.586579894266018975, -1.172543786506787145, 1.511232097859278367 ) ) ;
#49321 = CARTESIAN_POINT ( 'NONE',  ( 4.617920694193921705, -2.164688156338661962, 0.4286357439418769788 ) ) ;
#49322 = AXIS2_PLACEMENT_3D ( 'NONE', #111540, #145081, #141883 ) ;
#49323 = CARTESIAN_POINT ( 'NONE',  ( 1.501302152069685647, 1.803625081967351829, -1.271268654958551014 ) ) ;
#49324 = CARTESIAN_POINT ( 'NONE',  ( -11.81907076198591966, 12.34268775403524643, 1.592066415281218505 ) ) ;
#49325 = CARTESIAN_POINT ( 'NONE',  ( 0.6098336241119780565, -0.6879379538977903330, 1.784437680087819666 ) ) ;
#49326 = CARTESIAN_POINT ( 'NONE',  ( -0.4360851681528791768, -8.730413173480725320, 9.960047168614407198 ) ) ;
#49327 = CARTESIAN_POINT ( 'NONE',  ( 9.398826802771546696, 11.98838390803207865, -1.599625672291262513 ) ) ;
#49328 = CARTESIAN_POINT ( 'NONE',  ( 3.789561645344252216, -1.914057400617325211, 0.7896510022299549902 ) ) ;
#49330 = CARTESIAN_POINT ( 'NONE',  ( 1.639762333045853726, -1.565812861550972324, -1.490595759849028035 ) ) ;
#49329 = DIRECTION ( 'NONE',  ( 0.000000000000000000, 0.000000000000000000, -1.000000000000000000 ) ) ;
#49331 = CARTESIAN_POINT ( 'NONE',  ( 3.650093349144762023, 0.7902683543556283663, 2.044282924279612779 ) ) ;
#49332 = LINE ( 'NONE', #102325, #107389 ) ;
#49333 = DIRECTION ( 'NONE',  ( 5.578564026256504688E-16, 1.000000000000000000, 9.066213480720158442E-32 ) ) ;
#49334 = CARTESIAN_POINT ( 'NONE',  ( 1.419999999067301788, 7.203691543881689086, 4.238255391842193909 ) ) ;
#49335 = ADVANCED_FACE ( 'NONE', ( #34923, #170266 ), #1344, .F. ) ;
#49336 = CARTESIAN_POINT ( 'NONE',  ( -0.6823417656250039265, 14.13020833367473195, -1.181850606188755259 ) ) ;
#49337 = CARTESIAN_POINT ( 'NONE',  ( -5.327428015527048366, 5.180030537728460338, -0.7998128361456362523 ) ) ;
#49338 = CARTESIAN_POINT ( 'NONE',  ( 0.8092204703840089053, 1.198858234535697065, -1.621184076614573533 ) ) ;
#49339 = CARTESIAN_POINT ( 'NONE',  ( -10.31739171031960822, 11.13930453823545186, 1.040834085586084257E-14 ) ) ;
#49340 = CARTESIAN_POINT ( 'NONE',  ( 4.416890754593222113, -1.537527071031305814, 1.386575359339572655 ) ) ;
#49341 = CARTESIAN_POINT ( 'NONE',  ( 5.976184116172984950, -2.107040639921609504, -0.2072291863110999888 ) ) ;
#49342 = CARTESIAN_POINT ( 'NONE',  ( 6.257251587906815793, 7.258880593101466161, 1.199719254218462483 ) ) ;
#49343 = CARTESIAN_POINT ( 'NONE',  ( 0.000000000000000000, 0.000000000000000000, 0.000000000000000000 ) ) ;
#49344 = CARTESIAN_POINT ( 'NONE',  ( 4.469560827962531846, -0.3407972494764506810, 1.939574385640041809 ) ) ;
#49345 = CARTESIAN_POINT ( 'NONE',  ( 6.158190107012026182, -1.625331280325162053, 1.616661686624631944 ) ) ;
#49346 = CARTESIAN_POINT ( 'NONE',  ( 3.141029808440584326, -1.609794727316344209, 0.8612202190056221784 ) ) ;
#49347 = CARTESIAN_POINT ( 'NONE',  ( 3.444653546323793947, 6.176457016423196222, 1.199719254218451159 ) ) ;
#49348 = CARTESIAN_POINT ( 'NONE',  ( 5.355107487273504496, 6.310342158982962246, -1.082531754730543083 ) ) ;
#49349 = CARTESIAN_POINT ( 'NONE',  ( -5.831978632172702071, 9.955725504176825780, 0.7998128361456481317 ) ) ;
#49350 = CARTESIAN_POINT ( 'NONE',  ( 4.355912491740495440, 8.303924683664389406, 0.000000000000000000 ) ) ;
#49351 = ORIENTED_EDGE ( 'NONE', *, *, #67862, .T. ) ;
#49352 = CARTESIAN_POINT ( 'NONE',  ( 3.709243207436668577, 1.698441389738635676, -1.080623863572414356 ) ) ;
#49353 = CARTESIAN_POINT ( 'NONE',  ( 0.2284049197783468987, -2.054502581980635956, -1.030649272238814085 ) ) ;
#49354 = CARTESIAN_POINT ( 'NONE',  ( 4.610177715184628155, 1.961415711727178213, -0.04403062578262756377 ) ) ;
#49355 = CARTESIAN_POINT ( 'NONE',  ( -6.856673000209188906, 9.022537805042615489, 1.599625672291283607 ) ) ;
#49356 = CARTESIAN_POINT ( 'NONE',  ( -5.623934791570306402, 5.455678766453782913, 0.7998128361456341429 ) ) ;
#49357 = CARTESIAN_POINT ( 'NONE',  ( -4.827585214917754719, 7.789877296449459365, -1.199719254218453823 ) ) ;
#49359 = CARTESIAN_POINT ( 'NONE',  ( 5.840640841166978348, 0.3488620263497018703, 1.734928340252988033 ) ) ;
#49358 = CARTESIAN_POINT ( 'NONE',  ( 0.5739142741672832448, -1.158190483201524179, 1.740425096305434183 ) ) ;
#49360 = CARTESIAN_POINT ( 'NONE',  ( 1.535386672163775668, -1.589036399888818618, -1.509351277865833563 ) ) ;
#49361 = CARTESIAN_POINT ( 'NONE',  ( 1.188542350144041304, 1.317171145998846216, 1.137751157100845623 ) ) ;
#49362 = CARTESIAN_POINT ( 'NONE',  ( 5.991813822235618758, 9.077867661661846554, 1.199719254218462483 ) ) ;
#49363 = DIRECTION ( 'NONE',  ( -1.000000000000000000, 0.000000000000000000, 0.000000000000000000 ) ) ;
#49364 = CARTESIAN_POINT ( 'NONE',  ( 1.154464490038846547, -1.361941861570209467, 1.058318063114448648 ) ) ;
#49365 = CARTESIAN_POINT ( 'NONE',  ( 1.118978350340808614, -0.04878210919301298465, 2.191179638975069732 ) ) ;
#49366 = CARTESIAN_POINT ( 'NONE',  ( 3.545738602337618506, -1.670889076328873069, -1.441789439710974063 ) ) ;
#49367 = PRESENTATION_LAYER_ASSIGNMENT (  '', '', ( #149722 ) ) ;
#49368 = CARTESIAN_POINT ( 'NONE',  ( 1.059715561420447205, 1.773747297294786307, 1.251667063311131312 ) ) ;
#49369 = CARTESIAN_POINT ( 'NONE',  ( -1.203907071533411699, 2.993479746939697872, 0.7750000000000152323 ) ) ;
#49370 = CARTESIAN_POINT ( 'NONE',  ( 2.835287003684193508, -1.733785568389034193, -1.215143187034111838 ) ) ;
#49371 = CARTESIAN_POINT ( 'NONE',  ( 6.827182134110198142, 6.033542260787205791, 2.783941933017803905 ) ) ;
#49372 = EDGE_CURVE ( 'NONE', #195805, #170920, #21852, .T. ) ;
#49373 = ORIENTED_EDGE ( 'NONE', *, *, #831, .F. ) ;
#49375 = CARTESIAN_POINT ( 'NONE',  ( -1.364683531250014514, -0.1572916663252435232, 0.7879004041258379498 ) ) ;
#49374 = CARTESIAN_POINT ( 'NONE',  ( 2.542860532589632960, -1.904047414228837942, 1.276277502183044810 ) ) ;
#49376 = CARTESIAN_POINT ( 'NONE',  ( 3.344057444064992168, 7.053150784717805877, 1.040834085586084257E-14 ) ) ;
#49377 = CARTESIAN_POINT ( 'NONE',  ( 4.389451384964074165, 0.0001031656717501855256, -2.221473415372441806 ) ) ;
#49378 = CARTESIAN_POINT ( 'NONE',  ( -7.700668062882078502, 9.046829497192987901, -1.082531754730543971 ) ) ;
#49379 = CARTESIAN_POINT ( 'NONE',  ( 0.09540182900466742666, -7.837949925775435922, -10.99983588129881618 ) ) ;
#49380 = CARTESIAN_POINT ( 'NONE',  ( 4.202664430556247055, 6.886563688082179446, 1.082531754730558626 ) ) ;
#49381 = CARTESIAN_POINT ( 'NONE',  ( -5.856759170979136897, 9.776710099543576504, 0.000000000000000000 ) ) ;
#49382 = CARTESIAN_POINT ( 'NONE',  ( 3.580761967785000888, 7.191656372475549119, -0.7216878364870338292 ) ) ;
#49383 = ORIENTED_EDGE ( 'NONE', *, *, #57719, .F. ) ;
#49384 = CARTESIAN_POINT ( 'NONE',  ( 3.129529892704606464, 0.4926417352555876872, 1.955172657653013957 ) ) ;
#49386 = CARTESIAN_POINT ( 'NONE',  ( 0.6200784347700560861, 2.040642744413103671, -0.2990284185609564105 ) ) ;
#49385 = CARTESIAN_POINT ( 'NONE',  ( 7.775764792637399836, 9.030479331953833011, -1.199719254218441611 ) ) ;
#49387 = DIRECTION ( 'NONE',  ( 0.9982742078614211811, 0.000000000000000000, 0.05872483221476467591 ) ) ;
#49388 = EDGE_CURVE ( 'NONE', #1801, #96623, #85964, .T. ) ;
#49389 = CARTESIAN_POINT ( 'NONE',  ( 4.868786560638885597, 7.733982516503781213, 1.082531754730548412 ) ) ;
#49390 = CARTESIAN_POINT ( 'NONE',  ( -6.726765607527585011, -8.198316282514451103, -6.726765607527558366 ) ) ;
#49391 = CARTESIAN_POINT ( 'NONE',  ( -1.364683531249997417, 4.259375000341424133, 1.214306433183764966E-14 ) ) ;
#49392 = CARTESIAN_POINT ( 'NONE',  ( 4.136819237485493517, -1.907179771870757268, 1.079280405373375773 ) ) ;
#49393 = CARTESIAN_POINT ( 'NONE',  ( 1.354138928560550292, 0.1455316553338575902, -2.011204400906742240 ) ) ;
#49394 = CARTESIAN_POINT ( 'NONE',  ( 1.188719773494644860, 1.394467456127197025, 1.202481090285527632 ) ) ;
#49395 = CARTESIAN_POINT ( 'NONE',  ( 6.608709811657416999, 9.797579649320619311, -1.199719254218440723 ) ) ;
#49396 = CARTESIAN_POINT ( 'NONE',  ( 4.752862199841776381, -1.465721779273346792, 1.088108411805274622 ) ) ;
#49397 = CARTESIAN_POINT ( 'NONE',  ( 6.451795992440088057, -1.844709169062180409, -0.8146298745319994206 ) ) ;
#49398 = CARTESIAN_POINT ( 'NONE',  ( -9.016335848287868160, 10.47781223021269170, 1.199719254218462483 ) ) ;
#49400 = CARTESIAN_POINT ( 'NONE',  ( -5.121948170912633991, 9.197632976031879792, -0.7998128361456362523 ) ) ;
#49399 = CARTESIAN_POINT ( 'NONE',  ( 4.944316486460487603, 2.256077187801101669, 0.1715336590100754455 ) ) ;
#49401 = CARTESIAN_POINT ( 'NONE',  ( 1.190214010286832602, -0.9452824899213798648, 1.882083610947625107 ) ) ;
#49402 = CARTESIAN_POINT ( 'NONE',  ( -5.576146316970437944, 9.727530813099326323, 0.000000000000000000 ) ) ;
#49403 = CARTESIAN_POINT ( 'NONE',  ( 4.352052382902608763, -0.7952921280917917279, 1.911720769834825973 ) ) ;
#49404 = CARTESIAN_POINT ( 'NONE',  ( 9.738834413317897898, 10.25639499182604730, 0.000000000000000000 ) ) ;
#49405 = APPLICATION_PROTOCOL_DEFINITION ( 'draft international standard', 'automotive_design', 1998, #40891 ) ;
#49406 = CARTESIAN_POINT ( 'NONE',  ( -7.503547950159405566, 10.84155747757291266, 1.199719254218453823 ) ) ;
#49407 = UNCERTAINTY_MEASURE_WITH_UNIT (LENGTH_MEASURE( 1.000000000000000082E-05 ), #31107, 'distance_accuracy_value', 'NONE');
#49408 = CARTESIAN_POINT ( 'NONE',  ( 7.526711554241970248, 8.810193563817646734, -1.199719254218452047 ) ) ;
#49409 = CARTESIAN_POINT ( 'NONE',  ( 5.737025562671778545, 6.072208551910874164, -0.6475843906825241580 ) ) ;
#49410 = CARTESIAN_POINT ( 'NONE',  ( -9.571693261567968847, 12.19006144329456731, 1.443375672974076540 ) ) ;
#49412 = CARTESIAN_POINT ( 'NONE',  ( 1.582608957317205522, 1.147345939325004283, 1.902073548153013327 ) ) ;
#49411 = CARTESIAN_POINT ( 'NONE',  ( 0.2641366190093488164, 0.6592694798918593557, -2.015615888626711705 ) ) ;
#49413 = CIRCLE ( 'NONE', #153302, 0.08000000000000041800 ) ;
#49414 = CARTESIAN_POINT ( 'NONE',  ( -5.608744109800250399, 5.623033084029449569, 0.4489015171048596486 ) ) ;
#49415 = CARTESIAN_POINT ( 'NONE',  ( -5.901542003698421190, 10.10715911428198055, 0.000000000000000000 ) ) ;
#49416 = CARTESIAN_POINT ( 'NONE',  ( 6.799577732453452761, 7.891594428405881878, -1.199719254218446718 ) ) ;
#49417 = CARTESIAN_POINT ( 'NONE',  ( 3.490630252122446375, 1.913478943654752129, 0.4322817992908413176 ) ) ;
#49418 = CARTESIAN_POINT ( 'NONE',  ( 6.823831386379729302, 6.855558127064808716, -0.7998128361456281477 ) ) ;
#49419 = CARTESIAN_POINT ( 'NONE',  ( -4.014161209245137307, 7.626991082632122776, -0.01188119308113272377 ) ) ;
#49420 = CARTESIAN_POINT ( 'NONE',  ( 3.063252641683779753, 5.661212951017999373, 1.199719254218450271 ) ) ;
#49421 = CARTESIAN_POINT ( 'NONE',  ( -4.814553946628611136, 8.631080347793099961, 0.000000000000000000 ) ) ;
#49422 = CARTESIAN_POINT ( 'NONE',  ( -6.697364695470783502, 10.75741654478384035, 0.7216878364870458196 ) ) ;
#49423 = CARTESIAN_POINT ( 'NONE',  ( 2.408575119285644384, -2.115224228095522907, -0.1514441693673748146 ) ) ;
#49424 = CARTESIAN_POINT ( 'NONE',  ( -5.088052786878465739, 9.158088361325352977, 0.000000000000000000 ) ) ;
#49425 = CARTESIAN_POINT ( 'NONE',  ( 4.017981030900905637, 1.947309607215493621, -0.2378496960543720617 ) ) ;
#49426 = CARTESIAN_POINT ( 'NONE',  ( 2.799875798528407511, -0.6792266858460673795, 2.052276964324008635 ) ) ;
#49427 = CARTESIAN_POINT ( 'NONE',  ( 2.876309626556411203, -0.1380247437976732383, -1.836149222064882514 ) ) ;
#49428 = CARTESIAN_POINT ( 'NONE',  ( -4.117634752470962667, 7.483002602015099924, 0.6335975934644126895 ) ) ;
#49429 = CARTESIAN_POINT ( 'NONE',  ( 0.6823417656249882723, -1.094791666325249713, 1.181850606188755259 ) ) ;
#49430 = CARTESIAN_POINT ( 'NONE',  ( 4.558407276396470920, -1.556374654738747587, -0.7788941851257675797 ) ) ;
#49431 = CARTESIAN_POINT ( 'NONE',  ( 4.570507181582611267, 8.346359121906111511, 0.000000000000000000 ) ) ;
#49432 = CARTESIAN_POINT ( 'NONE',  ( 4.690757960648231695, 5.535267711253469614, 1.082531754730560403 ) ) ;
#49433 = CARTESIAN_POINT ( 'NONE',  ( -1.114695358586659246E-15, -9.448428148670501514, 9.261795338153662627 ) ) ;
#49434 = CARTESIAN_POINT ( 'NONE',  ( 1.780366757100563913, -1.156431984057613827, 1.826190802295484472 ) ) ;
#49435 = AXIS2_PLACEMENT_3D ( 'NONE', #151041, #11964, #47701 ) ;
#49436 = CARTESIAN_POINT ( 'NONE',  ( 4.516953773913958692, 2.015725170860783066, -0.04666989112152990921 ) ) ;
#49437 = CARTESIAN_POINT ( 'NONE',  ( -9.205623113554631587, 11.76297960394566466, 1.443375672974076540 ) ) ;
#49439 = TOROIDAL_SURFACE ( 'NONE', #125580, 6.330000000000000959, 0.08000000000000000167 ) ;
#49438 = CARTESIAN_POINT ( 'NONE',  ( 0.9366540776252421097, 2.129889809250965271, 0.3686189752144660714 ) ) ;
#49440 = CARTESIAN_POINT ( 'NONE',  ( 2.266812238764161158, -1.800804572728794239, -0.8025143323158872022 ) ) ;
#49441 = CARTESIAN_POINT ( 'NONE',  ( 10.35569247086020894, 1.405922845961228962, 6.063183772476113731 ) ) ;
#49442 = CARTESIAN_POINT ( 'NONE',  ( 3.808095655114822176, 1.371164123868431117, -1.375570907105559293 ) ) ;
#49445 = ORIENTED_EDGE ( 'NONE', *, *, #58073, .T. ) ;
#49444 = CARTESIAN_POINT ( 'NONE',  ( -4.882344714696960075, 5.829061934302122161, 1.082531754730549078 ) ) ;
#49443 = DIRECTION ( 'NONE',  ( 0.6507913734559640506, -0.7592566023653004592, 0.000000000000000000 ) ) ;
#49446 = CARTESIAN_POINT ( 'NONE',  ( -4.977251789548269301, 4.979417640660637190, 0.7216878364870257245 ) ) ;
#49447 = CARTESIAN_POINT ( 'NONE',  ( 4.329849954717849947, 6.144853928627882489, 1.599625672291262513 ) ) ;
#49448 = CARTESIAN_POINT ( 'NONE',  ( -4.444040490229335560, 8.406740681901359480, 0.7998128361456352531 ) ) ;
#49449 = CARTESIAN_POINT ( 'NONE',  ( -8.609064354553318310, 12.98773281371349775, 0.7216878364870317197 ) ) ;
#49450 = CARTESIAN_POINT ( 'NONE',  ( 1.044295067165665669, 0.8929887407379886177, -2.018210024696056148 ) ) ;
#49451 = CARTESIAN_POINT ( 'NONE',  ( -3.285556943750000070, -2.909374999522040817, 0.000000000000000000 ) ) ;
#49452 = AXIS2_PLACEMENT_3D ( 'NONE', #50972, #119228, #86663 ) ;
#49453 = CARTESIAN_POINT ( 'NONE',  ( 5.295737746731337126, -1.384591195607473235, -1.390005841682784959 ) ) ;
#49454 = ORIENTED_EDGE ( 'NONE', *, *, #170571, .F. ) ;
#49455 = CARTESIAN_POINT ( 'NONE',  ( 3.960252432329254724, -1.215859836287141116, 1.733281388416860525 ) ) ;
#49456 = CARTESIAN_POINT ( 'NONE',  ( 0.7499999999999902300, 3.014583334016149418, 1.299038105676669330 ) ) ;
#49457 = CARTESIAN_POINT ( 'NONE',  ( 0.07479286986305369589, 4.095183424177953668, -2.410510762676120411 ) ) ;
#49458 = CARTESIAN_POINT ( 'NONE',  ( 4.189278935350455590, -0.7026162016144417155, 1.701997885059022497 ) ) ;
#49459 = EDGE_LOOP ( 'NONE', ( #58883, #254, #173662, #47826 ) ) ;
#49460 = CARTESIAN_POINT ( 'NONE',  ( -8.670602931139386627, 10.07445716020612103, 1.199719254218462483 ) ) ;
#49461 = CARTESIAN_POINT ( 'NONE',  ( 0.001128590447023392540, 8.210952333604110365, 2.038660652713624177 ) ) ;
#49463 = EDGE_CURVE ( 'NONE', #53554, #168636, #145486, .T. ) ;
#49462 = CARTESIAN_POINT ( 'NONE',  ( 5.467072749063267345, -1.670387955228332277, 1.306269166133757986 ) ) ;
#49464 = CARTESIAN_POINT ( 'NONE',  ( -5.542386507442576438, 5.938373294205037567, -0.8979104349328557166 ) ) ;
#49465 = CARTESIAN_POINT ( 'NONE',  ( 5.986088515633498197, 6.942523675449257858, -1.199719254218446718 ) ) ;
#49466 = VECTOR ( 'NONE', #9403, 1000.000000000000000 ) ;
#49467 = CARTESIAN_POINT ( 'NONE',  ( 5.483688661837972766, 1.380929853543419128, 1.529855004671219820 ) ) ;
#49469 = CARTESIAN_POINT ( 'NONE',  ( 4.177188522404684079, 1.205947341878073287, 1.391433828303423326 ) ) ;
#49468 = CARTESIAN_POINT ( 'NONE',  ( 0.6427239283240515633, -0.2220358882154548907, -1.847681390136299839 ) ) ;
#49470 = CARTESIAN_POINT ( 'NONE',  ( 6.774270308322468459, 11.05506579301824743, 0.7998128361456462443 ) ) ;
#49471 =( NAMED_UNIT ( * ) PLANE_ANGLE_UNIT ( ) SI_UNIT ( $, .RADIAN. ) );
#49472 = CARTESIAN_POINT ( 'NONE',  ( -4.846024844760177253, 5.033942040585545286, -0.8809814305317772432 ) ) ;
#49473 = LINE ( 'NONE', #129747, #157108 ) ;
#49474 = CARTESIAN_POINT ( 'NONE',  ( 2.948105999307056635, 0.7938017206191756436, -2.059354589195587337 ) ) ;
#49475 = CARTESIAN_POINT ( 'NONE',  ( 4.411571241670419141, -0.3925092328114428986, 2.227967001921112633 ) ) ;
#49476 = CARTESIAN_POINT ( 'NONE',  ( -6.236387472606145010, 9.259240570473746601, -1.082531754730538864 ) ) ;
#49477 = CARTESIAN_POINT ( 'NONE',  ( 4.746265919983247983, 0.9249516081627707775, -1.557494045171695651 ) ) ;
#49478 = CARTESIAN_POINT ( 'NONE',  ( 5.401554078093819378, -1.867474805896391032, 0.4264384668619321528 ) ) ;
#49479 = CARTESIAN_POINT ( 'NONE',  ( 6.727182134110201162, 0.003007720480356954919, 1.910970182385363980 ) ) ;
#49480 = CARTESIAN_POINT ( 'NONE',  ( 5.576977133510579776, -0.04717937999037385977, -1.870219006134994588 ) ) ;
#49481 = CARTESIAN_POINT ( 'NONE',  ( 5.951566935816642534, 1.409582436273165706, 1.215217600354216554 ) ) ;
#49482 = CARTESIAN_POINT ( 'NONE',  ( -1.500000000000001110, 13.02083333333333393, 0.8660254037844418162 ) ) ;
#49483 = CARTESIAN_POINT ( 'NONE',  ( 6.121911923048983795, -0.9866791243483238327, -1.469064191006617337 ) ) ;
#49484 = CARTESIAN_POINT ( 'NONE',  ( -0.03006412033006514162, -0.9462945741195265548, 1.780671068589256834 ) ) ;
#49486 = CARTESIAN_POINT ( 'NONE',  ( 2.385502688336095911, 1.925211662925530254, -0.8542917040773172488 ) ) ;
#49485 = CARTESIAN_POINT ( 'NONE',  ( -3.972175818679615222, 4.696921878956699103, 1.082531754730558626 ) ) ;
#49487 = CARTESIAN_POINT ( 'NONE',  ( 10.39640486358069360, 11.02356051713265650, 0.7998128361456462443 ) ) ;
#49489 = CARTESIAN_POINT ( 'NONE',  ( -7.641992139597101108, 12.06740792950531649, 0.7998128361456481317 ) ) ;
#49488 = CARTESIAN_POINT ( 'NONE',  ( -3.602337597214539753E-15, 11.84375000068279604, 1.500000000000001554 ) ) ;
#49490 = DIRECTION ( 'NONE',  ( -1.000000000000000000, 0.000000000000000000, 0.000000000000000000 ) ) ;
#49491 = CARTESIAN_POINT ( 'NONE',  ( 2.215108757275308982, 1.619595947845490436, -1.206587912388109141 ) ) ;
#49492 = CARTESIAN_POINT ( 'NONE',  ( 0.6823417656249899377, 1.842708333674752952, 1.181850606188755259 ) ) ;
#49493 = CARTESIAN_POINT ( 'NONE',  ( 4.090809663021327758, 5.795697244990093644, 1.599625672291267398 ) ) ;
#49494 = CARTESIAN_POINT ( 'NONE',  ( 3.339309863714147397, -1.908069850993234340, 1.015702806061814734 ) ) ;
#49495 = CARTESIAN_POINT ( 'NONE',  ( 6.620655732516649294, 2.985444497229528871, 2.280274006979409407 ) ) ;
#49498 = CARTESIAN_POINT ( 'NONE',  ( 1.452583904633400591, -1.374772708486727391, 1.500000000000001332 ) ) ;
#49497 = DIRECTION ( 'NONE',  ( 1.000000000000000000, -0.000000000000000000, -0.000000000000000000 ) ) ;
#49496 = CARTESIAN_POINT ( 'NONE',  ( 2.925527285498711549, 6.635141943048991742, 0.7998128361456281477 ) ) ;
#49499 = CARTESIAN_POINT ( 'NONE',  ( 8.880227426826630577, 12.34372051706435869, 1.082531754730546636 ) ) ;
#49500 = DIRECTION ( 'NONE',  ( -0.9885327375000381167, 0.000000000000000000, 0.1510067114093955609 ) ) ;
#49501 = CARTESIAN_POINT ( 'NONE',  ( -7.456621297836087514, 9.722477485607340597, 1.443375672974090751 ) ) ;
#49502 = CARTESIAN_POINT ( 'NONE',  ( -0.6823417656250003738, 0.4677083336747517306, -1.181850606188749264 ) ) ;
#49503 = CARTESIAN_POINT ( 'NONE',  ( 1.277182604683280598, 2.023070758711601691, -0.8431670391453591762 ) ) ;
#49504 = CARTESIAN_POINT ( 'NONE',  ( 0.4545350412507122573, 7.933623023433559851, 1.993241281637238460 ) ) ;
#49505 = CARTESIAN_POINT ( 'NONE',  ( 1.182923723612337774, -2.207873014618145113, -0.4935663919954368373 ) ) ;
#49506 = CARTESIAN_POINT ( 'NONE',  ( -9.155833807930273238, 9.576227618873799585, -0.7998128361456291469 ) ) ;
#49507 = CARTESIAN_POINT ( 'NONE',  ( -5.544921637864841379, 5.571422787038166291, -0.7216878364870197293 ) ) ;
#49508 = CARTESIAN_POINT ( 'NONE',  ( -1.364683531250012516, 2.842708333674754506, 0.7879004041258379498 ) ) ;
#49509 = CARTESIAN_POINT ( 'NONE',  ( 4.675188888464441028, 8.274035074156913083, -0.5495550137140058355 ) ) ;
#49510 = CARTESIAN_POINT ( 'NONE',  ( 1.499999999999997113, 11.64583333333333748, -0.8660254037844378194 ) ) ;
#49511 = CARTESIAN_POINT ( 'NONE',  ( 4.228163802615382494, 6.026220084508304708, -1.599625672291269396 ) ) ;
#49512 = CARTESIAN_POINT ( 'NONE',  ( 2.881836681058600913, -0.9132262334808398663, 1.515770159524139515 ) ) ;
#49513 = CARTESIAN_POINT ( 'NONE',  ( 6.088949818052607377, -0.3178892970779038096, -2.183640257897196513 ) ) ;
#49514 =( GEOMETRIC_REPRESENTATION_CONTEXT ( 3 ) GLOBAL_UNCERTAINTY_ASSIGNED_CONTEXT ( ( #23272 ) ) GLOBAL_UNIT_ASSIGNED_CONTEXT ( ( #80900, #164281, #99290 ) ) REPRESENTATION_CONTEXT ( 'NONE', 'WORKASPACE' ) );
#49515 = CARTESIAN_POINT ( 'NONE',  ( -1.364683531250014514, 9.588541667008064096, -0.7879004041258335089 ) ) ;
#49516 = CARTESIAN_POINT ( 'NONE',  ( -6.934069218746458318, 7.054445274817795486, -0.7998128361456362523 ) ) ;
#49517 = CARTESIAN_POINT ( 'NONE',  ( 4.833611329963474645, 0.6298591494234163646, -1.915606498650752831 ) ) ;
#49518 = EDGE_LOOP ( 'NONE', ( #138920, #53703, #196339, #126661 ) ) ;
#49519 = CARTESIAN_POINT ( 'NONE',  ( 2.571000202304725590, 0.09389976206976291540, -1.868427151830873267 ) ) ;
#49520 = CARTESIAN_POINT ( 'NONE',  ( 2.764580022184208730, -0.7881864689132519475, -1.914544693583389634 ) ) ;
#49521 = CARTESIAN_POINT ( 'NONE',  ( -5.926322542504860458, 9.928143709648733051, -0.7216878364870338292 ) ) ;
#49522 = CARTESIAN_POINT ( 'NONE',  ( 2.408343312057196872, -1.907530749141531423, -0.1368029246449145864 ) ) ;
#49523 = CARTESIAN_POINT ( 'NONE',  ( -0.4153311931458959494, 3.850000000000006306, 0.5000000000000064393 ) ) ;
#49524 = CARTESIAN_POINT ( 'NONE',  ( -10.83922355283164407, 5.627439893072524235, -6.488667358217312220 ) ) ;
#49525 = CARTESIAN_POINT ( 'NONE',  ( -5.821562047661695161, 5.964446275831489785, 0.1636455158913159846 ) ) ;
#49526 = CARTESIAN_POINT ( 'NONE',  ( 1.364683531249988535, 4.426041667008082214, 0.7879004041258500513 ) ) ;
#49527 = CARTESIAN_POINT ( 'NONE',  ( 0.8789968191965717992, -1.730013457311157188, -0.8152767527440167861 ) ) ;
#49528 = CARTESIAN_POINT ( 'NONE',  ( 5.343321937561575474, 8.287607122913563273, -1.082531754730548412 ) ) ;
#49529 = CARTESIAN_POINT ( 'NONE',  ( 2.787496613063783713, -1.831585881375777713, 0.7034878451678548972 ) ) ;
#49530 = CARTESIAN_POINT ( 'NONE',  ( 1.850000000000000311, -0.09855238430051822818, 0.5999999999999969802 ) ) ;
#49531 = CARTESIAN_POINT ( 'NONE',  ( -4.664887371553763096, 7.600063145858131364, -1.199719254218453823 ) ) ;
#49532 = CARTESIAN_POINT ( 'NONE',  ( 8.048736748007069508, 12.54194330598362406, -0.7998128361456352531 ) ) ;
#49533 = CARTESIAN_POINT ( 'NONE',  ( 6.573508854753547404, 1.887220770608761589, -0.5698601248695351895 ) ) ;
#49534 = CARTESIAN_POINT ( 'NONE',  ( 1.364683531249988535, 2.905208333674754506, -0.7879004041258239610 ) ) ;
#49535 = CARTESIAN_POINT ( 'NONE',  ( 1.881109812905419343, -1.842300511448742739, -0.8121059663154740482 ) ) ;
#49537 = CARTESIAN_POINT ( 'NONE',  ( 2.530995666134610911, -1.758555926239983691, 1.178765877976214016 ) ) ;
#49536 = CARTESIAN_POINT ( 'NONE',  ( -8.053180056837398126, 8.497724275839514618, 0.7216878364870578100 ) ) ;
#49538 = CARTESIAN_POINT ( 'NONE',  ( 9.000805734720596973, 12.35661786295821329, -7.869413734470969146 ) ) ;
#49539 = CARTESIAN_POINT ( 'NONE',  ( 3.244645865714153032, -2.039272935636734285, -0.3565889006169955522 ) ) ;
#49540 = CARTESIAN_POINT ( 'NONE',  ( 4.278479993564246797, 7.149254538203735798, 1.199719254218452047 ) ) ;
#49542 = CARTESIAN_POINT ( 'NONE',  ( 3.493197133815315603, 7.227147089426516402, -0.7998128361456291469 ) ) ;
#49541 = CARTESIAN_POINT ( 'NONE',  ( 6.105435528804215473, -2.075010666747591159, 0.2545828925317530911 ) ) ;
#49544 = ORIENTED_EDGE ( 'NONE', *, *, #102718, .F. ) ;
#49543 = CARTESIAN_POINT ( 'NONE',  ( 4.612205747861584548, -0.7811881352849485705, -1.650120847746315622 ) ) ;
#49545 = CARTESIAN_POINT ( 'NONE',  ( 7.703003830858588863, 12.13858823597705872, -0.7998128361456291469 ) ) ;
#49547 = AXIS2_PLACEMENT_3D ( 'NONE', #22001, #19889, #205035 ) ;
#49546 = CARTESIAN_POINT ( 'NONE',  ( 10.14144399767215532, 13.65493833298847548, 7.304070082181278956 ) ) ;
#49548 = CARTESIAN_POINT ( 'NONE',  ( 5.895608061265788180, 1.667329832391790667, 1.445732890734657161 ) ) ;
#49549 = CARTESIAN_POINT ( 'NONE',  ( 1.364683531249997417, 10.79687500034139802, 2.602085213965210642E-15 ) ) ;
#49550 = VERTEX_POINT ( 'NONE', #19743 ) ;
#49551 = CARTESIAN_POINT ( 'NONE',  ( 4.143145976665215002, 0.09703654569752531711, 1.909951782607082427 ) ) ;
#49552 = CARTESIAN_POINT ( 'NONE',  ( -10.63367255181986160, 11.30037282007833532, 1.040834085586084257E-14 ) ) ;
#49553 = CARTESIAN_POINT ( 'NONE',  ( 7.820355676984174664, 8.018169799436671852, -0.7998128361456281477 ) ) ;
#49554 = CARTESIAN_POINT ( 'NONE',  ( 0.6801582343749761339, 1.838541667008058988, -1.178068619123876282 ) ) ;
#49555 = CARTESIAN_POINT ( 'NONE',  ( 4.161989969270892153, 6.839110149915929249, 1.082531754730558626 ) ) ;
#49556 = CARTESIAN_POINT ( 'NONE',  ( 6.614806895146394972, -0.1608752592793839531, 2.155998228907447523 ) ) ;
#49558 = ADVANCED_FACE ( 'NONE', ( #85824 ), #56026, .T. ) ;
#49557 = CARTESIAN_POINT ( 'NONE',  ( 7.104014429467876646, 14.55305237038501076, -9.619583963686880068 ) ) ;
#49559 = CARTESIAN_POINT ( 'NONE',  ( 0.08126746489400815676, -0.8690269180096841239, 1.623235155968821841 ) ) ;
#49560 = ORIENTED_EDGE ( 'NONE', *, *, #173138, .F. ) ;
#49561 = DIRECTION ( 'NONE',  ( 0.000000000000000000, -1.561251128379122346E-12, 1.000000000000000000 ) ) ;
#49562 = EDGE_CURVE ( 'NONE', #143389, #204176, #166727, .T. ) ;
#49563 = CARTESIAN_POINT ( 'NONE',  ( 4.393722961847310593, -0.7179090532695198146, 1.727491627791829742 ) ) ;
#49564 = CARTESIAN_POINT ( 'NONE',  ( 3.834746474454188013E-15, 10.81250000000000355, 1.500000000000001554 ) ) ;
#49565 = DIRECTION ( 'NONE',  ( 0.000000000000000000, 0.000000000000000000, 1.000000000000000000 ) ) ;
#49566 = AXIS2_PLACEMENT_3D ( 'NONE', #199096, #116868, #26224 ) ;
#49567 = VECTOR ( 'NONE', #14960, 1000.000000000000000 ) ;
#49568 = CARTESIAN_POINT ( 'NONE',  ( -8.053180056837398126, 8.497724275839514618, 0.7216878364870578100 ) ) ;
#49569 = CARTESIAN_POINT ( 'NONE',  ( 5.118366684358879759, 5.930181538962194132, 1.199719254218462483 ) ) ;
#49570 = CARTESIAN_POINT ( 'NONE',  ( 1.235132629255174974, -0.04286028942791567098, -1.969139623717565790 ) ) ;
#49571 = CARTESIAN_POINT ( 'NONE',  ( 1.880482680076976720, -0.5405129038237622696, -1.942536604102131026 ) ) ;
#49572 = CARTESIAN_POINT ( 'NONE',  ( -8.670602931139386627, 10.07445716020612103, 1.199719254218462483 ) ) ;
#49573 = CARTESIAN_POINT ( 'NONE',  ( 7.517069824134078537, 7.734612647770044092, 0.000000000000000000 ) ) ;
#49574 = DIRECTION ( 'NONE',  ( 0.000000000000000000, 0.000000000000000000, -1.000000000000000000 ) ) ;
#49575 = CARTESIAN_POINT ( 'NONE',  ( 1.974822964535282610, -0.1094934731284517848, -2.188836591978132518 ) ) ;
#49576 = FILL_AREA_STYLE ('',( #148161 ) ) ;
#49577 = CARTESIAN_POINT ( 'NONE',  ( -9.297140650669053485, 11.86975006391249643, 1.599625672291281386 ) ) ;
#49578 = DIRECTION ( 'NONE',  ( -1.000000000000000000, -1.561251128379122346E-12, 0.000000000000000000 ) ) ;
#49579 = DIRECTION ( 'NONE',  ( -0.5005768354468330683, -0.8656921114426503472, 1.942890293094028284E-15 ) ) ;
#49580 = EDGE_CURVE ( 'NONE', #190224, #144059, #25186, .T. ) ;
#49581 = CARTESIAN_POINT ( 'NONE',  ( 4.584065335196260804, 6.441438539186039591, 1.443375672974065660 ) ) ;
#49582 = CARTESIAN_POINT ( 'NONE',  ( 8.015895134177609904, 10.37496362800581018, 1.599625672291281386 ) ) ;
#49583 = CIRCLE ( 'NONE', #46218, 3.150000000000000799 ) ;
#49584 = CARTESIAN_POINT ( 'NONE',  ( 2.191614386903386613, 5.708633884695917260, -0.7998128361456281477 ) ) ;
#49585 = CARTESIAN_POINT ( 'NONE',  ( 6.129694847154206983, 8.244672969803623630, -1.443375672974078761 ) ) ;
#49586 = ORIENTED_EDGE ( 'NONE', *, *, #162125, .F. ) ;
#49588 = CARTESIAN_POINT ( 'NONE',  ( 1.260403266252381416, 2.010875322206317151, 0.09671919503399273310 ) ) ;
#49587 = CARTESIAN_POINT ( 'NONE',  ( 5.478019777291557979, -1.797689181224306321, -0.3974485807837144224 ) ) ;
#49589 = CARTESIAN_POINT ( 'NONE',  ( 3.163697234774452305, -0.6641558444393131921, -2.200356767709225725 ) ) ;
#49591 = CARTESIAN_POINT ( 'NONE',  ( 1.217372920688150506, 0.3700031967454868176, -1.823611282344459239 ) ) ;
#49590 = CARTESIAN_POINT ( 'NONE',  ( 2.738383840280328663, 5.178236332760252303, 1.082531754730548412 ) ) ;
#49592 = CARTESIAN_POINT ( 'NONE',  ( 3.285556943749998737, -3.405208332855374831, -1.896917185911906500 ) ) ;
#49593 = CARTESIAN_POINT ( 'NONE',  ( -4.060830702492950195, 4.696389560118578999, -1.199719254218452047 ) ) ;
#49594 = FACE_OUTER_BOUND ( 'NONE', #58050, .T. ) ;
#49595 = CARTESIAN_POINT ( 'NONE',  ( 4.623256175466385010, 1.666654777633369555, 0.9376445158523971646 ) ) ;
#49596 = CARTESIAN_POINT ( 'NONE',  ( -8.993135964566285168, 9.386413468282476913, -0.7998128361456291469 ) ) ;
#49597 = CARTESIAN_POINT ( 'NONE',  ( -5.139949633356594383, 9.010708648975750634, 0.000000000000000000 ) ) ;
#49599 = CARTESIAN_POINT ( 'NONE',  ( 1.832664747978371533, 0.1804508633567840359, 1.861920966532565336 ) ) ;
#49598 = CARTESIAN_POINT ( 'NONE',  ( 4.247661304151585604, 2.090252499381782147, -0.05307422152340918187 ) ) ;
#49600 = CARTESIAN_POINT ( 'NONE',  ( 6.317736394288122170, 10.31451686007074997, 0.7216878364870438212 ) ) ;
#49601 = CARTESIAN_POINT ( 'NONE',  ( -1.001543065824772872E-14, 4.884375000341420581, 1.575800808251672791 ) ) ;
#49602 = CARTESIAN_POINT ( 'NONE',  ( 6.093280168761200599, -0.6138376400152152357, 1.736067454429328416 ) ) ;
#49603 = CARTESIAN_POINT ( 'NONE',  ( 2.198393463710220264, 5.716542807637226886, 0.7998128361456462443 ) ) ;
#49604 = DIRECTION ( 'NONE',  ( 5.828670879282089587E-16, -0.8656921114426507913, 0.5005768354468322912 ) ) ;
#49605 = CARTESIAN_POINT ( 'NONE',  ( 4.951616564603428472, 0.5366251361543332710, -1.639350107105986831 ) ) ;
#49606 = CARTESIAN_POINT ( 'NONE',  ( -5.689618019229208734, 9.789638122409414223, 0.7998128361456481317 ) ) ;
#49607 = FACE_OUTER_BOUND ( 'NONE', #166501, .T. ) ;
#49608 = CARTESIAN_POINT ( 'NONE',  ( 1.913843809498073645, 3.268536626279786805, 0.4294081188992979192 ) ) ;
#49609 = CARTESIAN_POINT ( 'NONE',  ( -1.393942678861017415, 0.9000000000000014655, 1.636894562288534694 ) ) ;
#49610 = CARTESIAN_POINT ( 'NONE',  ( 4.926734997883643885, -1.423062915019442043, 1.639699324398981251 ) ) ;
#49611 = CARTESIAN_POINT ( 'NONE',  ( 2.982817717652554101, -0.1347461720548545627, -1.820777111243766733 ) ) ;
#49612 = CARTESIAN_POINT ( 'NONE',  ( 1.006607400890747295, 0.5640878064397096825, 1.878940696355746454 ) ) ;
#49613 = CARTESIAN_POINT ( 'NONE',  ( 5.419199134695255715, -1.912947687149676668, 0.9079543477103575455 ) ) ;
#49615 = CARTESIAN_POINT ( 'NONE',  ( 1.364683531249990311, 3.446875000341416584, 1.214306433183764966E-14 ) ) ;
#49614 = CARTESIAN_POINT ( 'NONE',  ( 6.304234482382112148, 1.701787343685069009, -1.536020108501337855 ) ) ;
#49616 = CARTESIAN_POINT ( 'NONE',  ( 1.608462485350607762, 8.735270501766764895, 2.463594439587639240 ) ) ;
#49617 = CARTESIAN_POINT ( 'NONE',  ( 8.646349277213076334, 11.11049346154719508, 1.599625672291281386 ) ) ;
#49618 = CARTESIAN_POINT ( 'NONE',  ( 1.383610671357866639, 0.1525377206293351273, -2.115047022047947589 ) ) ;
#49619 = CARTESIAN_POINT ( 'NONE',  ( -5.924549939491850381, 6.014322472269677533, 0.000000000000000000 ) ) ;
#49620 = DIRECTION ( 'NONE',  ( 0.6507913734559641616, -0.7592566023653004592, 0.000000000000000000 ) ) ;
#49621 = CARTESIAN_POINT ( 'NONE',  ( -5.233084104750526322, 5.207612331738130429, 0.000000000000000000 ) ) ;
#49622 = CARTESIAN_POINT ( 'NONE',  ( 6.825048293896172957, -1.981324744236719004, -0.8880960284254543202 ) ) ;
#49624 = CARTESIAN_POINT ( 'NONE',  ( -1.500000000000015099, 13.01041666734946567, -0.8660254037844309360 ) ) ;
#49623 = FACE_OUTER_BOUND ( 'NONE', #42167, .T. ) ;
#49626 = VERTEX_POINT ( 'NONE', #174574 ) ;
#49625 = CARTESIAN_POINT ( 'NONE',  ( 2.350487294161308860, 1.044453463271700633, -1.960417310804033031 ) ) ;
#49627 = CARTESIAN_POINT ( 'NONE',  ( -0.03393210605391345364, -2.232032725161440023, -0.5493522527948471179 ) ) ;
#49629 = CARTESIAN_POINT ( 'NONE',  ( 4.346570391463054683, -2.039393746373055372, -0.3077390332135512829 ) ) ;
#49628 = CARTESIAN_POINT ( 'NONE',  ( 5.007038802148489509, 4.735966778795008381, 0.7998128361456341429 ) ) ;
#49631 = CARTESIAN_POINT ( 'NONE',  ( -1.737499999999997824, -3.791666666666665186, 3.009438278150925683 ) ) ;
#49630 = CARTESIAN_POINT ( 'NONE',  ( 5.773793314573267388, 7.829454515125894964, 1.599625672291268286 ) ) ;
#49632 = EDGE_CURVE ( 'NONE', #70421, #31187, #111433, .T. ) ;
#49633 = CARTESIAN_POINT ( 'NONE',  ( 5.363132282657546490, 8.414682208812571673, -1.199719254218452047 ) ) ;
#49634 = CARTESIAN_POINT ( 'NONE',  ( 1.642778471875001811, -3.230208332855373676, 2.845375778867859751 ) ) ;
#49636 = CARTESIAN_POINT ( 'NONE',  ( 0.2344723086637650333, 0.3594713984965206000, 2.059332689821891105 ) ) ;
#49635 = B_SPLINE_CURVE_WITH_KNOTS ( 'NONE', 3,
 ( #100917, #18596, #173416, #24997, #39130, #91099 ),
 .UNSPECIFIED., .F., .F.,
 ( 4, 2, 4 ),
 ( 0.000000000000000000, 0.0001363166885564072721, 0.0002726333771128145443 ),
 .UNSPECIFIED. ) ;
#49637 = CARTESIAN_POINT ( 'NONE',  ( 4.810013364240863787, 1.265987717737980134, -1.337210144835267345 ) ) ;
#49638 = EDGE_CURVE ( 'NONE', #80984, #146527, #98579, .T. ) ;
#49639 = CARTESIAN_POINT ( 'NONE',  ( 4.710568305744190276, 7.583081225755162968, 1.199719254218462483 ) ) ;
#49640 = SURFACE_STYLE_USAGE ( .BOTH. , #111510 ) ;
#49641 = CARTESIAN_POINT ( 'NONE',  ( 1.307153468561640164, -0.4245502288011630543, 1.671566548543522268 ) ) ;
#49642 = CARTESIAN_POINT ( 'NONE',  ( 0.4093891192313535710, -1.913260280790154866, 0.6371585790938688598 ) ) ;
#49643 = CARTESIAN_POINT ( 'NONE',  ( 1.864337758866913441, -0.1181282521124735752, -2.295782230965204285 ) ) ;
#49644 = CARTESIAN_POINT ( 'NONE',  ( -1.001543065824772872E-14, 4.384375000341417916, 1.575800808251672791 ) ) ;
#49645 = CARTESIAN_POINT ( 'NONE',  ( 1.370828697373091432, -1.435183881573602216, 1.748884408748638597 ) ) ;
#49646 = CARTESIAN_POINT ( 'NONE',  ( 4.336618311946851101, 2.065336219181472366, 0.4112933666130594301 ) ) ;
#49647 = CARTESIAN_POINT ( 'NONE',  ( -3.471769853551161411, 6.208092708188416076, 1.199719254218452935 ) ) ;
#49648 = CARTESIAN_POINT ( 'NONE',  ( 2.934531203469164851, 0.2125141484592401875, 1.756833830538252483 ) ) ;
#49649 = CARTESIAN_POINT ( 'NONE',  ( 5.937581207780954884, 9.014596278131406848, -1.199719254218440723 ) ) ;
#49650 = CARTESIAN_POINT ( 'NONE',  ( 4.055297343818923039, 7.745280977848496562, 0.7216878364870257245 ) ) ;
#49651 = CARTESIAN_POINT ( 'NONE',  ( -4.564291269294938225, 8.476756914152748124, 1.040834085586084257E-14 ) ) ;
#49652 = UNCERTAINTY_MEASURE_WITH_UNIT (LENGTH_MEASURE( 1.000000000000000082E-05 ), #51684, 'distance_accuracy_value', 'NONE');
#49653 = CARTESIAN_POINT ( 'NONE',  ( 5.788968402910805722, 7.776882441527838807, 1.443375672974062551 ) ) ;
#49654 = CARTESIAN_POINT ( 'NONE',  ( -1.201851678989727383E-14, 2.212500000000021672, 1.732050807568877637 ) ) ;
#49655 = CARTESIAN_POINT ( 'NONE',  ( -4.948889764188092677, 5.732458465429559169, 1.199719254218462483 ) ) ;
#49656 = CARTESIAN_POINT ( 'NONE',  ( 5.168325547630102434, 2.218848025724213802, -0.1096118590232265239 ) ) ;
#49657 = CARTESIAN_POINT ( 'NONE',  ( 3.257961296797746265, 0.9855263100190698733, 1.957416934251283935 ) ) ;
#49658 = CARTESIAN_POINT ( 'NONE',  ( -4.076197739202962467, 7.907314462378773001, 1.040834085586084257E-14 ) ) ;
#49659 = CARTESIAN_POINT ( 'NONE',  ( -2.972980823146582186, 6.690504403638126263, 0.000000000000000000 ) ) ;
#49660 = CARTESIAN_POINT ( 'NONE',  ( 5.479186192515411946, -1.917069751554843160, -0.9065152316691318379 ) ) ;
#49661 = CIRCLE ( 'NONE', #4639, 10.99999999999999112 ) ;
#49662 = CARTESIAN_POINT ( 'NONE',  ( -1.201851678989727383E-14, 3.071875000341420137, 1.575800808251672791 ) ) ;
#49663 = CARTESIAN_POINT ( 'NONE',  ( 6.889999999999985469, 0.6064005686075202295, 1.774654002403662778 ) ) ;
#49664 = CARTESIAN_POINT ( 'NONE',  ( -3.606105671554953318, 7.150947683548662503, 0.7216878364870317197 ) ) ;
#49665 = CARTESIAN_POINT ( 'NONE',  ( 5.414351406770180120, -2.120778210838507150, 0.002142078463891750485 ) ) ;
#49666 = CARTESIAN_POINT ( 'NONE',  ( -7.593975437430151132, 8.032261896522864930, -0.7216878364870338292 ) ) ;
#49667 = ORIENTED_EDGE ( 'NONE', *, *, #84346, .F. ) ;
#49669 = CARTESIAN_POINT ( 'NONE',  ( -1.483456582844936422, 7.293967155396054558, 4.258619948151441292 ) ) ;
#49668 = CARTESIAN_POINT ( 'NONE',  ( -4.909461021924285795, 6.821066840368686712, 1.443375672974058777 ) ) ;
#49670 = CARTESIAN_POINT ( 'NONE',  ( 6.003563092752934871, 5.898578451166879510, 0.7998128361456341429 ) ) ;
#49671 = CARTESIAN_POINT ( 'NONE',  ( 5.917501325027624937, -1.028386522942719816, -1.527094029191010893 ) ) ;
#49672 = CARTESIAN_POINT ( 'NONE',  ( 1.364683531249988535, 3.176041667008084435, 0.7879004041258500513 ) ) ;
#49673 = CARTESIAN_POINT ( 'NONE',  ( 1.645671328968565605, 0.5460171089132167532, 1.652615436037402130 ) ) ;
#49674 = CARTESIAN_POINT ( 'NONE',  ( 3.521367211247359741, 5.131347717920458962, -1.599625672291262513 ) ) ;
#49675 = CARTESIAN_POINT ( 'NONE',  ( 0.3616705494772323726, -0.5269360983083425376, 1.889693748445469224 ) ) ;
#49676 = CARTESIAN_POINT ( 'NONE',  ( -1.364683531250014514, 0.3427083336747508424, 0.7879004041258379498 ) ) ;
#49677 = DIRECTION ( 'NONE',  ( 0.000000000000000000, -1.000000000000000000, 0.000000000000000000 ) ) ;
#49678 = CARTESIAN_POINT ( 'NONE',  ( 5.629794960336353071, -1.368038101806166029, -1.673757646710342550 ) ) ;
#49679 = CARTESIAN_POINT ( 'NONE',  ( -2.286521462199063492, 5.819358805874190743, 1.040834085586084257E-14 ) ) ;
#49680 = CARTESIAN_POINT ( 'NONE',  ( -5.544921637864820951, 9.412899644243539754, -0.7216878364870207285 ) ) ;
#49681 = CARTESIAN_POINT ( 'NONE',  ( 4.575171270262055501, 0.003154952768896768234, -2.161883445794945846 ) ) ;
#49683 = VERTEX_POINT ( 'NONE', #137794 ) ;
#49682 = CARTESIAN_POINT ( 'NONE',  ( -4.767627293860968507, 5.591261926706423857, -1.199719254218453823 ) ) ;
#49684 = CARTESIAN_POINT ( 'NONE',  ( -1.201851678989727383E-14, 2.821875000341418804, 1.575800808251672791 ) ) ;
#49685 = CARTESIAN_POINT ( 'NONE',  ( 5.712177144062582812, -0.8841330711255364072, -1.762019952394773936 ) ) ;
#49686 = CARTESIAN_POINT ( 'NONE',  ( 5.290307710256559659, -1.645723771949607173, 0.5459688634881465497 ) ) ;
#49688 = CARTESIAN_POINT ( 'NONE',  ( 2.419692422129790632, -1.264489869534379141, -1.789777738334753732 ) ) ;
#49687 = CARTESIAN_POINT ( 'NONE',  ( 0.6801582343749952297, -0.9427083329919122567, -1.178068619123855409 ) ) ;
#49689 = CARTESIAN_POINT ( 'NONE',  ( 2.837322237161111094, 0.2816050128923338058, 2.290267077920715710 ) ) ;
#49690 = CARTESIAN_POINT ( 'NONE',  ( 5.272755944101470860, -1.938957023840400362, -0.6983732565980956819 ) ) ;
#49691 = CARTESIAN_POINT ( 'NONE',  ( -0.02948999725180690215, 0.001137248348246927814, -1.926291057026579656 ) ) ;
#49692 = CARTESIAN_POINT ( 'NONE',  ( -7.836249598574384301, 8.244638741199329601, 1.040834085586084257E-14 ) ) ;
#49693 = CARTESIAN_POINT ( 'NONE',  ( -3.820365424000704557, 7.679119771301277098, -0.7998128361456481317 ) ) ;
#49694 = CARTESIAN_POINT ( 'NONE',  ( 0.000000000000000000, -7.666862915010147717, 0.000000000000000000 ) ) ;
#49695 = CARTESIAN_POINT ( 'NONE',  ( 4.430007776716601953, -2.079114408633813582, 0.4165480963118637914 ) ) ;
#49696 = SURFACE_STYLE_USAGE ( .BOTH. , #102720 ) ;
#49697 = CARTESIAN_POINT ( 'NONE',  ( 1.705704151892040832, 1.882474636155605507, 0.7231385473688843879 ) ) ;
#49698 = CARTESIAN_POINT ( 'NONE',  ( -7.361714222096077620, 7.691014135307965738, 0.7216878364870317197 ) ) ;
#49699 = CARTESIAN_POINT ( 'NONE',  ( 4.137865722265689605, -1.519559189622637252, -1.600479987451455699 ) ) ;
#49700 = CARTESIAN_POINT ( 'NONE',  ( -1.642778471875000035, -0.9552083328553742092, -2.845375778867859751 ) ) ;
#49701 = CARTESIAN_POINT ( 'NONE',  ( -0.1288028175206361037, 4.078893953557697571, -2.828657143142800034 ) ) ;
#49702 = CARTESIAN_POINT ( 'NONE',  ( 0.000000000000000000, 0.5000000000000004441, -3.475000000000000089 ) ) ;
#49703 = DIRECTION ( 'NONE',  ( 1.000000000000000000, 3.451266460341926649E-31, 0.000000000000000000 ) ) ;
#49705 = CARTESIAN_POINT ( 'NONE',  ( 6.825078400183575589, -0.005632053428735600553, 2.144262460745151255 ) ) ;
#49704 = CARTESIAN_POINT ( 'NONE',  ( -4.586029276033976920, 8.497253585842676316, 0.07182003436798957419 ) ) ;
#49706 = PLANE ( 'NONE',  #113232 ) ;
#49707 = ORIENTED_EDGE ( 'NONE', *, *, #42099, .T. ) ;
#49708 = CARTESIAN_POINT ( 'NONE',  ( 3.590745217537123057, -0.4003831998886059340, -2.021439917362640504 ) ) ;
#49709 = CARTESIAN_POINT ( 'NONE',  ( 0.6801582343749761339, 1.973958333674710630, 1.178068619123801675 ) ) ;
#49710 = CARTESIAN_POINT ( 'NONE',  ( -4.543954038874438162, 8.453030145328826350, 1.040834085586084257E-14 ) ) ;
#49711 = CARTESIAN_POINT ( 'NONE',  ( 3.088540408894335787, -1.201353318763114020, 1.623377594596470352 ) ) ;
#49712 = CARTESIAN_POINT ( 'NONE',  ( -0.7500000000000249800, -0.5583333333333134751, 1.299038105676659116 ) ) ;
#49713 = CARTESIAN_POINT ( 'NONE',  ( 2.347533153460546806, 5.890539112345938300, 0.000000000000000000 ) ) ;
#49714 = CARTESIAN_POINT ( 'NONE',  ( 3.625900526125751089, -1.226333045360414653, -1.656161981788171200 ) ) ;
#49715 = CARTESIAN_POINT ( 'NONE',  ( 3.734320285776532078, 4.105063559066064016, 0.9403128211546033510 ) ) ;
#49716 = CARTESIAN_POINT ( 'NONE',  ( 5.952193131599331721, 6.902979060742733708, 1.199719254218462483 ) ) ;
#49717 = CARTESIAN_POINT ( 'NONE',  ( 3.169157936054858293, 1.820986098869777470, -0.8666075021629695563 ) ) ;
#49718 = CARTESIAN_POINT ( 'NONE',  ( -0.2409995289980245703, 0.2355275985303668385, -2.034371242098035548 ) ) ;
#49719 = CARTESIAN_POINT ( 'NONE',  ( 1.587592257565925813, -1.832131100469553520, -0.1817911664281982032 ) ) ;
#49720 = CARTESIAN_POINT ( 'NONE',  ( 6.217417563691929772, -0.2743312036321900460, 2.189694890431858276 ) ) ;
#49721 = CARTESIAN_POINT ( 'NONE',  ( 6.658989722967328717, 7.797851427330578566, 1.199719254218452935 ) ) ;
#49722 = CARTESIAN_POINT ( 'NONE',  ( 1.704591423195594535, -0.7763021076895926242, -2.017573427605146907 ) ) ;
#49723 = CARTESIAN_POINT ( 'NONE',  ( -4.175548123328963079, 4.934189567714277302, 1.082531754730560403 ) ) ;
#49724 = CARTESIAN_POINT ( 'NONE',  ( 1.798064920797682653, -0.9548589541341389042, -1.776165177175797583 ) ) ;
#49725 = CARTESIAN_POINT ( 'NONE',  ( 2.109147326763362695, 0.8800818102412102384, -2.123382460422203355 ) ) ;
#49726 = CARTESIAN_POINT ( 'NONE',  ( 1.806654366501771136, 0.000000000000000000, 2.419999999999998597 ) ) ;
#49727 = CARTESIAN_POINT ( 'NONE',  ( 0.5142528298564854605, 1.293200884458247657, -1.351890787750304135 ) ) ;
#49728 = CARTESIAN_POINT ( 'NONE',  ( 11.45846087878786612, 11.09311600781393814, 3.566076377698156996 ) ) ;
#49729 =( GEOMETRIC_REPRESENTATION_CONTEXT ( 3 ) GLOBAL_UNCERTAINTY_ASSIGNED_CONTEXT ( ( #107569 ) ) GLOBAL_UNIT_ASSIGNED_CONTEXT ( ( #50152, #167110, #57621 ) ) REPRESENTATION_CONTEXT ( 'NONE', 'WORKASPACE' ) );
#49730 = CARTESIAN_POINT ( 'NONE',  ( 4.838727080925394830, 0.3361901323847040213, 1.942436603694275510 ) ) ;
#49731 = CARTESIAN_POINT ( 'NONE',  ( 5.155482549980198392, 1.942097955248718533, -0.5424665614216088727 ) ) ;
#49733 = CARTESIAN_POINT ( 'NONE',  ( 10.66990370383054731, 11.55056853066490952, 0.7216878364870317197 ) ) ;
#49732 = CARTESIAN_POINT ( 'NONE',  ( 0.6823417656249899377, 1.842708333674752952, 1.181850606188755259 ) ) ;
#49735 = CARTESIAN_POINT ( 'NONE',  ( 6.551405291548149101, -1.690254494844857014, -1.256206543278805876 ) ) ;
#49734 = CARTESIAN_POINT ( 'NONE',  ( -6.042130013184518589, 10.20090211535728031, -0.7998128361456291469 ) ) ;
#49736 = AXIS2_PLACEMENT_3D ( 'NONE', #20872, #150925, #136801 ) ;
#49737 = CARTESIAN_POINT ( 'NONE',  ( 5.318829906782316819, -1.502041817331278173, 1.425132596443792643 ) ) ;
#49738 = CARTESIAN_POINT ( 'NONE',  ( 7.630541526392844887, 7.796719957080126662, 0.7998128361456341429 ) ) ;
#49739 = CARTESIAN_POINT ( 'NONE',  ( -6.898401231254901234, 6.942556279419168419, -0.7998128361456291469 ) ) ;
#49740 = CARTESIAN_POINT ( 'NONE',  ( -1.458514304043844634, 8.731595392684152301, 2.560210433951525033 ) ) ;
#49741 = CARTESIAN_POINT ( 'NONE',  ( 5.115492516475182327, 1.653579564094692866, 1.159561630411933830 ) ) ;
#49742 = CARTESIAN_POINT ( 'NONE',  ( -1.602468905319636405E-14, -1.131249999317182064, -1.732050807568870754 ) ) ;
#49743 = CARTESIAN_POINT ( 'NONE',  ( 3.545847025713305012, -1.747029255069532550, -1.507864240153370172 ) ) ;
#49744 = EDGE_CURVE ( 'NONE', #78710, #182393, #139068, .T. ) ;
#49745 = CARTESIAN_POINT ( 'NONE',  ( 0.4794367124230074495, -0.1050040150484717050, 2.060039547518006664 ) ) ;
#49746 = CARTESIAN_POINT ( 'NONE',  ( 6.968527767744088663, 11.07377346243604599, 0.7216878364870438212 ) ) ;
#49747 = CARTESIAN_POINT ( 'NONE',  ( 6.587282531393223728, 8.778525268082516320, 1.599625672291268286 ) ) ;
#49748 = CARTESIAN_POINT ( 'NONE',  ( 5.682802662783380754, 6.658966523782627434, 1.199719254218452935 ) ) ;
#49749 = CARTESIAN_POINT ( 'NONE',  ( -0.6823417656250003738, 0.5302083336747518416, -1.181850606188749264 ) ) ;
#49750 = CARTESIAN_POINT ( 'NONE',  ( 5.727393547130178675, 5.646656991265468939, 0.000000000000000000 ) ) ;
#49751 = CARTESIAN_POINT ( 'NONE',  ( 7.266807146800403849, 7.580289214129690478, 1.040834085586084257E-14 ) ) ;
#49753 = CARTESIAN_POINT ( 'NONE',  ( 11.41176686791169281, 12.34049196513144153, 3.404018756831826309 ) ) ;
#49752 = CARTESIAN_POINT ( 'NONE',  ( 3.983024850003999973, 2.060528110339276520, 0.6844299113566986170 ) ) ;
#49754 = CARTESIAN_POINT ( 'NONE',  ( -5.817857313595549584, 6.920493299683823096, 1.082531754730549078 ) ) ;
#49756 = CARTESIAN_POINT ( 'NONE',  ( 2.682954136603598272, 1.303717545168959990, 1.300458928786947688 ) ) ;
#49755 = CARTESIAN_POINT ( 'NONE',  ( -5.151735183512911043, 6.073074471262228435, 1.082531754730548412 ) ) ;
#49757 = B_SPLINE_CURVE_WITH_KNOTS ( 'NONE', 3,
 ( #106060, #92981, #125541, #160087, #189386, #23675, #77762, #41028, #75645, #11690 ),
 .UNSPECIFIED., .F., .F.,
 ( 4, 3, 3, 4 ),
 ( 0.000000000000000000, 6.254645189632222226E-05, 9.576573040555354656E-05, 0.0001290265995014244630 ),
 .UNSPECIFIED. ) ;
#49758 = CARTESIAN_POINT ( 'NONE',  ( 1.364683531249988535, 4.905208333674756283, -0.7879004041258300672 ) ) ;
#49759 = CARTESIAN_POINT ( 'NONE',  ( 4.687173145698103838, 1.624054394666199830, 1.471728111018810070 ) ) ;
#49760 = CARTESIAN_POINT ( 'NONE',  ( 8.456790047136887978, 13.99512100581969065, 8.514254332811203696 ) ) ;
#49761 = CARTESIAN_POINT ( 'NONE',  ( 5.137693465899466183, -1.596169073733178845, -1.603756505840604918 ) ) ;
#49762 = CARTESIAN_POINT ( 'NONE',  ( -5.904496024515287544, 6.143719773163115683, -0.8530293227379917020 ) ) ;
#49763 = CARTESIAN_POINT ( 'NONE',  ( 5.318333368960210805, 7.618274611128187601, -1.232678415538956518 ) ) ;
#49764 = CARTESIAN_POINT ( 'NONE',  ( -5.926322542504872892, 8.007405281046052536, -1.443375672974066548 ) ) ;
#49765 = CARTESIAN_POINT ( 'NONE',  ( 5.234856708652235291, 5.279956712948652431, 0.7216878364870338292 ) ) ;
#49766 = CARTESIAN_POINT ( 'NONE',  ( 0.1976571007769452604, -1.769309276362411643, -0.05040135802934773979 ) ) ;
#49767 = CARTESIAN_POINT ( 'NONE',  ( 4.055341430421886884, -1.750343679372264205, 0.9943053665309193878 ) ) ;
#49768 = CARTESIAN_POINT ( 'NONE',  ( 7.955937213120826357, 8.176348258262782664, 0.7998128361456481317 ) ) ;
#49769 = CARTESIAN_POINT ( 'NONE',  ( 3.346800460960248191, 0.5101267414385314281, 2.043117269239830947 ) ) ;
#49770 = CARTESIAN_POINT ( 'NONE',  ( 0.5795164177304649167, -0.6885740665637375413, 1.787764417203549172 ) ) ;
#49771 = CARTESIAN_POINT ( 'NONE',  ( 3.063252641683779753, 5.661212951017999373, 1.199719254218450271 ) ) ;
#49772 = CARTESIAN_POINT ( 'NONE',  ( 1.750388463564346075, -1.959780499145358679, -0.1960735186044142708 ) ) ;
#49773 = CARTESIAN_POINT ( 'NONE',  ( 0.3736316133628528879, 1.073300769168658908, 1.531925686032776124 ) ) ;
#49774 = CARTESIAN_POINT ( 'NONE',  ( 1.416376618315864144, 0.7919773292732554815, 1.795081228748253377 ) ) ;
#49776 = ORIENTED_EDGE ( 'NONE', *, *, #175293, .F. ) ;
#49775 = CARTESIAN_POINT ( 'NONE',  ( 0.1055216070770526038, 1.418477292093557329, 1.282857148695019989 ) ) ;
#49777 = CARTESIAN_POINT ( 'NONE',  ( 6.344852701515477200, 6.504675694630598137, -0.7216878364870257245 ) ) ;
#49778 = CARTESIAN_POINT ( 'NONE',  ( -1.364683531250014514, 0.8010416670080889867, -0.7879004041258289570 ) ) ;
#49779 = ADVANCED_FACE ( 'NONE', ( #203813 ), #145899, .T. ) ;
#49780 = CARTESIAN_POINT ( 'NONE',  ( 6.473518811298506037, 1.789458955665638396, -0.5451884755478533240 ) ) ;
#49781 = CARTESIAN_POINT ( 'NONE',  ( -1.580000000000022276, 8.674529973577531194, 2.420000000000010587 ) ) ;
#49782 = CARTESIAN_POINT ( 'NONE',  ( 6.157099584139436033, 1.695871835526874483, -1.187180358042688511 ) ) ;
#49783 = CARTESIAN_POINT ( 'NONE',  ( 9.579665964948882007, -7.473374494045003757, 1.734723475976807094E-15 ) ) ;
#49784 =( BOUNDED_CURVE ( )  B_SPLINE_CURVE ( 2, ( #93191, #137665, #74786, #88916, #141951 ),
 .UNSPECIFIED., .F., .T. ) 
 B_SPLINE_CURVE_WITH_KNOTS ( ( 3, 2, 3 ),
 ( 0.02182863351722338224, 0.02500000000000000139, 0.02741006098507890384 ),
 .UNSPECIFIED. ) 
 CURVE ( )  GEOMETRIC_REPRESENTATION_ITEM ( )  RATIONAL_B_SPLINE_CURVE ( ( 0.9368349873065047184, 0.9490140947222125423, 1.000000000000000000, 0.9612535663203012337, 0.9449186369899758020 ) ) 
 REPRESENTATION_ITEM ( '' )  );
#49785 = CARTESIAN_POINT ( 'NONE',  ( 0.8013346216862862192, -1.776568573310655985, 1.062853015585236482 ) ) ;
#49786 = CARTESIAN_POINT ( 'NONE',  ( -1.499999999999997780, 1.900000000000019673, 0.000000000000000000 ) ) ;
#49787 = CARTESIAN_POINT ( 'NONE',  ( 7.637320603199683866, 7.804628880021436288, -0.7998128361456281477 ) ) ;
#49788 = CARTESIAN_POINT ( 'NONE',  ( -6.530223543276495235, 10.77034456713125188, -0.7998128361456291469 ) ) ;
#49789 = CARTESIAN_POINT ( 'NONE',  ( 4.193214648376505593, 8.114110533073061404, 0.000000000000000000 ) ) ;
#49790 = CARTESIAN_POINT ( 'NONE',  ( 5.022192282182047940, -2.110239842997441606, 0.2083548542347323507 ) ) ;
#49791 = CARTESIAN_POINT ( 'NONE',  ( 3.386504508363381571, 7.172948703057747011, -0.7998128361456362523 ) ) ;
#49792 = CARTESIAN_POINT ( 'NONE',  ( -1.201851678989727383E-14, 1.071875000341418138, 1.575800808251672791 ) ) ;
#49793 = ORIENTED_EDGE ( 'NONE', *, *, #119633, .T. ) ;
#49794 = CARTESIAN_POINT ( 'NONE',  ( 1.499999999999989120, 2.525000000000020339, 1.214306433183764966E-14 ) ) ;
#49796 = CARTESIAN_POINT ( 'NONE',  ( 4.416205349749311004, 6.175325546172740765, 1.599625672291267398 ) ) ;
#49795 = CARTESIAN_POINT ( 'NONE',  ( 5.863715402168388380, -0.4781514528688200483, 1.902565108626976809 ) ) ;
#49797 = CARTESIAN_POINT ( 'NONE',  ( 3.093124880496417983, 1.122326866504215426, -1.674630914042275709 ) ) ;
#49798 = CARTESIAN_POINT ( 'NONE',  ( 3.362411380332845035, -1.847649188899632255, -0.5059680389012406465 ) ) ;
#49799 = CARTESIAN_POINT ( 'NONE',  ( 11.89839339040395316, 9.771225315960784030, -1.560885614203536997 ) ) ;
#49800 = CARTESIAN_POINT ( 'NONE',  ( 1.663894474538109236, 1.130263417742288112, 1.877492182091732076 ) ) ;
#49801 = CARTESIAN_POINT ( 'NONE',  ( 0.2335667940002632559, 2.006215057630795773, -2.568298294197084886 ) ) ;
#49802 = CARTESIAN_POINT ( 'NONE',  ( 3.110468855859845672, 1.357358932127524120, -1.287316363804760888 ) ) ;
#49803 = CARTESIAN_POINT ( 'NONE',  ( -1.500000000000015099, -1.047916665983845919, 0.8660254037844403729 ) ) ;
#49804 = CARTESIAN_POINT ( 'NONE',  ( -6.021792782764022078, 10.17717534653336209, -0.7998128361456291469 ) ) ;
#49806 = CARTESIAN_POINT ( 'NONE',  ( 5.501600788752927684, -2.065472302299308893, 0.4645820118519652930 ) ) ;
#49805 = CARTESIAN_POINT ( 'NONE',  ( -5.450014563013544588, 5.460697866378308341, 0.7216878364870317197 ) ) ;
#49807 = CARTESIAN_POINT ( 'NONE',  ( -1.329432108394029477, 13.36331283326043007, 0.3989760537385304007 ) ) ;
#49808 = CARTESIAN_POINT ( 'NONE',  ( -1.500000000000053957, 7.176846818246210624, -4.202462424328210489 ) ) ;
#49810 = CARTESIAN_POINT ( 'NONE',  ( 6.620655732516645742, 7.051964633898824886, 2.771890290588132189 ) ) ;
#49809 = CARTESIAN_POINT ( 'NONE',  ( 2.208638616728377357, 1.868957087031404285, 0.9372459875717062960 ) ) ;
#49812 = VERTEX_POINT ( 'NONE', #139939 ) ;
#49811 = CARTESIAN_POINT ( 'NONE',  ( 0.2699429432127123385, -1.132711312255540115, 1.300796998575669772 ) ) ;
#49813 = ADVANCED_FACE ( 'NONE', ( #92265 ), #190832, .T. ) ;
#49814 = CARTESIAN_POINT ( 'NONE',  ( 5.452350330990040739, 9.512825819463730070, 0.7998128361456462443 ) ) ;
#49815 = CARTESIAN_POINT ( 'NONE',  ( -0.7500000000000179856, 12.07291666734946389, 1.299038105676658228 ) ) ;
#49816 = CARTESIAN_POINT ( 'NONE',  ( -10.97030176249251276, 13.79999999999998295, 1.695215491223428739 ) ) ;
#49817 = CARTESIAN_POINT ( 'NONE',  ( -10.10575425844435138, 4.358269247758318699, 5.859476710806498900 ) ) ;
#49819 = CARTESIAN_POINT ( 'NONE',  ( 8.392133896734662812, 10.81390885098904420, 1.443375672974076540 ) ) ;
#49818 = CARTESIAN_POINT ( 'NONE',  ( 6.877010230629674759, 9.046264573866535486, 1.599625672291281386 ) ) ;
#49820 = CARTESIAN_POINT ( 'NONE',  ( 8.923337013803674722, 2.630042260599927850, 8.023366178422937978 ) ) ;
#49822 = CARTESIAN_POINT ( 'NONE',  ( 1.084272394670304118, -1.149816064065724230, 1.399778539804387822 ) ) ;
#49821 = CARTESIAN_POINT ( 'NONE',  ( 4.667750024854814050, 8.667735138964429709, -0.7998128361456381397 ) ) ;
#49823 = CARTESIAN_POINT ( 'NONE',  ( -7.314787569772770226, 8.492672571945082183, -1.199719254218452935 ) ) ;
#49824 = CARTESIAN_POINT ( 'NONE',  ( 3.181359600701000989, 6.863336634126477875, 0.000000000000000000 ) ) ;
#49825 = CARTESIAN_POINT ( 'NONE',  ( -6.492041734278776843, 6.763935894940780180, 0.1675349064616058481 ) ) ;
#49826 = CARTESIAN_POINT ( 'NONE',  ( 6.038177310039780643, 8.137902509836795417, -1.599625672291283607 ) ) ;
#49827 = CARTESIAN_POINT ( 'NONE',  ( 11.86145016429272836, 13.40000000000000036, -1.100000000000002087 ) ) ;
#49828 = CARTESIAN_POINT ( 'NONE',  ( 0.000000000000000000, -0.9200000000000041478, 0.000000000000000000 ) ) ;
#49829 = CARTESIAN_POINT ( 'NONE',  ( 4.001984418394623155, 7.593073144423666321, -0.1798963839820325039 ) ) ;
#49830 = CARTESIAN_POINT ( 'NONE',  ( 9.490344339885973923, 12.09515436799890331, -1.443375672974057666 ) ) ;
#49831 = ORIENTED_EDGE ( 'NONE', *, *, #115920, .T. ) ;
#49832 = CARTESIAN_POINT ( 'NONE',  ( 3.244433657958167849, -1.833057675465451730, -0.3206290368645177136 ) ) ;
#49833 = CARTESIAN_POINT ( 'NONE',  ( -0.1060672704247594272, -0.8202269080865699502, -1.729793120397028927 ) ) ;
#49834 = CARTESIAN_POINT ( 'NONE',  ( 6.088885551643496541, -0.2832829338282101261, -1.905325039026314560 ) ) ;
#49835 = CARTESIAN_POINT ( 'NONE',  ( -1.844031106778978302, 8.927559574663328945, 0.7750000000000013545 ) ) ;
#49836 = CARTESIAN_POINT ( 'NONE',  ( 4.851297196472967421, 8.072458764906237150, -0.9094135686919021522 ) ) ;
#49837 = SURFACE_STYLE_USAGE ( .BOTH. , #82327 ) ;
#49838 = CARTESIAN_POINT ( 'NONE',  ( -4.772106882330241717, 5.630174786549132726, -1.082531754730544860 ) ) ;
#49839 = CARTESIAN_POINT ( 'NONE',  ( 7.931156674314368438, 12.19684052010138586, 1.040834085586084257E-14 ) ) ;
#49840 = CARTESIAN_POINT ( 'NONE',  ( 5.049637312653283416, 1.456549282395647849, 1.325737238711437893 ) ) ;
#49841 = CARTESIAN_POINT ( 'NONE',  ( 1.401209248766785542, -0.3145075555085960484, -2.096923750572597722 ) ) ;
#49842 = CARTESIAN_POINT ( 'NONE',  ( -5.205440912643032547, 8.160432600470439723, 1.199719254218452047 ) ) ;
#49843 = CARTESIAN_POINT ( 'NONE',  ( -11.94980361058168938, 10.19999999999999929, -1.100000000000000311 ) ) ;
#49844 = CARTESIAN_POINT ( 'NONE',  ( -7.065207446497166366, 9.336104335703744539, 0.000000000000000000 ) ) ;
#49845 = CARTESIAN_POINT ( 'NONE',  ( 5.912113082354764515, 1.474260358680115068, -1.621598248542432064 ) ) ;
#49846 = CARTESIAN_POINT ( 'NONE',  ( 2.679285714285720044, 0.4970443252110459120, -0.5000000000000004441 ) ) ;
#49847 = CARTESIAN_POINT ( 'NONE',  ( 4.155238220467009747, -1.601147421941846227, -1.070839854175157813 ) ) ;
#49848 = CARTESIAN_POINT ( 'NONE',  ( -7.043624497499477499, 8.176315654292865887, 1.199719254218450271 ) ) ;
#49849 = CARTESIAN_POINT ( 'NONE',  ( 0.08272424614634911466, -0.1293432359340887239, -1.795996506534849546 ) ) ;
#49850 = CARTESIAN_POINT ( 'NONE',  ( 1.383733252933561086, 2.037972573443189717, -0.8472329510355591786 ) ) ;
#49851 = ADVANCED_FACE ( 'NONE', ( #138862 ), #211700, .T. ) ;
#49852 = CARTESIAN_POINT ( 'NONE',  ( 3.469446951953614189E-15, 5.900000000000023448, 1.214306433183764966E-14 ) ) ;
#49853 = ORIENTED_EDGE ( 'NONE', *, *, #71271, .T. ) ;
#49854 = SURFACE_SIDE_STYLE ('',( #159609 ) ) ;
#49855 = ORIENTED_EDGE ( 'NONE', *, *, #18560, .T. ) ;
#49856 = CARTESIAN_POINT ( 'NONE',  ( 6.174653332693735841, 1.325436276047034179, -1.456821488112548080 ) ) ;
#49857 = CARTESIAN_POINT ( 'NONE',  ( 1.979929434068830929, -1.904991468646766606, -0.3768183752349169580 ) ) ;
#49858 = CARTESIAN_POINT ( 'NONE',  ( 6.362725135800558540, -0.7832434641057796076, 2.160938040253687742 ) ) ;
#49860 = CARTESIAN_POINT ( 'NONE',  ( 4.258551055683129860, -0.5805891344777401875, -1.768159363456432764 ) ) ;
#49859 = CARTESIAN_POINT ( 'NONE',  ( -7.391130018105325661, 8.652015104991543026, -1.199719254218452047 ) ) ;
#49861 = CARTESIAN_POINT ( 'NONE',  ( 6.550524494058025837, 7.671308660269694712, -1.199719254218452047 ) ) ;
#49862 = CARTESIAN_POINT ( 'NONE',  ( 9.030096778091543541, 1.000000000000000888, 7.742171412064401181 ) ) ;
#49863 = CARTESIAN_POINT ( 'NONE',  ( 1.492390896412032708, 7.408229809041984915, -4.235510822234025419 ) ) ;
#49864 = CARTESIAN_POINT ( 'NONE',  ( -5.205440912643032547, 8.160432600470439723, 1.199719254218452047 ) ) ;
#49865 = CARTESIAN_POINT ( 'NONE',  ( -5.017926250833627755, 5.026871178826882947, 0.7216878364870257245 ) ) ;
#49866 = CARTESIAN_POINT ( 'NONE',  ( 0.6619992422990974568, 1.085049530943157148, 1.904046507712559455 ) ) ;
#49867 = CARTESIAN_POINT ( 'NONE',  ( 4.311129659465574804, 7.013106455143060636, -1.082531754730548412 ) ) ;
#49868 = VERTEX_POINT ( 'NONE', #59723 ) ;
#49869 = CARTESIAN_POINT ( 'NONE',  ( 1.579999999999991189, 8.674529973577531194, 2.500000000000000444 ) ) ;
#49870 = CYLINDRICAL_SURFACE ( 'NONE', #165490, 1.250000000000000000 ) ;
#49872 = ADVANCED_FACE ( 'NONE', ( #125882 ), #18207, .T. ) ;
#49871 = CARTESIAN_POINT ( 'NONE',  ( 2.068725586703868746, -1.668841220716179130, -0.7407507213199536755 ) ) ;
#49873 = CARTESIAN_POINT ( 'NONE',  ( -3.249150368769345043, 6.942425863539538611, 0.7998128361456341429 ) ) ;
#49874 =( BOUNDED_CURVE ( )  B_SPLINE_CURVE ( 2, ( #137698, #107383, #187490, #56437, #152866, #138766, #40190, #170172, #73746 ),
 .UNSPECIFIED., .F., .T. ) 
 B_SPLINE_CURVE_WITH_KNOTS ( ( 3, 2, 2, 2, 3 ),
 ( 0.6339285714285713969, 0.6369047619047618625, 0.6428571428571429047, 0.6488095238095238360, 0.6517857142857143016 ),
 .UNSPECIFIED. ) 
 CURVE ( )  GEOMETRIC_REPRESENTATION_ITEM ( )  RATIONAL_B_SPLINE_CURVE ( ( 0.9330127018922194093, 0.9330127018922194093, 1.000000000000000000, 0.8660254037844387076, 1.000000000000000000, 0.8660254037844387076, 1.000000000000000000, 0.9330127018922194093, 0.9330127018922194093 ) ) 
 REPRESENTATION_ITEM ( '' )  );
#49875 = CARTESIAN_POINT ( 'NONE',  ( 3.955468362790943715, -1.619900715620861131, -0.6195580815930351593 ) ) ;
#49876 = CARTESIAN_POINT ( 'NONE',  ( -0.1074958596846934122, 2.600571376352757813, -2.078930272764640375 ) ) ;
#49877 = CARTESIAN_POINT ( 'NONE',  ( 6.609000000000012420, 2.052634316153336691, 2.306727925381938604 ) ) ;
#49878 = CARTESIAN_POINT ( 'NONE',  ( 4.151089105449103478, 2.978104760819428432, -0.7749999999999935829 ) ) ;
#49879 = CARTESIAN_POINT ( 'NONE',  ( -0.01707793031917748464, -0.1336475082493841504, -1.895772241332476682 ) ) ;
#49880 = CARTESIAN_POINT ( 'NONE',  ( 4.522284091987982535, 0.9210895807079204634, 1.732038000912524467 ) ) ;
#49881 = CARTESIAN_POINT ( 'NONE',  ( -9.176171038350775078, 9.599954387697719582, -0.7998128361456291469 ) ) ;
#49882 = CARTESIAN_POINT ( 'NONE',  ( 4.950698647284403009, 8.927565521807144577, 1.040834085586084257E-14 ) ) ;
#49883 = CARTESIAN_POINT ( 'NONE',  ( 4.881546266219149999, 0.2071824046101199135, -2.110321684233848583 ) ) ;
#49884 = CIRCLE ( 'NONE', #184681, 0.05000000000000056483 ) ;
#49885 = CARTESIAN_POINT ( 'NONE',  ( -7.147119532698295252, 11.49005655479003174, 0.000000000000000000 ) ) ;
#49886 = CARTESIAN_POINT ( 'NONE',  ( 0.07999999999999327094, -9.900000000000005684, 10.91970695577496286 ) ) ;
#49887 = CARTESIAN_POINT ( 'NONE',  ( 3.116144222688784549, 2.060704436481402890, -0.1983081510379124945 ) ) ;
#49889 = CARTESIAN_POINT ( 'NONE',  ( -1.402160292154681736E-14, -0.6156249996585817508, 1.575800808251672791 ) ) ;
#49888 = CARTESIAN_POINT ( 'NONE',  ( 4.951779652976496138, 6.537757797665411985, -2.442612065051301684 ) ) ;
#49891 = VERTEX_POINT ( 'NONE', #209153 ) ;
#49890 = PRESENTATION_LAYER_ASSIGNMENT (  '', '', ( #60243 ) ) ;
#49892 = CARTESIAN_POINT ( 'NONE',  ( 2.655266180633470086, 1.232652804806773528, 1.940110688254999438 ) ) ;
#49893 = CARTESIAN_POINT ( 'NONE',  ( 8.432808358020016826, 10.86136238915529084, 1.443375672974076540 ) ) ;
#49895 = CARTESIAN_POINT ( 'NONE',  ( 1.642778471875000035, -3.026041666188708401, -2.845375778867859751 ) ) ;
#49894 = CARTESIAN_POINT ( 'NONE',  ( 5.383996398402570271, 9.295429874862735531, 0.000000000000000000 ) ) ;
#49896 = EDGE_CURVE ( 'NONE', #184855, #38781, #80134, .T. ) ;
#49897 = CARTESIAN_POINT ( 'NONE',  ( 0.3282377607281084519, 1.676335450315393993, -1.225000000000026512 ) ) ;
#49898 = CARTESIAN_POINT ( 'NONE',  ( 1.833030277982334422, 0.000000000000000000, -2.500000000000000444 ) ) ;
#49899 = EDGE_LOOP ( 'NONE', ( #102910, #49283, #129722, #161676, #106785, #127007 ) ) ;
#49900 = CARTESIAN_POINT ( 'NONE',  ( 9.042925270190622200, 12.53353466765568669, 1.082531754730546636 ) ) ;
#49901 = ADVANCED_FACE ( 'NONE', ( #29368 ), #23906, .T. ) ;
#49902 = CARTESIAN_POINT ( 'NONE',  ( 3.990413957267644474, -1.096855775730350757, 1.566394476586838724 ) ) ;
#49903 = SURFACE_STYLE_FILL_AREA ( #129115 ) ;
#49904 = CARTESIAN_POINT ( 'NONE',  ( 4.823137214860290456, -0.08221903636504260260, 1.722948775904736385 ) ) ;
#49905 = CARTESIAN_POINT ( 'NONE',  ( 3.380092458137720968, -2.014432998692190058, -0.09411721906785883163 ) ) ;
#49906 = CARTESIAN_POINT ( 'NONE',  ( 5.221416903470996296, 2.264307454851313572, 0.3953409806420198347 ) ) ;
#49907 = CARTESIAN_POINT ( 'NONE',  ( -11.41126283316785361, 12.34125393091541056, -3.405403429622882783 ) ) ;
#49908 = CARTESIAN_POINT ( 'NONE',  ( 0.4170028235400899397, 1.518763190251697370, -1.601383572969114599 ) ) ;
#49909 = CARTESIAN_POINT ( 'NONE',  ( -3.512971199716682591, 7.112567143062499930, 0.000000000000000000 ) ) ;
#49910 = CARTESIAN_POINT ( 'NONE',  ( 6.432837487460982828, 0.1759369732093341021, 1.760927613267867953 ) ) ;
#49912 = CARTESIAN_POINT ( 'NONE',  ( 2.396762456488350956, 1.839990291603439632, -1.366890742103431755 ) ) ;
#49911 = CARTESIAN_POINT ( 'NONE',  ( 5.387385936583818591, 7.378645907471495846, -1.599625672291283607 ) ) ;
#49913 = CARTESIAN_POINT ( 'NONE',  ( 0.2689661900789627746, 0.9977586965290600185, 1.425695987021274647 ) ) ;
#49914 = CARTESIAN_POINT ( 'NONE',  ( 0.6383513625407178926, 4.335081533326786918, -0.1381026099400640694 ) ) ;
#49915 = CARTESIAN_POINT ( 'NONE',  ( 6.492125937493531396, -0.5805207454109837517, -2.113085764653479082 ) ) ;
#49916 = CARTESIAN_POINT ( 'NONE',  ( -3.142457743317409680, 6.888227477170756785, 0.7998128361456352531 ) ) ;
#49917 = CARTESIAN_POINT ( 'NONE',  ( -1.360316468750028651, -0.5781249996585913209, -4.510281037539698445E-14 ) ) ;
#49918 = CARTESIAN_POINT ( 'NONE',  ( -8.128493925383358132, 15.44816835653746345, 8.812316018300776932 ) ) ;
#49919 = CARTESIAN_POINT ( 'NONE',  ( 0.4323793472312524311, 1.250547990301904111, 1.774695861279996567 ) ) ;
#49920 = CARTESIAN_POINT ( 'NONE',  ( 1.903530124611974017, -1.954778955200174861, 0.4946342604733033887 ) ) ;
#49921 = CARTESIAN_POINT ( 'NONE',  ( -1.500000000000015099, -0.08958333265051321437, -0.8660254037844383745 ) ) ;
#49922 = CARTESIAN_POINT ( 'NONE',  ( 5.373632986646971865, 1.856140760046654403, -0.5156676092323666527 ) ) ;
#49923 = CARTESIAN_POINT ( 'NONE',  ( -0.6823417656250003738, 11.15104166700806765, 1.181850606188754593 ) ) ;
#49924 = CARTESIAN_POINT ( 'NONE',  ( 2.742673093864269163, 1.230450920196803022, -1.849320754654346866 ) ) ;
#49925 = ORIENTED_EDGE ( 'NONE', *, *, #79325, .T. ) ;
#49926 = CARTESIAN_POINT ( 'NONE',  ( 0.000000000000000000, 8.499999999999996447, 0.000000000000000000 ) ) ;
#49927 = DIRECTION ( 'NONE',  ( -0.000000000000000000, 1.000000000000000000, -0.000000000000000000 ) ) ;
#49928 = CARTESIAN_POINT ( 'NONE',  ( 9.459838494033030898, 12.05956421450382088, 1.599625672291281386 ) ) ;
#49929 = DIRECTION ( 'NONE',  ( 0.6507913734559640506, -0.7592566023653003482, 0.000000000000000000 ) ) ;
#49930 = CARTESIAN_POINT ( 'NONE',  ( 4.388070221843799246, -0.3869516340575751001, -1.696700118790330558 ) ) ;
#49931 = CARTESIAN_POINT ( 'NONE',  ( 3.648837080137564470, -0.3802854374791163616, -1.924481129451253603 ) ) ;
#49933 = CARTESIAN_POINT ( 'NONE',  ( -7.890482213473404727, 8.307910125248191946, 0.7216878364870578100 ) ) ;
#49932 = CARTESIAN_POINT ( 'NONE',  ( 4.955668840994886359, 5.740367388370866131, 1.199719254218462483 ) ) ;
#49934 =( LENGTH_UNIT ( ) NAMED_UNIT ( * ) SI_UNIT ( .MILLI., .METRE. ) );
#49935 = CARTESIAN_POINT ( 'NONE',  ( 4.587383588223284292, 2.023586100481920447, -1.011833202457941283 ) ) ;
#49936 = CARTESIAN_POINT ( 'NONE',  ( 1.398963405728241183, 0.4003750237208941742, 2.023287731994154015 ) ) ;
#49937 = CARTESIAN_POINT ( 'NONE',  ( -6.347188469492005325, 10.55680364771601809, -0.7998128361456291469 ) ) ;
#49938 = CARTESIAN_POINT ( 'NONE',  ( -3.267151830768952880, 5.795132321663641228, -1.082531754730549078 ) ) ;
#49939 = CARTESIAN_POINT ( 'NONE',  ( 0.7083710243460902278, -2.251296572208848712, 0.2248925466769024495 ) ) ;
#49940 = ORIENTED_EDGE ( 'NONE', *, *, #81974, .F. ) ;
#49941 = CARTESIAN_POINT ( 'NONE',  ( -0.7500000000000249800, -0.02708333265051543481, 1.299038105676659116 ) ) ;
#49942 = CARTESIAN_POINT ( 'NONE',  ( 2.758895227446885645, -1.625506345271657604, -0.9254698705311248386 ) ) ;
#49943 = CARTESIAN_POINT ( 'NONE',  ( 1.406441466896314996, -0.9629721463089849776, -1.441941353469172293 ) ) ;
#49944 = CARTESIAN_POINT ( 'NONE',  ( 5.284801750429747536, 1.933107837519608685, -1.032524723389722787 ) ) ;
#49945 = CARTESIAN_POINT ( 'NONE',  ( 6.247156018452869830, -1.954037266989640420, 1.227234044731172036 ) ) ;
#49946 = CARTESIAN_POINT ( 'NONE',  ( 1.692332502075646783, -2.050886281836623581, -0.2028688129896583647 ) ) ;
#49947 = CARTESIAN_POINT ( 'NONE',  ( 3.011592816664434569, -0.9578117005206161494, -1.689242170645321339 ) ) ;
#49948 = CARTESIAN_POINT ( 'NONE',  ( -4.460269348771590536, 5.266364330730674226, 1.082531754730558626 ) ) ;
#49949 = MECHANICAL_DESIGN_GEOMETRIC_PRESENTATION_REPRESENTATION (  '', ( #108926 ), #177984 ) ;
#49950 = CARTESIAN_POINT ( 'NONE',  ( 5.342975940791072631, -1.604858128155508101, 0.9606422304059699657 ) ) ;
#49951 = CARTESIAN_POINT ( 'NONE',  ( 1.531250000000001110, -0.7852924748300684765, -1.895863743164053927 ) ) ;
#49952 = CARTESIAN_POINT ( 'NONE',  ( 1.340960183756584767, 13.31717403215611739, 0.4859952365426111198 ) ) ;
#49953 = CARTESIAN_POINT ( 'NONE',  ( 6.450546045330813882, 1.388275245401158431, 1.462219883709668045 ) ) ;
#49954 = CARTESIAN_POINT ( 'NONE',  ( 3.390947817193682656, 6.009837315817661008, -1.082531754730549967 ) ) ;
#49955 = CARTESIAN_POINT ( 'NONE',  ( -3.755786496842899057E-14, 1.453125000341440876, 1.570758158831776052 ) ) ;
#49956 = CARTESIAN_POINT ( 'NONE',  ( 4.272111401563948085, 1.799923229630392640, -0.9091438646662284295 ) ) ;
#49957 = CARTESIAN_POINT ( 'NONE',  ( -10.10098813738111545, 11.74323990082152491, -1.199719254218441611 ) ) ;
#49958 = CARTESIAN_POINT ( 'NONE',  ( 6.760712154708803823, 11.03924794713562818, 1.040834085586084257E-14 ) ) ;
#49959 = CARTESIAN_POINT ( 'NONE',  ( 5.713835393516482952, 5.630839145382857680, 0.7998128361456352531 ) ) ;
#49961 = CARTESIAN_POINT ( 'NONE',  ( -4.163462365945426846, 7.871304665867801198, 0.01791990254118821721 ) ) ;
#49960 = CARTESIAN_POINT ( 'NONE',  ( 2.437895498511342574, 0.8609710149188254391, -1.609920059450341778 ) ) ;
#49962 = CYLINDRICAL_SURFACE ( 'NONE', #127152, 10.25000000000000000 ) ;
#49963 = CARTESIAN_POINT ( 'NONE',  ( -7.721398836998405457, -6.134628647623499909, -7.721398836998363713 ) ) ;
#49964 = VERTEX_POINT ( 'NONE', #17535 ) ;
#49965 = CARTESIAN_POINT ( 'NONE',  ( -5.763624699140883934, 6.857221916153382502, -1.082531754730549967 ) ) ;
#49966 = CARTESIAN_POINT ( 'NONE',  ( -1.642778471875000035, -3.405208332855375275, -2.845375778867859751 ) ) ;
#49967 = CARTESIAN_POINT ( 'NONE',  ( -8.025536864285518490, 11.45054454405341282, -1.199719254218446718 ) ) ;
#49968 = CARTESIAN_POINT ( 'NONE',  ( 0.03542360567958083295, -0.09470281839311225913, 2.017672626582614814 ) ) ;
#49969 = CARTESIAN_POINT ( 'NONE',  ( 6.340512354315207766, 1.281540423541355223, -1.814176132805396691 ) ) ;
#49970 = ORIENTED_EDGE ( 'NONE', *, *, #207366, .T. ) ;
#49971 = CARTESIAN_POINT ( 'NONE',  ( -5.803772275101700906, 8.928762199997411386, -1.199719254218452047 ) ) ;
#49972 = CARTESIAN_POINT ( 'NONE',  ( 5.691725559638619814, 5.534767995866836543, 1.040834085586084257E-14 ) ) ;
#49973 = CARTESIAN_POINT ( 'NONE',  ( 6.157116169989634180, -1.766321488544853935, -1.061543263526150138 ) ) ;
#49974 = CARTESIAN_POINT ( 'NONE',  ( 5.449842333688053486, -1.824117940560719298, -0.8596331684956671770 ) ) ;
#49975 = ORIENTED_EDGE ( 'NONE', *, *, #88237, .T. ) ;
#49976 = ORIENTED_EDGE ( 'NONE', *, *, #95699, .F. ) ;
#49977 = CARTESIAN_POINT ( 'NONE',  ( 3.615147460157889903, 7.348606074266929689, 0.4009180521483968196 ) ) ;
#49979 = EDGE_CURVE ( 'NONE', #37534, #14390, #64197, .T. ) ;
#49978 = CARTESIAN_POINT ( 'NONE',  ( -7.334597915313094241, 9.580116872663850813, 1.040834085586084257E-14 ) ) ;
#49982 = ORIENTED_EDGE ( 'NONE', *, *, #96366, .F. ) ;
#49981 = CARTESIAN_POINT ( 'NONE',  ( -1.270916165646597928, 3.166024509562812561, -0.7749999999999953593 ) ) ;
#49980 = CARTESIAN_POINT ( 'NONE',  ( -5.010620288702242853, 8.003418215864698482, -1.199719254218453823 ) ) ;
#49983 = CARTESIAN_POINT ( 'NONE',  ( 4.842126824027952026, 8.201492973507317430, 0.9351865777775794086 ) ) ;
#49984 = CARTESIAN_POINT ( 'NONE',  ( 4.938827285099913311, 1.158512636183751665, 1.649828125244500843 ) ) ;
#49985 = CARTESIAN_POINT ( 'NONE',  ( 4.365079047384805122, 1.785254547683400306, -0.4496667978745386152 ) ) ;
#49986 = CARTESIAN_POINT ( 'NONE',  ( -0.02319159430949970999, 2.891346550825595774, -2.299931007135449512 ) ) ;
#49987 = CARTESIAN_POINT ( 'NONE',  ( 2.965757426574578304, 0.3381026970978153745, -2.282680038778000853 ) ) ;
#49988 = CARTESIAN_POINT ( 'NONE',  ( 6.638652492546827766, 7.774124658506663010, 1.199719254218452047 ) ) ;
#49989 = CARTESIAN_POINT ( 'NONE',  ( 4.938837616837212785, 0.3641351946921667082, 2.130543054529559832 ) ) ;
#49990 = CARTESIAN_POINT ( 'NONE',  ( 6.096362627639171805, 10.26417349888772179, -0.7998128361456291469 ) ) ;
#49991 = CARTESIAN_POINT ( 'NONE',  ( 0.6791179963998601465, 1.305170301278056444, 1.438240348306470739 ) ) ;
#49992 = CARTESIAN_POINT ( 'NONE',  ( -4.355193658487827690, 6.104145239700998538, -1.599625672291256295 ) ) ;
#49993 = ORIENTED_EDGE ( 'NONE', *, *, #6048, .T. ) ;
#49994 = FACE_OUTER_BOUND ( 'NONE', #72789, .T. ) ;
#49995 = CARTESIAN_POINT ( 'NONE',  ( -3.806807270387036368, 7.663301925418665839, 0.000000000000000000 ) ) ;
#49996 = CARTESIAN_POINT ( 'NONE',  ( 3.449935675575486638, 1.870836310073907827, 0.001118452434160921221 ) ) ;
#49999 = CARTESIAN_POINT ( 'NONE',  ( -6.635789839245807897, 6.706452665400368218, 0.7998128361456341429 ) ) ;
#49998 = CARTESIAN_POINT ( 'NONE',  ( 0.6823417656249899377, 5.676041667008087543, -1.181850606188754593 ) ) ;
#49997 = CARTESIAN_POINT ( 'NONE',  ( 1.195406425308798148, 1.765864799226088744, -0.7346160280939582066 ) ) ;
#50000 = CARTESIAN_POINT ( 'NONE',  ( 2.684424123961434816, -1.133677649706768431, 1.893296980138805097 ) ) ;
#50001 = CARTESIAN_POINT ( 'NONE',  ( 0.07755575628184004089, 7.629137130509076492, -2.788902932953695846 ) ) ;
#50002 = CARTESIAN_POINT ( 'NONE',  ( 4.566398809704347528, 4.221886787610169556, -0.7998128361456211532 ) ) ;
#50003 = CARTESIAN_POINT ( 'NONE',  ( 6.007671464186825183, 8.102312356341712984, 1.443375672974064550 ) ) ;
#50004 = CARTESIAN_POINT ( 'NONE',  ( -2.923754682041362241, 6.562797562356882608, 0.7998128361456341429 ) ) ;
#50005 = CARTESIAN_POINT ( 'NONE',  ( -7.227905289416804102, 8.565549271475310533, -1.082531754730549967 ) ) ;
#50006 = CARTESIAN_POINT ( 'NONE',  ( 0.7726555735236986244, -1.854786837065467653, -0.6681536526091761408 ) ) ;
#50007 = CARTESIAN_POINT ( 'NONE',  ( 0.3589920806752691096, 0.8874099113769757796, 2.130322803234908857 ) ) ;
#50008 = CARTESIAN_POINT ( 'NONE',  ( 1.873419974815058842, -0.2433403713097622156, 1.946663811685337420 ) ) ;
#50009 = CARTESIAN_POINT ( 'NONE',  ( 5.418824339757763120, -1.497735668165665723, 1.418348116948890736 ) ) ;
#50010 = CARTESIAN_POINT ( 'NONE',  ( 5.233084105194869551, 6.167981546557892436, -1.082531754730548412 ) ) ;
#50011 = CARTESIAN_POINT ( 'NONE',  ( 5.180097208873055692, 8.201141289397330780, -1.199719254218450271 ) ) ;
#50012 = VERTEX_POINT ( 'NONE', #212558 ) ;
#50013 = CARTESIAN_POINT ( 'NONE',  ( 7.904040366642689719, 10.24446639921506552, 1.443375672974076540 ) ) ;
#50014 = CARTESIAN_POINT ( 'NONE',  ( 0.6823417656249899377, 4.988541667008086655, -1.181850606188754593 ) ) ;
#50015 = CARTESIAN_POINT ( 'NONE',  ( 11.81900460097218186, 12.34242865125861854, -1.592493057836596337 ) ) ;
#50016 = CARTESIAN_POINT ( 'NONE',  ( 4.324687812634887329, 6.068555086205916105, 1.443375672974062551 ) ) ;
#50017 = CARTESIAN_POINT ( 'NONE',  ( 1.024573611315128252, 1.068414711107899429, 1.889872971959544401 ) ) ;
#50019 = CARTESIAN_POINT ( 'NONE',  ( 6.269096963164666469, 1.759884223096353173, -0.5412972069449849544 ) ) ;
#50018 = CARTESIAN_POINT ( 'NONE',  ( 10.10516068267231127, -6.085430761754773599, -0.4362825330288160330 ) ) ;
#50020 = CARTESIAN_POINT ( 'NONE',  ( 11.92051736251533534, 12.44819756207319728, 1.381800029228856808 ) ) ;
#50021 = CARTESIAN_POINT ( 'NONE',  ( 1.772826578342723503, 3.950000000000526867, 0.3999999999999847566 ) ) ;
#50022 = CARTESIAN_POINT ( 'NONE',  ( 1.510794437334112672, 1.647127454408814362, 0.8865631655482277829 ) ) ;
#50023 = CARTESIAN_POINT ( 'NONE',  ( 5.852838158510675015, -1.708014377640250991, 1.324763891615586386 ) ) ;
#50025 = EDGE_CURVE ( 'NONE', #104947, #144257, #201175, .T. ) ;
#50024 = CARTESIAN_POINT ( 'NONE',  ( -6.126391799051042142, 6.003160260013642890, 0.2011063304240209848 ) ) ;
#50026 = CARTESIAN_POINT ( 'NONE',  ( -0.02264175331115856477, -0.002534049983802035520, -2.089079740194145440 ) ) ;
#50027 = CARTESIAN_POINT ( 'NONE',  ( 6.454497976780569246, 6.866128686250288382, -0.6735470152485992790 ) ) ;
#50028 = CARTESIAN_POINT ( 'NONE',  ( 1.364683531249988535, 5.217708333674750065, -0.7879004041258300672 ) ) ;
#50029 = CARTESIAN_POINT ( 'NONE',  ( 1.576665144504853400, -1.351504567317940664, 1.353124384123285839 ) ) ;
#50030 = CARTESIAN_POINT ( 'NONE',  ( 2.940057854958120220, 1.756256042272446694, 0.2183286820098342407 ) ) ;
#50031 = CARTESIAN_POINT ( 'NONE',  ( 1.066890508724306130, -1.507026839618429426, 1.177014404800474479 ) ) ;
#50033 = CARTESIAN_POINT ( 'NONE',  ( 6.028903631427566800, -1.615475894945080926, 1.029159534634891626 ) ) ;
#50032 = DIRECTION ( 'NONE',  ( -0.6123724356957922499, 0.7071067811865537900, -0.3535533905932651266 ) ) ;
#50034 = CARTESIAN_POINT ( 'NONE',  ( -1.500000000000001332, -0.8499999999999757749, 0.000000000000000000 ) ) ;
#50035 = CARTESIAN_POINT ( 'NONE',  ( 6.180130249528606790, -1.092802789126966934, -1.638350696670291651 ) ) ;
#50036 = CARTESIAN_POINT ( 'NONE',  ( 0.7499999999999920064, 4.233333333333352932, 1.299038105676669330 ) ) ;
#50038 = EDGE_CURVE ( 'NONE', #35460, #72572, #122072, .T. ) ;
#50037 = CARTESIAN_POINT ( 'NONE',  ( 1.529697670087664108, -0.2543295609688834835, 2.105205558366497698 ) ) ;
#50039 = FACE_OUTER_BOUND ( 'NONE', #21725, .T. ) ;
#50040 = CARTESIAN_POINT ( 'NONE',  ( 4.451927283622527654, 1.870250842541102410, -0.04591718433973044494 ) ) ;
#50042 = ORIENTED_EDGE ( 'NONE', *, *, #111757, .F. ) ;
#50041 = CARTESIAN_POINT ( 'NONE',  ( 0.4514209555319322331, 0.5758240286459560542, -1.732582669633643047 ) ) ;
#50044 = CARTESIAN_POINT ( 'NONE',  ( 4.893454165248502186, 8.027304163657891678, -0.9628252682179049282 ) ) ;
#50043 = CARTESIAN_POINT ( 'NONE',  ( 3.088704478669739295, -2.174299887604825177, -0.3769171259565203269 ) ) ;
#50045 = CARTESIAN_POINT ( 'NONE',  ( -1.001543065824772872E-14, 4.384375000341417916, 1.575800808251672791 ) ) ;
#50046 = CARTESIAN_POINT ( 'NONE',  ( 1.539586554034046539, 1.906627302964102988, -0.7874849336161419133 ) ) ;
#50048 = EDGE_CURVE ( 'NONE', #59479, #130487, #208150, .T. ) ;
#50047 = CARTESIAN_POINT ( 'NONE',  ( 5.449487677688982679, 8.445153826357429949, -1.199719254218446718 ) ) ;
#50050 = CARTESIAN_POINT ( 'NONE',  ( -9.664264568442742842, 10.16939683947169115, -0.7998128361456291469 ) ) ;
#50049 = AXIS2_PLACEMENT_3D ( 'NONE', #157499, #45888, #92515 ) ;
#50051 = CARTESIAN_POINT ( 'NONE',  ( 6.938893903907228378E-15, 10.64264068711930733, 1.214306433183764966E-14 ) ) ;
#50052 = CARTESIAN_POINT ( 'NONE',  ( 11.86145017031113902, 11.00581953513848354, -1.100000000000000533 ) ) ;
#50053 = CARTESIAN_POINT ( 'NONE',  ( 7.506374323821472849, 8.786466794993730289, -1.199719254218452047 ) ) ;
#50054 = VERTEX_POINT ( 'NONE', #180078 ) ;
#50055 = CARTESIAN_POINT ( 'NONE',  ( 4.756339170418532269, -2.069830778647030023, -0.05414847147890837487 ) ) ;
#50057 = CARTESIAN_POINT ( 'NONE',  ( -0.7500000000000215383, 5.691666666666685082, 1.299038105676671107 ) ) ;
#50056 =( GEOMETRIC_REPRESENTATION_CONTEXT ( 3 ) GLOBAL_UNCERTAINTY_ASSIGNED_CONTEXT ( ( #662 ) ) GLOBAL_UNIT_ASSIGNED_CONTEXT ( ( #182215, #181158, #154005 ) ) REPRESENTATION_CONTEXT ( 'NONE', 'WORKASPACE' ) );
#50058 = CARTESIAN_POINT ( 'NONE',  ( 1.687033600898584895, -0.3153356727807927751, -2.138329785107299319 ) ) ;
#50059 = CARTESIAN_POINT ( 'NONE',  ( -5.622963654236769138, 7.379252650573795869, -1.237363127855268141 ) ) ;
#50060 = CARTESIAN_POINT ( 'NONE',  ( 2.174478703267632707, 0.8655064541149575241, 1.824978016274068082 ) ) ;
#50061 = CARTESIAN_POINT ( 'NONE',  ( 5.802526556524483681, 5.871961858807763335, 1.040834085586084257E-14 ) ) ;
#50062 = ORIENTED_EDGE ( 'NONE', *, *, #186853, .T. ) ;
#50064 = CARTESIAN_POINT ( 'NONE',  ( 6.941411460516762943, 11.04213777067082702, -0.7216878364870267237 ) ) ;
#50063 = CARTESIAN_POINT ( 'NONE',  ( 1.001543065824772753E-15, -3.062499999999998668, 4.012584370867899430 ) ) ;
#50065 = CARTESIAN_POINT ( 'NONE',  ( 1.836970198721030181E-16, 13.49999999999999822, 1.500000000000000222 ) ) ;
#50066 = CARTESIAN_POINT ( 'NONE',  ( -0.2409995289980038091, -0.004801160710915519658, -2.000252362011435636 ) ) ;
#50067 = CARTESIAN_POINT ( 'NONE',  ( 6.639320575229257670, 2.957073754255258535, 2.555924021811271096 ) ) ;
#50068 = CARTESIAN_POINT ( 'NONE',  ( 5.073855206572205567, -1.217758175834412260, 1.821886007100224969 ) ) ;
#50069 =( BOUNDED_CURVE ( )  B_SPLINE_CURVE ( 2, ( #106534, #205025, #89186, #173648, #124953, #25222, #157385 ),
 .UNSPECIFIED., .F., .T. ) 
 B_SPLINE_CURVE_WITH_KNOTS ( ( 3, 2, 2, 3 ),
 ( 0.2321428571428570953, 0.2380952380952381098, 0.2440476190476191798, 0.2500000000000002220 ),
 .UNSPECIFIED. ) 
 CURVE ( )  GEOMETRIC_REPRESENTATION_ITEM ( )  RATIONAL_B_SPLINE_CURVE ( ( 1.000000000000001332, 0.8660254037844374864, 1.000000000000000000, 0.8660254037844387076, 1.000000000000000000, 0.8660254037844337116, 1.000000000000005107 ) ) 
 REPRESENTATION_ITEM ( '' )  );
#50070 = CIRCLE ( 'NONE', #105443, 2.000000000000000000 ) ;
#50071 = CARTESIAN_POINT ( 'NONE',  ( -0.7499999999999972244, 3.639583334016149863, -1.299038105676652011 ) ) ;
#50072 = CARTESIAN_POINT ( 'NONE',  ( 3.586107075002854305, 1.066394011600999780, 1.587261316105821551 ) ) ;
#50073 = CARTESIAN_POINT ( 'NONE',  ( -4.120788623549732854, 6.895004929861607401, -1.199719254218452047 ) ) ;
#50074 = CARTESIAN_POINT ( 'NONE',  ( 4.650083499362880346, 4.527444958785877382, 0.7216878364870317197 ) ) ;
#50076 = CARTESIAN_POINT ( 'NONE',  ( 2.038685622454153190, -1.556895902704044765, 1.281378572682637218 ) ) ;
#50075 = CARTESIAN_POINT ( 'NONE',  ( -9.612367721964606204, 12.23751498042398289, -1.443375672974058777 ) ) ;
#50077 = CARTESIAN_POINT ( 'NONE',  ( -1.364683531250010295, 12.94270833367473550, 0.7879004041258445001 ) ) ;
#50079 = CARTESIAN_POINT ( 'NONE',  ( -4.145761110728687804, 8.058748072483927771, -0.7998128361456481317 ) ) ;
#50078 = CARTESIAN_POINT ( 'NONE',  ( 0.8555022099123296142, 0.4403784002881392379, -2.249529875239093979 ) ) ;
#50080 = CARTESIAN_POINT ( 'NONE',  ( 3.715580044805122384, -1.699234090967314259, 0.2946211727567394911 ) ) ;
#50081 = CARTESIAN_POINT ( 'NONE',  ( 5.989670002187236442, 10.20997511251894529, -0.7998128361456481317 ) ) ;
#50082 = CARTESIAN_POINT ( 'NONE',  ( 4.630273154266905777, 5.360739087188218122, 1.199719254218464037 ) ) ;
#50083 = CARTESIAN_POINT ( 'NONE',  ( -1.284279953904132077, 2.909610286488902187, -0.7749999999999935829 ) ) ;
#50084 = CARTESIAN_POINT ( 'NONE',  ( 0.7132427667453158371, -1.655377960257615966, -1.052639099659122390 ) ) ;
#50085 = CARTESIAN_POINT ( 'NONE',  ( 0.2505829665140328899, -1.505242420826727656, 1.110479572284161831 ) ) ;
#50086 = CARTESIAN_POINT ( 'NONE',  ( 0.1751657365761885576, 5.722053558346082092, -2.638081460773045617 ) ) ;
#50087 = VERTEX_POINT ( 'NONE', #150785 ) ;
#50088 = FACE_OUTER_BOUND ( 'NONE', #117600, .T. ) ;
#50089 = VERTEX_POINT ( 'NONE', #147584 ) ;
#50090 = CARTESIAN_POINT ( 'NONE',  ( 4.951724851890283219, -1.284874556838147219, -1.277195305962516292 ) ) ;
#50091 = AXIS2_PLACEMENT_3D ( 'NONE', #151568, #69205, #135325 ) ;
#50092 = ORIENTED_EDGE ( 'NONE', *, *, #95039, .T. ) ;
#50093 = CARTESIAN_POINT ( 'NONE',  ( 6.017840079619279692, 8.114175741012878973, -1.599625672291281386 ) ) ;
#50094 = DIRECTION ( 'NONE',  ( 0.000000000000000000, 1.000000000000000000, 0.000000000000000000 ) ) ;
#50095 = CARTESIAN_POINT ( 'NONE',  ( 5.742768220754598474, 1.747532268389985433, 0.4768009125176131957 ) ) ;
#50096 = CARTESIAN_POINT ( 'NONE',  ( 7.336370518326124746, 7.731722824234849689, -0.7216878364870317197 ) ) ;
#50097 = CARTESIAN_POINT ( 'NONE',  ( 2.280903940472752467, 5.594607745005274246, -0.6109567437776646237 ) ) ;
#50098 = CARTESIAN_POINT ( 'NONE',  ( 5.718470792885002041, 6.083800970187063228, -0.6820517675651931455 ) ) ;
#50100 = CARTESIAN_POINT ( 'NONE',  ( 10.56588178375152864, 11.22128359066528169, -0.7998128361456281477 ) ) ;
#50099 = CARTESIAN_POINT ( 'NONE',  ( 6.162542460989155479, -0.6707643300355231597, -1.736165932305182125 ) ) ;
#50101 = CARTESIAN_POINT ( 'NONE',  ( 4.183139505431884508, 1.540756628010631735, 1.138051695910688998 ) ) ;
#50102 = CARTESIAN_POINT ( 'NONE',  ( -6.381095703207960490, -8.200000000000001066, -7.037870247915966715 ) ) ;
#50103 = MECHANICAL_DESIGN_GEOMETRIC_PRESENTATION_REPRESENTATION (  '', ( #133150 ), #15442 ) ;
#50104 = CARTESIAN_POINT ( 'NONE',  ( 11.48243876534946217, 13.79999999999998295, 3.199999999999997957 ) ) ;
#50105 = CARTESIAN_POINT ( 'NONE',  ( 6.317736394288140822, 7.433409217166723870, 1.082531754730558626 ) ) ;
#50107 = CARTESIAN_POINT ( 'NONE',  ( 5.753141757616087482, 0.1533694674813860792, -2.111807561841658742 ) ) ;
#50106 = CARTESIAN_POINT ( 'NONE',  ( -2.103486388414573138, 5.605817886458954291, 1.040834085586084257E-14 ) ) ;
#50108 = CARTESIAN_POINT ( 'NONE',  ( 0.9366540776252419986, 2.129889809250965271, 0.3686189752144660159 ) ) ;
#50109 = CARTESIAN_POINT ( 'NONE',  ( -6.798487682609798632, 6.896266815991691779, 0.7998128361456341429 ) ) ;
#50110 = VECTOR ( 'NONE', #73566, 1000.000000000000000 ) ;
#50111 = CARTESIAN_POINT ( 'NONE',  ( 3.718679271898170491, 7.560485927181699317, 0.7998128361456271485 ) ) ;
#50112 = CARTESIAN_POINT ( 'NONE',  ( 0.6744773098602949712, -1.717252091951677384, -0.6198786263262797691 ) ) ;
#50113 = CARTESIAN_POINT ( 'NONE',  ( -5.278201874421821316, 5.052323696447222900, 0.7998128361456341429 ) ) ;
#50114 = CARTESIAN_POINT ( 'NONE',  ( 3.944226942909400346, 1.816763600636053688, 0.1792749827478901103 ) ) ;
#50115 = EDGE_CURVE ( 'NONE', #136751, #80820, #49080, .T. ) ;
#50116 = CARTESIAN_POINT ( 'NONE',  ( 9.295773149506796784, 12.92845620919447036, 8.961466013164043787 ) ) ;
#50117 = ORIENTED_EDGE ( 'NONE', *, *, #77763, .F. ) ;
#50118 = CARTESIAN_POINT ( 'NONE',  ( 2.734760313433327372, -1.883857982319175450, -0.5745676990022812181 ) ) ;
#50119 = CARTESIAN_POINT ( 'NONE',  ( 4.687022505062548916, 1.441580155910677785, 1.301524815871560214 ) ) ;
#50120 = CARTESIAN_POINT ( 'NONE',  ( -2.993318053567081360, 6.714231172462041819, 0.000000000000000000 ) ) ;
#50122 = CARTESIAN_POINT ( 'NONE',  ( 4.904590598983499916, -2.104870323260544129, -0.2570220051709286579 ) ) ;
#50121 = CARTESIAN_POINT ( 'NONE',  ( 7.205232291019763480, 7.370802192470005565, -0.7998128361456341429 ) ) ;
#50123 = CARTESIAN_POINT ( 'NONE',  ( -5.763039058787290614, 7.049721345481786194, -2.500000000000000000 ) ) ;
#50124 = CARTESIAN_POINT ( 'NONE',  ( 2.684119430630255820, 1.024705199231435993, 1.614373862881289590 ) ) ;
#50125 = CARTESIAN_POINT ( 'NONE',  ( 6.115260013507548109, 6.015528159276049891, -0.005231617032384894284 ) ) ;
#50126 = CARTESIAN_POINT ( 'NONE',  ( 0.000000000000000000, 4.518467169708412889, 0.000000000000000000 ) ) ;
#50127 = CARTESIAN_POINT ( 'NONE',  ( 0.6823417656249934904, 12.69270833367473017, 1.181850606188764807 ) ) ;
#50128 = CARTESIAN_POINT ( 'NONE',  ( 4.366607992053101128, 7.252070536440704096, -1.199719254218448494 ) ) ;
#50129 = CARTESIAN_POINT ( 'NONE',  ( 4.497554271431305040, 6.270232621468402989, -1.599625672291256295 ) ) ;
#50130 = CARTESIAN_POINT ( 'NONE',  ( 0.09264309395030836947, -9.919020119916163836, 9.499548513212900502 ) ) ;
#50131 = CARTESIAN_POINT ( 'NONE',  ( 5.074738461036464088, -1.720261882950037124, -0.6118011564382742629 ) ) ;
#50132 = CARTESIAN_POINT ( 'NONE',  ( 1.154700538379228147, -2.500000000000002220, -1.734723475976807094E-15 ) ) ;
#50133 = CARTESIAN_POINT ( 'NONE',  ( -9.192064960385334160, 9.826423329978791088, 0.7216878364870438212 ) ) ;
#50134 = CARTESIAN_POINT ( 'NONE',  ( -6.606716786301501720, 6.763562328987043237, 0.1806677948501221598 ) ) ;
#50135 = CARTESIAN_POINT ( 'NONE',  ( 5.858239598252557911, 0.7595784280203803362, 1.709674162104061645 ) ) ;
#50136 = CARTESIAN_POINT ( 'NONE',  ( 8.101160479365381306, 9.410107633136481908, -1.199719254218446718 ) ) ;
#50137 = CARTESIAN_POINT ( 'NONE',  ( -4.086893239515592136, 6.855460315155083251, 1.199719254218464037 ) ) ;
#50138 = B_SPLINE_CURVE_WITH_KNOTS ( 'NONE', 3,
 ( #206693, #58321, #92976, #208810 ),
 .UNSPECIFIED., .F., .F.,
 ( 4, 4 ),
 ( 0.000000000000000000, 6.033646489354581229E-05 ),
 .UNSPECIFIED. ) ;
#50139 = CARTESIAN_POINT ( 'NONE',  ( 0.6823417656249969321, 10.58854166700806587, -1.181850606188757036 ) ) ;
#50140 = CARTESIAN_POINT ( 'NONE',  ( -6.573005544526917099, 6.562927978236513304, -0.7998128361456291469 ) ) ;
#50141 = CARTESIAN_POINT ( 'NONE',  ( 2.737856954955798727, 5.281584649835344258, 1.199719254218452047 ) ) ;
#50142 = CARTESIAN_POINT ( 'NONE',  ( -6.420668264523499147, 9.648474187656182366, 1.199719254218452935 ) ) ;
#50143 = CARTESIAN_POINT ( 'NONE',  ( -5.880485940025243607, 7.883652901494672349, 1.599625672291269396 ) ) ;
#50144 = CARTESIAN_POINT ( 'NONE',  ( 6.508646264616319677, 0.6728166153291449403, 2.064291235436790384 ) ) ;
#50145 = CARTESIAN_POINT ( 'NONE',  ( 2.759486767256282391, 2.009531813720342175, -0.6668115938158604150 ) ) ;
#50146 = CARTESIAN_POINT ( 'NONE',  ( 7.730120138085914583, 12.17022392774227768, 0.7998128361456462443 ) ) ;
#50147 = CARTESIAN_POINT ( 'NONE',  ( -7.013428937081410020, 5.939655416065873439, 2.436399677959149024 ) ) ;
#50148 = CARTESIAN_POINT ( 'NONE',  ( 6.139524545372063713, 1.915082402702467101, -0.7868883245659707981 ) ) ;
#50149 = CARTESIAN_POINT ( 'NONE',  ( 4.075930520424391190, 7.726065465775651120, -0.5982635945973235891 ) ) ;
#50150 = CARTESIAN_POINT ( 'NONE',  ( 5.585596099150174965, 7.539614753807099667, -1.443375672974057666 ) ) ;
#50152 =( LENGTH_UNIT ( ) NAMED_UNIT ( * ) SI_UNIT ( .MILLI., .METRE. ) );
#50151 = CARTESIAN_POINT ( 'NONE',  ( 11.33772463945036790, 10.19999999999999929, -3.600000000000000977 ) ) ;
#50153 = CARTESIAN_POINT ( 'NONE',  ( 2.994356955963250133, -0.6658908676899841783, -2.193406925754942893 ) ) ;
#50156 = EDGE_CURVE ( 'NONE', #8487, #96867, #182183, .T. ) ;
#50155 = CARTESIAN_POINT ( 'NONE',  ( 0.2333690889706925564, 2.018283468528142777, -2.468684669820114586 ) ) ;
#50154 = CARTESIAN_POINT ( 'NONE',  ( -5.765600714192440357, 7.067438534623913249, 2.440103264412582185 ) ) ;
#50157 = CARTESIAN_POINT ( 'NONE',  ( 2.285291272251275707, 0.09004542135446562401, -1.910373438827176251 ) ) ;
#50158 = VERTEX_POINT ( 'NONE', #165951 ) ;
#50159 = CARTESIAN_POINT ( 'NONE',  ( 6.548225005276093746, 9.623051025255367819, -1.082531754730537976 ) ) ;
#50160 = ADVANCED_FACE ( 'NONE', ( #149707 ), #200555, .T. ) ;
#50161 = CARTESIAN_POINT ( 'NONE',  ( 1.054940647564650336, 0.3968280277809080880, 1.973547778087578308 ) ) ;
#50162 = CARTESIAN_POINT ( 'NONE',  ( 0.7429250141685154185, -0.2344385519315282107, -1.947609053799495005 ) ) ;
#50163 = CARTESIAN_POINT ( 'NONE',  ( 4.322138105957547438, 3.567377917394175313, -2.444429911049615711 ) ) ;
#50164 = CARTESIAN_POINT ( 'NONE',  ( -6.692921386640485082, 10.96015871772258521, -0.7998128361456291469 ) ) ;
#50165 = DIRECTION ( 'NONE',  ( -2.498001805406606160E-16, 0.8656921114426522346, -0.5005768354468299597 ) ) ;
#50167 = CARTESIAN_POINT ( 'NONE',  ( 2.447821898584545242, 1.769419436591600725, 0.04612135499031978086 ) ) ;
#50166 = CARTESIAN_POINT ( 'NONE',  ( 4.013684974745008738, -1.074646439955847965, -1.793145193944564175 ) ) ;
#50168 = CARTESIAN_POINT ( 'NONE',  ( 0.000000000000000000, 15.44736672593543148, 0.000000000000000000 ) ) ;
#50169 = B_SPLINE_CURVE_WITH_KNOTS ( 'NONE', 3,
 ( #66970, #166642, #133109, #84317, #50751, #153168 ),
 .UNSPECIFIED., .F., .F.,
 ( 4, 2, 4 ),
 ( 0.000000000000000000, 0.0003202493251089926678, 0.0006404986502179853356 ),
 .UNSPECIFIED. ) ;
#50171 = CARTESIAN_POINT ( 'NONE',  ( 5.595737365542901465, -2.292435212557204949, -0.004933362929348399616 ) ) ;
#50170 = LINE ( 'NONE', #32851, #48728 ) ;
#50172 = CARTESIAN_POINT ( 'NONE',  ( 2.800428594868603405, 1.470281860783069439, 0.9307988129052218174 ) ) ;
#50173 = CARTESIAN_POINT ( 'NONE',  ( 8.866142388332804103, 12.43125098877526113, -1.199719254218446718 ) ) ;
#50174 = CARTESIAN_POINT ( 'NONE',  ( 3.725458348705031231, 7.568394850123006279, -1.734723475976807094E-15 ) ) ;
#50175 = CARTESIAN_POINT ( 'NONE',  ( 3.303724397909554078, -1.530444925530007216, 0.8147494179842218465 ) ) ;
#50176 = CARTESIAN_POINT ( 'NONE',  ( 4.000555764329702946, 2.160365084594504381, 0.2165898760093481201 ) ) ;
#50177 = CARTESIAN_POINT ( 'NONE',  ( 5.495132332240461714, 5.305409230568988832, 0.7998128361456341429 ) ) ;
#50178 = CARTESIAN_POINT ( 'NONE',  ( 5.190638768449240992, 1.523797776992100284, -1.320824044268428255 ) ) ;
#50179 = CARTESIAN_POINT ( 'NONE',  ( 6.687508294236179651, -1.450827213159664675, 1.451031289061379681 ) ) ;
#50180 = CARTESIAN_POINT ( 'NONE',  ( 0.7499999999999902300, 3.597916667349487785, -1.299038105676658228 ) ) ;
#50181 = CARTESIAN_POINT ( 'NONE',  ( 2.520427876150105995, 1.259661825572227167, -1.457548065151576200 ) ) ;
#50182 = CARTESIAN_POINT ( 'NONE',  ( -1.364683531250010295, 15.13020833367473017, 0.7879004041258445001 ) ) ;
#50183 = CARTESIAN_POINT ( 'NONE',  ( 5.695613681701293451, 2.052597959444299125, -0.8498680618601384129 ) ) ;
#50184 = ORIENTED_EDGE ( 'NONE', *, *, #140381, .T. ) ;
#50185 = CARTESIAN_POINT ( 'NONE',  ( 6.983263157960370116, 6.036630394911544073, 2.541087343977180613 ) ) ;
#50186 = CARTESIAN_POINT ( 'NONE',  ( -1.499999999999997780, 2.400000000000020339, 1.214306433183764966E-14 ) ) ;
#50187 = CARTESIAN_POINT ( 'NONE',  ( 5.764187864104357573, 9.876636274763768597, 1.040834085586084257E-14 ) ) ;
#50188 = CARTESIAN_POINT ( 'NONE',  ( 5.138177029454847222, 6.057256624861201644, 1.082531754730560403 ) ) ;
#50189 = CARTESIAN_POINT ( 'NONE',  ( 1.928696271399105600, -1.050554081124959183, -1.957186058178138399 ) ) ;
#50190 = CARTESIAN_POINT ( 'NONE',  ( -1.201851678989727383E-14, 4.837500000000018119, -1.732050807568863648 ) ) ;
#50191 = CARTESIAN_POINT ( 'NONE',  ( 6.954969614130424027, 11.05795561655343384, 1.040834085586084257E-14 ) ) ;
#50192 = SURFACE_STYLE_FILL_AREA ( #68543 ) ;
#50193 = AXIS2_PLACEMENT_3D ( 'NONE', #172162, #91995, #59462 ) ;
#50194 = EDGE_CURVE ( 'NONE', #186645, #127188, #151091, .T. ) ;
#50195 = CARTESIAN_POINT ( 'NONE',  ( 5.713835393516482952, 5.630839145382857680, 0.7998128361456352531 ) ) ;
#50196 = CARTESIAN_POINT ( 'NONE',  ( -3.689227196694346400, 6.357829925235092716, -1.082531754730546636 ) ) ;
#50197 = CARTESIAN_POINT ( 'NONE',  ( 4.088373676034792403, 1.106037789618707912, -1.740905279395239758 ) ) ;
#50198 = CARTESIAN_POINT ( 'NONE',  ( -5.603597561149804562, 5.431951997629870910, 0.7998128361456341429 ) ) ;
#50199 = PRESENTATION_LAYER_ASSIGNMENT (  '', '', ( #81279 ) ) ;
#50200 = CARTESIAN_POINT ( 'NONE',  ( -1.499999999999997780, 3.931250000682819046, 1.214306433183764966E-14 ) ) ;
#50201 = CARTESIAN_POINT ( 'NONE',  ( -1.402160292154681736E-14, -0.8031249996585825279, -1.575800808251665908 ) ) ;
#50202 = CARTESIAN_POINT ( 'NONE',  ( 6.081297793977560318, 1.728434112010367674, -0.7156336962577531935 ) ) ;
#50203 = CARTESIAN_POINT ( 'NONE',  ( 4.394945383863869459, -0.7467295182301251222, -1.565304230221546300 ) ) ;
#50204 = CARTESIAN_POINT ( 'NONE',  ( 4.915436192723389830, -0.9368120511010556983, -1.466610992562596527 ) ) ;
#50205 = CARTESIAN_POINT ( 'NONE',  ( 3.876741858503734761, 6.610283703974623393, 1.199719254218462483 ) ) ;
#50206 = CARTESIAN_POINT ( 'NONE',  ( 1.769451523944377769, 2.192225184321832554, -0.6701302238534474487 ) ) ;
#50207 = CARTESIAN_POINT ( 'NONE',  ( -1.201851678989727383E-14, 5.259375000341421469, -1.575800808251660134 ) ) ;
#50208 = CARTESIAN_POINT ( 'NONE',  ( 5.970280646434825478, -1.985518398909513982, -0.6551979098984096472 ) ) ;
#50209 = CARTESIAN_POINT ( 'NONE',  ( 0.6207436649305307919, -1.749090901066195691, 0.5750481222980761142 ) ) ;
#50210 = CARTESIAN_POINT ( 'NONE',  ( -0.3000000000000322409, 3.975028841772310084, 0.9637995837462181026 ) ) ;
#50211 =( NAMED_UNIT ( * ) SI_UNIT ( $, .STERADIAN. ) SOLID_ANGLE_UNIT ( ) );
#50212 = CARTESIAN_POINT ( 'NONE',  ( 1.670546294658280084, 1.392546765991018454, 1.458555661489918442 ) ) ;
#50213 = CARTESIAN_POINT ( 'NONE',  ( 0.6038064816080711550, -2.180521553291506986, 0.2185767975278959385 ) ) ;
#50214 = DIRECTION ( 'NONE',  ( 5.551115123125765446E-17, 0.000000000000000000, -1.000000000000000000 ) ) ;
#50215 = CARTESIAN_POINT ( 'NONE',  ( -8.050844288416501016, 8.287073179441051707, 1.040834085586084257E-14 ) ) ;
#50216 = CARTESIAN_POINT ( 'NONE',  ( 5.168682875307768931, 7.053215992657626110, -1.599625672291256295 ) ) ;
#50217 = CARTESIAN_POINT ( 'NONE',  ( -3.555477883677943599E-14, 1.578125000341449535, -1.570758158831814466 ) ) ;
#50218 = CARTESIAN_POINT ( 'NONE',  ( 3.739029402251158984, 2.014021593674422572, 0.6637135986873595739 ) ) ;
#50219 = CARTESIAN_POINT ( 'NONE',  ( -1.364683531250000748, -0.2406249996585799189, 0.000000000000000000 ) ) ;
#50220 = CARTESIAN_POINT ( 'NONE',  ( 5.883392091387671385, 1.685093539698417242, -0.7030590484573000509 ) ) ;
#50221 = CARTESIAN_POINT ( 'NONE',  ( -6.444921918449773024, 8.612437886315108315, 1.599625672291269396 ) ) ;
#50222 = DIRECTION ( 'NONE',  ( 0.000000000000000000, 0.000000000000000000, 1.000000000000000000 ) ) ;
#50223 = CARTESIAN_POINT ( 'NONE',  ( 5.668717623845194176, 9.627604637879139560, 0.000000000000000000 ) ) ;
#50224 = CARTESIAN_POINT ( 'NONE',  ( 1.737500000000001155, -3.689583332377416980, 3.009438278150922130 ) ) ;
#50225 = CARTESIAN_POINT ( 'NONE',  ( -6.287230548435221777, 8.358188277972981695, -1.599625672291263179 ) ) ;
#50226 = CARTESIAN_POINT ( 'NONE',  ( 3.322525440707891242, -0.8223705904544276191, -1.844992516297422780 ) ) ;
#50227 = CARTESIAN_POINT ( 'NONE',  ( 0.3937647135470741522, 1.560644430845319119, 1.414193795423605904 ) ) ;
#50228 = CARTESIAN_POINT ( 'NONE',  ( 8.055515824813896941, 12.54985222892493368, 0.7998128361456462443 ) ) ;
#50229 = CARTESIAN_POINT ( 'NONE',  ( 4.838624485402447384, -1.804320056961044694, -0.4549315660777561443 ) ) ;
#50230 = CARTESIAN_POINT ( 'NONE',  ( 9.915090410295563927, 10.46202698829998567, -0.7998128361456281477 ) ) ;
#50231 = CARTESIAN_POINT ( 'NONE',  ( -4.848826244296223109, 5.027555131033083491, -0.8732430475888955934 ) ) ;
#50232 = CARTESIAN_POINT ( 'NONE',  ( -4.762992037102518950, 4.451245552908022596, -0.7998128361456221525 ) ) ;
#50233 = CARTESIAN_POINT ( 'NONE',  ( -8.345207244411405156, 9.694828859023472134, 1.199719254218462483 ) ) ;
#50234 = CARTESIAN_POINT ( 'NONE',  ( 0.1632417891470130944, -1.931755829615459996, -0.9703963252955111196 ) ) ;
#50235 = CIRCLE ( 'NONE', #8622, 0.07999999999999997391 ) ;
#50237 = CARTESIAN_POINT ( 'NONE',  ( -4.762889583212370326, 6.995502248939536649, 1.426468515190159714 ) ) ;
#50236 = CARTESIAN_POINT ( 'NONE',  ( -6.505933609711270549, 8.683618192786854095, -1.599625672291271394 ) ) ;
#50238 = CARTESIAN_POINT ( 'NONE',  ( 0.6823417656249882723, -0.07395833299191079124, -1.181850606188749264 ) ) ;
#50239 = CARTESIAN_POINT ( 'NONE',  ( 1.721629994271107744, -1.484111423267266527, -0.8961763045370867431 ) ) ;
#50240 = CARTESIAN_POINT ( 'NONE',  ( 0.7259949354544228406, 0.1236639744153274628, 1.736007293746767655 ) ) ;
#50242 = CARTESIAN_POINT ( 'NONE',  ( 9.246297574839983824, 9.889694713509232571, 0.7216878364870438212 ) ) ;
#50241 = CARTESIAN_POINT ( 'NONE',  ( 6.498638929175646339, -0.6082784835782985011, -2.226023345802934372 ) ) ;
#50243 = CARTESIAN_POINT ( 'NONE',  ( 3.444653546323793947, 6.176457016423196222, 1.199719254218451159 ) ) ;
#50244 = CARTESIAN_POINT ( 'NONE',  ( 2.759116376063870391, -1.791426917979478395, -1.018529149919424892 ) ) ;
#50245 = CARTESIAN_POINT ( 'NONE',  ( 6.017121246366603060, 5.914396297049491658, 1.040834085586084257E-14 ) ) ;
#50246 = CARTESIAN_POINT ( 'NONE',  ( 1.054064285791616262, 1.779355684154381834, -0.9478921834336280217 ) ) ;
#50247 = CARTESIAN_POINT ( 'NONE',  ( -0.08058608058609216529, -9.900000000000005684, -10.99970480893080271 ) ) ;
#50248 = CARTESIAN_POINT ( 'NONE',  ( -4.960304097753355457, 6.880383762169266504, 1.599625672291263179 ) ) ;
#50249 = CARTESIAN_POINT ( 'NONE',  ( 0.3035114269093022732, -0.5280327476409033549, 1.899365994968700955 ) ) ;
#50250 = COLOUR_RGB ( '', 0.72549020, 0.75294118, 0.79215686) ;
#50251 = B_SPLINE_CURVE_WITH_KNOTS ( 'NONE', 3,
 ( #164965, #182267, #198509, #69570, #97857, #149794, #98913, #19767, #16557, #163920 ),
 .UNSPECIFIED., .F., .F.,
 ( 4, 2, 2, 2, 4 ),
 ( 0.000000000000000000, 0.0002554020510936943849, 0.0005108041021873887698, 0.0007662061532810831004, 0.001021608204374777540 ),
 .UNSPECIFIED. ) ;
#50253 = CARTESIAN_POINT ( 'NONE',  ( -6.455090533882201775, 8.624301270986276080, -1.443375672974066548 ) ) ;
#50252 = CARTESIAN_POINT ( 'NONE',  ( 4.781465250580236415, 0.1816826923375300662, -1.903719681147630016 ) ) ;
#50254 = CARTESIAN_POINT ( 'NONE',  ( 6.691986956589398794, -0.9478133180038283978, 1.990996264204819122 ) ) ;
#50255 = CARTESIAN_POINT ( 'NONE',  ( -6.577113915960836721, 8.766661883411348555, -1.443375672974066548 ) ) ;
#50256 = CARTESIAN_POINT ( 'NONE',  ( 8.188198428010544205, 8.517596018959260107, 0.000000000000000000 ) ) ;
#50257 = COLOUR_RGB ( '', 0.72549020, 0.75294118, 0.79215686) ;
#50258 = CARTESIAN_POINT ( 'NONE',  ( -3.323157048681004699, 6.891117300187535655, -0.7216878364870458196 ) ) ;
#50259 = CARTESIAN_POINT ( 'NONE',  ( 6.533838320793388554, -2.056994387304663885, 0.5145578593022880343 ) ) ;
#50260 = EDGE_LOOP ( 'NONE', ( #32065, #157965, #180514, #207777, #72193 ) ) ;
#50261 = CARTESIAN_POINT ( 'NONE',  ( 3.030630200643165573, 1.283085264563757599, -1.917795831646688320 ) ) ;
#50262 = CARTESIAN_POINT ( 'NONE',  ( 4.439869198996494681, 1.279870211898268550, 1.486999339763886097 ) ) ;
#50263 = EDGE_CURVE ( 'NONE', #140339, #97926, #142782, .T. ) ;
#50264 = CARTESIAN_POINT ( 'NONE',  ( 1.867943658074404434, -1.947550630801861526, 0.2349073745619503772 ) ) ;
#50265 = CARTESIAN_POINT ( 'NONE',  ( 10.39640486358069360, 11.02356051713265650, 0.7998128361456462443 ) ) ;
#50266 = DIRECTION ( 'NONE',  ( 0.000000000000000000, 0.000000000000000000, 1.000000000000000000 ) ) ;
#50267 = EDGE_LOOP ( 'NONE', ( #120311, #125979, #66186 ) ) ;
#50268 = CARTESIAN_POINT ( 'NONE',  ( 0.3216855292715998793, -1.502087118449943137, -1.492529068308690920 ) ) ;
#50269 = CARTESIAN_POINT ( 'NONE',  ( -5.623934791570306402, 5.455678766453782913, 0.7998128361456341429 ) ) ;
#50270 = CARTESIAN_POINT ( 'NONE',  ( 0.3922017905241963476, 1.532332584989907653, -1.020347975915262939 ) ) ;
#50271 = CARTESIAN_POINT ( 'NONE',  ( 4.153319900303814372, 1.837149938469440302, -1.156618460589062813 ) ) ;
#50272 = CARTESIAN_POINT ( 'NONE',  ( -0.2855459137565004024, 2.699313886258678963, 1.981008070493679218 ) ) ;
#50273 = CARTESIAN_POINT ( 'NONE',  ( 1.318772358905948794, -0.7683209907942339933, -1.976687055281033611 ) ) ;
#50274 = CARTESIAN_POINT ( 'NONE',  ( -1.500000000000011324, 2.952083334016149418, 0.8660254037844403729 ) ) ;
#50275 = CARTESIAN_POINT ( 'NONE',  ( 8.158255747121103241, 10.54105100977322174, 1.599625672291281386 ) ) ;
#50276 = CARTESIAN_POINT ( 'NONE',  ( 1.860129666708600693, 2.485233703330023580, 2.479905445520987239 ) ) ;
#50277 = CARTESIAN_POINT ( 'NONE',  ( 6.606590233575550641, 6.765807905838774339, 0.03828827652692379235 ) ) ;
#50278 = ORIENTED_EDGE ( 'NONE', *, *, #78480, .T. ) ;
#50279 = CARTESIAN_POINT ( 'NONE',  ( 2.425137330123087853, -0.003247232972201920167, 2.060967562036238210 ) ) ;
#50281 = CARTESIAN_POINT ( 'NONE',  ( 8.444108128620271714, 14.00294857740392551, -8.463389435957207496 ) ) ;
#50280 = CARTESIAN_POINT ( 'NONE',  ( -9.341731535015849630, 10.85744053139533349, 1.199719254218462483 ) ) ;
#50282 = CARTESIAN_POINT ( 'NONE',  ( 1.364683531249988535, 1.613541667008084879, 0.7879004041258500513 ) ) ;
#50283 = CARTESIAN_POINT ( 'NONE',  ( -1.500000000000001110, 9.270833333333332149, 0.8660254037844418162 ) ) ;
#50284 = LINE ( 'NONE', #32966, #149799 ) ;
#50285 = ORIENTED_EDGE ( 'NONE', *, *, #47557, .F. ) ;
#50286 = CARTESIAN_POINT ( 'NONE',  ( 4.494721087910215296, -1.855708629272670551, -0.4612273479895278583 ) ) ;
#50287 = CARTESIAN_POINT ( 'NONE',  ( 1.500000000000001332, 9.406250000682799595, 0.000000000000000000 ) ) ;
#50288 = CARTESIAN_POINT ( 'NONE',  ( 1.405971756114566595, -0.5497231165422427068, 2.194469222715933476 ) ) ;
#50289 = CARTESIAN_POINT ( 'NONE',  ( -2.591579918506545344, 6.175260338232929413, 1.040834085586084257E-14 ) ) ;
#50290 = CARTESIAN_POINT ( 'NONE',  ( 0.8260602286952464235, -0.8153974433127196830, -1.617802387155008681 ) ) ;
#50291 = CARTESIAN_POINT ( 'NONE',  ( 1.534256617913127174, 0.6047330867673149646, 1.817800723622571057 ) ) ;
#50292 = CARTESIAN_POINT ( 'NONE',  ( 3.139188941651628539, -0.1496422021231707811, -2.064996656166856237 ) ) ;
#50293 = CARTESIAN_POINT ( 'NONE',  ( -1.364683531250012516, 1.592708333674756727, 0.7879004041258379498 ) ) ;
#50294 = EDGE_CURVE ( 'NONE', #17249, #135745, #101151, .T. ) ;
#50295 = CARTESIAN_POINT ( 'NONE',  ( 0.9890677962714401472, 1.739647146885098694, -0.9275093368027197416 ) ) ;
#50296 = CARTESIAN_POINT ( 'NONE',  ( 5.039640240021522999, -1.363685002003648616, -1.361047059521299785 ) ) ;
#50298 = CARTESIAN_POINT ( 'NONE',  ( 6.093313910611117379, 7.014445836765536235, -0.9825430356366869900 ) ) ;
#50297 = CARTESIAN_POINT ( 'NONE',  ( 0.6280632297508845774, -2.189494644770412890, 0.7293192972532935858 ) ) ;
#50299 = CARTESIAN_POINT ( 'NONE',  ( -1.364683531250014514, 1.988541667008086655, -0.7879004041258289570 ) ) ;
#50300 = CARTESIAN_POINT ( 'NONE',  ( 5.441865409415975741, 1.382631645094612338, 1.530856317113358678 ) ) ;
#50301 = CARTESIAN_POINT ( 'NONE',  ( -4.740547266272593596, 8.682388910626682943, -0.7998128361456281477 ) ) ;
#50302 = CARTESIAN_POINT ( 'NONE',  ( 8.938903350111612411, 9.323142084752035430, -0.7998128361456221525 ) ) ;
#50303 = CARTESIAN_POINT ( 'NONE',  ( 0.9999999999999833467, 9.200000000000018829, -0.3999999999999961919 ) ) ;
#50305 = CARTESIAN_POINT ( 'NONE',  ( 0.7499999999999902300, 3.816666666666690411, -1.299038105676658228 ) ) ;
#50304 = CARTESIAN_POINT ( 'NONE',  ( 5.262764605058766421, -1.527415466006694533, 1.450107492850923441 ) ) ;
#50306 = CARTESIAN_POINT ( 'NONE',  ( 1.364683531249990311, 2.946875000341416140, 1.214306433183764966E-14 ) ) ;
#50307 = CARTESIAN_POINT ( 'NONE',  ( 5.343121995983710626, -1.856993961526328007, 1.106124453333141577 ) ) ;
#50308 = CARTESIAN_POINT ( 'NONE',  ( 5.619787797283516184, -0.4887302510508689801, 1.959527308111078669 ) ) ;
#50309 = B_SPLINE_SURFACE_WITH_KNOTS ( 'NONE', 1, 3, ( 
 ( #171853, #136165, #54903, #104735, #170781, #21302, #38655, #39720, #89558, #118896, #187023, #53840, #73266, #184881, #105827, #23448, #202183, #139371, #71122, #137238, #203260, #87409, #155609, #205401, #22371, #88483, #6123, #138300, #57041, #70051, #152404, #119971, #185948, #3983, #204315, #169712, #123207, #153473, #37580, #55972, #52761, #103664, #36506, #102586, #168645, #20248, #100089, #17736, #181333, #133695, #51344, #182384, #53467, #34014, #118534, #199699, #197578, #36138, #15618, #85971, #150987, #35068, #147789, #166150, #117469, #83825, #149918, #49222, #183462, #102221, #101139, #32960, #97984, #3616, #1486, #167227, #81708, #50277, #99035, #213805, #184517, #119604, #132624, #116396, #69694, #66484, #67551, #65427, #200758, #18813, #84900, #164043, #2551, #68626, #19887, #134749, #52407, #148840, #168290, #135798, #152046, #201822, #16681, #31907, #131577, #115341, #165091, #82766, #412, #198630, #70755, #37218, #153106, #139010, #140085, #137935, #104365, #169353, #156320, #171487, #21999, #122843, #170410, #88109, #71825, #154180, #87034, #186661, #187726, #58806, #5748, #207181, #90253, #24150, #55604, #40441, #107624, #206110, #121759, #73992, #203957, #57742, #123900, #189868, #38288, #20938, #141171, #39355, #185588, #105451, #75059, #4681, #103291, #136867, #202893, #41511, #54538, #155245, #188805, #106542, #205033, #23078, #120685, #89194, #6827, #72906, #56678, #172567, #157390, #7903, #173655, #25229, #91332, #8984, #192256, #143575, #209567, #159778, #13520, #30865, #28716, #61213, #94803, #127370, #63346, #10316, #26569, #142499, #208505, #92674, #193341, #176046, #195486, #11378, #158718, #178175, #162993, #60140, #79593, #126297, #47120, #76390, #44986, #111095, #43919, #177101, #160851, #77457, #96943, #12443, #161930, #78522, #110034, #145712, #59073, #129505, #194408, #144639, #191191, #210654, #62282, #128442, #46050, #27639 ),
 ( #112171, #125233, #93739, #29790, #42858, #211710, #75330, #95875, #113237, #179241, #141447, #207454, #108965, #174985, #148859, #100109, #80669, #32978, #133715, #2576, #149936, #165109, #131596, #151006, #200777, #182407, #66504, #213828, #433, #64413, #183481, #132643, #166170, #146760, #99054, #199721, #68646, #1505, #16701, #197598, #134769, #52429, #34036, #198649, #65445, #82787, #50298, #118555, #212778, #116416, #180302, #184536, #114304, #130559, #196549, #17758, #35090, #181352, #147809, #48192, #51367, #83847, #49241, #67571, #115360, #117490, #101160, #167246, #31924, #15639, #18834, #102238, #84918, #36159, #14574, #98003, #164060, #81726, #156341, #19907, #203976, #87055, #74012, #85992, #106563, #90272, #206131, #24169, #70774, #22019, #88129, #38308, #172590, #123922, #121780, #154200, #187747, #5767, #7926, #103311, #56697, #140104, #39375, #104385, #55623, #119624, #71848, #188825, #57761, #53486, #105472, #189890, #41531, #136887, #168309, #152066, #170432, #3636, #137956, #171505, #201842, #155266, #69715, #135818, #185608, #37240, #169373, #20957, #23098, #89213, #122864, #153127, #4698, #186680, #202914, #6847, #54559, #72925, #120705, #139031, #205055, #40459, #91350, #211458, #63093, #77200, #9003, #13272, #94554, #209313, #62038, #43667, #159524, #157412, #79345, #42604, #60960, #128192, #109784, #11123, #75078, #145463, #108711, #210396, #141191, #126039, #129262, #107643, #76141, #144395, #195232, #192002, #175793, #160592, #143319, #194153, #207201, #173675, #59890, #25250, #12199, #78269, #27384, #176847, #29536, #45801, #93485, #111922, #142244, #177922, #95628, #161678, #174739, #58826, #124979, #26312, #190940, #92425, #158465, #10065, #208256, #127117, #193084, #44734, #110841, #28460, #198402, #116167, #184, #114058, #64167, #130310, #96697, #15385, #16448, #14318, #18591, #180051, #132400, #65200, #196297, #17509, #31673, #50044 ) ),
 .UNSPECIFIED., .F., .T., .F.,
 ( 2, 2 ),
 ( 4, 2, 2, 2, 2, 2, 2, 2, 2, 2, 2, 2, 2, 2, 2, 2, 2, 2, 2, 2, 2, 2, 2, 2, 2, 2, 2, 2, 2, 2, 2, 2, 2, 2, 2, 2, 2, 2, 2, 2, 2, 2, 2, 2, 2, 2, 2, 2, 2, 2, 2, 2, 2, 2, 2, 2, 2, 2, 2, 2, 2, 2, 2, 2, 2, 2, 2, 2, 2, 2, 2, 2, 2, 2, 2, 2, 2, 2, 2, 2, 2, 2, 2, 2, 2, 2, 2, 2, 2, 2, 2, 2, 2, 2, 2, 2, 2, 2, 2, 2, 2, 2, 2, 2, 2, 2, 2, 2, 2, 2, 2, 4 ),
 ( 0.000000000000000000, 1.000000000000000000 ),
 ( 0.0003185708494972700616, 0.0004481554763622086794, 0.0005777401032271472971, 0.0007073247300920859149, 0.0008369093569570245326, 0.0009017016703894938957, 0.0009664939838219631504, 0.001031286297254432405, 0.001096078610686901768, 0.001225663237551840277, 0.001290455550984309641, 0.001322851707700544322, 0.001355247864416779004, 0.001420040177849248367, 0.001484832491281717730, 0.001614417118146656239, 0.001679209431579125385, 0.001744001745011594749, 0.001808794058444064112, 0.001873586371876533475, 0.001938378685309002621, 0.002003170998741471767, 0.002067963312173941130, 0.002132755625606410493, 0.002197547939038879856, 0.002229944095755114538, 0.002262340252471349220, 0.002391924879336287946, 0.002521509506201226672, 0.002586301819633696035, 0.002651094133066165398, 0.002715886446498634761, 0.002780678759931104124, 0.002910263386796042417, 0.002975055700228511346, 0.003039848013660980709, 0.003104640327093450072, 0.003169432640525919435, 0.003299017267390858162, 0.003428601894255796888, 0.003493394207688266251, 0.003558186521120735614, 0.003622978834553204977, 0.003687771147985673906, 0.003817355774850612199, 0.003946940401715550925, 0.003979336558431785173, 0.004011732715148020288, 0.004076525028580489651, 0.004141317342012959014, 0.004206109655445428377, 0.004270901968877897741, 0.004335694282310367104, 0.004400486595742836467, 0.004465278909175305830, 0.004594863536040244556, 0.004659655849472713919, 0.004724448162905183282, 0.004789240476337652645, 0.004854032789770122008, 0.004918825103202591371, 0.004983617416635060735, 0.005048409730067530098, 0.005113202043499999461, 0.005177994356932468824, 0.005210390513648703939, 0.005242786670364938187, 0.005372371297229876913, 0.005501955924094814772, 0.005566748237527284135, 0.005631540550959752631, 0.005696332864392221994, 0.005761125177824691357, 0.005890709804689630083, 0.005955502118122099446, 0.006020294431554568809, 0.006085086744987038172, 0.006149879058419507535, 0.006214671371851976898, 0.006279463685284446262, 0.006409048312149384988, 0.006473840625581854351, 0.006506236782298089466, 0.006538632939014323714, 0.006603425252446793077, 0.006668217565879262440, 0.006797802192744201166, 0.006862594506176670529, 0.006927386819609139892, 0.006992179133041609256, 0.007056971446474078619, 0.007121763759906547982, 0.007186556073339017345, 0.007251348386771486708, 0.007316140700203956071, 0.007380933013636425434, 0.007445725327068894797, 0.007510517640501363293, 0.007575309953933832656, 0.007704894580798770515, 0.007769686894231239878, 0.007834479207663709241, 0.007866875364379945224, 0.007899271521096179471, 0.007964063834528647967, 0.008093648461393586693, 0.008158440774826056924, 0.008223233088258525419, 0.008288025401690993915, 0.008352817715123464146, 0.008482402341988402872, 0.008611986968853341598 ),
 .UNSPECIFIED. ) ;
#50310 = EDGE_CURVE ( 'NONE', #79803, #21610, #186451, .T. ) ;
#50313 = CARTESIAN_POINT ( 'NONE',  ( 4.839897650398541806, 8.590371658866210680, 1.040834085586084257E-14 ) ) ;
#50312 = CARTESIAN_POINT ( 'NONE',  ( 3.285556943750000514, -2.413541666188708579, 1.896917185911906500 ) ) ;
#50311 = CARTESIAN_POINT ( 'NONE',  ( 7.635176783151273128, 8.936736330878529699, 1.199719254218452935 ) ) ;
#50314 = CARTESIAN_POINT ( 'NONE',  ( -4.630991987519598396, 7.560518531151607213, 1.199719254218452935 ) ) ;
#50315 = CARTESIAN_POINT ( 'NONE',  ( 3.169157936054858293, 1.820986098869777470, -0.8666075021629695563 ) ) ;
#50316 = CARTESIAN_POINT ( 'NONE',  ( -8.962103233833181193, 10.41454084668224489, -1.199719254218446718 ) ) ;
#50317 = CARTESIAN_POINT ( 'NONE',  ( -2.266184231778562541, 5.795632037050281404, 1.040834085586084257E-14 ) ) ;
#50318 = CARTESIAN_POINT ( 'NONE',  ( 0.6823417656249899377, 4.926041667008086655, -1.181850606188754593 ) ) ;
#50320 = CARTESIAN_POINT ( 'NONE',  ( -11.97302537858683991, 12.30124010191950035, -0.8111997896468238212 ) ) ;
#50319 = CARTESIAN_POINT ( 'NONE',  ( 4.961884481312108797, 2.138711985806662330, -0.3135959325617638238 ) ) ;
#50321 = CARTESIAN_POINT ( 'NONE',  ( 0.000000000000000000, 0.03624871340549007392, 0.000000000000000000 ) ) ;
#50322 = CARTESIAN_POINT ( 'NONE',  ( 6.720655732516641834, 7.051887106169240305, 2.771889904330120391 ) ) ;
#50324 = CARTESIAN_POINT ( 'NONE',  ( 6.099232498865051255, -0.2440123228986730841, 2.001514574626765075 ) ) ;
#50323 = CARTESIAN_POINT ( 'NONE',  ( -6.182154857707119255, 10.15633840072622363, 0.000000000000000000 ) ) ;
#50325 = CARTESIAN_POINT ( 'NONE',  ( 1.499999999999989120, 4.754166666666689522, 0.8660254037844524744 ) ) ;
#50326 = CARTESIAN_POINT ( 'NONE',  ( 0.5919146312290176626, -1.711225830157696137, -0.2159481953097255325 ) ) ;
#50327 = CARTESIAN_POINT ( 'NONE',  ( 3.711900195091365262, 7.552577004240394132, -0.7998128361456362523 ) ) ;
#50329 = CARTESIAN_POINT ( 'NONE',  ( 6.912678218121202534, 9.158153569265168770, 1.599625672291268286 ) ) ;
#50328 = CARTESIAN_POINT ( 'NONE',  ( 7.293923454472077239, 10.49303254931736262, 1.082531754730558626 ) ) ;
#50330 = CARTESIAN_POINT ( 'NONE',  ( -0.5000000000000264233, 3.999999999999976019, -0.4500000000000458633 ) ) ;
#50331 = CARTESIAN_POINT ( 'NONE',  ( 6.468025801952650866, 0.9617254617904011926, 1.604207369834034669 ) ) ;
#50332 = CARTESIAN_POINT ( 'NONE',  ( 0.6979027206182022436, 1.353502529517286446, 1.490303647139071153 ) ) ;
#50333 =( NAMED_UNIT ( * ) SI_UNIT ( $, .STERADIAN. ) SOLID_ANGLE_UNIT ( ) );
#50334 = CARTESIAN_POINT ( 'NONE',  ( -7.729556973122450714, 8.190440354830551328, 0.000000000000000000 ) ) ;
#50335 = VERTEX_POINT ( 'NONE', #72702 ) ;
#50336 = CARTESIAN_POINT ( 'NONE',  ( 10.04622863760192963, 10.82294762006482713, -0.7216878364870257245 ) ) ;
#50338 = CARTESIAN_POINT ( 'NONE',  ( 2.196888872880573551, 1.802427395782604247, 0.9040921628407010413 ) ) ;
#50337 = CARTESIAN_POINT ( 'NONE',  ( 2.174623584685225541, 0.9092215167782154994, 1.915816808323366871 ) ) ;
#50339 = CARTESIAN_POINT ( 'NONE',  ( 2.021461901335448896, -0.3940331753463456321, 1.768040416340182608 ) ) ;
#50340 = CARTESIAN_POINT ( 'NONE',  ( 5.840530312436913007, 10.03597880781023299, 0.000000000000000000 ) ) ;
#50341 = CARTESIAN_POINT ( 'NONE',  ( 6.438358464623771482, 2.137424745569570295, 0.3223339197731683869 ) ) ;
#50342 = ORIENTED_EDGE ( 'NONE', *, *, #128454, .F. ) ;
#50343 = CARTESIAN_POINT ( 'NONE',  ( 5.926885707468349196, 10.06645042535509660, 1.040834085586084257E-14 ) ) ;
#50345 = CARTESIAN_POINT ( 'NONE',  ( 0.3037315811481311467, -1.027229472348114347, -1.616837036282785078 ) ) ;
#50344 = CARTESIAN_POINT ( 'NONE',  ( -4.822949958159302497, 6.649860922651058992, -1.599625672291256295 ) ) ;
#50346 = CYLINDRICAL_SURFACE ( 'NONE', #149251, 0.3999999999999997446 ) ;
#50347 = DIRECTION ( 'NONE',  ( 0.8660254037844399289, -0.4999999999999976130, -6.938893903907224526E-18 ) ) ;
#50348 = AXIS2_PLACEMENT_3D ( 'NONE', #26717, #89614, #191337 ) ;
#50349 = CARTESIAN_POINT ( 'NONE',  ( 6.602457619730771832, 6.805214765881779648, 0.7216878364870317197 ) ) ;
#50350 = CARTESIAN_POINT ( 'NONE',  ( -1.364683531250014514, 0.09270833367475767028, 0.7879004041258379498 ) ) ;
#50351 = CARTESIAN_POINT ( 'NONE',  ( 4.067082894419602468, 3.847277586352047862, -0.7216878364870188411 ) ) ;
#50352 = CARTESIAN_POINT ( 'NONE',  ( -8.350932551013499960, 11.83017284523606172, -1.199719254218446718 ) ) ;
#50353 = CARTESIAN_POINT ( 'NONE',  ( 4.663041391408608405, -1.929494027986548232, -0.9748474430888447451 ) ) ;
#50354 = CARTESIAN_POINT ( 'NONE',  ( -5.153507786970267013, 8.066157280557016307, -1.082531754730549967 ) ) ;
#50355 = CARTESIAN_POINT ( 'NONE',  ( 5.736508392357904107, 5.865217010605237924, 0.000000000000000000 ) ) ;
#50356 = CARTESIAN_POINT ( 'NONE',  ( 1.547299434221154124, 0.2130619955753136618, 2.109896976817266179 ) ) ;
#50357 = CARTESIAN_POINT ( 'NONE',  ( 6.739283625173963621, -1.628968703954777553, 0.8242606506234579911 ) ) ;
#50358 = EDGE_CURVE ( 'NONE', #96370, #141262, #93659, .T. ) ;
#50359 = CARTESIAN_POINT ( 'NONE',  ( 3.040257615459122320, 1.956033444698499268, 0.2450028794991568337 ) ) ;
#50360 = EDGE_LOOP ( 'NONE', ( #86838, #16987, #59676, #48921 ) ) ;
#50361 = CARTESIAN_POINT ( 'NONE',  ( 9.597801448743146224, -7.025535116234753907, -0.01424860406303069330 ) ) ;
#50362 = CARTESIAN_POINT ( 'NONE',  ( 5.828554260932977904, -1.250890888562717684, 1.521285551415082482 ) ) ;
#50363 = CARTESIAN_POINT ( 'NONE',  ( 1.798672962244704410, 1.614485480382701565, 1.078883064099228628 ) ) ;
#50364 = EDGE_LOOP ( 'NONE', ( #155597, #184831, #181326, #169359 ) ) ;
#50365 = CARTESIAN_POINT ( 'NONE',  ( -5.307090785106547415, 5.156303768904543894, -0.7998128361456362523 ) ) ;
#50367 = CARTESIAN_POINT ( 'NONE',  ( 1.854520591217061476, 2.487866942973022244, -2.484107071883403961 ) ) ;
#50366 = CARTESIAN_POINT ( 'NONE',  ( -7.322812365156824654, 8.676274193172000437, 1.082531754730549078 ) ) ;
#50368 = CARTESIAN_POINT ( 'NONE',  ( 7.308008492965924141, 8.484763649003774333, -1.199719254218451159 ) ) ;
#50370 = CARTESIAN_POINT ( 'NONE',  ( 4.706088717274895750, 6.583799151611112954, 1.443375672974065660 ) ) ;
#50369 = CARTESIAN_POINT ( 'NONE',  ( 6.012151052656117933, 9.101594430485762999, 1.199719254218460707 ) ) ;
#50372 = ORIENTED_EDGE ( 'NONE', *, *, #129583, .F. ) ;
#50371 = CARTESIAN_POINT ( 'NONE',  ( 6.006500814222540008, -1.903516144586704151, -0.1827706444143817055 ) ) ;
#50373 = CARTESIAN_POINT ( 'NONE',  ( 4.705825944637973990, -0.5905853116198942487, 2.126329296355852883 ) ) ;
#50374 = CARTESIAN_POINT ( 'NONE',  ( 2.011028756337205348, 1.635159560789069655, -1.482119803565529859 ) ) ;
#50375 = FACE_OUTER_BOUND ( 'NONE', #4457, .T. ) ;
#50376 = CARTESIAN_POINT ( 'NONE',  ( 0.8735180803765253410, 0.3724630581584260081, -1.875478908130092215 ) ) ;
#50377 = CARTESIAN_POINT ( 'NONE',  ( 11.48243876534946217, 11.29999999999998117, 3.199999999999997957 ) ) ;
#50378 = DIRECTION ( 'NONE',  ( 0.8752544141058831162, 0.05606191405903982600, -0.4804027189558818245 ) ) ;
#50379 = CARTESIAN_POINT ( 'NONE',  ( 3.648938843998358106, -0.4010542052625790110, -2.030977206718207473 ) ) ;
#50380 = CARTESIAN_POINT ( 'NONE',  ( -4.924636110261798372, 6.768494766770632332, 1.599625672291267398 ) ) ;
#50381 = AXIS2_PLACEMENT_3D ( 'NONE', #25026, #58607, #9847 ) ;
#50383 = CARTESIAN_POINT ( 'NONE',  ( 1.516726440323381331, 1.451591637995581996, -1.601975981646540426 ) ) ;
#50382 = CARTESIAN_POINT ( 'NONE',  ( -4.762992037102518950, 4.451245552908022596, -0.7998128361456221525 ) ) ;
#50384 = CARTESIAN_POINT ( 'NONE',  ( 3.597391730528697540, -0.6346259394694170330, 2.097678010650514402 ) ) ;
#50385 = CYLINDRICAL_SURFACE ( 'NONE', #136, 1.500000000000000222 ) ;
#50386 = CARTESIAN_POINT ( 'NONE',  ( -1.499999999999946709, 7.750000000000000000, 15.75000000000000711 ) ) ;
#50387 = LINE ( 'NONE', #37326, #51116 ) ;
#50388 = CARTESIAN_POINT ( 'NONE',  ( -1.402160292154681736E-14, 14.98437500034140157, 1.575800808251682339 ) ) ;
#50389 = CARTESIAN_POINT ( 'NONE',  ( -3.980200614063634568, 6.801261928786307642, 1.199719254218452935 ) ) ;
#50390 = PRODUCT_DEFINITION_CONTEXT ( 'detailed design', #81028, 'design' ) ;
#50391 = CARTESIAN_POINT ( 'NONE',  ( 6.029869095562110815, -1.459853974539515153, 0.9356793305193217281 ) ) ;
#50393 = CARTESIAN_POINT ( 'NONE',  ( -3.195971524519394702, 4.751719416737803847, -1.599625672291262513 ) ) ;
#50392 = STYLED_ITEM ( 'NONE', ( #26911 ), #89439 ) ;
#50394 = CARTESIAN_POINT ( 'NONE',  ( 3.924723049676182018, -1.394041313093749457, 1.530695986988837021 ) ) ;
#50395 = CARTESIAN_POINT ( 'NONE',  ( 5.817987567751313982, 1.043164272916985214, -1.842315021624504778 ) ) ;
#50396 = CARTESIAN_POINT ( 'NONE',  ( 5.961834861707224320, 7.978559976790334574, -1.599625672291262513 ) ) ;
#50397 = CARTESIAN_POINT ( 'NONE',  ( -1.364683531249997417, 4.509375000341424133, 1.214306433183764966E-14 ) ) ;
#50398 = CARTESIAN_POINT ( 'NONE',  ( 3.362113288959746704, -1.967404159762261795, 0.09189030742163574461 ) ) ;
#50399 = CARTESIAN_POINT ( 'NONE',  ( 6.281209671116547710, 1.576043917979405684, 1.664718807710400705 ) ) ;
#50401 = EDGE_CURVE ( 'NONE', #94234, #78199, #152966, .T. ) ;
#50400 = CARTESIAN_POINT ( 'NONE',  ( 2.420285107995377327, 1.192830232448302441, -1.382225081888274643 ) ) ;
#50402 = AXIS2_PLACEMENT_3D ( 'NONE', #137781, #72751, #41358 ) ;
#50403 = CARTESIAN_POINT ( 'NONE',  ( 4.228163802615382494, 6.026220084508304708, -1.599625672291269396 ) ) ;
#50404 = CARTESIAN_POINT ( 'NONE',  ( 4.731432421044862835, 6.543090462684225450, -1.443375672974051449 ) ) ;
#50405 = CARTESIAN_POINT ( 'NONE',  ( -7.477485413136760073, 8.682486722536401302, -1.199719254218446718 ) ) ;
#50406 = ORIENTED_EDGE ( 'NONE', *, *, #182418, .F. ) ;
#50407 = EDGE_LOOP ( 'NONE', ( #42542, #144393, #103443, #5182, #170024 ) ) ;
#50408 = CARTESIAN_POINT ( 'NONE',  ( 3.603774441610514412, 1.461153639754816824, 1.385179026781646394 ) ) ;
#50409 = CARTESIAN_POINT ( 'NONE',  ( 3.907043859180459933, -1.606318986283063799, 1.125903821926607318 ) ) ;
#50410 = CARTESIAN_POINT ( 'NONE',  ( -7.426115451983156923, 9.686887332112256388, -1.599625672291263179 ) ) ;
#50411 = CARTESIAN_POINT ( 'NONE',  ( -5.220052836461385404, 6.048815383081766583, -1.199719254218446718 ) ) ;
#50413 = EDGE_CURVE ( 'NONE', #57833, #185672, #70710, .T. ) ;
#50412 = CARTESIAN_POINT ( 'NONE',  ( 3.023105066167310895, 5.702484939155337607, -7.499999999999997335 ) ) ;
#50415 = CARTESIAN_POINT ( 'NONE',  ( 5.541803865142582275, 0.7143684798897788069, -1.619465043896466616 ) ) ;
#50414 = CARTESIAN_POINT ( 'NONE',  ( -0.05888619351396630341, -1.618772603580875158, -1.322922665863958125 ) ) ;
#50416 = CARTESIAN_POINT ( 'NONE',  ( 10.97067990664313264, -5.250949308401987814, -0.2977236940312545377 ) ) ;
#50417 = CARTESIAN_POINT ( 'NONE',  ( 1.605704095283020605, -2.174604996184846595, 0.2706701637196773369 ) ) ;
#50418 = CARTESIAN_POINT ( 'NONE',  ( 0.5381063436600447281, -1.494009556959356999, 0.8925505203737462701 ) ) ;
#50419 = CARTESIAN_POINT ( 'NONE',  ( 6.962275575817444384, 8.081408578997208991, -1.199719254218446718 ) ) ;
#50420 = CARTESIAN_POINT ( 'NONE',  ( 0.6797846375097577054, -0.9621480743811950953, 1.431375779520219549 ) ) ;
#50421 = CARTESIAN_POINT ( 'NONE',  ( 0.6854589470919645322, -1.231871052372325526, -1.940221060253940699 ) ) ;
#50422 = CARTESIAN_POINT ( 'NONE',  ( 0.3983070667218471805, -0.7439898890007863308, -2.061537379893277677 ) ) ;
#50423 = CARTESIAN_POINT ( 'NONE',  ( 6.222016520869273926, -1.489155408782488088, -0.8877787665630013647 ) ) ;
#50424 = CARTESIAN_POINT ( 'NONE',  ( 3.229339687698820072, 0.05429069646168545316, 2.206380697113208722 ) ) ;
#50425 = CARTESIAN_POINT ( 'NONE',  ( 1.674930785650229792, 1.460053457903678131, -1.606915656648603141 ) ) ;
#50426 = CARTESIAN_POINT ( 'NONE',  ( 0.2756506080626683342, 1.048234779247591453, 1.494575289200591239 ) ) ;
#50427 = CARTESIAN_POINT ( 'NONE',  ( 2.272804288956633112, -0.3671671630497001515, -2.085132402650377248 ) ) ;
#50428 = CARTESIAN_POINT ( 'NONE',  ( 6.727182134110194056, 3.682851444631680682, 2.702965647100654234 ) ) ;
#50429 = CARTESIAN_POINT ( 'NONE',  ( 5.614262457756467484, -0.8664596825185383322, -1.720589126903127264 ) ) ;
#50430 = ORIENTED_EDGE ( 'NONE', *, *, #43529, .T. ) ;
#50432 = CARTESIAN_POINT ( 'NONE',  ( -1.499999999999997780, 5.400000000000022560, 1.214306433183764966E-14 ) ) ;
#50431 = CARTESIAN_POINT ( 'NONE',  ( 2.806493257264990326, 1.658461721128750677, -1.582772817771603169 ) ) ;
#50433 = CARTESIAN_POINT ( 'NONE',  ( 4.532503425670185493, 4.182342172903648070, 1.214306433183764966E-14 ) ) ;
#50434 = CARTESIAN_POINT ( 'NONE',  ( 4.924636110261782385, 6.768494766770632332, 1.599625672291267398 ) ) ;
#50435 = CARTESIAN_POINT ( 'NONE',  ( 5.233148740271514221, 2.051824077619863296, 0.8514482647801949744 ) ) ;
#50436 = CARTESIAN_POINT ( 'NONE',  ( -7.212574532790100079, 9.437756259720353924, -1.443375672974059665 ) ) ;
#50437 = DIRECTION ( 'NONE',  ( -0.000000000000000000, 1.000000000000000000, -0.000000000000000000 ) ) ;
#50438 = CARTESIAN_POINT ( 'NONE',  ( 5.504247177468175600, 8.405076892812779477, 1.082531754730558626 ) ) ;
#50439 = CARTESIAN_POINT ( 'NONE',  ( -7.307481607641392429, 11.46921960898288972, 0.7216878364870458196 ) ) ;
#50440 = EDGE_CURVE ( 'NONE', #53793, #6901, #201323, .T. ) ;
#50441 = CARTESIAN_POINT ( 'NONE',  ( 4.909461021924240498, 7.781436054670031410, 1.082531754730549078 ) ) ;
#50442 = ORIENTED_EDGE ( 'NONE', *, *, #69350, .T. ) ;
#50443 = CARTESIAN_POINT ( 'NONE',  ( 2.619767714365705658, 0.2496074646863334634, 2.000857082853441327 ) ) ;
#50445 = CARTESIAN_POINT ( 'NONE',  ( 0.9892170606862679128, 0.1480104381128030111, 2.057284718974061288 ) ) ;
#50444 = CARTESIAN_POINT ( 'NONE',  ( 7.800018446563675489, 7.994443030612759848, -0.7998128361456281477 ) ) ;
#50446 = SURFACE_STYLE_USAGE ( .BOTH. , #169520 ) ;
#50447 = CARTESIAN_POINT ( 'NONE',  ( 6.509323147892504657, 6.766834225395614411, 0.000000000000000000 ) ) ;
#50448 = CARTESIAN_POINT ( 'NONE',  ( -4.121315508874262790, 6.791656612786516334, -1.082531754730549967 ) ) ;
#50449 = CARTESIAN_POINT ( 'NONE',  ( -1.364683531250012516, 3.488541667008085767, -0.7879004041258300672 ) ) ;
#50450 = CARTESIAN_POINT ( 'NONE',  ( 4.470767510317084970, 0.001397387737574890204, -2.191629466793604930 ) ) ;
#50451 = CARTESIAN_POINT ( 'NONE',  ( 1.688125190044654556, 1.678006053171029688, 1.117831401076685660 ) ) ;
#50452 = CARTESIAN_POINT ( 'NONE',  ( 0.5382993156314471728, -1.579489783069366604, 0.9460463261394758128 ) ) ;
#50453 = CARTESIAN_POINT ( 'NONE',  ( 5.689115845898126800, 1.733752489355618875, 1.499825188574270607 ) ) ;
#50454 = CARTESIAN_POINT ( 'NONE',  ( 4.874869531740305462, 1.716800804850382223, -0.6655867697097294089 ) ) ;
#50455 = CARTESIAN_POINT ( 'NONE',  ( 7.446452682403650769, 9.710614100936176385, -1.599625672291262513 ) ) ;
#50456 = CARTESIAN_POINT ( 'NONE',  ( 4.330939430599492823, 0.08983702179986638447, 1.823481399301421169 ) ) ;
#50457 = CARTESIAN_POINT ( 'NONE',  ( 4.518204034511161815, -1.842447959940773705, 0.8197716922626956393 ) ) ;
#50458 = CARTESIAN_POINT ( 'NONE',  ( -8.474009703741204547, 9.845098394908269768, -1.199719254218446718 ) ) ;
#50460 = CARTESIAN_POINT ( 'NONE',  ( -6.794571259104023930, 7.956029886156682274, 1.199719254218452047 ) ) ;
#50459 = CARTESIAN_POINT ( 'NONE',  ( 4.030342351814687696, 1.213150246598847293, -1.909612865279747052 ) ) ;
#50461 = CARTESIAN_POINT ( 'NONE',  ( 6.387733883603046614, 1.449543625446013673, 1.527951702703828074 ) ) ;
#50462 = CARTESIAN_POINT ( 'NONE',  ( -1.826099658462952746, 3.981846818258216292, -0.4000000000000286104 ) ) ;
#50463 = CARTESIAN_POINT ( 'NONE',  ( 5.072747062355987602, 1.430223858385268665, -1.497173470029027120 ) ) ;
#50464 = CARTESIAN_POINT ( 'NONE',  ( 7.730120138085914583, 12.17022392774227768, 0.7998128361456462443 ) ) ;
#50465 = PLANE ( 'NONE',  #276 ) ;
#50466 = APPLICATION_PROTOCOL_DEFINITION ( 'draft international standard', 'automotive_design', 1998, #156970 ) ;
#50468 = CARTESIAN_POINT ( 'NONE',  ( 1.910648867733771850, 1.427813452364127045, -1.293523827780170166 ) ) ;
#50467 = CARTESIAN_POINT ( 'NONE',  ( -6.828502922777144768, 11.11833717654868892, 0.7998128361456481317 ) ) ;
#50469 = CARTESIAN_POINT ( 'NONE',  ( -2.788906526875773208E-15, 13.21875000068279604, -1.499999999999998446 ) ) ;
#50470 = CARTESIAN_POINT ( 'NONE',  ( 3.512971199272317602, 6.152197928242737923, -1.082531754730549967 ) ) ;
#50471 = CARTESIAN_POINT ( 'NONE',  ( 5.794097129154974546, 6.036864960932135205, -0.5213279746436976225 ) ) ;
#50472 = CARTESIAN_POINT ( 'NONE',  ( -3.090368948911150770, 5.692848642783215674, 1.199719254218462483 ) ) ;
#50474 = CARTESIAN_POINT ( 'NONE',  ( 1.547463978342083157, 0.2240547868478468541, 2.210115929984892258 ) ) ;
#50473 = CARTESIAN_POINT ( 'NONE',  ( 0.6332531790259123827, 1.961634380476449335, 0.8060562103610890983 ) ) ;
#50475 = CARTESIAN_POINT ( 'NONE',  ( 2.872209793879555217, 1.125368584265328264, 1.779858853945482489 ) ) ;
#50476 = CARTESIAN_POINT ( 'NONE',  ( -5.562588163356775972, 9.711712967216715953, 0.7998128361456291469 ) ) ;
#50477 = CARTESIAN_POINT ( 'NONE',  ( 5.615048174354031474, 9.702639970055050966, 0.7998128361456462443 ) ) ;
#50478 = CARTESIAN_POINT ( 'NONE',  ( 3.525789274851616639, 1.914599547803575330, -0.4273510147508317591 ) ) ;
#50479 = CARTESIAN_POINT ( 'NONE',  ( 5.606460214450851964, 6.499623990736163037, 1.199719254218462483 ) ) ;
#50481 =( BOUNDED_SURFACE ( )  B_SPLINE_SURFACE ( 3, 2, ( 
 ( #96341, #111566, #146160 ),
 ( #207919, #77927, #210043 ),
 ( #76853, #127851, #125700 ),
 ( #45450, #177574, #29187 ) ),
 .UNSPECIFIED., .F., .F., .F. ) 
 B_SPLINE_SURFACE_WITH_KNOTS ( ( 4, 4 ),
 ( 3, 3 ),
 ( 0.005025772024296196530, 0.008052159968022380709 ),
 ( 0.000000000000000000, 1.000000000000000000 ),
 .UNSPECIFIED. ) 
 GEOMETRIC_REPRESENTATION_ITEM ( )  RATIONAL_B_SPLINE_SURFACE ( (
 ( 1.000000000000000000, 0.7187737999613678097, 1.000000000000000000),
 ( 1.000000000000000000, 0.7186585579881044072, 1.000000000000000000),
 ( 1.000000000000000000, 0.7185467277397536989, 1.000000000000000000),
 ( 1.000000000000000000, 0.7184380228464064544, 1.000000000000000000) ) ) 
 REPRESENTATION_ITEM ( '' )  SURFACE ( )  );
#50480 = CARTESIAN_POINT ( 'NONE',  ( -4.022721148277657477, 7.614442113290216696, -0.1953124528039917873 ) ) ;
#50482 = CARTESIAN_POINT ( 'NONE',  ( 5.332434488876471868, 5.115595079977664383, 0.7998128361456341429 ) ) ;
#50483 = CARTESIAN_POINT ( 'NONE',  ( -5.099275172515603138, 8.002885897026576600, 1.082531754730549967 ) ) ;
#50484 = CARTESIAN_POINT ( 'NONE',  ( -8.215877900201387973, 8.687538426430837291, 0.7216878364870578100 ) ) ;
#50485 = CARTESIAN_POINT ( 'NONE',  ( 1.951583061186522583, -1.892041120407188304, 0.9578705467366486204 ) ) ;
#50486 = CARTESIAN_POINT ( 'NONE',  ( -5.478376588373717659, 8.549133898814758936, -1.199719254218452047 ) ) ;
#50488 = CARTESIAN_POINT ( 'NONE',  ( 4.984793487045196869, 1.876812866478014596, 0.5713181500588762063 ) ) ;
#50487 = CARTESIAN_POINT ( 'NONE',  ( 0.6124999999999655165, 0.08333333333334497217, 1.060881119635885828 ) ) ;
#50489 = CARTESIAN_POINT ( 'NONE',  ( 3.836934241894359054, 0.3148432204054998351, 2.138525872868973998 ) ) ;
#50490 = CARTESIAN_POINT ( 'NONE',  ( 2.946635061770471076, -1.506786691049965432, -1.057933238436038925 ) ) ;
#50491 = CARTESIAN_POINT ( 'NONE',  ( -4.082753340799282427, 7.529786358835235838, 0.5248769202933333267 ) ) ;
#50492 = CARTESIAN_POINT ( 'NONE',  ( -1.402160292154681736E-14, -0.8656249996585829720, 1.575800808251672791 ) ) ;
#50493 = CARTESIAN_POINT ( 'NONE',  ( 4.259493880088534468, 0.8231460567260719952, 1.533345966155388540 ) ) ;
#50494 = CARTESIAN_POINT ( 'NONE',  ( -9.117697077652850979, 16.00000000001154987, -7.299999999985687715 ) ) ;
#50495 = CARTESIAN_POINT ( 'NONE',  ( 5.558479791922850133, 6.547609847740540445, -1.082531754730542195 ) ) ;
#50496 = CARTESIAN_POINT ( 'NONE',  ( -10.87640920097716091, 5.776148811624420176, 6.414305308649663750 ) ) ;
#50497 = CARTESIAN_POINT ( 'NONE',  ( 1.692469166403000491, -2.151312531270420436, -0.2117842694067117448 ) ) ;
#50498 = AXIS2_PLACEMENT_3D ( 'NONE', #204986, #154133, #188754 ) ;
#50499 = CARTESIAN_POINT ( 'NONE',  ( 3.954453749441131816, 1.458333106491338960, 1.392332789497241263 ) ) ;
#50500 = CARTESIAN_POINT ( 'NONE',  ( 1.499999999999993117, 12.88541666734946567, 0.8660254037844408170 ) ) ;
#50501 = CARTESIAN_POINT ( 'NONE',  ( 1.428841412761387986, 2.083414371474631377, 0.5762002773818803991 ) ) ;
#50502 = CARTESIAN_POINT ( 'NONE',  ( 3.309407512850143451, -0.3859909667141645517, 1.933149248684182808 ) ) ;
#50503 = CARTESIAN_POINT ( 'NONE',  ( -1.737499999999997824, -2.697916665710752060, 3.009438278150925683 ) ) ;
#50504 = CARTESIAN_POINT ( 'NONE',  ( 3.263160552478797882, 1.894124000634039851, -0.4281397233536556879 ) ) ;
#50507 = ORIENTED_EDGE ( 'NONE', *, *, #54338, .F. ) ;
#50506 = CARTESIAN_POINT ( 'NONE',  ( -3.291193844602480212, -0.1067382855773401085, -0.04028451622573153701 ) ) ;
#50505 = CARTESIAN_POINT ( 'NONE',  ( -8.283668667825340393, 12.60810451253083997, 0.7216878364870458196 ) ) ;
#50508 = CARTESIAN_POINT ( 'NONE',  ( -8.093291352714894415, 8.406871097780989288, -0.7998128361456362523 ) ) ;
#50509 = CARTESIAN_POINT ( 'NONE',  ( 3.549202351727371862, 7.362762853649070571, -0.7998128361456362523 ) ) ;
#50510 = CARTESIAN_POINT ( 'NONE',  ( -5.281783360975562225, 8.319775133516907673, 1.199719254218452935 ) ) ;
#50511 = CARTESIAN_POINT ( 'NONE',  ( -9.368320956918621434, 11.95279375453699622, 1.443375672974076540 ) ) ;
#50512 = CARTESIAN_POINT ( 'NONE',  ( 1.061882456046374434, 0.4290601450722114074, -2.164491299336705588 ) ) ;
#50513 = CARTESIAN_POINT ( 'NONE',  ( -3.285556943750000514, -2.938541666188710266, -1.896917185911906500 ) ) ;
#50514 = CARTESIAN_POINT ( 'NONE',  ( 5.576992410575341452, 1.811172876804711507, 0.7542287045681006497 ) ) ;
#50515 = CARTESIAN_POINT ( 'NONE',  ( 2.479138880926802901, -2.011204309026824344, -0.1455328587063598189 ) ) ;
#50516 = ORIENTED_EDGE ( 'NONE', *, *, #143132, .F. ) ;
#50517 = CARTESIAN_POINT ( 'NONE',  ( 2.993478482863177081, -0.4084587893785693868, 2.077413892881809776 ) ) ;
#50518 = CARTESIAN_POINT ( 'NONE',  ( 1.499999999999990896, 3.306250000682818602, 1.214306433183764966E-14 ) ) ;
#50520 = CARTESIAN_POINT ( 'NONE',  ( -7.067878151425722955, 7.140279352951794500, 0.7998128361456341429 ) ) ;
#50519 = CARTESIAN_POINT ( 'NONE',  ( 0.07459516483345089710, 0.2549822845471191868, -1.790622017744479155 ) ) ;
#50521 = CARTESIAN_POINT ( 'NONE',  ( 4.417794048288587128, 1.130693009273657124, -1.452954439256304520 ) ) ;
#50522 = ORIENTED_EDGE ( 'NONE', *, *, #6214, .F. ) ;
#50523 = CARTESIAN_POINT ( 'NONE',  ( -9.494787648271923786, 9.971673765939062406, 1.040834085586084257E-14 ) ) ;
#50524 = CARTESIAN_POINT ( 'NONE',  ( 4.887034483293543730, -1.997634423138573867, -0.7120497732875651353 ) ) ;
#50525 = FACE_OUTER_BOUND ( 'NONE', #25903, .T. ) ;
#50526 = CARTESIAN_POINT ( 'NONE',  ( 5.178324605415663306, 8.128796908705222535, 1.199719254218462483 ) ) ;
#50527 = CARTESIAN_POINT ( 'NONE',  ( 5.167286647625595641, 0.2060095241231186813, -2.050478191761321956 ) ) ;
#50530 = CARTESIAN_POINT ( 'NONE',  ( 2.893917256732419396, -0.5369380550670297403, -1.761199466696103499 ) ) ;
#50529 = CARTESIAN_POINT ( 'NONE',  ( 1.293147247811817779, -1.684623093139308025, 0.7912131235938785201 ) ) ;
#50528 = DIRECTION ( 'NONE',  ( 0.6507913734559627184, 0.7592566023653016805, 0.000000000000000000 ) ) ;
#50531 = CARTESIAN_POINT ( 'NONE',  ( 9.596473800374404561, 10.09030761005864285, 0.000000000000000000 ) ) ;
#50532 = CARTESIAN_POINT ( 'NONE',  ( 11.92619526913699879, 19.00000000000000000, -1.328859060402686199 ) ) ;
#50533 = CYLINDRICAL_SURFACE ( 'NONE', #84416, 1.250000000000000000 ) ;
#50534 = CIRCLE ( 'NONE', #40027, 0.4000000000000010214 ) ;
#50535 = CARTESIAN_POINT ( 'NONE',  ( 2.614145488985010424, -2.182733025630137824, 0.3247920039054427721 ) ) ;
#50536 = CARTESIAN_POINT ( 'NONE',  ( 4.727936083913598431, -1.386761530526101405, -1.787517356406182811 ) ) ;
#50537 = CARTESIAN_POINT ( 'NONE',  ( -5.883875478650828050, 9.808345791827219884, 0.7216878364870458196 ) ) ;
#50538 = CARTESIAN_POINT ( 'NONE',  ( 4.377109366116209266, -1.621248278760094363, -0.8084319655582442588 ) ) ;
#50539 = CARTESIAN_POINT ( 'NONE',  ( 4.926915384452605018, -1.639780065798799757, 0.9903009516807855794 ) ) ;
#50540 = CARTESIAN_POINT ( 'NONE',  ( 1.364683531249990311, 5.426041667008086655, 0.7879004041258500513 ) ) ;
#50541 = EDGE_CURVE ( 'NONE', #69383, #202042, #53265, .T. ) ;
#50542 = CARTESIAN_POINT ( 'NONE',  ( 4.733189744967194024, -1.710186631362722531, 0.7584244158565585092 ) ) ;
#50543 = CARTESIAN_POINT ( 'NONE',  ( 4.545250530879026307, 1.662896905596674468, -0.8357390809586220382 ) ) ;
#50544 = CARTESIAN_POINT ( 'NONE',  ( -0.6823417656249969321, 4.967708333674755394, -1.181850606188749264 ) ) ;
#50545 = CARTESIAN_POINT ( 'NONE',  ( 6.244957947127046438, -1.492741346086885024, 0.9504933407481640506 ) ) ;
#50546 = CARTESIAN_POINT ( 'NONE',  ( -0.08279552664090458758, -1.841734517378278424, 0.8216794407479923734 ) ) ;
#50548 = CARTESIAN_POINT ( 'NONE',  ( 2.860102072500060544, 2.095886770163409185, -0.2068341903323153708 ) ) ;
#50547 = CARTESIAN_POINT ( 'NONE',  ( -9.561524646135538319, 12.17819805862340310, -1.599625672291263179 ) ) ;
#50549 = CARTESIAN_POINT ( 'NONE',  ( 10.42352117080803708, 11.05519620889787724, -0.7998128361456281477 ) ) ;
#50551 = CARTESIAN_POINT ( 'NONE',  ( -8.618179199781044630, 13.20629283305325963, 0.7998128361456341429 ) ) ;
#50550 = CARTESIAN_POINT ( 'NONE',  ( -1.734723475976807094E-15, 2.999999999999988898, -6.938893903907228378E-15 ) ) ;
#50552 = FILL_AREA_STYLE ('',( #63610 ) ) ;
#50553 = CARTESIAN_POINT ( 'NONE',  ( 2.355728564803623915, -1.499445635549499389, -1.353443481924651470 ) ) ;
#50554 = CARTESIAN_POINT ( 'NONE',  ( -1.364683531250000748, 2.009375000341421913, 1.214306433183764966E-14 ) ) ;
#50555 = STYLED_ITEM ( 'NONE', ( #57321 ), #141351 ) ;
#50556 = CARTESIAN_POINT ( 'NONE',  ( 6.720655732516679137, 4.703287744343486843, 2.289001594030832365 ) ) ;
#50557 = CARTESIAN_POINT ( 'NONE',  ( 3.323720213644492993, 7.029424015893889433, 1.040834085586084257E-14 ) ) ;
#50558 = ORIENTED_EDGE ( 'NONE', *, *, #18068, .F. ) ;
#50559 = CARTESIAN_POINT ( 'NONE',  ( 2.179201376995115513, -0.1036959380565916911, -2.159207860300814463 ) ) ;
#50560 = FACE_OUTER_BOUND ( 'NONE', #204987, .T. ) ;
#50563 = FACE_OUTER_BOUND ( 'NONE', #71758, .T. ) ;
#50562 = CARTESIAN_POINT ( 'NONE',  ( 1.499999999999996891, 13.17708333401612997, -0.8660254037844378194 ) ) ;
#50561 = CARTESIAN_POINT ( 'NONE',  ( 4.061549535745618833, 6.896169004081968090, -1.199719254218452047 ) ) ;
#50564 = CARTESIAN_POINT ( 'NONE',  ( 9.747949258101261449, 11.43532422494874368, -1.082531754730537088 ) ) ;
#50565 = CARTESIAN_POINT ( 'NONE',  ( 6.491432910188612126, -0.4373703761123280964, 1.975813455233149218 ) ) ;
#50566 = CARTESIAN_POINT ( 'NONE',  ( -6.968527767744110868, 9.153035033833367251, 1.443375672974078761 ) ) ;
#50567 = CARTESIAN_POINT ( 'NONE',  ( 1.470551405592795957, -2.082434148983134392, -0.6831980896230758216 ) ) ;
#50568 = CARTESIAN_POINT ( 'NONE',  ( -3.652727762210548068, 6.150616677256791398, 1.207173405259515775 ) ) ;
#50569 = CARTESIAN_POINT ( 'NONE',  ( 2.026610535765199561, 1.302222112816675326, -1.850007447375429104 ) ) ;
#50570 = CARTESIAN_POINT ( 'NONE',  ( -8.993135964566285168, 9.386413468282476913, -0.7998128361456291469 ) ) ;
#50571 = CARTESIAN_POINT ( 'NONE',  ( -4.080641047588907888, 6.744203074620265248, -1.082531754730548412 ) ) ;
#50572 = CARTESIAN_POINT ( 'NONE',  ( -1.364683531250012516, 3.301041667008084879, -0.7879004041258289570 ) ) ;
#50573 = CARTESIAN_POINT ( 'NONE',  ( 4.871809496981259535, 8.050285353323946680, -0.9368363805376724862 ) ) ;
#50574 = CARTESIAN_POINT ( 'NONE',  ( -6.009258394948636914E-15, 10.68750000000000355, -1.732050807568875195 ) ) ;
#50575 = CARTESIAN_POINT ( 'NONE',  ( 3.984117037569365305, 5.741498858621315371, 1.599625672291261402 ) ) ;
#50576 = CARTESIAN_POINT ( 'NONE',  ( 2.723612921674794407, -1.015349471937683656, -1.449289906420585305 ) ) ;
#50577 = CARTESIAN_POINT ( 'NONE',  ( 3.176434313366371942, 0.9072602101105414762, 1.797144717478225795 ) ) ;
#50578 = CARTESIAN_POINT ( 'NONE',  ( 6.721690211428396289, -2.142211831252617493, 0.5295551626897446740 ) ) ;
#50579 = CARTESIAN_POINT ( 'NONE',  ( 0.6823417656249969321, 8.526041667008064096, -1.181850606188757036 ) ) ;
#50580 = EDGE_LOOP ( 'NONE', ( #103997, #140075, #155489, #84478 ) ) ;
#50581 = CARTESIAN_POINT ( 'NONE',  ( -4.613517410400161722, 8.604463755433990002, -0.7998128361456362523 ) ) ;
#50582 = CARTESIAN_POINT ( 'NONE',  ( 5.378529868213833609, -0.4926607797600784378, -1.955169007017331317 ) ) ;
#50583 = ORIENTED_EDGE ( 'NONE', *, *, #134927, .T. ) ;
#50584 = CARTESIAN_POINT ( 'NONE',  ( 2.781945002432617997, -0.9632652739061452474, 1.603442845774772474 ) ) ;
#50585 = CARTESIAN_POINT ( 'NONE',  ( 2.114207291064807759, 2.064986537539798661, -0.1480984254652456533 ) ) ;
#50586 = CARTESIAN_POINT ( 'NONE',  ( -6.197485614778184271, 9.284131412999601096, 1.082531754730549967 ) ) ;
#50587 = CARTESIAN_POINT ( 'NONE',  ( 2.496234081663367022, -0.9796988711565941532, 1.642222327643327873 ) ) ;
#50588 = CARTESIAN_POINT ( 'NONE',  ( -4.489157070319179432, 8.251450656689856444, 5.811111664500048210E-05 ) ) ;
#50589 = CARTESIAN_POINT ( 'NONE',  ( -9.928285507789787800, 5.423409019249701757, -6.081825614513333811 ) ) ;
#50590 = CARTESIAN_POINT ( 'NONE',  ( -1.201851678989727383E-14, 3.884375000341423689, 1.575800808251672791 ) ) ;
#50591 = CARTESIAN_POINT ( 'NONE',  ( -0.08783152977152529350, -1.912005390248720627, -0.04503566501021933483 ) ) ;
#50592 = CARTESIAN_POINT ( 'NONE',  ( 6.265276383290871109, 7.442482214328385304, -1.082531754730548412 ) ) ;
#50593 = CARTESIAN_POINT ( 'NONE',  ( 2.558977423257744022, 1.577441344615847951, -1.166261179026031325 ) ) ;
#50594 = CARTESIAN_POINT ( 'NONE',  ( 0.000000000000000000, -6.527411821100059797, 0.000000000000000000 ) ) ;
#50595 = CARTESIAN_POINT ( 'NONE',  ( -5.808742468812186033, 5.741564066561132940, 0.000000000000000000 ) ) ;
#50596 = CARTESIAN_POINT ( 'NONE',  ( 5.045234882716379765, 0.1584239314957915090, 2.114765283346302205 ) ) ;
#50598 = CARTESIAN_POINT ( 'NONE',  ( 10.91970695577495043, -5.907420853759282053, 8.673617379884035472E-15 ) ) ;
#50597 = CARTESIAN_POINT ( 'NONE',  ( 9.748476143425788720, 11.33197590787365172, -1.199719254218440723 ) ) ;
#50599 = CARTESIAN_POINT ( 'NONE',  ( 6.854760797074392897, -1.525272977149809694, 1.248552938341955798 ) ) ;
#50600 = CARTESIAN_POINT ( 'NONE',  ( -1.364683531250012516, 2.988541667008091096, -0.7879004041258289570 ) ) ;
#50601 = CARTESIAN_POINT ( 'NONE',  ( 1.529542846128278066, -0.2424046428922912721, 1.998471667700427057 ) ) ;
#50603 = CARTESIAN_POINT ( 'NONE',  ( 1.282980312568120951, 1.728570797422763095, -1.222324810828350428 ) ) ;
#50602 = CARTESIAN_POINT ( 'NONE',  ( -7.754900677336769022, 9.110100880723427608, 1.082531754730558626 ) ) ;
#50604 = CARTESIAN_POINT ( 'NONE',  ( 11.71300746584224228, 6.994125539613667897, 2.416616313326010346 ) ) ;
#50605 = CARTESIAN_POINT ( 'NONE',  ( 2.611853368047814872, 0.5545374748289233491, -1.994631108499920646 ) ) ;
#50606 = B_SPLINE_CURVE_WITH_KNOTS ( 'NONE', 3,
 ( #213463, #31558, #148501, #47827, #29425, #163690, #13152, #131243, #82412, #66133, #15272, #78156, #128080, #95516, #113939, #197230 ),
 .UNSPECIFIED., .F., .F.,
 ( 4, 3, 3, 3, 3, 4 ),
 ( 0.000000000000000000, 3.357822776042505863E-05, 6.715700932737113144E-05, 0.0001007352753633138738, 0.0001343124815392893027, 0.0001562160020015778686 ),
 .UNSPECIFIED. ) ;
#50607 = CARTESIAN_POINT ( 'NONE',  ( 5.415556014015861841, 5.282846535965431300, -0.7998128361456481317 ) ) ;
#50608 = CARTESIAN_POINT ( 'NONE',  ( 5.086243903782109221, 5.962981304947771122, -1.199719254218452047 ) ) ;
#50609 = ORIENTED_EDGE ( 'NONE', *, *, #153621, .F. ) ;
#50611 = CARTESIAN_POINT ( 'NONE',  ( 4.436542580169809291, 6.199052314996659874, 1.599625672291267398 ) ) ;
#50610 = CARTESIAN_POINT ( 'NONE',  ( 5.999963288868293887, -0.7514721766869683073, -1.951089947871258001 ) ) ;
#50614 = EDGE_LOOP ( 'NONE', ( #135576, #25025, #41459, #198299, #16293 ) ) ;
#50613 = CARTESIAN_POINT ( 'NONE',  ( 3.176200218816268350, 0.8167180202140277290, 1.616994655555709981 ) ) ;
#50612 = CARTESIAN_POINT ( 'NONE',  ( 3.750846114953470867, -1.492790808496821775, 1.050590184284278861 ) ) ;
#50615 = CARTESIAN_POINT ( 'NONE',  ( 8.269583629331492602, 11.73526576994040482, 1.199719254218450271 ) ) ;
#50616 = CARTESIAN_POINT ( 'NONE',  ( 1.734723475976807094E-15, 0.7598076211376200151, 3.469446951953614189E-15 ) ) ;
#50617 = CARTESIAN_POINT ( 'NONE',  ( 9.476162529375914190, 12.06195001017501411, -6.315961596902559982 ) ) ;
#50618 = CARTESIAN_POINT ( 'NONE',  ( 4.840968367003476658, 0.3731960759543617168, 2.174832070070693568 ) ) ;
#50619 = CARTESIAN_POINT ( 'NONE',  ( -8.012344526598182026E-15, 10.35937500034139624, -1.575800808251669460 ) ) ;
#50620 = ORIENTED_EDGE ( 'NONE', *, *, #49638, .F. ) ;
#50621 = CARTESIAN_POINT ( 'NONE',  ( 4.213462193461685601, 1.537813053725526569, 1.136448645172025262 ) ) ;
#50622 = CARTESIAN_POINT ( 'NONE',  ( -4.959585264500673496, 4.680604318205876524, 1.214306433183764966E-14 ) ) ;
#50623 = CARTESIAN_POINT ( 'NONE',  ( 5.798083248138522272, 9.916180889470295412, 0.7998128361456462443 ) ) ;
#50624 = CARTESIAN_POINT ( 'NONE',  ( 1.360316468749963592, 1.317708333674712184, -0.7853790794158981292 ) ) ;
#50625 = CARTESIAN_POINT ( 'NONE',  ( 5.639828713160493834, 5.682147708216442439, 1.040834085586084257E-14 ) ) ;
#50626 = CARTESIAN_POINT ( 'NONE',  ( 8.081892667527529994, -5.166862915010145052, -7.462104991928515396 ) ) ;
#50627 = DIRECTION ( 'NONE',  ( -1.000000000000000000, 5.421010862427531636E-15, -8.638326563840826660E-31 ) ) ;
#50628 = CARTESIAN_POINT ( 'NONE',  ( 0.1164230846485321547, -0.09151219166612066525, 1.839079034809627755 ) ) ;
#50629 = ORIENTED_EDGE ( 'NONE', *, *, #52880, .F. ) ;
#50630 = DIRECTION ( 'NONE',  ( 0.000000000000000000, 1.000000000000000000, 0.000000000000000000 ) ) ;
#50631 = CARTESIAN_POINT ( 'NONE',  ( 3.760894150569486616, -1.648321677062795976, -0.8843367818652316803 ) ) ;
#50632 = CARTESIAN_POINT ( 'NONE',  ( 11.84668730067608600, 10.90000000000000036, -1.400000000000001910 ) ) ;
#50633 = STYLED_ITEM ( 'NONE', ( #64172 ), #125288 ) ;
#50634 = CARTESIAN_POINT ( 'NONE',  ( 0.008622056077349157799, 14.55305231409391808, 11.95585894185517084 ) ) ;
#50635 = CARTESIAN_POINT ( 'NONE',  ( -6.643132081016132062, 8.773406732650713025, 1.443375672974078761 ) ) ;
#50636 = VECTOR ( 'NONE', #119490, 1000.000000000000000 ) ;
#50637 = CARTESIAN_POINT ( 'NONE',  ( 5.684946482831785275, 5.526859072925533134, -0.7998128361456231517 ) ) ;
#50638 = CARTESIAN_POINT ( 'NONE',  ( 1.059349595761612584, 1.606854154984382443, 1.138435182648824373 ) ) ;
#50639 = CARTESIAN_POINT ( 'NONE',  ( 2.706657832681820697, 1.899625987897411772, 0.6766965020792228280 ) ) ;
#50640 = CARTESIAN_POINT ( 'NONE',  ( -8.833300774503376473, 10.26427131079744193, 1.199719254218462483 ) ) ;
#50641 = CARTESIAN_POINT ( 'NONE',  ( 7.367930134383754215, 7.560616343061329125, -0.7998128361456341429 ) ) ;
#50642 = DIRECTION ( 'NONE',  ( 1.000000000000000000, -7.771561172376097755E-16, -4.440892098500627148E-16 ) ) ;
#50643 = CARTESIAN_POINT ( 'NONE',  ( 2.800927341068761844, 1.851789894747071008, 1.171597702228709181 ) ) ;
#50644 = CARTESIAN_POINT ( 'NONE',  ( 6.428339884752385380, 1.046657586246093175, -1.495688092090129873 ) ) ;
#50645 = CARTESIAN_POINT ( 'NONE',  ( -2.137381772448751605, 5.645362501165475777, -0.7998128361456281477 ) ) ;
#50646 = CARTESIAN_POINT ( 'NONE',  ( 10.18461545817735470, 3.956598013261175772, -5.433575010662928584 ) ) ;
#50647 = CARTESIAN_POINT ( 'NONE',  ( 5.750066545971570520, 5.881034856487848295, -0.7216878364870458196 ) ) ;
#50648 = CARTESIAN_POINT ( 'NONE',  ( 7.723341061279088038, 12.16231500480096983, -0.7998128361456291469 ) ) ;
#50649 =( BOUNDED_SURFACE ( )  B_SPLINE_SURFACE ( 3, 2, ( 
 ( #183826, #70052, #201121 ),
 ( #72192, #10140, #86334 ),
 ( #174817, #20249, #119972 ),
 ( #154543, #185949, #71123 ),
 ( #136166, #104736, #39721 ),
 ( #202184, #102587, #108791 ),
 ( #153474, #37581, #184882 ),
 ( #170782, #103665, #36507 ),
 ( #152405, #52762, #53841 ),
 ( #169713, #117835, #92506 ),
 ( #118897, #35438, #22372 ),
 ( #2916, #21303, #87410 ),
 ( #5048, #167585, #137239 ),
 ( #203261, #55973, #54904 ) ),
 .UNSPECIFIED., .F., .F., .T. ) 
 B_SPLINE_SURFACE_WITH_KNOTS ( ( 4, 2, 2, 2, 2, 2, 4 ),
 ( 3, 3 ),
 ( 0.000000000000000000, 0.002683261324918884486, 0.004024891987378326728, 0.005366522649837768971, 0.006708153312297211214, 0.008049783974756653457, 0.01073304529967553794 ),
 ( 0.000000000000000000, 1.000000000000000000 ),
 .UNSPECIFIED. ) 
 GEOMETRIC_REPRESENTATION_ITEM ( )  RATIONAL_B_SPLINE_SURFACE ( (
 ( 1.000000000000000000, 0.8509629433967599299, 1.000000000000000000),
 ( 1.000000000000000000, 0.8507446670468529204, 1.000000000000000000),
 ( 1.000000000000000000, 0.8493858944964507440, 1.000000000000000000),
 ( 1.000000000000000000, 0.8493961065500198471, 1.000000000000000000),
 ( 1.000000000000000000, 0.8496860651742271786, 1.000000000000000000),
 ( 1.000000000000000000, 0.8504612216956620729, 1.000000000000000000),
 ( 1.000000000000000000, 0.8509399017528684883, 1.000000000000000000),
 ( 1.000000000000000000, 0.8509844523289342710, 1.000000000000000000),
 ( 1.000000000000000000, 0.8505593500240633542, 1.000000000000000000),
 ( 1.000000000000000000, 0.8498310943761082648, 1.000000000000000000),
 ( 1.000000000000000000, 0.8495301021900780736, 1.000000000000000000),
 ( 1.000000000000000000, 0.8494575155450423409, 1.000000000000000000),
 ( 1.000000000000000000, 0.8507364992962466177, 1.000000000000000000),
 ( 1.000000000000000000, 0.8509629433892478279, 1.000000000000000000) ) ) 
 REPRESENTATION_ITEM ( '' )  SURFACE ( )  );
#50650 = CARTESIAN_POINT ( 'NONE',  ( 3.018661757337009810, 6.673522483535157868, 0.000000000000000000 ) ) ;
#50651 = CARTESIAN_POINT ( 'NONE',  ( 7.038091139269835317, 7.383730215335837954, 0.000000000000000000 ) ) ;
#50652 = ORIENTED_EDGE ( 'NONE', *, *, #212049, .F. ) ;
#50654 = CARTESIAN_POINT ( 'NONE',  ( 0.6803381722274345345, 0.9942335676262317179, 1.750384451323853785 ) ) ;
#50653 = CARTESIAN_POINT ( 'NONE',  ( 4.352959896991869471, 0.3989296284454147412, -1.797357466088687961 ) ) ;
#50655 = CARTESIAN_POINT ( 'NONE',  ( 2.741952636841408442, -2.198962954702073702, -0.6686182857488265352 ) ) ;
#50657 = CARTESIAN_POINT ( 'NONE',  ( 0.6724161089360582988, 1.288989887148813018, -1.342485977130857711 ) ) ;
#50656 = CARTESIAN_POINT ( 'NONE',  ( -3.054546515950523400, 6.451825606165701998, 0.6676900015689657408 ) ) ;
#50658 = CARTESIAN_POINT ( 'NONE',  ( 1.737500000000001155, -0.2333333333333319215, 3.009438278150922130 ) ) ;
#50659 = CARTESIAN_POINT ( 'NONE',  ( -3.952365473583647315, 4.569846793057691592, 1.199719254218462483 ) ) ;
#50660 = CARTESIAN_POINT ( 'NONE',  ( 6.938893903907228378E-15, 10.64264068711930733, 1.214306433183764966E-14 ) ) ;
#50661 = CARTESIAN_POINT ( 'NONE',  ( 4.640819915729988310, 1.831716588661407963, 0.5496940206762624959 ) ) ;
#50662 = CARTESIAN_POINT ( 'NONE',  ( -9.820183334999905256, 10.35130206712171130, 1.040834085586084257E-14 ) ) ;
#50663 = EDGE_CURVE ( 'NONE', #109724, #24478, #201765, .T. ) ;
#50664 = CARTESIAN_POINT ( 'NONE',  ( -7.105881907338178038, 7.462819444748888920, -0.7216878364870338292 ) ) ;
#50666 = CARTESIAN_POINT ( 'NONE',  ( 2.113927203836548419, -0.8795192785214582809, -1.650985937663045577 ) ) ;
#50665 = CARTESIAN_POINT ( 'NONE',  ( 3.843375017719421916, 0.7025675959630849343, -1.969317001441653670 ) ) ;
#50667 = CARTESIAN_POINT ( 'NONE',  ( 8.120970824905713314, 8.576813505252564696, 1.040834085586084257E-14 ) ) ;
#50668 = CARTESIAN_POINT ( 'NONE',  ( 1.364683531249990311, 5.176041667008085767, 0.7879004041258499402 ) ) ;
#50669 = CARTESIAN_POINT ( 'NONE',  ( 5.565905774130330386, -1.163279849954502287, 1.427249551226833502 ) ) ;
#50670 = CARTESIAN_POINT ( 'NONE',  ( 4.708759422647839976, 4.387974169377582001, -0.7998128361456211532 ) ) ;
#50671 = CARTESIAN_POINT ( 'NONE',  ( -6.724721492623500829, -6.244189044378177122, -7.341412881700118298 ) ) ;
#50672 = CARTESIAN_POINT ( 'NONE',  ( 4.371539443043367612, 1.672179000890521516, -0.4225743650863537648 ) ) ;
#50673 = CARTESIAN_POINT ( 'NONE',  ( -5.879432169820529630, 10.01108796476595764, -0.7998128361456221525 ) ) ;
#50674 = CARTESIAN_POINT ( 'NONE',  ( 6.428370569364434850, 1.274405893209800356, -1.801548588985131039 ) ) ;
#50675 = CARTESIAN_POINT ( 'NONE',  ( 1.500000000000001332, 8.625000000000000000, 0.000000000000000000 ) ) ;
#50676 = CIRCLE ( 'NONE', #123304, 1.850000000000000089 ) ;
#50677 = CARTESIAN_POINT ( 'NONE',  ( 9.578659721986364062, -9.971093151297267809, -0.1384029864567958568 ) ) ;
#50678 = CARTESIAN_POINT ( 'NONE',  ( 4.909118719746323301, -1.747747579089290237, 1.287847701716714255 ) ) ;
#50679 = CARTESIAN_POINT ( 'NONE',  ( 3.756323439517950558, 0.6585720284536450420, 1.702948436616057881 ) ) ;
#50680 = CARTESIAN_POINT ( 'NONE',  ( 1.270277045833507312, -0.8771146801004360283, -1.754798696806989078 ) ) ;
#50681 = CARTESIAN_POINT ( 'NONE',  ( 5.225823379661913570, 0.8554599082026111967, -1.936989086107894664 ) ) ;
#50682 = ORIENTED_EDGE ( 'NONE', *, *, #89522, .F. ) ;
#50684 = CARTESIAN_POINT ( 'NONE',  ( -1.201851678989727383E-14, 3.384375000341421469, 1.575800808251672791 ) ) ;
#50683 = CARTESIAN_POINT ( 'NONE',  ( 6.462434034201492317, -2.093801447487374734, -0.9336288876484639676 ) ) ;
#50685 = CARTESIAN_POINT ( 'NONE',  ( 10.07778825365955733, 10.65184113889131012, -0.7998128361456281477 ) ) ;
#50686 = CARTESIAN_POINT ( 'NONE',  ( 1.489100733002651555, -2.014586327357254181, -0.6619970261998938676 ) ) ;
#50687 = CARTESIAN_POINT ( 'NONE',  ( -3.782361668532609134, 7.356579680022602652, 1.040834085586084257E-14 ) ) ;
#50688 = CARTESIAN_POINT ( 'NONE',  ( 0.000000000000000000, 0.5000000000000004441, 0.000000000000000000 ) ) ;
#50689 = CARTESIAN_POINT ( 'NONE',  ( -4.568734577680894304, 5.392907097791561633, -1.082531754730543971 ) ) ;
#50690 = EDGE_CURVE ( 'NONE', #33202, #84740, #25085, .T. ) ;
#50691 = CARTESIAN_POINT ( 'NONE',  ( 6.526262532640958902, 1.108799689610693751, 1.866440817598405966 ) ) ;
#50693 = CARTESIAN_POINT ( 'NONE',  ( -1.500000000000015099, 12.51041666734946212, -0.8660254037844309360 ) ) ;
#50692 = CARTESIAN_POINT ( 'NONE',  ( 6.983263157960330147, 2.017328405816510628, 2.456467998350126525 ) ) ;
#50695 = ORIENTED_EDGE ( 'NONE', *, *, #60337, .F. ) ;
#50694 = CARTESIAN_POINT ( 'NONE',  ( 2.526306204038858194, -2.196730012672935661, 0.3287970392919815632 ) ) ;
#50696 = CARTESIAN_POINT ( 'NONE',  ( 6.399064592084179992, -0.9530083391863402031, -1.777013033299412292 ) ) ;
#50698 = CARTESIAN_POINT ( 'NONE',  ( 4.452046733557501135, -0.7940950990443145230, 1.903769949380555770 ) ) ;
#50697 = CARTESIAN_POINT ( 'NONE',  ( 5.495132332240461714, 5.305409230568988832, 0.7998128361456341429 ) ) ;
#50700 = CARTESIAN_POINT ( 'NONE',  ( 3.475000000000000533, -3.645833333333333037, -2.006292185433951047 ) ) ;
#50699 = CARTESIAN_POINT ( 'NONE',  ( 6.587282531393223728, 8.778525268082516320, 1.599625672291268286 ) ) ;
#50701 = CARTESIAN_POINT ( 'NONE',  ( 6.873057527484919937, 6.983264968346048818, 0.7998128361456352531 ) ) ;
#50702 = CARTESIAN_POINT ( 'NONE',  ( -1.642778471874998480, -3.638541666188710444, 2.845375778867863303 ) ) ;
#50703 = CARTESIAN_POINT ( 'NONE',  ( 0.1331565106231606399, 5.723858289613107608, -2.539976893513963052 ) ) ;
#50704 = CARTESIAN_POINT ( 'NONE',  ( 0.8672654471616656480, 2.014311826519481929, -0.5594637955527237416 ) ) ;
#50705 = CARTESIAN_POINT ( 'NONE',  ( 4.395157833011634096, -0.8647231026696032830, -1.821742675176166060 ) ) ;
#50706 = CARTESIAN_POINT ( 'NONE',  ( 4.054132754448328768, -1.361571661076573792, 1.239656203754435193 ) ) ;
#50707 = CARTESIAN_POINT ( 'NONE',  ( 5.840865249388943248, 5.708764300575555062, 0.7998128361456341429 ) ) ;
#50708 = CARTESIAN_POINT ( 'NONE',  ( 2.098289149679245735, -0.4564329974444079618, -1.663208130003128948 ) ) ;
#50709 = CARTESIAN_POINT ( 'NONE',  ( 0.5851731681005939434, 1.651346252830317551, 1.157095189655330092 ) ) ;
#50710 = CARTESIAN_POINT ( 'NONE',  ( 2.356409458221408126, 0.1091249688820790792, -2.296199191736052025 ) ) ;
#50711 = CARTESIAN_POINT ( 'NONE',  ( -5.982172092127739482, 8.002286745614243912, -1.599625672291263179 ) ) ;
#50712 = CARTESIAN_POINT ( 'NONE',  ( 1.511376755312091591, 1.995097771225157635, 1.066857341152693373 ) ) ;
#50713 = CARTESIAN_POINT ( 'NONE',  ( 4.371769818753069359, 2.042916674203521854, -0.5113404140953855537 ) ) ;
#50714 = CARTESIAN_POINT ( 'NONE',  ( -5.984998465789844069, 5.947196063035064206, 0.7998128361456281477 ) ) ;
#50715 = CARTESIAN_POINT ( 'NONE',  ( 6.124532705071213279, 8.168374127381657246, -1.599625672291262513 ) ) ;
#50716 = CARTESIAN_POINT ( 'NONE',  ( 4.787437638956922648, 6.678706226906775179, -1.443375672974068769 ) ) ;
#50717 = B_SPLINE_CURVE_WITH_KNOTS ( 'NONE', 3,
 ( #51103, #132395, #169110, #147551, #213573, #117228, #183226, #150753, #85729, #2315 ),
 .UNSPECIFIED., .F., .F.,
 ( 4, 2, 2, 2, 4 ),
 ( 0.000000000000000000, 0.0002216178067634642641, 0.0004432356135269285282, 0.0006648534202903928466, 0.0008864712270538553218 ),
 .UNSPECIFIED. ) ;
#50718 = CARTESIAN_POINT ( 'NONE',  ( 6.739650031034449817, -0.2601230917362121753, 2.000000000000034639 ) ) ;
#50719 = CARTESIAN_POINT ( 'NONE',  ( -5.494078562035765501, 7.432844293840273231, -1.599625672291256295 ) ) ;
#50720 = CARTESIAN_POINT ( 'NONE',  ( -1.201851678989727383E-14, 1.712500000000019229, 1.732050807568877637 ) ) ;
#50721 = CARTESIAN_POINT ( 'NONE',  ( -4.273844736805832767, 6.009238164405336313, 1.599625672291267398 ) ) ;
#50722 = CARTESIAN_POINT ( 'NONE',  ( 5.379204547434111028, -2.008251482569714419, -0.9497353344293004707 ) ) ;
#50723 = CARTESIAN_POINT ( 'NONE',  ( 3.345827479060593301, 2.191629467292684819, -0.0001215010576177677764 ) ) ;
#50724 = CARTESIAN_POINT ( 'NONE',  ( -5.168682875307782254, 7.053215992657626110, -1.599625672291256295 ) ) ;
#50725 = CARTESIAN_POINT ( 'NONE',  ( -11.97929049433705373, 9.719999999999998863, 0.7046979865771804130 ) ) ;
#50726 = CARTESIAN_POINT ( 'NONE',  ( -1.201851678989727383E-14, 3.321875000341421025, 1.575800808251672791 ) ) ;
#50727 = CARTESIAN_POINT ( 'NONE',  ( 6.889999999999967706, 3.707772630975701311, 2.234475054783117809 ) ) ;
#50728 = CARTESIAN_POINT ( 'NONE',  ( -4.121315508874262790, 6.791656612786516334, -1.082531754730549967 ) ) ;
#50729 = CARTESIAN_POINT ( 'NONE',  ( 5.836213162209912930, -1.179542664122106510, -1.762073437084572314 ) ) ;
#50730 = CARTESIAN_POINT ( 'NONE',  ( -7.431277594066160397, 7.842447745931541370, -0.7216878364870338292 ) ) ;
#50731 = ORIENTED_EDGE ( 'NONE', *, *, #78129, .F. ) ;
#50733 = CARTESIAN_POINT ( 'NONE',  ( 6.526263005029544928, 1.249015235541932167, -1.764162671312206498 ) ) ;
#50732 = CARTESIAN_POINT ( 'NONE',  ( -5.641601317062247212, 7.675230518029648508, -1.443375672974066548 ) ) ;
#50734 = CARTESIAN_POINT ( 'NONE',  ( 4.547870462380197765, 7.393267075163835855, 1.199719254218462483 ) ) ;
#50735 = CARTESIAN_POINT ( 'NONE',  ( 6.532758020889952277, -1.641319963461195464, 0.8346263169811756200 ) ) ;
#50736 = SURFACE_STYLE_FILL_AREA ( #36612 ) ;
#50737 = CARTESIAN_POINT ( 'NONE',  ( -0.6823417656250212460, 2.613541667008084879, 1.181850606188767472 ) ) ;
#50738 = CARTESIAN_POINT ( 'NONE',  ( 0.7139227764019463462, 1.607345104371117772, 0.6680024673673248259 ) ) ;
#50739 = CARTESIAN_POINT ( 'NONE',  ( 2.198393463710220264, 5.716542807637226886, 0.7998128361456462443 ) ) ;
#50740 = CARTESIAN_POINT ( 'NONE',  ( -0.7500000000000179856, 11.32291666734946212, 1.299038105676658228 ) ) ;
#50741 = CARTESIAN_POINT ( 'NONE',  ( 1.364683531249988757, 0.1968750003414204697, 0.000000000000000000 ) ) ;
#50742 = CARTESIAN_POINT ( 'NONE',  ( 0.000000000000000000, -4.500000000000003553, 2.000000000000000000 ) ) ;
#50743 = CARTESIAN_POINT ( 'NONE',  ( 4.979442225389012933, 2.018306902694905425, -0.7746836383674888804 ) ) ;
#50744 = CARTESIAN_POINT ( 'NONE',  ( -3.297657676621885692, 4.870353260857385180, 1.599625672291267398 ) ) ;
#50745 = CARTESIAN_POINT ( 'NONE',  ( -6.304178240230145391, 9.338329799368375816, 1.082531754730548412 ) ) ;
#50746 = CARTESIAN_POINT ( 'NONE',  ( 4.873979933848565871, 1.241796773192262116, 1.769252301715443565 ) ) ;
#50747 = VERTEX_POINT ( 'NONE', #155037 ) ;
#50748 = CARTESIAN_POINT ( 'NONE',  ( -0.6823417656250003738, 2.967708333674754062, -1.181850606188749264 ) ) ;
#50749 = CARTESIAN_POINT ( 'NONE',  ( 6.134049847598044281, 0.9739642658876453973, -1.713909437456696105 ) ) ;
#50750 = CARTESIAN_POINT ( 'NONE',  ( 4.780456778825039166, -1.700172319169111157, 0.3389010404759411621 ) ) ;
#50752 = CARTESIAN_POINT ( 'NONE',  ( 2.296645709751913955, 1.758124065145909798, -1.308193547052277861 ) ) ;
#50751 = CARTESIAN_POINT ( 'NONE',  ( -10.50000000000003730, 11.00843159320399955, -3.600000000000042277 ) ) ;
#50753 = CARTESIAN_POINT ( 'NONE',  ( 2.556097155687846900, 0.6156694008866661072, -2.223864192518353544 ) ) ;
#50754 = CARTESIAN_POINT ( 'NONE',  ( 4.569639033146696505, 1.999850647628642175, -0.4969485059727016263 ) ) ;
#50755 = CARTESIAN_POINT ( 'NONE',  ( 0.5857530202744161141, -1.927162159831939503, -0.2386530530817491391 ) ) ;
#50756 = CARTESIAN_POINT ( 'NONE',  ( -7.849807752188049825, 8.260456587081938196, 0.7216878364870578100 ) ) ;
#50757 = CARTESIAN_POINT ( 'NONE',  ( -5.164730172163054966, 4.990216387137135889, -0.7998128361456362523 ) ) ;
#50758 = CARTESIAN_POINT ( 'NONE',  ( 8.326672684688675286E-17, 3.599999999999999201, -1.500000000000005107 ) ) ;
#50759 = CARTESIAN_POINT ( 'NONE',  ( 3.445663904809421307, -1.957918079443463855, 0.8150281543025169606 ) ) ;
#50760 = CARTESIAN_POINT ( 'NONE',  ( 1.336564801266389990, 0.5826540126645517459, -1.930418273149013153 ) ) ;
#50761 = CARTESIAN_POINT ( 'NONE',  ( -5.368665640887164692, 9.207267647769599606, 0.000000000000000000 ) ) ;
#50762 = CARTESIAN_POINT ( 'NONE',  ( 4.419099417909471583, 2.016199240759775524, 0.8975180220924662278 ) ) ;
#50763 = CARTESIAN_POINT ( 'NONE',  ( -1.642778471875000035, -1.305208332855377407, -2.845375778867859751 ) ) ;
#50764 = B_SPLINE_CURVE_WITH_KNOTS ( 'NONE', 3,
 ( #91620, #41800, #23365, #18299, #155529, #6040, #120972, #157671, #72111, #105742, #206392, #170696, #54823, #107913, #138220, #55885 ),
 .UNSPECIFIED., .F., .F.,
 ( 4, 3, 3, 3, 3, 4 ),
 ( 0.000000000000000000, 2.533473342638976539E-05, 5.061406379858726976E-05, 7.673069672129158672E-05, 0.0001048028779199228796, 0.0001300696341146173867 ),
 .UNSPECIFIED. ) ;
#50765 = CARTESIAN_POINT ( 'NONE',  ( 1.955673630663162132, -0.6329532555123269510, 1.750116298748620958 ) ) ;
#50766 = CARTESIAN_POINT ( 'NONE',  ( 3.475000000000000533, -1.852083332377418401, -2.006292185433951047 ) ) ;
#50767 = DIRECTION ( 'NONE',  ( 0.000000000000000000, 0.000000000000000000, 1.000000000000000000 ) ) ;
#50768 = CARTESIAN_POINT ( 'NONE',  ( 4.057816120971201812, 3.809087209364407478, -2.500000000000000888 ) ) ;
#50771 = CIRCLE ( 'NONE', #99170, 0.08000000000000025147 ) ;
#50770 = CARTESIAN_POINT ( 'NONE',  ( 6.825078400183546279, 2.419143596098617621, 2.525240329153962904 ) ) ;
#50769 = CARTESIAN_POINT ( 'NONE',  ( -5.031572470839103417, 8.001347149079229837, -1.166850223539055875 ) ) ;
#50772 = CARTESIAN_POINT ( 'NONE',  ( 1.446373960595475516, 8.704174803020480411, -2.603708784378553354 ) ) ;
#50773 = ORIENTED_EDGE ( 'NONE', *, *, #133776, .T. ) ;
#50774 = CARTESIAN_POINT ( 'NONE',  ( 3.854412985283267368, 0.7401793164230722200, 1.923571582979522798 ) ) ;
#50775 = CARTESIAN_POINT ( 'NONE',  ( 0.6801582343749970061, 2.223958333674731946, 1.178068619123799898 ) ) ;
#50776 = CARTESIAN_POINT ( 'NONE',  ( -4.557512192488103686, 8.468847991211438497, -0.7998128361456281477 ) ) ;
#50777 = CARTESIAN_POINT ( 'NONE',  ( 3.404948832191158736, -0.3961486058311721736, -1.980257767865372109 ) ) ;
#50778 = CARTESIAN_POINT ( 'NONE',  ( -1.500000000000013101, -0.3291666666666463459, 0.8660254037844403729 ) ) ;
#50779 = CARTESIAN_POINT ( 'NONE',  ( 4.356247428692526569, 3.976710176429713250, 0.7998128361456341429 ) ) ;
#50780 = CARTESIAN_POINT ( 'NONE',  ( 1.657177242756900926, -1.767118338917167852, -1.060216354352721435 ) ) ;
#50782 = CARTESIAN_POINT ( 'NONE',  ( -8.012344526598182026E-15, 13.29687500034140157, -1.575800808251669460 ) ) ;
#50781 = CARTESIAN_POINT ( 'NONE',  ( 6.983263157960363010, -0.003310164959547157865, 1.953544951557646403 ) ) ;
#50783 = CARTESIAN_POINT ( 'NONE',  ( 4.482942347612929979, 8.381849838857084123, 1.040834085586084257E-14 ) ) ;
#50784 = CARTESIAN_POINT ( 'NONE',  ( -0.1409997244346088141, 2.874455162768466909, -2.488748179275114492 ) ) ;
#50785 = CARTESIAN_POINT ( 'NONE',  ( 1.130510352786683326, -1.665311210022573540, 0.7854980884962547982 ) ) ;
#50786 = CARTESIAN_POINT ( 'NONE',  ( 5.619807753665406302, -2.153844256707802440, 0.4802137346974973409 ) ) ;
#50787 = CARTESIAN_POINT ( 'NONE',  ( 4.688087255275310561, 8.691461907788344377, -0.7998128361456381397 ) ) ;
#50788 = CARTESIAN_POINT ( 'NONE',  ( 1.440939128517594758, 0.4201678954103040819, 2.120193794684998245 ) ) ;
#50789 = CARTESIAN_POINT ( 'NONE',  ( -3.253593677599670109, 5.779314476299451719, 1.082531754730560403 ) ) ;
#50790 = CARTESIAN_POINT ( 'NONE',  ( 2.448454179885679149, -1.387098808145654560, 1.463928423225707931 ) ) ;
#50791 = CARTESIAN_POINT ( 'NONE',  ( 2.056460162951703197, 1.999754300726686029, -1.132793482217157033 ) ) ;
#50792 = ADVANCED_FACE ( 'NONE', ( #139872 ), #153973, .F. ) ;
#50793 =( GEOMETRIC_REPRESENTATION_CONTEXT ( 3 ) GLOBAL_UNCERTAINTY_ASSIGNED_CONTEXT ( ( #87799 ) ) GLOBAL_UNIT_ASSIGNED_CONTEXT ( ( #61778, #161422, #205502 ) ) REPRESENTATION_CONTEXT ( 'NONE', 'WORKASPACE' ) );
#50794 = CARTESIAN_POINT ( 'NONE',  ( -0.4421197159228375528, 6.952754122461416664, 3.903672163281833640 ) ) ;
#50795 = CARTESIAN_POINT ( 'NONE',  ( 2.969872605471563176, 6.610416373784151034, 0.02023234969686484030 ) ) ;
#50796 = CARTESIAN_POINT ( 'NONE',  ( 4.961777154302105863, 1.950117994852887282, -0.2885197095366370257 ) ) ;
#50797 = STYLED_ITEM ( 'NONE', ( #148191 ), #197936 ) ;
#50798 = CARTESIAN_POINT ( 'NONE',  ( 3.643767777461913493, 2.000731686840724333, -0.2516315899964287617 ) ) ;
#50800 = CARTESIAN_POINT ( 'NONE',  ( 9.449669878600614581, 12.04770082983265844, -1.443375672974058777 ) ) ;
#50799 = CARTESIAN_POINT ( 'NONE',  ( -0.6823417656250212460, 1.801041667008083991, 1.181850606188755259 ) ) ;
#50802 = CARTESIAN_POINT ( 'NONE',  ( 6.709622069694824553, -0.4604308047033068840, 2.062537096560501659 ) ) ;
#50801 = CARTESIAN_POINT ( 'NONE',  ( -7.497822643557261024, 8.706213491360317747, -1.199719254218446718 ) ) ;
#50803 = CARTESIAN_POINT ( 'NONE',  ( 5.195788487752976081, -1.461605715988937515, -1.466586839339318882 ) ) ;
#50804 = CARTESIAN_POINT ( 'NONE',  ( 5.957918438201454059, 9.038323046955323292, -1.199719254218440723 ) ) ;
#50805 = CARTESIAN_POINT ( 'NONE',  ( -7.335124800193271177, 8.516399340768996851, -1.199719254218452935 ) ) ;
#50806 = CARTESIAN_POINT ( 'NONE',  ( 6.539320575229251808, 7.629137130509035636, 2.603262396134010892 ) ) ;
#50807 = CARTESIAN_POINT ( 'NONE',  ( 5.027605771429075610, -0.2921156310390393140, 1.998402611621821423 ) ) ;
#50808 = CARTESIAN_POINT ( 'NONE',  ( 1.499999999999987121, -0.7145833326505161009, 0.8660254037844524744 ) ) ;
#50809 = ADVANCED_FACE ( 'NONE', ( #142018 ), #4281, .T. ) ;
#50810 = CARTESIAN_POINT ( 'NONE',  ( 0.3915631436273382948, -1.887207296038289961, 0.8326094146433449250 ) ) ;
#50811 = CARTESIAN_POINT ( 'NONE',  ( 9.422553571817644524, 10.09532670998316384, 0.000000000000000000 ) ) ;
#50812 = CARTESIAN_POINT ( 'NONE',  ( 5.936491157937257235, 8.019268665717216749, 1.599625672291268286 ) ) ;
#50813 = CARTESIAN_POINT ( 'NONE',  ( 6.561219994370630637, 6.619454513046008515, 0.000000000000000000 ) ) ;
#50814 = CARTESIAN_POINT ( 'NONE',  ( -0.6823417656250246877, 0.6135416670080897639, 1.181850606188755259 ) ) ;
#50816 = CARTESIAN_POINT ( 'NONE',  ( 6.827182134110161726, 7.629137130509067610, 2.310944104600751281 ) ) ;
#50815 = CARTESIAN_POINT ( 'NONE',  ( 4.203910148689107729, 7.062256385849379647, -1.199719254218448494 ) ) ;
#50817 = CARTESIAN_POINT ( 'NONE',  ( 7.280365300414074703, 7.596107060012304402, -0.7216878364870257245 ) ) ;
#50819 = CARTESIAN_POINT ( 'NONE',  ( 11.35605497252127449, 12.48581854048353001, 3.553547709190206572 ) ) ;
#50818 = CARTESIAN_POINT ( 'NONE',  ( 2.664704904736223234, -0.8290184881076659851, -2.006861667775594160 ) ) ;
#50820 = CARTESIAN_POINT ( 'NONE',  ( -2.768263461985202234, -0.8887487162373161054, -1.782739746934519198 ) ) ;
#50822 = CARTESIAN_POINT ( 'NONE',  ( 3.069684041021227827, -1.094477399149307306, 1.480508570315848482 ) ) ;
#50821 = CARTESIAN_POINT ( 'NONE',  ( -4.284013352238262407, 6.021101549076499637, -1.443375672974053447 ) ) ;
#50823 = CARTESIAN_POINT ( 'NONE',  ( -1.001543065824772872E-14, 5.321875000341422357, 1.575800808251672791 ) ) ;
#50824 = CARTESIAN_POINT ( 'NONE',  ( 4.862908538974716421, 0.2148362657848035262, -2.180980218048253150 ) ) ;
#50825 = CARTESIAN_POINT ( 'NONE',  ( 1.396097351027982424E-15, 0.000000000000000000, -11.29999999999999893 ) ) ;
#50826 = CARTESIAN_POINT ( 'NONE',  ( 4.645576076348203465, -1.746196445045271606, -1.438666788099978389 ) ) ;
#50827 = CARTESIAN_POINT ( 'NONE',  ( -4.069418662396130593, 7.899405539437467816, -0.7998128361456281477 ) ) ;
#50828 = CARTESIAN_POINT ( 'NONE',  ( -5.703190497605960196, 6.276721696052339539, -1.111643793752248754 ) ) ;
#50829 = CARTESIAN_POINT ( 'NONE',  ( 5.348725299209624140, 7.591689785053232775, -1.238827213252717163 ) ) ;
#50830 = CARTESIAN_POINT ( 'NONE',  ( -5.709392084686210289, 8.714688961225625974, 1.082531754730550855 ) ) ;
#50831 = CARTESIAN_POINT ( 'NONE',  ( 4.204437034013637664, 6.958908068774287692, -1.082531754730548412 ) ) ;
#50832 = CARTESIAN_POINT ( 'NONE',  ( 6.661408102931688724, 0.2994711133218473931, -1.744046391327475964 ) ) ;
#50833 = AXIS2_PLACEMENT_3D ( 'NONE', #188080, #205393, #123198 ) ;
#50834 = CARTESIAN_POINT ( 'NONE',  ( 3.633450831153079541, -0.1460068579729571769, 2.007839618615501642 ) ) ;
#50835 = CARTESIAN_POINT ( 'NONE',  ( 8.281332899848809603, 8.555976559445431562, 0.7998128361456481317 ) ) ;
#50836 = CARTESIAN_POINT ( 'NONE',  ( 2.555815334374893943, 0.5629295958425766244, -2.029244372067032565 ) ) ;
#50837 = CARTESIAN_POINT ( 'NONE',  ( 1.054133004535224849, -1.214278006866207571, 1.481595424536867656 ) ) ;
#50840 = EDGE_CURVE ( 'NONE', #97926, #7066, #13441, .T. ) ;
#50839 = CARTESIAN_POINT ( 'NONE',  ( -0.7500000000000215383, 2.691666666666689522, 1.299038105676671107 ) ) ;
#50838 = CARTESIAN_POINT ( 'NONE',  ( 0.6823417656249969321, 12.02604166700806054, -1.181850606188757036 ) ) ;
#50841 = CARTESIAN_POINT ( 'NONE',  ( 2.225000061332568890, -1.799552404990023113, -0.8009105870329900068 ) ) ;
#50842 = CARTESIAN_POINT ( 'NONE',  ( 0.3033014811697418711, -0.5033704626738467747, 1.801585485020948951 ) ) ;
#50843 = CARTESIAN_POINT ( 'NONE',  ( 1.029656018189710309, 1.891699080040713410, -0.5197978237033785698 ) ) ;
#50845 = VERTEX_POINT ( 'NONE', #24530 ) ;
#50844 = CARTESIAN_POINT ( 'NONE',  ( 6.539320575229251808, 0.01001626003939220556, 1.796977979958065852 ) ) ;
#50846 = CARTESIAN_POINT ( 'NONE',  ( 4.189106276942576201, 7.831115056500907556, 1.040834085586084257E-14 ) ) ;
#50847 = STYLED_ITEM ( 'NONE', ( #213253 ), #150547 ) ;
#50848 = CARTESIAN_POINT ( 'NONE',  ( 1.364683531249988757, 0.1968750003414204697, 0.000000000000000000 ) ) ;
#50849 = CARTESIAN_POINT ( 'NONE',  ( 6.086763352761943580, -0.2763008855245497331, -1.850001521387992565 ) ) ;
#50850 = CARTESIAN_POINT ( 'NONE',  ( 10.16199982864259788, 11.81442020729326536, 1.199719254218452047 ) ) ;
#50851 = DIRECTION ( 'NONE',  ( 0.000000000000000000, -1.000000000000000000, -0.000000000000000000 ) ) ;
#50852 = CARTESIAN_POINT ( 'NONE',  ( 6.561392567526037389, 1.717850402480676664, 1.155108059606273052 ) ) ;
#50853 = FACE_OUTER_BOUND ( 'NONE', #163849, .T. ) ;
#50854 = CARTESIAN_POINT ( 'NONE',  ( 2.486770427477404954, 2.630042260599927850, -11.73951962969540119 ) ) ;
#50855 = CARTESIAN_POINT ( 'NONE',  ( -0.7500000000000215383, 0.9416666666666878571, 1.299038105676659116 ) ) ;
#50856 = CARTESIAN_POINT ( 'NONE',  ( 5.913327553854682783, 10.05063257947248800, -0.7998128361456291469 ) ) ;
#50857 = CARTESIAN_POINT ( 'NONE',  ( -6.665805079413154921, 10.92852302595736447, 0.7998128361456481317 ) ) ;
#50858 = CARTESIAN_POINT ( 'NONE',  ( 7.178115983792402233, 7.339166500704784823, 0.7998128361456281477 ) ) ;
#50859 = EDGE_CURVE ( 'NONE', #192662, #6739, #210530, .T. ) ;
#50860 = CARTESIAN_POINT ( 'NONE',  ( 1.364683531249988757, 0.8843750003414210248, 0.000000000000000000 ) ) ;
#50861 = VECTOR ( 'NONE', #52059, 1000.000000000000114 ) ;
#50862 = EDGE_CURVE ( 'NONE', #148041, #105242, #87253, .T. ) ;
#50863 = CARTESIAN_POINT ( 'NONE',  ( -1.499999999999997780, 2.150000000000019895, 1.214306433183764966E-14 ) ) ;
#50865 = CARTESIAN_POINT ( 'NONE',  ( 4.090809663021327758, 5.795697244990093644, 1.599625672291267398 ) ) ;
#50864 = CARTESIAN_POINT ( 'NONE',  ( 5.758247127753066685, -1.962046631956643195, -0.001586170976335121285 ) ) ;
#50866 = CARTESIAN_POINT ( 'NONE',  ( 2.987657498945671453, 1.897406709466815444, 0.6818930838706840358 ) ) ;
#50867 = CARTESIAN_POINT ( 'NONE',  ( 3.380013747803870316, -1.913774515330651127, -0.08860483629866824917 ) ) ;
#50868 = FACE_OUTER_BOUND ( 'NONE', #162815, .T. ) ;
#50869 = CARTESIAN_POINT ( 'NONE',  ( 1.997856853652695497, -2.190977152517746163, 0.05759783203293508680 ) ) ;
#50870 = CARTESIAN_POINT ( 'NONE',  ( 0.1333692844072802142, 0.2389375359408679178, -2.087895146362698906 ) ) ;
#50871 = CARTESIAN_POINT ( 'NONE',  ( 2.881944908259078453, -0.9649329312324153030, 1.602325162460143559 ) ) ;
#50872 = CARTESIAN_POINT ( 'NONE',  ( -0.7500000000000006661, -0.8604166659838472508, -1.299038105676652011 ) ) ;
#50873 = CARTESIAN_POINT ( 'NONE',  ( -8.667740277838301921, 9.006785167099828016, -0.7998128361456291469 ) ) ;
#50875 = CARTESIAN_POINT ( 'NONE',  ( 4.798512230019831293, 1.459014486584905956, -1.534486623482501644 ) ) ;
#50874 = CARTESIAN_POINT ( 'NONE',  ( -3.470524135418300737, 6.032400010421219427, -1.082531754730549967 ) ) ;
#50876 = CARTESIAN_POINT ( 'NONE',  ( 0.6823417656249969321, 8.838541667008065872, -1.181850606188757036 ) ) ;
#50877 = CARTESIAN_POINT ( 'NONE',  ( 6.338344951546218908, -1.110931056888088353, 1.746890944850580052 ) ) ;
#50879 = CARTESIAN_POINT ( 'NONE',  ( 6.620655732516651071, -0.002413161512292844035, 2.173887093218453082 ) ) ;
#50878 = CARTESIAN_POINT ( 'NONE',  ( 2.138330579027637679, 0.4610650599585190967, 2.039099516977191495 ) ) ;
#50881 = ORIENTED_EDGE ( 'NONE', *, *, #87068, .T. ) ;
#50880 = CARTESIAN_POINT ( 'NONE',  ( 0.9555556167152472469, 1.723134239262851475, -0.07815038326265508206 ) ) ;
#50882 = CARTESIAN_POINT ( 'NONE',  ( 5.777746017718023097, 9.892454120646377191, 0.7998128361456462443 ) ) ;
#50883 = DIRECTION ( 'NONE',  ( 0.000000000000000000, 0.7766560405359869135, 0.6299249119529750640 ) ) ;
#50884 = DIRECTION ( 'NONE',  ( -0.000000000000000000, 1.000000000000000000, -0.000000000000000000 ) ) ;
#50885 =( LENGTH_UNIT ( ) NAMED_UNIT ( * ) SI_UNIT ( .MILLI., .METRE. ) );
#50887 = CARTESIAN_POINT ( 'NONE',  ( 7.754900676892376055, 8.149731665903665601, 1.040834085586084257E-14 ) ) ;
#50886 = CARTESIAN_POINT ( 'NONE',  ( 7.983053520348166288, 8.207983950027992748, -0.7998128361456281477 ) ) ;
#50888 = CARTESIAN_POINT ( 'NONE',  ( -0.4735722981419963062, 7.464727232010883284, -4.424040350390532339 ) ) ;
#50890 = CARTESIAN_POINT ( 'NONE',  ( 1.119438638434491429, -0.4408070000805932032, 1.756890142956100576 ) ) ;
#50889 = CARTESIAN_POINT ( 'NONE',  ( 5.481239241674765950, 9.616805891921051952, -0.7998128361456481317 ) ) ;
#50891 = CARTESIAN_POINT ( 'NONE',  ( -5.506582945444718824, 9.576097202994168001, 0.7998128361456481317 ) ) ;
#50892 = CARTESIAN_POINT ( 'NONE',  ( 5.030238685870051185, 5.827365540725222282, -1.199719254218452047 ) ) ;
#50893 = CARTESIAN_POINT ( 'NONE',  ( -6.488192154978348114, 6.766396236290696642, 0.1981293719705672085 ) ) ;
#50894 = CARTESIAN_POINT ( 'NONE',  ( 5.742760583840166966, 8.857581893525663830, 1.199719254218452047 ) ) ;
#50895 = CARTESIAN_POINT ( 'NONE',  ( 6.539320575229234933, 1.301352213286063320, 1.914891792149053140 ) ) ;
#50896 =( NAMED_UNIT ( * ) SI_UNIT ( $, .STERADIAN. ) SOLID_ANGLE_UNIT ( ) );
#50897 = CARTESIAN_POINT ( 'NONE',  ( 4.073938026035560434, 7.494178044256873505, -0.5588469191320240004 ) ) ;
#50898 = CARTESIAN_POINT ( 'NONE',  ( 9.897088948295943212, 11.60932053017587506, 1.082531754730548412 ) ) ;
#50899 = ORIENTED_EDGE ( 'NONE', *, *, #60938, .F. ) ;
#50900 = CARTESIAN_POINT ( 'NONE',  ( 3.103785861066649776, 0.6724651444435655323, -1.735490194124859054 ) ) ;
#50901 = CARTESIAN_POINT ( 'NONE',  ( 0.2103571609669597775, 1.833310535235525673, 0.5554914372104239328 ) ) ;
#50902 = CARTESIAN_POINT ( 'NONE',  ( 0.3641364058636682999, 0.6611385597973111761, -2.014868753213174823 ) ) ;
#50903 = CARTESIAN_POINT ( 'NONE',  ( -1.865214468731750452, 8.973543201141316317, 0.7750000000000013545 ) ) ;
#50904 = CARTESIAN_POINT ( 'NONE',  ( 1.224999999999961231, 1.416666667349490760, 0.7072540797572558491 ) ) ;
#50905 = CARTESIAN_POINT ( 'NONE',  ( -1.555203039002693188, 8.692270211428450466, -2.503634413632307876 ) ) ;
#50906 = CARTESIAN_POINT ( 'NONE',  ( -3.456965981804629884, 6.976951378839947537, 1.040834085586084257E-14 ) ) ;
#50907 = CARTESIAN_POINT ( 'NONE',  ( 9.761507412159302177, 10.49077285704843199, -0.7216878364870257245 ) ) ;
#50908 = CARTESIAN_POINT ( 'NONE',  ( 4.346514977827297344, -1.947402357529237626, -0.2931004117151541633 ) ) ;
#50909 = CARTESIAN_POINT ( 'NONE',  ( 1.858217301831434964, 0.8087058978607818416, -1.960417502992222838 ) ) ;
#50910 = CARTESIAN_POINT ( 'NONE',  ( -6.254388934605767503, 6.191208599995166040, 0.7998128361456341429 ) ) ;
#50911 = CARTESIAN_POINT ( 'NONE',  ( -11.37655908458146037, 7.827155916726787233, -3.682564549178993119 ) ) ;
#50912 = CARTESIAN_POINT ( 'NONE',  ( -3.116716552580018451, 6.446646959060242210, -0.7524088503868963107 ) ) ;
#50913 = CARTESIAN_POINT ( 'NONE',  ( 5.999973295341066937, -0.7855225714627244171, -2.046000194487001433 ) ) ;
#50914 = FACE_OUTER_BOUND ( 'NONE', #41213, .T. ) ;
#50915 = CARTESIAN_POINT ( 'NONE',  ( 4.401339437636656804, 1.546884307994823793, 1.147896415085915667 ) ) ;
#50916 = CARTESIAN_POINT ( 'NONE',  ( -8.182509401047415309, 9.505014708432145909, 1.199719254218462483 ) ) ;
#50917 = CARTESIAN_POINT ( 'NONE',  ( -0.6124999999999984901, 2.354166667349471886, 1.060881119635896264 ) ) ;
#50918 = CARTESIAN_POINT ( 'NONE',  ( 0.8915962724085277902, 1.944627461026976034, -1.043433064090833140 ) ) ;
#50919 = CARTESIAN_POINT ( 'NONE',  ( -0.2802162696003129283, 8.153957901067540703, 2.020850277443522192 ) ) ;
#50920 = ORIENTED_EDGE ( 'NONE', *, *, #4614, .F. ) ;
#50921 = CARTESIAN_POINT ( 'NONE',  ( 2.929970594329034395, 6.432399770110250437, -0.7216878364870338292 ) ) ;
#50922 = ORIENTED_EDGE ( 'NONE', *, *, #80683, .F. ) ;
#50923 = CARTESIAN_POINT ( 'NONE',  ( 5.823099318722479545, -1.778931037738925802, -0.8454068362369684397 ) ) ;
#50924 = CARTESIAN_POINT ( 'NONE',  ( 1.522887052880964598, -1.828065777178315532, 0.6558840488102948285 ) ) ;
#50925 = CIRCLE ( 'NONE', #185715, 0.07999999999999993228 ) ;
#50926 = CARTESIAN_POINT ( 'NONE',  ( 0.1927366488196740335, -1.238295061544148812, -1.591656064170659191 ) ) ;
#50928 = CARTESIAN_POINT ( 'NONE',  ( 4.803460451949028709, -1.436610920757129817, -1.182842806638328526 ) ) ;
#50927 = CARTESIAN_POINT ( 'NONE',  ( -7.306918443122272677, 7.489436036589583345, 0.7998128361456341429 ) ) ;
#50929 = CARTESIAN_POINT ( 'NONE',  ( 5.027041095616958444, 9.086908054853605421, 0.000000000000000000 ) ) ;
#50930 = CARTESIAN_POINT ( 'NONE',  ( 0.000000000000000000, 19.00000000000000000, 0.000000000000000000 ) ) ;
#50931 = CARTESIAN_POINT ( 'NONE',  ( 1.772826578343066117, 3.950000000000009059, 0.4499999999999590994 ) ) ;
#50932 = CARTESIAN_POINT ( 'NONE',  ( -6.230135280679522936, 7.227244901336242755, 1.199719254218450271 ) ) ;
#50933 = ADVANCED_FACE ( 'NONE', ( #44020 ), #8291, .F. ) ;
#50934 = CARTESIAN_POINT ( 'NONE',  ( 6.720655732516647163, 0.5950723047917580999, 1.879543361893110109 ) ) ;
#50935 = CARTESIAN_POINT ( 'NONE',  ( 0.7850416839378616674, 1.930235501049954339, -1.037882601892345713 ) ) ;
#50936 = CARTESIAN_POINT ( 'NONE',  ( 5.680503174445848735, 5.729601246382692636, 1.040834085586084257E-14 ) ) ;
#50937 = CARTESIAN_POINT ( 'NONE',  ( 2.493461049780987260, 3.507114751586604129, -11.73081193161139169 ) ) ;
#50938 = DIRECTION ( 'NONE',  ( 0.000000000000000000, -1.000000000000000000, 0.000000000000000000 ) ) ;
#50939 = CARTESIAN_POINT ( 'NONE',  ( 1.101864800459760207, -1.825872481749410525, -0.002338443969775172437 ) ) ;
#50940 = CARTESIAN_POINT ( 'NONE',  ( -3.438964519360665051, 7.163875705896082913, -0.7998128361456281477 ) ) ;
#50941 = CARTESIAN_POINT ( 'NONE',  ( 3.164447786964882603, 1.103041557463914524, 1.338080049202054145 ) ) ;
#50942 =( NAMED_UNIT ( * ) SI_UNIT ( $, .STERADIAN. ) SOLID_ANGLE_UNIT ( ) );
#50943 = CARTESIAN_POINT ( 'NONE',  ( -0.6125000000000053735, 2.708333333333333481, -1.060881119635955327 ) ) ;
#50944 = CARTESIAN_POINT ( 'NONE',  ( 1.349890321011204986, 8.200329036966268248, -10.79298809153610961 ) ) ;
#50945 = CARTESIAN_POINT ( 'NONE',  ( 0.04732232356348483465, -1.488192626783080952, -1.223051670295220994 ) ) ;
#50946 = CARTESIAN_POINT ( 'NONE',  ( 4.785966450049039089, -1.203721183051874810, -1.548998264137561254 ) ) ;
#50947 = CARTESIAN_POINT ( 'NONE',  ( -6.665805079413154921, 10.92852302595736447, 0.7998128361456481317 ) ) ;
#50948 = CARTESIAN_POINT ( 'NONE',  ( 7.447506452608354088, 7.583179037664891098, 0.7998128361456341429 ) ) ;
#50949 = CARTESIAN_POINT ( 'NONE',  ( 4.371814246616528621, 0.4635510597098577712, -2.069045912693792566 ) ) ;
#50950 = EDGE_CURVE ( 'NONE', #173465, #197280, #165743, .T. ) ;
#50951 = CARTESIAN_POINT ( 'NONE',  ( 7.018280793729500644, 8.217024343219755167, -1.199719254218452047 ) ) ;
#50952 = CARTESIAN_POINT ( 'NONE',  ( -8.616370316684697883, 10.01118577667568132, -1.199719254218446718 ) ) ;
#50953 = CYLINDRICAL_SURFACE ( 'NONE', #163581, 10.99999999999999112 ) ;
#50954 = CARTESIAN_POINT ( 'NONE',  ( 3.010663864534826928, 0.6931938328994196041, 1.950912564768356727 ) ) ;
#50956 = CARTESIAN_POINT ( 'NONE',  ( -1.364683531250012516, 0.5927083336747520637, 0.7879004041258379498 ) ) ;
#50955 = CARTESIAN_POINT ( 'NONE',  ( 3.741289556128908345, 7.428763123923395106, -2.448390356388091327 ) ) ;
#50957 = EDGE_LOOP ( 'NONE', ( #168384, #154276, #152456, #13846, #28642 ) ) ;
#50958 = CARTESIAN_POINT ( 'NONE',  ( 2.532212319380182208, -1.909192193906615209, 1.279991936841210043 ) ) ;
#50959 = CARTESIAN_POINT ( 'NONE',  ( 7.592202833972727660, 11.80139437303613015, -0.7216878364870267237 ) ) ;
#50961 = CARTESIAN_POINT ( 'NONE',  ( -1.642778471875000035, -1.917708332855375897, -2.845375778867859751 ) ) ;
#50960 = CARTESIAN_POINT ( 'NONE',  ( 7.865138509703455405, 8.348618814175074121, -0.7216878364870317197 ) ) ;
#50962 = PRESENTATION_STYLE_ASSIGNMENT (( #202512 ) ) ;
#50963 = SURFACE_STYLE_FILL_AREA ( #86655 ) ;
#50964 = ORIENTED_EDGE ( 'NONE', *, *, #167075, .T. ) ;
#50965 = FACE_BOUND ( 'NONE', #191319, .T. ) ;
#50966 = ADVANCED_FACE ( 'NONE', ( #185601 ), #174524, .T. ) ;
#50967 = CARTESIAN_POINT ( 'NONE',  ( 4.007995338699682719, -0.7271224857151190601, 1.768968726348684406 ) ) ;
#50968 = DIRECTION ( 'NONE',  ( -0.000000000000000000, -1.000000000000000000, -0.000000000000000000 ) ) ;
#50969 = CARTESIAN_POINT ( 'NONE',  ( 5.245002492778637837, -1.477622881800463306, 0.8893561077145789584 ) ) ;
#50970 = CARTESIAN_POINT ( 'NONE',  ( 3.081267818761534105, 1.592661989535900435, 1.236799713577160009 ) ) ;
#50971 = CARTESIAN_POINT ( 'NONE',  ( 4.817139702178411476, 1.183121084409150425, -1.970709701559998805 ) ) ;
#50972 = CARTESIAN_POINT ( 'NONE',  ( 0.000000000000000000, 7.980384757729337863, 0.000000000000000000 ) ) ;
#50973 = CARTESIAN_POINT ( 'NONE',  ( 0.4697016844467936103, 0.2121168557088908557, -2.196667960996725011 ) ) ;
#50974 = CARTESIAN_POINT ( 'NONE',  ( -4.340018570150318666, 6.156717313299049366, -1.443375672974066548 ) ) ;
#50975 = CARTESIAN_POINT ( 'NONE',  ( 6.221911924188020748, -0.9849534058487903199, -1.470084644806458174 ) ) ;
#50977 = CARTESIAN_POINT ( 'NONE',  ( 1.535548486519675571, -1.662869323620078665, -1.577994866025609566 ) ) ;
#50976 = CARTESIAN_POINT ( 'NONE',  ( 6.873057527484919937, 6.983264968346048818, 0.7998128361456352531 ) ) ;
#50978 = CARTESIAN_POINT ( 'NONE',  ( 0.4623611518889169103, 0.1752324854824957590, -1.731468860160074952 ) ) ;
#50979 = B_SPLINE_CURVE_WITH_KNOTS ( 'NONE', 3,
 ( #99693, #17348, #25, #180937, #148455, #1096, #165763, #67157, #83430, #16280 ),
 .UNSPECIFIED., .F., .F.,
 ( 4, 1, 1, 1, 1, 1, 1, 4 ),
 ( 0.000000000000000000, 0.09599525230796020214, 0.1893027314675523320, 0.2592390727089966540, 0.3619855251144610819, 0.5211967264240887632, 0.7336899926499302893, 1.000000000000000000 ),
 .UNSPECIFIED. ) ;
#50980 = CARTESIAN_POINT ( 'NONE',  ( -2.272963308585411735, 5.803540959991587478, 0.7998128361456341429 ) ) ;
#50981 = CARTESIAN_POINT ( 'NONE',  ( 6.562441972333600937, -2.001882313047067985, -0.8919867065708479981 ) ) ;
#50982 = CARTESIAN_POINT ( 'NONE',  ( -5.666381855868691808, 5.575476684793721383, 0.000000000000000000 ) ) ;
#50983 = CARTESIAN_POINT ( 'NONE',  ( 0.6801582343749674742, -0.2447916663252461267, 1.178068619123796568 ) ) ;
#50984 = DIRECTION ( 'NONE',  ( 0.000000000000000000, 0.000000000000000000, -1.000000000000000000 ) ) ;
#50985 = CARTESIAN_POINT ( 'NONE',  ( 6.443811375169310907, 1.424792453395683500, 1.502365266013883538 ) ) ;
#50986 = CARTESIAN_POINT ( 'NONE',  ( 0.6906390985809904848, 1.523792322931913468, -1.320830384837400118 ) ) ;
#50987 = CIRCLE ( 'NONE', #5962, 0.07999999999999971023 ) ;
#50988 = CARTESIAN_POINT ( 'NONE',  ( -0.7500000000000006661, -0.1104166659838465292, -1.299038105676652011 ) ) ;
#50989 = CARTESIAN_POINT ( 'NONE',  ( 5.338475953816137931, 1.898335173771143580, 0.3273637156304096130 ) ) ;
#50990 = CARTESIAN_POINT ( 'NONE',  ( -1.364683531250010295, 11.13020833367473372, 0.7879004041258445001 ) ) ;
#50991 = CARTESIAN_POINT ( 'NONE',  ( 2.197798511016679335, 2.028856164703813025, -0.9050913924920337417 ) ) ;
#50992 = ORIENTED_EDGE ( 'NONE', *, *, #93121, .T. ) ;
#50994 = DIRECTION ( 'NONE',  ( 0.6507913734559640506, -0.7592566023653004592, 0.000000000000000000 ) ) ;
#50993 = CARTESIAN_POINT ( 'NONE',  ( -2.788906526875773208E-15, 12.96875000068279782, -1.499999999999998446 ) ) ;
#50995 = CARTESIAN_POINT ( 'NONE',  ( -4.272227801637582090, 7.998366511970294468, 0.7216878364870059626 ) ) ;
#50996 = CARTESIAN_POINT ( 'NONE',  ( 8.646349277213076334, 11.11049346154719508, 1.599625672291281386 ) ) ;
#50997 = CARTESIAN_POINT ( 'NONE',  ( 7.634649897826744080, 9.040084647953621655, 1.082531754730549078 ) ) ;
#50998 = DIRECTION ( 'NONE',  ( 0.7592566023652990159, -0.6507913734559659380, 1.175982368226361624E-15 ) ) ;
#50999 = CARTESIAN_POINT ( 'NONE',  ( 4.792390001771311248, 1.443284891743993770, -0.9723301709525405956 ) ) ;
#51001 = CARTESIAN_POINT ( 'NONE',  ( 2.295295855072278624, -1.753792786583353580, 0.8793850528211948347 ) ) ;
#51000 = AXIS2_PLACEMENT_3D ( 'NONE', #54317, #104138, #134531 ) ;
#51003 = CARTESIAN_POINT ( 'NONE',  ( -6.060131475628484310, 10.01397778830115470, 0.000000000000000000 ) ) ;
#51002 = CARTESIAN_POINT ( 'NONE',  ( 3.928111819657337911, 5.605883094398769195, 1.599625672291267398 ) ) ;
#51004 = EDGE_CURVE ( 'NONE', #138703, #170885, #106855, .T. ) ;
#51005 = DIRECTION ( 'NONE',  ( 8.881784197001252323E-16, 0.000000000000000000, -1.000000000000000000 ) ) ;
#51006 = CARTESIAN_POINT ( 'NONE',  ( 0.6606829430093235089, -0.6931630328321845003, -1.942862509804524906 ) ) ;
#51007 = CARTESIAN_POINT ( 'NONE',  ( -7.670162217029145246, 9.971608557999250166, 1.599625672291295375 ) ) ;
#51008 = CARTESIAN_POINT ( 'NONE',  ( -4.568734577680899633, 4.432537883490215158, -0.7216878364870207285 ) ) ;
#51009 = CARTESIAN_POINT ( 'NONE',  ( 1.077466299836680630, -0.05792418700063763082, -2.261926406141855583 ) ) ;
#51010 = ORIENTED_EDGE ( 'NONE', *, *, #50541, .F. ) ;
#51011 = CARTESIAN_POINT ( 'NONE',  ( -1.500000000000001332, -0.06874999931718445145, 0.000000000000000000 ) ) ;
#51012 = CARTESIAN_POINT ( 'NONE',  ( 2.108475139129362574, 1.389272611029747750, -1.252756881873963168 ) ) ;
#51013 = CARTESIAN_POINT ( 'NONE',  ( 1.564674090997038025, -0.9275931817575002736, 1.464960531123546961 ) ) ;
#51014 = CARTESIAN_POINT ( 'NONE',  ( 4.985950990042907094, -2.174969566330759996, -0.2684501861200879747 ) ) ;
#51015 = CARTESIAN_POINT ( 'NONE',  ( 5.368347952151684588, 1.131674353116480569, 2.010972138180310065 ) ) ;
#51016 = CARTESIAN_POINT ( 'NONE',  ( 1.323197370116558469, -0.05141181009169673577, 2.060424651611890479 ) ) ;
#51017 = CARTESIAN_POINT ( 'NONE',  ( 3.749888610702892144, 0.6998405808875374223, 1.811630882863373149 ) ) ;
#51018 = CARTESIAN_POINT ( 'NONE',  ( -3.240035523541616502, 6.723865844199768738, 0.7216878364870317197 ) ) ;
#51019 = CARTESIAN_POINT ( 'NONE',  ( 5.589076619078012342, 1.650032040524500143, -0.8810306647013476100 ) ) ;
#51020 = CARTESIAN_POINT ( 'NONE',  ( 1.281250000000000444, 0.7852924748300526003, 1.895863743164061255 ) ) ;
#51021 = CARTESIAN_POINT ( 'NONE',  ( 0.09230638003325472574, 13.28780466659584292, 1.452645848652445171 ) ) ;
#51022 = CARTESIAN_POINT ( 'NONE',  ( 6.538435458278026857, 1.930121188254026787, -0.5825698962980339068 ) ) ;
#51023 = CARTESIAN_POINT ( 'NONE',  ( 4.421367491832282504, 5.291255174293369556, 1.082531754730549078 ) ) ;
#51024 = CARTESIAN_POINT ( 'NONE',  ( 1.360316468749953600, 1.786458333674746601, -0.7853790794159161148 ) ) ;
#51025 = CARTESIAN_POINT ( 'NONE',  ( 4.940077362011475515, -1.704937458037486531, -1.076318853994034930 ) ) ;
#51026 = CARTESIAN_POINT ( 'NONE',  ( -2.589244150085650009, 5.964609241834465614, 0.7216878364870317197 ) ) ;
#51027 = CARTESIAN_POINT ( 'NONE',  ( 7.560643217915098191, 11.97250085420964716, -0.7998128361456291469 ) ) ;
#51028 = CARTESIAN_POINT ( 'NONE',  ( 5.578253857379852576, 5.472660686556754861, -0.7998128361456481317 ) ) ;
#51029 = CARTESIAN_POINT ( 'NONE',  ( 1.980809073483770000, -0.08854697198140694392, -1.823669195971427071 ) ) ;
#51030 = CARTESIAN_POINT ( 'NONE',  ( -5.984998465789844069, 5.947196063035064206, 0.7998128361456281477 ) ) ;
#51031 = CARTESIAN_POINT ( 'NONE',  ( -0.1296875068448137269, 7.629137130509075604, -2.426516348560475045 ) ) ;
#51032 = CARTESIAN_POINT ( 'NONE',  ( -7.591565991045862383, -6.646943093533998592, -7.792125355486802185 ) ) ;
#51033 = EDGE_LOOP ( 'NONE', ( #47336, #166064, #214265, #31989 ) ) ;
#51034 = CARTESIAN_POINT ( 'NONE',  ( -4.936577328707246082, 8.773440960218172435, 0.000000000000000000 ) ) ;
#51035 = CARTESIAN_POINT ( 'NONE',  ( -5.249999999999987566, 0.000000000000000000, 0.5999999999999969802 ) ) ;
#51036 = CARTESIAN_POINT ( 'NONE',  ( -9.806625181386236179, 10.33548422123910449, -0.7998128361456291469 ) ) ;
#51037 = CARTESIAN_POINT ( 'NONE',  ( 6.375650237155517708, 0.3431015828706286408, -1.990142738341105000 ) ) ;
#51039 = VERTEX_POINT ( 'NONE', #187740 ) ;
#51038 = CARTESIAN_POINT ( 'NONE',  ( 6.463560548549353690, -1.782115098378980855, -1.325830300435285825 ) ) ;
#51040 = CARTESIAN_POINT ( 'NONE',  ( -5.413448473606448985, 9.537716662508005427, 0.000000000000000000 ) ) ;
#51041 = CARTESIAN_POINT ( 'NONE',  ( 6.030679399980265920, 5.930214142932100252, -0.7998128361456281477 ) ) ;
#51042 = CARTESIAN_POINT ( 'NONE',  ( 5.735248378139378822, -1.864208485850331609, 0.8789154904798938128 ) ) ;
#51043 = CARTESIAN_POINT ( 'NONE',  ( 4.781875055470904634, 1.674888562130649960, -1.122497055794105414 ) ) ;
#51044 = ORIENTED_EDGE ( 'NONE', *, *, #25664, .T. ) ;
#51045 = ORIENTED_EDGE ( 'NONE', *, *, #58523, .F. ) ;
#51046 = CARTESIAN_POINT ( 'NONE',  ( -3.022498986271275001, 2.800000000000024691, 2.500000000000011102 ) ) ;
#51047 = DIRECTION ( 'NONE',  ( -1.000000000000000000, 0.000000000000000000, 0.000000000000000000 ) ) ;
#51050 = ORIENTED_EDGE ( 'NONE', *, *, #146654, .T. ) ;
#51049 = CARTESIAN_POINT ( 'NONE',  ( -5.717785742877115496, 7.006476535625803415, 2.500000000000000000 ) ) ;
#51048 = CARTESIAN_POINT ( 'NONE',  ( -6.119526231721793330, 8.232809585132461194, 1.599625672291263179 ) ) ;
#51051 = CARTESIAN_POINT ( 'NONE',  ( 4.690754089986846509, 8.373302309308519042, 0.6171781843518510113 ) ) ;
#51052 = CARTESIAN_POINT ( 'NONE',  ( 4.991564454312596766, 1.928456700051227379, 0.5879293935868237231 ) ) ;
#51053 = CARTESIAN_POINT ( 'NONE',  ( 4.997927640213790212, -0.6233917918176261619, -1.732523409203725606 ) ) ;
#51054 = CARTESIAN_POINT ( 'NONE',  ( 0.07661050522435489119, 4.099791711901569435, -2.265836654070508605 ) ) ;
#51055 = CARTESIAN_POINT ( 'NONE',  ( 3.580997583313150212, -2.223846063185720645, -0.6162045312432282707 ) ) ;
#51056 = CARTESIAN_POINT ( 'NONE',  ( 6.505933609711257226, 8.683618192786854095, -1.599625672291281386 ) ) ;
#51057 = CARTESIAN_POINT ( 'NONE',  ( 5.097027542433036018, 1.800287743887505343, -1.196142203056582920 ) ) ;
#51058 = CARTESIAN_POINT ( 'NONE',  ( 7.969495366734495434, 8.192166104145387706, 1.040834085586084257E-14 ) ) ;
#51059 = CARTESIAN_POINT ( 'NONE',  ( 0.02871324022350740107, -1.775192216153992808, 0.7880070256306227483 ) ) ;
#51060 = CARTESIAN_POINT ( 'NONE',  ( -5.596818484342970912, 5.424043074688562172, -0.7998128361456221525 ) ) ;
#51061 = CARTESIAN_POINT ( 'NONE',  ( 3.919517222396780909, 0.8229245375931023565, 2.146178768164926254 ) ) ;
#51062 = CARTESIAN_POINT ( 'NONE',  ( 2.675383846940436072, 0.4458684588860059028, -0.1127173061977529422 ) ) ;
#51063 = CARTESIAN_POINT ( 'NONE',  ( -5.601453741101424022, 6.564059448486966986, -1.199719254218453823 ) ) ;
#51064 = CARTESIAN_POINT ( 'NONE',  ( 3.608139902456270143, -0.7572706533398064765, -1.710698989992056607 ) ) ;
#51065 =( BOUNDED_CURVE ( )  B_SPLINE_CURVE ( 2, ( #70732, #170388, #21977, #154159, #5726, #121739, #89173 ),
 .UNSPECIFIED., .F., .T. ) 
 B_SPLINE_CURVE_WITH_KNOTS ( ( 3, 2, 2, 3 ),
 ( 0.4000000000000002998, 0.4083333333333336590, 0.4166666666666671293, 0.4250000000000004885 ),
 .UNSPECIFIED. ) 
 CURVE ( )  GEOMETRIC_REPRESENTATION_ITEM ( )  RATIONAL_B_SPLINE_CURVE ( ( 0.9999999999999955591, 0.8660254037844431485, 1.000000000000000000, 0.8660254037844387076, 1.000000000000000000, 0.8660254037844307140, 1.000000000000007994 ) ) 
 REPRESENTATION_ITEM ( '' )  );
#51068 = CARTESIAN_POINT ( 'NONE',  ( -5.803772275101700906, 8.928762199997411386, -1.199719254218452047 ) ) ;
#51067 = CARTESIAN_POINT ( 'NONE',  ( -1.364683531249997417, 5.509375000341417916, 1.214306433183764966E-14 ) ) ;
#51066 = CARTESIAN_POINT ( 'NONE',  ( 1.494246876672610025, -1.020364814108923213, 1.617233793950809906 ) ) ;
#51069 = CARTESIAN_POINT ( 'NONE',  ( 2.825073394047578734, 2.078234123670623212, 0.7428476018367863309 ) ) ;
#51070 = CARTESIAN_POINT ( 'NONE',  ( 2.706824224222692088, 6.309712028235118453, 0.7998128361456362523 ) ) ;
#51071 = CARTESIAN_POINT ( 'NONE',  ( 6.604230223188150894, 9.758666789477915771, -1.082531754730548412 ) ) ;
#51072 = CARTESIAN_POINT ( 'NONE',  ( -2.785310492603665367, 5.336947110424484109, 1.199719254218462483 ) ) ;
#51073 = CARTESIAN_POINT ( 'NONE',  ( -7.444835747235459600, 8.818634805597074688, 1.082531754730549078 ) ) ;
#51074 = CARTESIAN_POINT ( 'NONE',  ( 0.2453084554022276487, -1.520975263078115258, -1.253778558530042053 ) ) ;
#51075 = CARTESIAN_POINT ( 'NONE',  ( 6.691963835194851384, -0.9925954392468823162, 2.080958020993000979 ) ) ;
#51077 = EDGE_CURVE ( 'NONE', #56590, #88193, #6840, .T. ) ;
#51076 = CARTESIAN_POINT ( 'NONE',  ( 1.275752070009423367, -1.914805681740685106, 0.4264308320794732432 ) ) ;
#51078 = CARTESIAN_POINT ( 'NONE',  ( 4.241124981676721362, -0.1973008666005781619, -2.053083420615212429 ) ) ;
#51079 = CARTESIAN_POINT ( 'NONE',  ( 4.636525346193557162, 7.392734756325715750, -1.082531754730549078 ) ) ;
#51080 = CARTESIAN_POINT ( 'NONE',  ( 7.205232291019763480, 7.370802192470005565, -0.7998128361456341429 ) ) ;
#51081 = ORIENTED_EDGE ( 'NONE', *, *, #9913, .T. ) ;
#51082 = CARTESIAN_POINT ( 'NONE',  ( 6.738039155867407537, 10.80487008191325771, -0.7216878364870267237 ) ) ;
#51083 = CARTESIAN_POINT ( 'NONE',  ( -1.364683531249997417, 4.321875000341417028, 1.214306433183764966E-14 ) ) ;
#51084 = CARTESIAN_POINT ( 'NONE',  ( 1.347439764754987941E-16, 3.466143782776612170, 2.000000000000000000 ) ) ;
#51085 = CARTESIAN_POINT ( 'NONE',  ( 4.812781342726866640, 5.677628323678546529, 1.082531754730560403 ) ) ;
#51086 = CARTESIAN_POINT ( 'NONE',  ( 6.373493056145338009, -0.2723341383174918695, 2.153988726128319264 ) ) ;
#51088 = CARTESIAN_POINT ( 'NONE',  ( 6.444863656277017405, -1.483217659742748218, -1.090817886357238198 ) ) ;
#51087 = CARTESIAN_POINT ( 'NONE',  ( 9.578206935421269108, -9.746166700192988586, -0.1671882239536438552 ) ) ;
#51089 = CARTESIAN_POINT ( 'NONE',  ( -2.315885204923618268, 3.829536045110814690, 11.43841291973005703 ) ) ;
#51090 = DIRECTION ( 'NONE',  ( 1.000000000000000000, -7.771561172376097755E-16, -4.440892098500627148E-16 ) ) ;
#51091 = CARTESIAN_POINT ( 'NONE',  ( 1.774454573425466863, -1.774572579973210384, -0.5916213571805841731 ) ) ;
#51092 = CARTESIAN_POINT ( 'NONE',  ( -6.126358594793636314, 6.003181085514223803, -0.2003443317756918585 ) ) ;
#51093 = CARTESIAN_POINT ( 'NONE',  ( 6.098455030413784783, 7.112933956528650015, -1.126327413477963502 ) ) ;
#51094 = CARTESIAN_POINT ( 'NONE',  ( -0.6823417656250212460, 4.863541667008086655, 1.181850606188767472 ) ) ;
#51095 = CARTESIAN_POINT ( 'NONE',  ( 1.523922206041250949, -1.897707704667614736, 0.2351830868887184178 ) ) ;
#51096 = CARTESIAN_POINT ( 'NONE',  ( 3.379546851323252721, 1.122120933264129539, 1.368648242959294992 ) ) ;
#51097 = CARTESIAN_POINT ( 'NONE',  ( 1.242663310189826564, 1.843194135250892707, 0.5091577964371830634 ) ) ;
#51099 = CARTESIAN_POINT ( 'NONE',  ( 3.849167162397474140, 0.2308054593076276639, -1.901561516516042660 ) ) ;
#51098 = CARTESIAN_POINT ( 'NONE',  ( -5.606383287671886428, 5.556235044223195807, 0.1555002321169836055 ) ) ;
#51100 = CARTESIAN_POINT ( 'NONE',  ( 1.499999999999985123, -0.9541666666666493990, -0.8660254037844323793 ) ) ;
#51101 = CARTESIAN_POINT ( 'NONE',  ( 5.687944394218412469, -1.248225810400976465, -1.523521433493113308 ) ) ;
#51102 = CARTESIAN_POINT ( 'NONE',  ( 1.266058358664986949, 0.6103625328083387425, -2.030891291126469600 ) ) ;
#51103 = CARTESIAN_POINT ( 'NONE',  ( -1.734723475976807094E-15, -8.407420853759283830, -10.91970695577494332 ) ) ;
#51104 = CARTESIAN_POINT ( 'NONE',  ( 3.520239479114236403, 1.187513476551487424, -1.445374034619356207 ) ) ;
#51106 = ORIENTED_EDGE ( 'NONE', *, *, #108140, .F. ) ;
#51105 = CARTESIAN_POINT ( 'NONE',  ( 1.119449510670032177, -1.781678707675336870, 0.3977030049751931196 ) ) ;
#51108 = DIRECTION ( 'NONE',  ( -0.8164965809277274778, -1.312140583148642173E-14, -0.5773502691896237327 ) ) ;
#51107 = CARTESIAN_POINT ( 'NONE',  ( 3.492985898914053866, -0.4302566696539159574, -2.164365734511737305 ) ) ;
#51109 = CARTESIAN_POINT ( 'NONE',  ( -1.364683531250010295, 4.592708333674755394, 0.7879004041258379498 ) ) ;
#51110 = CARTESIAN_POINT ( 'NONE',  ( 0.7837256325555241876, -1.959260395640700203, 0.6451903852672227213 ) ) ;
#51111 = CARTESIAN_POINT ( 'NONE',  ( 7.962716289927667113, 8.184257181204083409, -0.7998128361456291469 ) ) ;
#51112 = CARTESIAN_POINT ( 'NONE',  ( -10.01677656239806247, 10.58066083241955901, 0.7998128361456462443 ) ) ;
#51113 = CARTESIAN_POINT ( 'NONE',  ( 0.000000000000000000, 15.44694763437329676, -11.95586206896577153 ) ) ;
#51114 = CARTESIAN_POINT ( 'NONE',  ( -3.426641765799319561, -0.01965654466554235882, -0.4167094806288151321 ) ) ;
#51115 = CARTESIAN_POINT ( 'NONE',  ( 5.969332771766739931, 10.18624834369502885, -0.7998128361456481317 ) ) ;
#51117 = AXIS2_PLACEMENT_3D ( 'NONE', #143713, #177236, #28849 ) ;
#51116 = VECTOR ( 'NONE', #85011, 1000.000000000000000 ) ;
#51118 = ORIENTED_EDGE ( 'NONE', *, *, #116869, .T. ) ;
#51119 = CARTESIAN_POINT ( 'NONE',  ( 4.281733463571851139, -1.982135700070002615, 0.5980053909793592304 ) ) ;
#51120 = CARTESIAN_POINT ( 'NONE',  ( -1.500000000000013101, 4.129166666666687746, -0.8660254037844313801 ) ) ;
#51121 = CARTESIAN_POINT ( 'NONE',  ( 1.810078809455554438, -2.145489296895970011, 0.2626290421628638128 ) ) ;
#51122 = CARTESIAN_POINT ( 'NONE',  ( -5.527359202251545867, 7.456348097644321271, -1.248928334283349040 ) ) ;
#51124 = EDGE_CURVE ( 'NONE', #159043, #10129, #28785, .T. ) ;
#51123 = CARTESIAN_POINT ( 'NONE',  ( 1.963541569377712959, -1.623395098231813494, -1.201329681988633657 ) ) ;
#51125 = CARTESIAN_POINT ( 'NONE',  ( 4.881142843665459807, 6.718083573547731113, -1.292325262782492823 ) ) ;
#51126 = ORIENTED_EDGE ( 'NONE', *, *, #202990, .F. ) ;
#51127 = EDGE_CURVE ( 'NONE', #35700, #49868, #111732, .T. ) ;
#51129 = CARTESIAN_POINT ( 'NONE',  ( 7.266807147244743526, 11.42176607185347414, -0.7216878364870267237 ) ) ;
#51128 = CARTESIAN_POINT ( 'NONE',  ( 1.737500000000001155, -3.733333333333331616, 3.009438278150922130 ) ) ;
#51130 = CARTESIAN_POINT ( 'NONE',  ( 1.817608056788092563, -0.8389924079203456841, 1.022373108394124985 ) ) ;
#51131 = CARTESIAN_POINT ( 'NONE',  ( 0.4797043241997685503, -0.7212876333932433104, 1.883314553594167107 ) ) ;
#51132 = CARTESIAN_POINT ( 'NONE',  ( 6.539320575229280230, 7.629137130509070275, 2.703262396134015866 ) ) ;
#51133 = CARTESIAN_POINT ( 'NONE',  ( 4.458633810090739225, -1.957822973221786667, -0.9849130632908837946 ) ) ;
#51134 = CARTESIAN_POINT ( 'NONE',  ( -0.7499999999999972244, 3.889583334016149863, -1.299038105676652011 ) ) ;
#51135 = CARTESIAN_POINT ( 'NONE',  ( 3.621269620730773298, 1.642686141288721480, 0.9789267784374030557 ) ) ;
#51136 = CARTESIAN_POINT ( 'NONE',  ( -3.391510981712833939, 7.108513245306943062, 0.7998128361456341429 ) ) ;
#51137 = CARTESIAN_POINT ( 'NONE',  ( 3.782361668088245921, 6.396210465202840645, -1.082531754730548412 ) ) ;
#51138 = CARTESIAN_POINT ( 'NONE',  ( 1.423454079394898875, -1.462460055423294047, -1.388472309132340321 ) ) ;
#51139 = CARTESIAN_POINT ( 'NONE',  ( 0.6823417656249969321, 12.08854166700806765, -1.181850606188757036 ) ) ;
#51141 = CARTESIAN_POINT ( 'NONE',  ( -5.829079699232685208, 5.765290835385048496, 0.000000000000000000 ) ) ;
#51140 = CARTESIAN_POINT ( 'NONE',  ( 0.1348729467166914497, 0.4002676433968958558, 2.257031873882467732 ) ) ;
#51142 = CARTESIAN_POINT ( 'NONE',  ( 4.506709144069167117, 1.332172526941363344, -1.095522069602150372 ) ) ;
#51143 = CARTESIAN_POINT ( 'NONE',  ( 0.1405533004714253908, 5.720147882271004569, -2.873730252010114228 ) ) ;
#51144 = CARTESIAN_POINT ( 'NONE',  ( 4.253507506385319381, 5.985511395581417204, 1.599625672291267398 ) ) ;
#51145 = CARTESIAN_POINT ( 'NONE',  ( -0.02244404828157658613, -0.004869073801674199918, -2.189079685368473527 ) ) ;
#51146 = CARTESIAN_POINT ( 'NONE',  ( 1.644895634054041933, -0.2845770130874228365, -1.940982728367894206 ) ) ;
#51147 = CARTESIAN_POINT ( 'NONE',  ( 11.44779963594988637, 10.19999999999999929, -3.600000000000000977 ) ) ;
#51148 = CARTESIAN_POINT ( 'NONE',  ( 3.181359600701000989, 6.863336634126477875, 0.000000000000000000 ) ) ;
#51149 = CARTESIAN_POINT ( 'NONE',  ( 0.07536363704237906969, 4.084105538841027894, -2.698926661290324880 ) ) ;
#51150 = ADVANCED_FACE ( 'NONE', ( #41523 ), #166254, .T. ) ;
#51151 = VERTEX_POINT ( 'NONE', #153120 ) ;
#51152 = VECTOR ( 'NONE', #211698, 1000.000000000000000 ) ;
#51153 =( BOUNDED_SURFACE ( )  B_SPLINE_SURFACE ( 3, 3, ( 
 ( #210147, #8765, #61790, #127957, #45558, #29292, #95384, #123685, #113808, #80162, #46619, #82282, #114858, #179809, #66006, #146267, #31428, #212279, #96451, #145212, #163562, #181909, #162502, #97505, #15146, #81232, #63913, #133211, #33541, #17268, #129006, #180858, #132156, #147314, #211219, #130069, #196064, #213341, #47694, #64964, #131117, #32480, #100671, #62845, #198161, #14072, #194983, #197105, #99614, #48745, #98554, #164615, #16200, #148375, #199217, #165680, #83344, #112740, #214376, #49795, #115921, #178751, #149429, #1011, #67076, #50864, #116986, #182986, #34603, #166749, #30364, #18344, #2074, #200286, #38879, #51937, #171005, #152623, #85489, #20474, #104963, #102815, #19411, #52986, #202410, #86561, #106063, #84424, #35664, #4210, #121276, #151576, #201346, #204547, #172086, #186176, #70278, #37810, #136394, #118061, #184046, #56196, #3144, #103886, #120201, #137463, #154768, #167811, #101743, #135332, #69213, #119122, #54066, #122358, #185102, #169934, #36728, #21518, #87629, #168870, #150513, #68148, #153701, #134281, #138524, #188315, #5269, #203478, #71346, #55131, #187252, #22602, #88709, #6351, #72422, #39956, #140685, #205627, #75647, #192569, #206701, #90847, #189389, #44224, #76696, #77766, #74582, #7419, #73501, #58328, #143887, #124484, #156911, #190442, #42101, #108215, #139603, #174239, #41031, #10621, #25812, #141754, #45287, #91922, #173167, #57265, #175294, #207761, #157982, #159028, #24746, #9570, #8501, #59388, #125544, #191506, #43172, #92983, #109284, #26880, #142812, #208818, #193645, #60449, #126606, #110346, #123427, #176349, #27956, #94049, #160089, #11692, #209880, #61519, #127685, #111407, #23678, #89789, #155835, #107141, #98292, #114603, #112469, #214117, #78820, #99359, #144942, #62575, #162230, #47425, #163292, #129808, #14873, #148113, #180594, #65744, #197899, #97238, #17006, #181648, #13817, #164354, #128737, #130850, #79890, #30089, #149160, #15938, #95111, #212010, #12747, #131891, #82022, #210949, #49529, #146000, #738, #165410, #115653, #46351, #32219, #198951, #63653, #161160, #96179, #195787, #33274, #50593, #113540, #83081, #66804, #80965, #177411, #132946, #179544, #29028, #194711, #178478, #31165, #147057, #213077, #64707, #196847, #48485, #203227, #70015, #117800, #54871, #91400, #167549, #67874, #200027, #19149, #186992, #3948, #168610, #184845, #100411, #185913, #157460, #68951, #202146, #119937, #53807, #87372, #84160, #37547, #173721, #169679, #153442, #103627, #21267, #36474, #182718, #35400, #135072, #150247, #9055, #207248, #75130, #141239, #116718, #134020, #102546, #5014, #183792, #85223, #25298, #34336, #136131, #118859, #71087, #20212, #1816, #51679, #166480, #101478, #137204, #152370, #121025, #38623, #151312, #2880, #201085, #52726, #86300, #107695, #18072, #43717, #176898, #93532, #193137, #12243, #59936, #58874, #42651, #127166, #146560, #113036, #179042, #108761, #111970, #175843, #94601, #109833, #126091, #143366, #125030, #45850, #29586, #27434, #26361, #110891, #13320, #159576, #192052, #10113, #79393, #177973, #30660, #11173, #174786, #92475, #77249, #96744, #209363, #61009, #44785, #28511, #160643, #158515, #78318, #76188, #95674, #144442, #210445, #80461, #62083, #208306, #142296, #128241, #194205, #161728, #145511, #211510, #63146, #129308 ),
 ( #195286, #46918, #162794, #14371, #190987, #64220, #131400, #16501, #180100, #35966, #85792, #168113, #19713, #197397, #32777, #82582, #147607, #67372, #181154, #115160, #133514, #17560, #212580, #49040, #164906, #116220, #31726, #148668, #132455, #99915, #213626, #84721, #165976, #65251, #150809, #184343, #98855, #163858, #81527, #235, #68451, #83646, #50099, #66308, #196350, #199520, #102044, #198454, #149732, #1310, #51165, #183284, #97799, #117287, #52228, #34889, #100961, #167050, #18642, #182211, #130361, #33835, #2373, #15438, #47993, #114108, #134580, #200580, #118356, #186481, #21819, #86859, #6652, #120506, #54366, #72729, #171303, #107442, #202715, #104185, #55424, #119423, #170235, #71646, #39178, #23973, #152924, #38114, #89011, #155064, #70572, #123719, #121577, #204844, #138824, #56497, #122655, #4502, #188618, #53290, #73804, #185410, #37028, #136690, #87924, #137760, #153999, #203780, #40250, #106361, #172385, #90075, #187548, #205929, #156138, #5567, #7721, #103114, #105262, #22895, #139898, #189682, #57562, #69513, #41334, #201643, #173467, #25046, #169171, #151872, #3446, #135622, #20765, #177719, #174534, #28257, #112777, #142041, #74878, #158274, #9863, #29328, #178789, #208056, #111710, #144193, #10917, #91147, #78067, #75940, #157202, #127992, #129047, #211256, #59683, #195023, #191800, #46656, #193947, #95422, #140984, #60750, #210186, #125843, #8799, #43464, #109584, #159321, #175589, #27179, #93284, #126912, #206994, #58625, #61825, #124778, #190737, #45593, #42401, #161475, #76993, #92223, #143120, #13053, #209112, #26111, #192870, #44526, #110644, #108509, #176645, #94350, #160391, #79133, #11992, #145250, #62879, #34639, #164653, #197142, #16237, #48780, #146302, #212314, #199254, #47731, #82321, #98590, #49832, #149466, #196098, #63950, #97541, #130105, #113848, #32516, #50900, #163599, #148414, #81269, #114895, #166411, #179844, #30402, #14109, #180894, #96488, #117026, #183022, #31467, #181947, #147348, #66046, #15181, #213375, #132189, #80198, #115957, #99649, #64998, #131151, #198197, #17306, #33576, #165717, #83384, #1050, #67114, #100710, #133248, #162538, #207696, #44153, #129742, #192502, #76628, #60377, #110274, #126540, #59317, #176283, #175226, #210887, #160024, #127617, #31104, #27885, #158959, #125474, #161092, #193581, #93982, #144881, #10554, #11623, #142743, #26811, #9502, #77697, #46288, #92913, #143818, #209815, #61450, #208751, #211950, #97177, #45225, #191434, #111340, #177345, #162167, #75574, #28957, #30026, #62512, #95042, #141683, #128677, #12681, #43101, #112405, #47361, #195725, #78757, #113475, #194646, #179482, #178416, #96111, #13754, #79828, #145938, #109215, #63585, #114537, #32153, #214052, #19077, #50529, #672, #16936, #146995, #18002, #201012, #115587, #34271, #166407, #100343, #133953, #130788, #84092, #2810, #1747, #199960, #150179, #67804, #83017, #14813, #81959, #181581, #196783, #52659, #36399, #118787, #184773, #148044, #197836, #33210, #98231, #51608, #131827, #65680, #117732, #182649, #163231, #49468, #99294, #66738, #48424, #165341, #149090, #116652, #35330, #164286, #132881, #183721, #101409, #198883, #135001, #167482, #85158, #151241, #68882, #80904, #15874, #213012, #64648, #180531, #91174, #155090, #22920, #75967, #72753, #89035, #40276, #6676 ),
 ( #57589, #77018, #43493, #109613, #39196, #42429, #106386, #25072, #188645, #56522, #73833, #55447, #190765, #174564, #172409, #171324, #138850, #124806, #175618, #108534, #26140, #141013, #92253, #123746, #121599, #122682, #7746, #204867, #27205, #203801, #159347, #10944, #23997, #90100, #139929, #156165, #58652, #205956, #189707, #158299, #8828, #187571, #41360, #107470, #173496, #157233, #74905, #207021, #9890, #142070, #208084, #59711, #125871, #191830, #93312, #105288, #46685, #196125, #146327, #63983, #80229, #78093, #179872, #44553, #65026, #98619, #210214, #110669, #197171, #129076, #95451, #195047, #113877, #212342, #31497, #163629, #62906, #48807, #147378, #164680, #14136, #144220, #143147, #126940, #211283, #16265, #114924, #180923, #192897, #47763, #45619, #178816, #128017, #61850, #13081, #209142, #130136, #97572, #111736, #176669, #112803, #15210, #177742, #193971, #94375, #81301, #213405, #32544, #29357, #28281, #160416, #161501, #60781, #79161, #145277, #30429, #96515, #162564, #12021, #131181, #33606, #69274, #18408, #200348, #103950, #50928, #17332, #198224, #19471, #51997, #117053, #3205, #83413, #183050, #149495, #99676, #82349, #100735, #119181, #165746, #34665, #166814, #84484, #150574, #148440, #67143, #133277, #2136, #199285, #1078, #68212, #118123, #37873, #8, #135388, #66073, #49860, #36791, #115987, #168934, #134343, #184108, #35728, #102876, #101804, #167873, #85548, #151638, #201409, #169992, #132215, #53048, #185167, #20537, #86619, #152687, #202474, #181975, #4269, #70339, #136456, #54127, #120264, #186238, #141816, #22659, #123487, #187313, #55191, #108274, #105024, #121338, #72484, #38941, #171062, #139665, #59447, #6412, #9625, #41092, #191564, #107200, #88770, #21579, #5328, #89845, #109345, #75702, #207819, #71409, #74639, #138585, #57322, #204608, #154827, #106124, #87684, #8559, #206757, #56259, #203538, #73564, #190501, #122416, #188375, #40013, #42159, #140745, #125604, #172147, #137521, #23739, #155894, #43228, #7482, #205686, #189450, #173224, #24804, #90906, #156969, #58388, #124544, #174295, #25870, #153758, #91980, #158038, #76753, #112526, #145004, #143946, #96238, #176408, #209942, #28014, #126666, #175355, #193705, #212070, #192631, #127748, #45349, #111468, #94112, #163357, #63709, #47490, #159085, #211009, #162288, #177474, #160153, #14932, #129866, #113600, #10682, #62632, #13876, #61580, #26935, #11750, #77825, #29088, #95172, #161221, #12808, #128792, #130913, #93043, #79954, #142874, #208876, #195849, #60506, #179603, #78881, #194773, #46410, #31224, #178539, #110404, #30149, #146057, #97298, #196905, #44283, #81027, #147115, #213141, #64771, #48545, #20277, #136195, #1876, #116783, #67936, #182780, #82082, #214177, #86361, #115715, #134081, #65804, #148175, #201150, #197962, #131951, #165471, #49591, #181705, #18133, #152432, #99417, #102618, #200089, #70081, #51738, #33335, #114663, #98347, #34398, #202213, #168673, #4011, #164413, #167612, #17067, #150310, #83146, #149224, #199012, #180657, #101543, #85289, #799, #66867, #166545, #69016, #133012, #50657, #100470, #135133, #19210, #32282, #84222, #15997, #117861, #183853, #35465, #151375, #2944, #52788, #118927, #184907, #36531, #6150, #5074, #40834, #204343, #171882, #75450, #22403, #203286, #169740, #205430, #23479 ),
 ( #72220, #88512, #170812, #189197, #73294, #9379, #104763, #138327, #89586, #21329, #56001, #188120, #155635, #140490, #54933, #154574, #57068, #123232, #187052, #25618, #7220, #106943, #172966, #24545, #90653, #121085, #156714, #87436, #190250, #141563, #38684, #153504, #108019, #39751, #122152, #105856, #8305, #74389, #206501, #58132, #139397, #91730, #124291, #157781, #41908, #71149, #174045, #53867, #120000, #185977, #37610, #103691, #137266, #42978, #95993, #128558, #175103, #29908, #44034, #179362, #195607, #79709, #76506, #144762, #14693, #110152, #191310, #60259, #126416, #145824, #80788, #176165, #13636, #46171, #127495, #207571, #194523, #192379, #59192, #162046, #30984, #113357, #27765, #97059, #93861, #163112, #208625, #211829, #160973, #159899, #63466, #125347, #11506, #158837, #142617, #77577, #129621, #94924, #45110, #61336, #109088, #62393, #26690, #143700, #78637, #210773, #112285, #178301, #92792, #47242, #10434, #209692, #193466, #111220, #177223, #28836, #12563, #65561, #165221, #114415, #184649, #20015, #102347, #168418, #131708, #181465, #16813, #81840, #1621, #146878, #197712, #167360, #199837, #66610, #212898, #133824, #49354, #64530, #183594, #36270, #52532, #115472, #130675, #33094, #196663, #147924, #18948, #100218, #213940, #85032, #118666, #99168, #98119, #15756, #82898, #2686, #34148, #198760, #545, #48304, #67680, #180415, #148971, #17875, #150049, #83960, #117602, #32033, #51479, #200886, #35201, #101276, #151120, #68759, #132757, #164171, #50409, #116528, #182518, #166286, #134879, #41648, #107762, #4805, #120814, #170543, #21066, #155369, #54666, #203024, #6954, #105581, #173788, #136997, #38419, #204079, #53601, #104499, #5882, #187856, #172700, #87164, #186791, #23209, #89322, #70886, #57869, #55732, #139133, #73035, #205161, #56803, #153234, #122973, #201945, #8038, #86103, #22127, #119735, #140223, #71956, #88240, #138066, #188932, #40571, #106677, #24278, #121886, #124032, #90384, #189998, #156453, #37347, #39483, #154310, #171615, #152175, #74128, #3744, #206244, #135927, #69819, #185713, #103421, #169482, #76256, #211573, #13383, #112037, #108828, #176966, #46982, #142365, #9120, #92542, #158582, #178039, #25364, #191055, #93603, #62151, #10182, #208374, #145575, #113098, #127237, #27503, #193206, #159648, #207319, #125097, #63207, #26432, #44853, #42720, #58940, #29655, #174854, #60006, #126159, #192122, #43788, #143436, #129371, #109900, #79459, #110959, #195350, #28583, #175912, #91464, #75195, #11245, #157525, #141307, #77323, #209433, #78388, #61077, #94671, #160713, #12307, #144508, #210516, #128310, #194273, #45918, #95741, #161792, #133581, #81588, #31791, #130428, #199585, #17626, #18703, #15501, #162858, #14436, #213690, #84786, #147673, #97865, #65312, #131461, #197462, #80526, #49105, #196413, #166042, #115226, #82647, #203575, #181216, #114171, #146623, #116283, #148731, #32842, #99977, #180165, #98919, #163926, #48058, #179104, #164972, #1375, #16564, #299, #66370, #132518, #198516, #167116, #67436, #51228, #212640, #50162, #83711, #182274, #30726, #33898, #149801, #117352, #183350, #34954, #101025, #150874, #137557, #96809, #5363, #64282, #71445, #55226, #22691, #207856, #189485, #122453, #57358, #141851, #139700, #56293, #89879, #24842, #123521, #142912, #23774, #26973 ),
 ( #175387, #107240, #73598, #173261, #92016, #124578, #158074, #59482, #41128, #159120, #125639, #93078, #42195, #72523, #74675, #172184, #188412, #10721, #108310, #38976, #155931, #171100, #9662, #174330, #88804, #75738, #7516, #76790, #109380, #191600, #204642, #58425, #208912, #205723, #105062, #40049, #106158, #43262, #121372, #90941, #187347, #25906, #157007, #154863, #6445, #8593, #138619, #140778, #206793, #190539, #111504, #164451, #161258, #16038, #61617, #147153, #13911, #127787, #213178, #32319, #177510, #11788, #143985, #29122, #130954, #162327, #112568, #128829, #44319, #129904, #98387, #12845, #146097, #63745, #212108, #31264, #28055, #195888, #114700, #113639, #97338, #47526, #179644, #194811, #126704, #193742, #78919, #94148, #82121, #148214, #60546, #192665, #45388, #95209, #145041, #209976, #163396, #211044, #62670, #14970, #79993, #110441, #46447, #178579, #30187, #160187, #96277, #81067, #64807, #196944, #48584, #180694, #176443, #77862, #133050, #151414, #199052, #186015, #117900, #52829, #2988, #135175, #69055, #149266, #36571, #115754, #136232, #169780, #66910, #181745, #53906, #200130, #166588, #51783, #184944, #201190, #102657, #20318, #134121, #37651, #4051, #103729, #118966, #165513, #167650, #50698, #116822, #21369, #168714, #131994, #34440, #49629, #86404, #152471, #33375, #70121, #182824, #87477, #202255, #120041, #83183, #214216, #65845, #100513, #198003, #18177, #84264, #99456, #17105, #150349, #845, #1919, #183893, #67978, #35505, #101582, #19251, #85331, #191350, #59226, #204385, #43015, #39792, #109128, #154612, #25656, #106980, #6191, #91766, #125384, #56041, #104805, #22440, #122197, #9418, #40875, #205473, #7259, #137306, #8344, #175142, #105899, #24586, #156755, #90693, #124329, #121126, #74429, #207607, #206541, #190289, #140529, #58171, #73335, #5112, #72260, #171923, #187090, #26728, #153543, #71189, #203323, #138368, #188159, #23519, #88551, #41946, #89625, #155677, #108059, #173005, #54974, #139438, #57105, #123274, #38724, #189236, #174084, #157822, #75489, #141600, #170850, #29946, #180451, #48341, #114452, #11544, #127532, #177260, #27802, #162082, #61374, #209731, #13671, #112322, #92830, #143737, #45145, #210807, #60296, #111257, #12602, #194561, #179400, #93900, #193504, #96031, #79743, #77614, #64567, #62432, #145860, #211866, #63505, #129659, #159939, #195643, #208665, #14731, #158874, #28874, #126454, #146913, #78674, #94959, #144800, #47279, #113391, #31020, #97094, #128595, #130710, #163147, #196701, #80823, #44072, #46206, #161007, #178337, #10470, #212931, #76544, #142655, #192417, #110191, #176201, #213974, #68794, #82933, #3780, #20051, #118700, #115505, #183632, #53636, #149006, #15791, #99208, #165257, #184686, #119769, #582, #52569, #85067, #166322, #32068, #18986, #16850, #98157, #134914, #69854, #152210, #66648, #135964, #132793, #201980, #33128, #36306, #199872, #198796, #102385, #164204, #50445, #197748, #181500, #116564, #168452, #133865, #83997, #100253, #81877, #101314, #147961, #182557, #117640, #35239, #167395, #2722, #65594, #151153, #86139, #200921, #131743, #49386, #34181, #17911, #150086, #1657, #67714, #51515, #9154, #57904, #120853, #71993, #123013, #188965, #104534, #157561, #89358, #24314, #40607, #106712, #172738, #186827, #8078, #87203, #107797 ),
 ( #105620, #75231, #190033, #141341, #90420, #137033, #139168, #22163, #38457, #207355, #156489, #103457, #5921, #21100, #74166, #140259, #153268, #206281, #88278, #58975, #173822, #124068, #54703, #41686, #185749, #154343, #169519, #170580, #138105, #25400, #37382, #204115, #91500, #4843, #171649, #70922, #203060, #55767, #121925, #187892, #39520, #23246, #155406, #6989, #73069, #205199, #56840, #211606, #78421, #126193, #63242, #96841, #175943, #76289, #208406, #27539, #195384, #12341, #176999, #193241, #108861, #194309, #162889, #77357, #210550, #128343, #62186, #95772, #92576, #45950, #179138, #178071, #161829, #112070, #29689, #44888, #191088, #43819, #143470, #158618, #14471, #212673, #80560, #146659, #109934, #159676, #209467, #60040, #13416, #93634, #11278, #79491, #144543, #125130, #61110, #127270, #28615, #10215, #110994, #94705, #145610, #160746, #129404, #192156, #47016, #30761, #42757, #113131, #174887, #26467, #142398, #31824, #163959, #184444, #65347, #166075, #15537, #97900, #150910, #147705, #81621, #115257, #213724, #131494, #182307, #102143, #49141, #52328, #83748, #19809, #149840, #197498, #64314, #48092, #132550, #151970, #118458, #36062, #114204, #117390, #181250, #100010, #32877, #98954, #148763, #130459, #51266, #34992, #165005, #16599, #116316, #18738, #82680, #332, #66405, #84822, #183386, #168210, #198549, #180202, #50197, #33936, #85895, #17663, #1410, #67470, #133618, #199620, #101064, #167151, #2472, #68549, #134676, #200679, #196449, #186585, #153029, #119523, #155169, #187649, #38213, #138931, #4602, #104286, #70677, #169275, #3543, #21918, #40361, #20861, #170334, #88027, #154099, #136787, #206031, #106464, #90182, #201746, #39275, #204952, #5668, #69614, #202815, #54464, #71747, #120608, #137863, #203883, #105370, #173579, #135723, #56600, #53387, #185510, #172490, #37133, #156245, #55527, #121682, #171407, #24077, #22997, #89114, #6752, #72828, #122764, #25149, #103215, #86960, #188723, #7823, #73915, #140008, #57666, #123824, #189786, #41436, #107545, #91250, #125949, #9967, #208160, #191905, #59792, #141089, #109687, #108611, #144297, #93387, #60856, #178892, #43568, #92332, #58728, #94454, #127018, #175690, #78168, #158374, #27281, #76044, #174638, #157310, #159423, #194047, #26215, #11023, #77100, #143225, #142146, #145359, #45699, #29435, #207100, #192977, #210290, #209215, #8900, #44630, #110746, #176744, #28358, #160492, #12099, #61931, #112878, #74981, #128089, #124879, #190843, #111817, #42505, #95526, #177819, #161576, #13163, #79241, #211359, #62984, #129153, #195128, #46766, #30506, #96587, #47839, #164752, #133353, #163703, #213474, #2213, #118198, #198295, #98694, #49936, #16342, #64059, #196196, #68289, #97644, #116057, #113950, #130202, #183129, #179946, #31569, #147451, #15284, #81370, #79, #134422, #65097, #84561, #182047, #52071, #33677, #131254, #162636, #80305, #82423, #184185, #150651, #200425, #146405, #149571, #197241, #132289, #48880, #114998, #180997, #14210, #83488, #67217, #32616, #148512, #66144, #51006, #99751, #1155, #199359, #165821, #117127, #17404, #212417, #34735, #100807, #166893, #18485, #123563, #205769, #57398, #169011, #70416, #120342, #185246, #105104, #4347, #152766, #171143, #55270, #35807, #86697, #202552, #153841, #3286, #54203, #170073, #137602 ),
 ( #187389, #36869, #72567, #151716, #172228, #101884, #102952, #69353, #89922, #21659, #186318, #87765, #6492, #39021, #138665, #56337, #5411, #73646, #40090, #7560, #22735, #201485, #203619, #136532, #20609, #139745, #88852, #167949, #37953, #85629, #204687, #154908, #135463, #122498, #104025, #19552, #23817, #188459, #119260, #106202, #53130, #71490, #121417, #155973, #108351, #130747, #214014, #25952, #210022, #28095, #109424, #65636, #176485, #174373, #189526, #11830, #15830, #98194, #92058, #81916, #75783, #148003, #190580, #64607, #142955, #42238, #196741, #164242, #158115, #140822, #58468, #9707, #48381, #76835, #27015, #43304, #173302, #44363, #41173, #141890, #60590, #192707, #126748, #160231, #157050, #110486, #32109, #107281, #207899, #94191, #77907, #144027, #114494, #8638, #180490, #24882, #90987, #74718, #206835, #124622, #175429, #59522, #125682, #191640, #93123, #159162, #10761, #208957, #87250, #50488, #166365, #1704, #66690, #200966, #100298, #34226, #52613, #151196, #153315, #182602, #84043, #35284, #99250, #150131, #51562, #19030, #3826, #132837, #17956, #68838, #134958, #116609, #103504, #101360, #184726, #118742, #36350, #102428, #198841, #168497, #33168, #53683, #4890, #67758, #165298, #185794, #117687, #133909, #183679, #20096, #86184, #152253, #69899, #167438, #169564, #136010, #21146, #202023, #82974, #85110, #199915, #2767, #131784, #119814, #49425, #37427, #181540, #197788, #115545, #16893, #149047, #623, #42800, #59017, #157605, #154389, #8126, #92620, #121969, #54748, #138150, #204159, #9201, #158662, #187935, #91547, #124115, #205243, #70968, #57950, #55814, #137078, #107839, #108908, #191134, #39565, #174931, #171694, #26511, #72037, #75273, #24358, #105667, #141388, #203103, #23293, #22212, #5967, #89403, #207398, #172785, #123059, #139212, #120898, #140307, #186871, #125173, #38503, #104581, #190078, #155452, #106757, #7035, #73112, #56884, #170626, #41730, #173866, #189013, #88325, #40656, #25441, #90468, #156535, #74212, #206325, #29732, #113177, #77400, #208449, #142442, #61153, #179181, #209512, #93681, #143516, #127315, #193285, #60082, #44930, #43863, #178117, #111038, #12386, #14514, #177045, #27583, #126239, #194352, #78465, #28661, #95814, #159723, #94747, #11321, #109979, #10260, #160794, #79536, #144584, #210598, #62227, #128384, #45994, #30804, #145654, #63287, #192201, #112114, #161872, #13460, #76335, #211650, #129448, #195430, #47060, #96884, #162933, #80607, #175989, #54351, #169155, #2357, #103096, #183268, #117270, #135607, #19697, #170219, #51146, #167033, #118341, #182192, #18628, #134563, #102029, #86843, #149716, #100946, #151856, #3432, #133499, #186463, #184325, #53276, #69499, #201627, #119407, #1296, #37014, #116205, #136676, #21803, #67354, #33820, #120490, #200566, #84707, #52212, #185396, #20748, #152909, #4486, #35950, #38099, #70557, #104170, #202701, #165960, #168098, #34872, #199502, #17544, #219, #150794, #87910, #83634, #68433, #85775, #66291, #132437, #198438, #50084, #99899, #137745, #123705, #140969, #122641, #5550, #138809, #204828, #7705, #56479, #72713, #188603, #189666, #109570, #71632, #106346, #187533, #203765, #208042, #55409, #26096, #73788, #155048, #90061, #174520, #172368, #88995, #40235, #57547, #156122, #175574, #153983, #105247, #139882 ) ),
 .UNSPECIFIED., .T., .F., .T. ) 
 B_SPLINE_SURFACE_WITH_KNOTS ( ( 4, 3, 4 ),
 ( 4, 1, 1, 1, 1, 1, 1, 1, 1, 1, 1, 1, 1, 1, 1, 1, 1, 1, 1, 1, 1, 1, 1, 1, 1, 1, 1, 1, 1, 1, 1, 1, 1, 1, 1, 1, 1, 1, 1, 1, 1, 1, 1, 1, 1, 1, 1, 1, 1, 1, 1, 1, 1, 1, 1, 1, 1, 1, 1, 1, 1, 1, 1, 1, 1, 1, 1, 1, 1, 1, 1, 1, 1, 1, 1, 1, 1, 1, 1, 1, 1, 1, 1, 1, 1, 1, 1, 1, 1, 1, 1, 1, 1, 1, 1, 1, 1, 1, 1, 1, 1, 1, 1, 1, 1, 1, 1, 1, 1, 1, 1, 1, 1, 1, 1, 1, 1, 1, 1, 1, 1, 1, 1, 1, 1, 1, 1, 1, 1, 1, 1, 1, 1, 1, 1, 1, 1, 1, 1, 1, 1, 1, 1, 1, 1, 1, 1, 1, 1, 1, 1, 1, 1, 1, 1, 1, 1, 1, 1, 1, 1, 1, 1, 1, 1, 1, 1, 1, 1, 1, 1, 1, 1, 1, 1, 1, 1, 1, 1, 1, 1, 1, 1, 1, 1, 1, 1, 1, 1, 1, 1, 1, 1, 1, 1, 1, 1, 1, 1, 1, 1, 1, 1, 1, 1, 1, 1, 1, 1, 1, 1, 1, 1, 1, 1, 1, 1, 1, 1, 1, 1, 1, 1, 1, 1, 1, 1, 1, 1, 1, 1, 1, 1, 1, 1, 1, 1, 1, 1, 1, 1, 1, 1, 1, 1, 1, 1, 1, 1, 1, 1, 1, 1, 1, 1, 1, 1, 1, 1, 1, 1, 1, 1, 1, 1, 1, 1, 1, 1, 1, 1, 1, 1, 1, 1, 1, 1, 1, 1, 1, 1, 1, 1, 1, 1, 1, 1, 1, 1, 1, 1, 1, 1, 1, 1, 1, 1, 1, 1, 1, 1, 1, 1, 1, 1, 1, 1, 1, 1, 1, 1, 1, 1, 1, 1, 1, 1, 1, 1, 1, 1, 1, 1, 1, 1, 1, 1, 1, 1, 1, 1, 1, 1, 1, 1, 1, 1, 1, 1, 1, 1, 1, 1, 1, 1, 1, 1, 1, 1, 1, 1, 1, 1, 1, 1, 1, 1, 1, 1, 1, 1, 1, 1, 1, 1, 1, 1, 1, 1, 1, 1, 1, 1, 1, 1, 1, 1, 1, 1, 1, 1, 1, 1, 1, 4 ),
 ( 0.000000000000000000, 0.5000000000000000000, 1.000000000000000000 ),
 ( 0.000000000000000000, 0.002600063085273907840, 0.005208809393482579861, 0.007813201938950280895, 0.01041611862257568050, 0.01302098276518856741, 0.01562474632808895890, 0.01822919105953027183, 0.02083324087635668453, 0.02343728507989274734, 0.02604173773626635227, 0.02864548761524753420, 0.03125016255115702773, 0.03385383280295282959, 0.03645844125268089125, 0.03906229690237970897, 0.04166656525949016115, 0.04427081591349327910, 0.04687468903198145631, 0.04947928942627017462, 0.05208296534865054783, 0.05468764290212216328, 0.05729137561078536528, 0.05989584521530456201, 0.06249987723257615507, 0.06510392926424246607, 0.06770838613806146045, 0.07031213076997053224, 0.07291680575263978503, 0.07552047744215656389, 0.07812508546332513903, 0.08072894086165181837, 0.08333320924388483431, 0.08593745993457323207, 0.08854133291633270453, 0.09114593330519306369, 0.09374960916840779923, 0.09635428668231969807, 0.09895801939011879267, 0.1015624889210437753, 0.1041665209728785957, 0.1067705729027476208, 0.1093750297965602747, 0.1119787743537518920, 0.1145834493281674554, 0.1171871210017138010, 0.1197917289818775377, 0.1223955844170728779, 0.1249998527215379351, 0.1276041034591044177, 0.1302079763611066199, 0.1328125767709825433, 0.1354162526020633861, 0.1380209301064295735, 0.1406246628425296130, 0.1432291323291436380, 0.1458331644451768827, 0.1484372163025670099, 0.1510416732455448496, 0.1536454177576472568, 0.1562500927529001105, 0.1588537644400710158, 0.1614583724083656635, 0.1640622279099430147, 0.1666664961659596600, 0.1692707469797122277, 0.1718746198314790308, 0.1744792202914958457, 0.1770828961200470730, 0.1796875736439581817, 0.1822913064379278192, 0.1848957759094348730, 0.1874998081190861754, 0.1901038599334289314, 0.1927083169547665342, 0.1953120614513534081, 0.1979167364965291054, 0.2005204082269216870, 0.2031250162124720871, 0.2057288718099357372, 0.2083331400468157457, 0.2109373909660553770, 0.2135412637971000893, 0.2161458643363758370, 0.2187495401919937743, 0.2213542177645327069, 0.2239579506459335456, 0.2265624201315297737, 0.2291664524642116896, 0.2317705042649303715, 0.2343749613938155840, 0.2369787059044528299, 0.2395833810286300269, 0.2421870528318344207, 0.2447916608637582536, 0.2473955165866061623, 0.2499997848336539263, 0.2526040358876752157, 0.2552079087275039293, 0.2578125093751503782, 0.2604161852874245509, 0.2630208629376679097, 0.2656245959360551967, 0.2682290654649299166, 0.2708330979500496172, 0.2734371497665608608, 0.2760416070321756732, 0.2786453515864226738, 0.2812500268186742258, 0.2838536987242743503, 0.2864583068316831627, 0.2890621627094078216, 0.2916664309959213219, 0.2942706822140139789, 0.2968745550921262355, 0.2994791558772498252, 0.3020828318757637354, 0.3046875096327826826, 0.3072912427777066413, 0.3098957123790437307, 0.3124997450460035853, 0.3151037969077182255, 0.3177082543392401592, 0.3203119989666507461, 0.3229166743360447622, 0.3255203463736199843, 0.3281249545856204097, 0.3307288106477103140, 0.3333330790029824242, 0.3359373304144318562, 0.3385412033603223403, 0.3411458043120255135, 0.3437494804263583337, 0.3463541583192197293, 0.3489578916402267250, 0.3515623613432052874, 0.3541663942214042238, 0.3567704461577280162, 0.3593749037843310123, 0.3619786485144548260, 0.3645833240500557237, 0.3671869962491814965, 0.3697916045948764219, 0.3723954608708167080, 0.3749997293241361662, 0.3776039809582251716, 0.3802078540013843488, 0.3828124551487663840, 0.3854161314084936785, 0.3880208094662612184, 0.3906245429928945634, 0.3932290128266905938, 0.3958330459455252637, 0.3984370979858605777, 0.4010415558367163569, 0.4036453006990994852, 0.4062499764299690730, 0.4088536488202184072, 0.4114582573287078326, 0.4140621138479816388, 0.4166663824286341855, 0.4192706343146435644, 0.4218745074845589027, 0.4244791088567174686, 0.4270827852914125256, 0.4296874635431477407, 0.4322911973049493040, 0.4348956672987361882, 0.4374997006876018557, 0.4401037528613486738, 0.4427082109656274023, 0.4453119559898139901, 0.4479166319450127998, 0.4505203045559570407, 0.4531249132563394122, 0.4557287700484292658, 0.4583330387856985322, 0.4609372909529084184, 0.4635411642790657205, 0.4661457659050973201, 0.4687494425443319290, 0.4713541210190953512, 0.4739578550456061690, 0.4765623252285562383, 0.4791663589168480009, 0.4817704112534048067, 0.4843748696402766507, 0.4869786148558097882, 0.4895832910643978519, 0.4921869639256079565, 0.4947915728469811647, 0.4973954299413693159, 0.4999996988645384333, 0.5026039513422294602, 0.5052078248541136407, 0.5078124267631153321, 0.5104161036364611714, 0.5130207823633133879, 0.5156245166840751626, 0.5182289870853604707, 0.5208330211024742029, 0.5234370736312391470, 0.5260415323298749390, 0.5286452777662975500, 0.5312499542573357880, 0.5338536273983837122, 0.5364582365698458144, 0.5390620939960163449, 0.5416663631343685559, 0.5442706159518226894, 0.5468744896789192733, 0.5494790918999890028, 0.5520827690370186946, 0.5546874480450217915, 0.5572911826895774468, 0.5598956533383712131, 0.5624996877137050655, 0.5651037404640770756, 0.5677081995036498130, 0.5703119451905063197, 0.5729166219930570403, 0.5755202954435161278, 0.5781249048941674573, 0.5807287626816063364, 0.5833330320644263267, 0.5859372852509285856, 0.5885411592227242084, 0.5911457617849628088, 0.5937494392152512512, 0.5963541185334689798, 0.5989578535313645480, 0.6015623244568418793, 0.6041663592197970001, 0.6067704122211770024, 0.6093748716308627911, 0.6119786175976995590, 0.6145832947408284008, 0.6171869685302752151, 0.6197915782892181591, 0.6223954364674153528, 0.6249997061239902507, 0.6276039597088286515, 0.6302078339548128350, 0.6328124368873246919, 0.6354161146404495586, 0.6380207942979494451, 0.6406245296787346222, 0.6432290009100736228, 0.6458330360900554901, 0.6484370893718474083, 0.6510415491808263511, 0.6536452954571934093, 0.6562499729699700080, 0.6588536471279848872, 0.6614582572243260516, 0.6640621158227759668, 0.6666663857823964534, 0.6692706397948642305, 0.6718745143445301604, 0.6744791176764239893, 0.6770827957819672838, 0.6796874758078212952, 0.6822912116010506622, 0.6848956831674339885, 0.6874997187938534093, 0.6901037723854651640, 0.6927082326229228038, 0.6953119792383747333, 0.6979166571498732763, 0.7005203317060422208, 0.7031249421688929857, 0.7057288012170955804, 0.7083330715090569996, 0.7109373259784533827, 0.7135412008612989077, 0.7161458046216893081, 0.7187494831092385850, 0.7213541635325240176, 0.7239578997677582617, 0.7265623716983737879, 0.7291664078006476757, 0.7317704617314926274, 0.7343749224266207243, 0.7369786694107173242, 0.7395833477500189934, 0.7421870227339337767, 0.7447916335924112952, 0.7473954931198736329, 0.7499997637734774347, 0.7526040187291080930, 0.7552078939746372788, 0.7578124981926457338, 0.7604161770917949870, 0.7630208579415957981, 0.7656245946484027121, 0.7682290669724446408, 0.7708331035799980135, 0.7734371578794957403, 0.7760416190614934928, 0.7786453664438016675, 0.7812500452399944173, 0.7838537206812543623, 0.7864583319644831150, 0.7890621920007202528, 0.7916664630452742157, 0.7942707185164536998, 0.7968745941541772737, 0.7994791988589329268, 0.8020828781992835887, 0.8046875595046918406, 0.8072912967126475436, 0.8098957694593176271, 0.8124998066015838294, 0.8151038612991610144, 0.8177083229972362810, 0.8203120708073305956, 0.8229167500895105958, 0.8255204260177235742, 0.8281250377548363684, 0.8307288983293719120, 0.8333331697941922522, 0.8359374258102438837, 0.8385413018696807885, 0.8411459070903221091, 0.8437495869014844940, 0.8463542686916004643, 0.8489580064302900686, 0.8515624796287988296, 0.8541665173352209761, 0.8567705724603134065, 0.8593750347036837045, 0.8619787829711476057, 0.8645834627684209073, 0.8671871392132045608, 0.8697917514333429745, 0.8723956125757112989, 0.8749998844901232253, 0.8776041410803804288, 0.8802080175910590443, 0.8828126233567346048, 0.8854163036683286858, 0.8880209859722626442, 0.8906247242712825862, 0.8932291979508502067, 0.8958332362508822921, 0.8984372918329353030, 0.9010417546508288078, 0.9036455034052560675, 0.9062501837467389354, 0.9088538607377212308, 0.9114584734700372781, 0.9140623352097841936, 0.9166666076031229071, 0.9192708647969299873, 0.9218747417883903505, 0.9244793481282622682, 0.9270830289699085736, 0.9296877118167798937, 0.9322914507057830091, 0.9348959248956096868, 0.9374999638185942397, 0.9401040198872741005, 0.9427084833090058069, 0.9453122325795346725, 0.9479169134952544207, 0.9505205910598265584, 0.9531252043308329203, 0.9557290667238423909, 0.9583333396063040688, 0.9609375973010293448, 0.9635414750455153499, 0.9661460823481272664, 0.9687497623469286667, 0.9713544456720903941, 0.9739581901020435417, 0.9765626606554614897, 0.9791666924408860551, 0.9817707657828746992, 0.9843752055175947202, 0.9869789906880002128, 0.9895838567146432174, 0.9921867690109741345, 0.9947911791560083428, 0.9973999138825643263, 0.9999999999999998890 ),
 .UNSPECIFIED. ) 
 GEOMETRIC_REPRESENTATION_ITEM ( )  RATIONAL_B_SPLINE_SURFACE ( (
 ( 1.000000000000000222, 1.000000000000000222, 1.000000000000000222, 1.000000000000000222, 1.000000000000000444, 1.000000000000000444, 1.000000000000000222, 1.000000000000000444, 1.000000000000000222, 1.000000000000000444, 1.000000000000000444, 1.000000000000000000, 1.000000000000000222, 1.000000000000000000, 1.000000000000000222, 1.000000000000000222, 1.000000000000000444, 1.000000000000000000, 1.000000000000000444, 1.000000000000000444, 1.000000000000000222, 1.000000000000000222, 1.000000000000000000, 1.000000000000000222, 1.000000000000000000, 1.000000000000000444, 1.000000000000000000, 1.000000000000000444, 1.000000000000000222, 1.000000000000000000, 1.000000000000000666, 1.000000000000000000, 1.000000000000000222, 1.000000000000000666, 1.000000000000000222, 1.000000000000000444, 1.000000000000000222, 1.000000000000000444, 1.000000000000000000, 1.000000000000000444, 1.000000000000000000, 1.000000000000000444, 1.000000000000000000, 1.000000000000000444, 1.000000000000000000, 1.000000000000000222, 1.000000000000000444, 1.000000000000000000, 1.000000000000000444, 1.000000000000000222, 1.000000000000000222, 1.000000000000000444, 1.000000000000000222, 1.000000000000000444, 1.000000000000000222, 1.000000000000000222, 1.000000000000000444, 1.000000000000000444, 1.000000000000000222, 1.000000000000000222, 1.000000000000000444, 1.000000000000000222, 1.000000000000000444, 1.000000000000000000, 1.000000000000000222, 1.000000000000000222, 1.000000000000000222, 1.000000000000000222, 1.000000000000000444, 1.000000000000000000, 0.9999999999999997780, 1.000000000000000444, 1.000000000000000444, 1.000000000000000222, 1.000000000000000222, 1.000000000000000444, 0.9999999999999997780, 1.000000000000000666, 1.000000000000000000, 1.000000000000000000, 1.000000000000000444, 1.000000000000000222, 1.000000000000000222, 0.9999999999999997780, 1.000000000000000222, 1.000000000000000444, 0.9999999999999997780, 1.000000000000000444, 1.000000000000000000, 1.000000000000000000, 1.000000000000000444, 1.000000000000000000, 1.000000000000000444, 1.000000000000000444, 0.9999999999999997780, 1.000000000000000444, 1.000000000000000444, 1.000000000000000444, 1.000000000000000444, 1.000000000000000000, 1.000000000000000444, 1.000000000000000222, 1.000000000000000000, 1.000000000000000444, 1.000000000000000444, 1.000000000000000222, 1.000000000000000000, 1.000000000000000444, 1.000000000000000444, 1.000000000000000000, 1.000000000000000222, 1.000000000000000000, 1.000000000000000444, 1.000000000000000222, 1.000000000000000444, 1.000000000000000222, 1.000000000000000444, 1.000000000000000444, 1.000000000000000000, 1.000000000000000666, 1.000000000000000222, 1.000000000000000222, 1.000000000000000000, 1.000000000000000222, 1.000000000000000222, 1.000000000000000222, 1.000000000000000444, 1.000000000000000222, 1.000000000000000222, 1.000000000000000444, 0.9999999999999997780, 1.000000000000000666, 0.9999999999999997780, 1.000000000000000222, 1.000000000000000000, 1.000000000000000444, 1.000000000000000000, 1.000000000000000444, 1.000000000000000000, 1.000000000000000222, 1.000000000000000222, 1.000000000000000444, 1.000000000000000444, 1.000000000000000222, 1.000000000000000444, 1.000000000000000444, 1.000000000000000000, 1.000000000000000666, 1.000000000000000222, 1.000000000000000222, 1.000000000000000444, 1.000000000000000000, 1.000000000000000222, 1.000000000000000444, 1.000000000000000000, 1.000000000000000222, 1.000000000000000222, 1.000000000000000444, 1.000000000000000222, 1.000000000000000222, 1.000000000000000444, 1.000000000000000000, 1.000000000000000222, 1.000000000000000000, 1.000000000000000444, 1.000000000000000222, 1.000000000000000444, 1.000000000000000222, 1.000000000000000222, 1.000000000000000444, 1.000000000000000000, 1.000000000000000222, 1.000000000000000444, 1.000000000000000000, 1.000000000000000444, 1.000000000000000222, 1.000000000000000444, 1.000000000000000444, 1.000000000000000222, 1.000000000000000222, 1.000000000000000000, 1.000000000000000444, 1.000000000000000444, 1.000000000000000000, 1.000000000000000444, 1.000000000000000222, 1.000000000000000444, 1.000000000000000444, 1.000000000000000222, 1.000000000000000000, 1.000000000000000444, 1.000000000000000222, 1.000000000000000444, 1.000000000000000000, 1.000000000000000444, 1.000000000000000222, 1.000000000000000222, 1.000000000000000444, 1.000000000000000222, 1.000000000000000222, 1.000000000000000222, 1.000000000000000222, 1.000000000000000444, 1.000000000000000000, 1.000000000000000666, 1.000000000000000000, 1.000000000000000222, 1.000000000000000444, 1.000000000000000000, 1.000000000000000222, 1.000000000000000444, 1.000000000000000000, 1.000000000000000666, 0.9999999999999997780, 1.000000000000000222, 1.000000000000000444, 1.000000000000000000, 1.000000000000000444, 1.000000000000000222, 1.000000000000000444, 1.000000000000000000, 1.000000000000000444, 1.000000000000000222, 1.000000000000000222, 1.000000000000000000, 1.000000000000000444, 1.000000000000000222, 1.000000000000000000, 1.000000000000000222, 1.000000000000000222, 1.000000000000000222, 1.000000000000000444, 1.000000000000000000, 1.000000000000000444, 1.000000000000000222, 1.000000000000000222, 1.000000000000000222, 1.000000000000000000, 1.000000000000000666, 1.000000000000000000, 1.000000000000000000, 1.000000000000000222, 1.000000000000000444, 1.000000000000000222, 1.000000000000000444, 0.9999999999999997780, 1.000000000000000444, 1.000000000000000444, 0.9999999999999997780, 1.000000000000000444, 1.000000000000000444, 1.000000000000000444, 1.000000000000000222, 1.000000000000000444, 1.000000000000000444, 1.000000000000000000, 1.000000000000000444, 0.9999999999999997780, 1.000000000000000444, 0.9999999999999997780, 1.000000000000000444, 1.000000000000000000, 1.000000000000000444, 1.000000000000000444, 1.000000000000000444, 1.000000000000000222, 1.000000000000000444, 1.000000000000000444, 1.000000000000000222, 1.000000000000000222, 1.000000000000000000, 1.000000000000000222, 1.000000000000000444, 0.9999999999999997780, 1.000000000000000666, 0.9999999999999997780, 1.000000000000000444, 1.000000000000000222, 1.000000000000000222, 1.000000000000000000, 1.000000000000000222, 1.000000000000000222, 1.000000000000000000, 1.000000000000000000, 1.000000000000000444, 1.000000000000000222, 1.000000000000000444, 0.9999999999999997780, 1.000000000000000444, 1.000000000000000444, 1.000000000000000222, 1.000000000000000444, 1.000000000000000000, 1.000000000000000444, 1.000000000000000444, 0.9999999999999997780, 1.000000000000000444, 1.000000000000000222, 1.000000000000000444, 1.000000000000000222, 1.000000000000000222, 1.000000000000000444, 1.000000000000000000, 1.000000000000000000, 1.000000000000000444, 1.000000000000000444, 1.000000000000000444, 0.9999999999999997780, 1.000000000000000444, 1.000000000000000222, 1.000000000000000222, 1.000000000000000444, 1.000000000000000000, 1.000000000000000444, 1.000000000000000222, 1.000000000000000444, 1.000000000000000000, 1.000000000000000444, 1.000000000000000444, 1.000000000000000444, 1.000000000000000000, 1.000000000000000444, 1.000000000000000000, 1.000000000000000222, 1.000000000000000444, 1.000000000000000444, 1.000000000000000000, 1.000000000000000444, 1.000000000000000444, 1.000000000000000000, 1.000000000000000444, 1.000000000000000222, 1.000000000000000000, 1.000000000000000444, 1.000000000000000222, 1.000000000000000222, 1.000000000000000444, 1.000000000000000444, 1.000000000000000000, 1.000000000000000000, 1.000000000000000444, 1.000000000000000000, 1.000000000000000222, 1.000000000000000444, 1.000000000000000000, 1.000000000000000222, 1.000000000000000444, 0.9999999999999997780, 1.000000000000000444, 1.000000000000000222, 1.000000000000000000, 1.000000000000000444, 1.000000000000000000, 1.000000000000000444, 1.000000000000000444, 1.000000000000000000, 1.000000000000000222, 1.000000000000000222, 1.000000000000000222, 1.000000000000000444, 1.000000000000000222, 1.000000000000000000, 1.000000000000000222, 1.000000000000000444, 1.000000000000000444, 1.000000000000000222, 1.000000000000000444, 1.000000000000000444, 1.000000000000000000, 1.000000000000000000, 1.000000000000000666, 0.9999999999999997780, 1.000000000000000444, 0.9999999999999997780, 1.000000000000000222, 0.9999999999999997780, 1.000000000000000444, 1.000000000000000000, 1.000000000000000222, 1.000000000000000222, 1.000000000000000444, 1.000000000000000000, 1.000000000000000000, 1.000000000000000444, 1.000000000000000000, 1.000000000000000222, 1.000000000000000222),
 ( 0.3333333333333334259, 0.3333333333333334259, 0.3333333333333334814, 0.3333333333333333703, 0.3333333333333335369, 0.3333333333333335369, 0.3333333333333334259, 0.3333333333333334259, 0.3333333333333334259, 0.3333333333333334814, 0.3333333333333334259, 0.3333333333333334259, 0.3333333333333334259, 0.3333333333333334259, 0.3333333333333333148, 0.3333333333333334259, 0.3333333333333334814, 0.3333333333333333703, 0.3333333333333335369, 0.3333333333333335924, 0.3333333333333334259, 0.3333333333333334814, 0.3333333333333333703, 0.3333333333333334259, 0.3333333333333333703, 0.3333333333333334814, 0.3333333333333333703, 0.3333333333333334259, 0.3333333333333333703, 0.3333333333333333703, 0.3333333333333335369, 0.3333333333333334259, 0.3333333333333333703, 0.3333333333333335924, 0.3333333333333334259, 0.3333333333333334259, 0.3333333333333333703, 0.3333333333333334814, 0.3333333333333333703, 0.3333333333333334814, 0.3333333333333333703, 0.3333333333333335369, 0.3333333333333333148, 0.3333333333333334814, 0.3333333333333333703, 0.3333333333333334814, 0.3333333333333334259, 0.3333333333333333703, 0.3333333333333334259, 0.3333333333333334259, 0.3333333333333334814, 0.3333333333333333703, 0.3333333333333335369, 0.3333333333333334259, 0.3333333333333334259, 0.3333333333333334814, 0.3333333333333334259, 0.3333333333333334259, 0.3333333333333333703, 0.3333333333333333703, 0.3333333333333335924, 0.3333333333333334259, 0.3333333333333335369, 0.3333333333333333703, 0.3333333333333333703, 0.3333333333333333703, 0.3333333333333334814, 0.3333333333333333703, 0.3333333333333335369, 0.3333333333333332593, 0.3333333333333333703, 0.3333333333333334259, 0.3333333333333335369, 0.3333333333333334259, 0.3333333333333333703, 0.3333333333333334814, 0.3333333333333333703, 0.3333333333333335369, 0.3333333333333334259, 0.3333333333333333148, 0.3333333333333334814, 0.3333333333333334814, 0.3333333333333334259, 0.3333333333333333148, 0.3333333333333333703, 0.3333333333333334814, 0.3333333333333333703, 0.3333333333333334814, 0.3333333333333333148, 0.3333333333333334259, 0.3333333333333334814, 0.3333333333333333703, 0.3333333333333335369, 0.3333333333333334814, 0.3333333333333333148, 0.3333333333333335369, 0.3333333333333334814, 0.3333333333333334259, 0.3333333333333334814, 0.3333333333333333703, 0.3333333333333334814, 0.3333333333333334259, 0.3333333333333333703, 0.3333333333333334259, 0.3333333333333335369, 0.3333333333333334259, 0.3333333333333334259, 0.3333333333333334814, 0.3333333333333335369, 0.3333333333333333148, 0.3333333333333334259, 0.3333333333333333148, 0.3333333333333335924, 0.3333333333333334259, 0.3333333333333334814, 0.3333333333333333703, 0.3333333333333334814, 0.3333333333333334259, 0.3333333333333333703, 0.3333333333333335924, 0.3333333333333334259, 0.3333333333333334259, 0.3333333333333333703, 0.3333333333333334259, 0.3333333333333333703, 0.3333333333333333703, 0.3333333333333335369, 0.3333333333333334259, 0.3333333333333333703, 0.3333333333333334814, 0.3333333333333333148, 0.3333333333333335924, 0.3333333333333333148, 0.3333333333333334259, 0.3333333333333333148, 0.3333333333333335924, 0.3333333333333333703, 0.3333333333333335369, 0.3333333333333333148, 0.3333333333333334259, 0.3333333333333334814, 0.3333333333333334259, 0.3333333333333334259, 0.3333333333333334259, 0.3333333333333334259, 0.3333333333333334259, 0.3333333333333334259, 0.3333333333333334814, 0.3333333333333334259, 0.3333333333333333703, 0.3333333333333334814, 0.3333333333333333148, 0.3333333333333334259, 0.3333333333333334814, 0.3333333333333334259, 0.3333333333333333703, 0.3333333333333334259, 0.3333333333333334814, 0.3333333333333333703, 0.3333333333333334259, 0.3333333333333334814, 0.3333333333333333703, 0.3333333333333333703, 0.3333333333333333703, 0.3333333333333335369, 0.3333333333333333703, 0.3333333333333334814, 0.3333333333333334259, 0.3333333333333333703, 0.3333333333333334814, 0.3333333333333333703, 0.3333333333333334259, 0.3333333333333335369, 0.3333333333333333703, 0.3333333333333334259, 0.3333333333333334814, 0.3333333333333334259, 0.3333333333333335924, 0.3333333333333333703, 0.3333333333333334259, 0.3333333333333333148, 0.3333333333333335369, 0.3333333333333334259, 0.3333333333333334259, 0.3333333333333334259, 0.3333333333333333703, 0.3333333333333335369, 0.3333333333333334259, 0.3333333333333333703, 0.3333333333333334259, 0.3333333333333334259, 0.3333333333333333703, 0.3333333333333335369, 0.3333333333333333703, 0.3333333333333335369, 0.3333333333333333703, 0.3333333333333334814, 0.3333333333333334259, 0.3333333333333333703, 0.3333333333333334259, 0.3333333333333333703, 0.3333333333333334814, 0.3333333333333334259, 0.3333333333333333703, 0.3333333333333335369, 0.3333333333333333703, 0.3333333333333333703, 0.3333333333333334814, 0.3333333333333333703, 0.3333333333333333148, 0.3333333333333335924, 0.3333333333333333148, 0.3333333333333335924, 0.3333333333333332593, 0.3333333333333334814, 0.3333333333333334814, 0.3333333333333334259, 0.3333333333333334259, 0.3333333333333334814, 0.3333333333333334259, 0.3333333333333333703, 0.3333333333333335369, 0.3333333333333334259, 0.3333333333333334814, 0.3333333333333333703, 0.3333333333333334259, 0.3333333333333333703, 0.3333333333333334814, 0.3333333333333333703, 0.3333333333333335369, 0.3333333333333333148, 0.3333333333333335924, 0.3333333333333333703, 0.3333333333333334259, 0.3333333333333333703, 0.3333333333333334259, 0.3333333333333333703, 0.3333333333333333703, 0.3333333333333335924, 0.3333333333333334259, 0.3333333333333333148, 0.3333333333333334814, 0.3333333333333335369, 0.3333333333333333703, 0.3333333333333334814, 0.3333333333333333703, 0.3333333333333334259, 0.3333333333333335369, 0.3333333333333333148, 0.3333333333333334814, 0.3333333333333334814, 0.3333333333333333703, 0.3333333333333334259, 0.3333333333333334259, 0.3333333333333335369, 0.3333333333333333148, 0.3333333333333335369, 0.3333333333333333148, 0.3333333333333335369, 0.3333333333333332593, 0.3333333333333335924, 0.3333333333333333148, 0.3333333333333335369, 0.3333333333333335369, 0.3333333333333334814, 0.3333333333333334259, 0.3333333333333334814, 0.3333333333333334814, 0.3333333333333334259, 0.3333333333333334259, 0.3333333333333334259, 0.3333333333333334814, 0.3333333333333334259, 0.3333333333333333703, 0.3333333333333334814, 0.3333333333333333703, 0.3333333333333335369, 0.3333333333333333703, 0.3333333333333334259, 0.3333333333333333148, 0.3333333333333334259, 0.3333333333333334259, 0.3333333333333333703, 0.3333333333333333703, 0.3333333333333335924, 0.3333333333333334259, 0.3333333333333335369, 0.3333333333333333148, 0.3333333333333335369, 0.3333333333333334814, 0.3333333333333334259, 0.3333333333333334814, 0.3333333333333334259, 0.3333333333333333703, 0.3333333333333335369, 0.3333333333333333148, 0.3333333333333335369, 0.3333333333333333703, 0.3333333333333335369, 0.3333333333333333703, 0.3333333333333334814, 0.3333333333333334259, 0.3333333333333333703, 0.3333333333333334259, 0.3333333333333333703, 0.3333333333333335924, 0.3333333333333334259, 0.3333333333333333148, 0.3333333333333334259, 0.3333333333333334259, 0.3333333333333334259, 0.3333333333333335924, 0.3333333333333333703, 0.3333333333333334259, 0.3333333333333334259, 0.3333333333333335369, 0.3333333333333333703, 0.3333333333333334814, 0.3333333333333334814, 0.3333333333333334814, 0.3333333333333333703, 0.3333333333333334814, 0.3333333333333333148, 0.3333333333333335369, 0.3333333333333334259, 0.3333333333333334814, 0.3333333333333333703, 0.3333333333333334259, 0.3333333333333334259, 0.3333333333333334259, 0.3333333333333334259, 0.3333333333333333703, 0.3333333333333333703, 0.3333333333333334814, 0.3333333333333333703, 0.3333333333333334259, 0.3333333333333334814, 0.3333333333333334259, 0.3333333333333334259, 0.3333333333333333703, 0.3333333333333334814, 0.3333333333333333703, 0.3333333333333334259, 0.3333333333333335369, 0.3333333333333333148, 0.3333333333333333703, 0.3333333333333334814, 0.3333333333333333148, 0.3333333333333334259, 0.3333333333333333703, 0.3333333333333333703, 0.3333333333333334814, 0.3333333333333333703, 0.3333333333333334259, 0.3333333333333334814, 0.3333333333333333703, 0.3333333333333334259, 0.3333333333333334259, 0.3333333333333334259, 0.3333333333333335369, 0.3333333333333334259, 0.3333333333333334259, 0.3333333333333333703, 0.3333333333333334259, 0.3333333333333334259, 0.3333333333333334259, 0.3333333333333334814, 0.3333333333333335369, 0.3333333333333333148, 0.3333333333333333703, 0.3333333333333335924, 0.3333333333333333148, 0.3333333333333334259, 0.3333333333333334259, 0.3333333333333333703, 0.3333333333333333148, 0.3333333333333335369, 0.3333333333333334259, 0.3333333333333333703, 0.3333333333333334814, 0.3333333333333334259, 0.3333333333333334259, 0.3333333333333333148, 0.3333333333333335369, 0.3333333333333333703, 0.3333333333333334259, 0.3333333333333334259),
 ( 0.3333333333333334259, 0.3333333333333334259, 0.3333333333333334814, 0.3333333333333333703, 0.3333333333333335369, 0.3333333333333335369, 0.3333333333333334259, 0.3333333333333334259, 0.3333333333333334259, 0.3333333333333334814, 0.3333333333333334259, 0.3333333333333334259, 0.3333333333333334259, 0.3333333333333334259, 0.3333333333333333148, 0.3333333333333334259, 0.3333333333333334814, 0.3333333333333333703, 0.3333333333333335369, 0.3333333333333335924, 0.3333333333333334259, 0.3333333333333334814, 0.3333333333333333703, 0.3333333333333334259, 0.3333333333333333703, 0.3333333333333334814, 0.3333333333333333703, 0.3333333333333334259, 0.3333333333333333703, 0.3333333333333333703, 0.3333333333333335369, 0.3333333333333334259, 0.3333333333333333703, 0.3333333333333335924, 0.3333333333333334259, 0.3333333333333334259, 0.3333333333333333703, 0.3333333333333334814, 0.3333333333333333703, 0.3333333333333334814, 0.3333333333333333703, 0.3333333333333335369, 0.3333333333333333148, 0.3333333333333334814, 0.3333333333333333703, 0.3333333333333334814, 0.3333333333333334259, 0.3333333333333333703, 0.3333333333333334259, 0.3333333333333334259, 0.3333333333333334814, 0.3333333333333333703, 0.3333333333333335369, 0.3333333333333334259, 0.3333333333333334259, 0.3333333333333334814, 0.3333333333333334259, 0.3333333333333334259, 0.3333333333333333703, 0.3333333333333333703, 0.3333333333333335924, 0.3333333333333334259, 0.3333333333333335369, 0.3333333333333333703, 0.3333333333333333703, 0.3333333333333333703, 0.3333333333333334814, 0.3333333333333333703, 0.3333333333333335369, 0.3333333333333332593, 0.3333333333333333703, 0.3333333333333334259, 0.3333333333333335369, 0.3333333333333334259, 0.3333333333333333703, 0.3333333333333334814, 0.3333333333333333703, 0.3333333333333335369, 0.3333333333333334259, 0.3333333333333333148, 0.3333333333333334814, 0.3333333333333334814, 0.3333333333333334259, 0.3333333333333333148, 0.3333333333333333703, 0.3333333333333334814, 0.3333333333333333703, 0.3333333333333334814, 0.3333333333333333148, 0.3333333333333334259, 0.3333333333333334814, 0.3333333333333333703, 0.3333333333333335369, 0.3333333333333334814, 0.3333333333333333148, 0.3333333333333335369, 0.3333333333333334814, 0.3333333333333334259, 0.3333333333333334814, 0.3333333333333333703, 0.3333333333333334814, 0.3333333333333334259, 0.3333333333333333703, 0.3333333333333334259, 0.3333333333333335369, 0.3333333333333334259, 0.3333333333333334259, 0.3333333333333334814, 0.3333333333333335369, 0.3333333333333333148, 0.3333333333333334259, 0.3333333333333333148, 0.3333333333333335924, 0.3333333333333334259, 0.3333333333333334814, 0.3333333333333333703, 0.3333333333333334814, 0.3333333333333334259, 0.3333333333333333703, 0.3333333333333335924, 0.3333333333333334259, 0.3333333333333334259, 0.3333333333333333703, 0.3333333333333334259, 0.3333333333333333703, 0.3333333333333333703, 0.3333333333333335369, 0.3333333333333334259, 0.3333333333333333703, 0.3333333333333334814, 0.3333333333333333148, 0.3333333333333335924, 0.3333333333333333148, 0.3333333333333334259, 0.3333333333333333148, 0.3333333333333335924, 0.3333333333333333703, 0.3333333333333335369, 0.3333333333333333148, 0.3333333333333334259, 0.3333333333333334814, 0.3333333333333334259, 0.3333333333333334259, 0.3333333333333334259, 0.3333333333333334259, 0.3333333333333334259, 0.3333333333333334259, 0.3333333333333334814, 0.3333333333333334259, 0.3333333333333333703, 0.3333333333333334814, 0.3333333333333333148, 0.3333333333333334259, 0.3333333333333334814, 0.3333333333333334259, 0.3333333333333333703, 0.3333333333333334259, 0.3333333333333334814, 0.3333333333333333703, 0.3333333333333334259, 0.3333333333333334814, 0.3333333333333333703, 0.3333333333333333703, 0.3333333333333333703, 0.3333333333333335369, 0.3333333333333333703, 0.3333333333333334814, 0.3333333333333334259, 0.3333333333333333703, 0.3333333333333334814, 0.3333333333333333703, 0.3333333333333334259, 0.3333333333333335369, 0.3333333333333333703, 0.3333333333333334259, 0.3333333333333334814, 0.3333333333333334259, 0.3333333333333335924, 0.3333333333333333703, 0.3333333333333334259, 0.3333333333333333148, 0.3333333333333335369, 0.3333333333333334259, 0.3333333333333334259, 0.3333333333333334259, 0.3333333333333333703, 0.3333333333333335369, 0.3333333333333334259, 0.3333333333333333703, 0.3333333333333334259, 0.3333333333333334259, 0.3333333333333333703, 0.3333333333333335369, 0.3333333333333333703, 0.3333333333333335369, 0.3333333333333333703, 0.3333333333333334814, 0.3333333333333334259, 0.3333333333333333703, 0.3333333333333334259, 0.3333333333333333703, 0.3333333333333334814, 0.3333333333333334259, 0.3333333333333333703, 0.3333333333333335369, 0.3333333333333333703, 0.3333333333333333703, 0.3333333333333334814, 0.3333333333333333703, 0.3333333333333333148, 0.3333333333333335924, 0.3333333333333333148, 0.3333333333333335924, 0.3333333333333332593, 0.3333333333333334814, 0.3333333333333334814, 0.3333333333333334259, 0.3333333333333334259, 0.3333333333333334814, 0.3333333333333334259, 0.3333333333333333703, 0.3333333333333335369, 0.3333333333333334259, 0.3333333333333334814, 0.3333333333333333703, 0.3333333333333334259, 0.3333333333333333703, 0.3333333333333334814, 0.3333333333333333703, 0.3333333333333335369, 0.3333333333333333148, 0.3333333333333335924, 0.3333333333333333703, 0.3333333333333334259, 0.3333333333333333703, 0.3333333333333334259, 0.3333333333333333703, 0.3333333333333333703, 0.3333333333333335924, 0.3333333333333334259, 0.3333333333333333148, 0.3333333333333334814, 0.3333333333333335369, 0.3333333333333333703, 0.3333333333333334814, 0.3333333333333333703, 0.3333333333333334259, 0.3333333333333335369, 0.3333333333333333148, 0.3333333333333334814, 0.3333333333333334814, 0.3333333333333333703, 0.3333333333333334259, 0.3333333333333334259, 0.3333333333333335369, 0.3333333333333333148, 0.3333333333333335369, 0.3333333333333333148, 0.3333333333333335369, 0.3333333333333332593, 0.3333333333333335924, 0.3333333333333333148, 0.3333333333333335369, 0.3333333333333335369, 0.3333333333333334814, 0.3333333333333334259, 0.3333333333333334814, 0.3333333333333334814, 0.3333333333333334259, 0.3333333333333334259, 0.3333333333333334259, 0.3333333333333334814, 0.3333333333333334259, 0.3333333333333333703, 0.3333333333333334814, 0.3333333333333333703, 0.3333333333333335369, 0.3333333333333333703, 0.3333333333333334259, 0.3333333333333333148, 0.3333333333333334259, 0.3333333333333334259, 0.3333333333333333703, 0.3333333333333333703, 0.3333333333333335924, 0.3333333333333334259, 0.3333333333333335369, 0.3333333333333333148, 0.3333333333333335369, 0.3333333333333334814, 0.3333333333333334259, 0.3333333333333334814, 0.3333333333333334259, 0.3333333333333333703, 0.3333333333333335369, 0.3333333333333333148, 0.3333333333333335369, 0.3333333333333333703, 0.3333333333333335369, 0.3333333333333333703, 0.3333333333333334814, 0.3333333333333334259, 0.3333333333333333703, 0.3333333333333334259, 0.3333333333333333703, 0.3333333333333335924, 0.3333333333333334259, 0.3333333333333333148, 0.3333333333333334259, 0.3333333333333334259, 0.3333333333333334259, 0.3333333333333335924, 0.3333333333333333703, 0.3333333333333334259, 0.3333333333333334259, 0.3333333333333335369, 0.3333333333333333703, 0.3333333333333334814, 0.3333333333333334814, 0.3333333333333334814, 0.3333333333333333703, 0.3333333333333334814, 0.3333333333333333148, 0.3333333333333335369, 0.3333333333333334259, 0.3333333333333334814, 0.3333333333333333703, 0.3333333333333334259, 0.3333333333333334259, 0.3333333333333334259, 0.3333333333333334259, 0.3333333333333333703, 0.3333333333333333703, 0.3333333333333334814, 0.3333333333333333703, 0.3333333333333334259, 0.3333333333333334814, 0.3333333333333334259, 0.3333333333333334259, 0.3333333333333333703, 0.3333333333333334814, 0.3333333333333333703, 0.3333333333333334259, 0.3333333333333335369, 0.3333333333333333148, 0.3333333333333333703, 0.3333333333333334814, 0.3333333333333333148, 0.3333333333333334259, 0.3333333333333333703, 0.3333333333333333703, 0.3333333333333334814, 0.3333333333333333703, 0.3333333333333334259, 0.3333333333333334814, 0.3333333333333333703, 0.3333333333333334259, 0.3333333333333334259, 0.3333333333333334259, 0.3333333333333335369, 0.3333333333333334259, 0.3333333333333334259, 0.3333333333333333703, 0.3333333333333334259, 0.3333333333333334259, 0.3333333333333334259, 0.3333333333333334814, 0.3333333333333335369, 0.3333333333333333148, 0.3333333333333333703, 0.3333333333333335924, 0.3333333333333333148, 0.3333333333333334259, 0.3333333333333334259, 0.3333333333333333703, 0.3333333333333333148, 0.3333333333333335369, 0.3333333333333334259, 0.3333333333333333703, 0.3333333333333334814, 0.3333333333333334259, 0.3333333333333334259, 0.3333333333333333148, 0.3333333333333335369, 0.3333333333333333703, 0.3333333333333334259, 0.3333333333333334259),
 ( 1.000000000000000222, 1.000000000000000222, 1.000000000000000222, 1.000000000000000222, 1.000000000000000444, 1.000000000000000444, 1.000000000000000222, 1.000000000000000444, 1.000000000000000222, 1.000000000000000444, 1.000000000000000444, 1.000000000000000000, 1.000000000000000222, 1.000000000000000000, 1.000000000000000222, 1.000000000000000222, 1.000000000000000444, 1.000000000000000000, 1.000000000000000444, 1.000000000000000444, 1.000000000000000222, 1.000000000000000222, 1.000000000000000000, 1.000000000000000222, 1.000000000000000000, 1.000000000000000444, 1.000000000000000000, 1.000000000000000444, 1.000000000000000222, 1.000000000000000000, 1.000000000000000666, 1.000000000000000000, 1.000000000000000222, 1.000000000000000666, 1.000000000000000222, 1.000000000000000444, 1.000000000000000222, 1.000000000000000444, 1.000000000000000000, 1.000000000000000444, 1.000000000000000000, 1.000000000000000444, 1.000000000000000000, 1.000000000000000444, 1.000000000000000000, 1.000000000000000222, 1.000000000000000444, 1.000000000000000000, 1.000000000000000444, 1.000000000000000222, 1.000000000000000222, 1.000000000000000444, 1.000000000000000222, 1.000000000000000444, 1.000000000000000222, 1.000000000000000222, 1.000000000000000444, 1.000000000000000444, 1.000000000000000222, 1.000000000000000222, 1.000000000000000444, 1.000000000000000222, 1.000000000000000444, 1.000000000000000000, 1.000000000000000222, 1.000000000000000222, 1.000000000000000222, 1.000000000000000222, 1.000000000000000444, 1.000000000000000000, 0.9999999999999997780, 1.000000000000000444, 1.000000000000000444, 1.000000000000000222, 1.000000000000000222, 1.000000000000000444, 0.9999999999999997780, 1.000000000000000666, 1.000000000000000000, 1.000000000000000000, 1.000000000000000444, 1.000000000000000222, 1.000000000000000222, 0.9999999999999997780, 1.000000000000000222, 1.000000000000000444, 0.9999999999999997780, 1.000000000000000444, 1.000000000000000000, 1.000000000000000000, 1.000000000000000444, 1.000000000000000000, 1.000000000000000444, 1.000000000000000444, 0.9999999999999997780, 1.000000000000000444, 1.000000000000000444, 1.000000000000000444, 1.000000000000000444, 1.000000000000000000, 1.000000000000000444, 1.000000000000000222, 1.000000000000000000, 1.000000000000000444, 1.000000000000000444, 1.000000000000000222, 1.000000000000000000, 1.000000000000000444, 1.000000000000000444, 1.000000000000000000, 1.000000000000000222, 1.000000000000000000, 1.000000000000000444, 1.000000000000000222, 1.000000000000000444, 1.000000000000000222, 1.000000000000000444, 1.000000000000000444, 1.000000000000000000, 1.000000000000000666, 1.000000000000000222, 1.000000000000000222, 1.000000000000000000, 1.000000000000000222, 1.000000000000000222, 1.000000000000000222, 1.000000000000000444, 1.000000000000000222, 1.000000000000000222, 1.000000000000000444, 0.9999999999999997780, 1.000000000000000666, 0.9999999999999997780, 1.000000000000000222, 1.000000000000000000, 1.000000000000000444, 1.000000000000000000, 1.000000000000000444, 1.000000000000000000, 1.000000000000000222, 1.000000000000000222, 1.000000000000000444, 1.000000000000000444, 1.000000000000000222, 1.000000000000000444, 1.000000000000000444, 1.000000000000000000, 1.000000000000000666, 1.000000000000000222, 1.000000000000000222, 1.000000000000000444, 1.000000000000000000, 1.000000000000000222, 1.000000000000000444, 1.000000000000000000, 1.000000000000000222, 1.000000000000000222, 1.000000000000000444, 1.000000000000000222, 1.000000000000000222, 1.000000000000000444, 1.000000000000000000, 1.000000000000000222, 1.000000000000000000, 1.000000000000000444, 1.000000000000000222, 1.000000000000000444, 1.000000000000000222, 1.000000000000000222, 1.000000000000000444, 1.000000000000000000, 1.000000000000000222, 1.000000000000000444, 1.000000000000000000, 1.000000000000000444, 1.000000000000000222, 1.000000000000000444, 1.000000000000000444, 1.000000000000000222, 1.000000000000000222, 1.000000000000000000, 1.000000000000000444, 1.000000000000000444, 1.000000000000000000, 1.000000000000000444, 1.000000000000000222, 1.000000000000000444, 1.000000000000000444, 1.000000000000000222, 1.000000000000000000, 1.000000000000000444, 1.000000000000000222, 1.000000000000000444, 1.000000000000000000, 1.000000000000000444, 1.000000000000000222, 1.000000000000000222, 1.000000000000000444, 1.000000000000000222, 1.000000000000000222, 1.000000000000000222, 1.000000000000000222, 1.000000000000000444, 1.000000000000000000, 1.000000000000000666, 1.000000000000000000, 1.000000000000000222, 1.000000000000000444, 1.000000000000000000, 1.000000000000000222, 1.000000000000000444, 1.000000000000000000, 1.000000000000000666, 0.9999999999999997780, 1.000000000000000222, 1.000000000000000444, 1.000000000000000000, 1.000000000000000444, 1.000000000000000222, 1.000000000000000444, 1.000000000000000000, 1.000000000000000444, 1.000000000000000222, 1.000000000000000222, 1.000000000000000000, 1.000000000000000444, 1.000000000000000222, 1.000000000000000000, 1.000000000000000222, 1.000000000000000222, 1.000000000000000222, 1.000000000000000444, 1.000000000000000000, 1.000000000000000444, 1.000000000000000222, 1.000000000000000222, 1.000000000000000222, 1.000000000000000000, 1.000000000000000666, 1.000000000000000000, 1.000000000000000000, 1.000000000000000222, 1.000000000000000444, 1.000000000000000222, 1.000000000000000444, 0.9999999999999997780, 1.000000000000000444, 1.000000000000000444, 0.9999999999999997780, 1.000000000000000444, 1.000000000000000444, 1.000000000000000444, 1.000000000000000222, 1.000000000000000444, 1.000000000000000444, 1.000000000000000000, 1.000000000000000444, 0.9999999999999997780, 1.000000000000000444, 0.9999999999999997780, 1.000000000000000444, 1.000000000000000000, 1.000000000000000444, 1.000000000000000444, 1.000000000000000444, 1.000000000000000222, 1.000000000000000444, 1.000000000000000444, 1.000000000000000222, 1.000000000000000222, 1.000000000000000000, 1.000000000000000222, 1.000000000000000444, 0.9999999999999997780, 1.000000000000000666, 0.9999999999999997780, 1.000000000000000444, 1.000000000000000222, 1.000000000000000222, 1.000000000000000000, 1.000000000000000222, 1.000000000000000222, 1.000000000000000000, 1.000000000000000000, 1.000000000000000444, 1.000000000000000222, 1.000000000000000444, 0.9999999999999997780, 1.000000000000000444, 1.000000000000000444, 1.000000000000000222, 1.000000000000000444, 1.000000000000000000, 1.000000000000000444, 1.000000000000000444, 0.9999999999999997780, 1.000000000000000444, 1.000000000000000222, 1.000000000000000444, 1.000000000000000222, 1.000000000000000222, 1.000000000000000444, 1.000000000000000000, 1.000000000000000000, 1.000000000000000444, 1.000000000000000444, 1.000000000000000444, 0.9999999999999997780, 1.000000000000000444, 1.000000000000000222, 1.000000000000000222, 1.000000000000000444, 1.000000000000000000, 1.000000000000000444, 1.000000000000000222, 1.000000000000000444, 1.000000000000000000, 1.000000000000000444, 1.000000000000000444, 1.000000000000000444, 1.000000000000000000, 1.000000000000000444, 1.000000000000000000, 1.000000000000000222, 1.000000000000000444, 1.000000000000000444, 1.000000000000000000, 1.000000000000000444, 1.000000000000000444, 1.000000000000000000, 1.000000000000000444, 1.000000000000000222, 1.000000000000000000, 1.000000000000000444, 1.000000000000000222, 1.000000000000000222, 1.000000000000000444, 1.000000000000000444, 1.000000000000000000, 1.000000000000000000, 1.000000000000000444, 1.000000000000000000, 1.000000000000000222, 1.000000000000000444, 1.000000000000000000, 1.000000000000000222, 1.000000000000000444, 0.9999999999999997780, 1.000000000000000444, 1.000000000000000222, 1.000000000000000000, 1.000000000000000444, 1.000000000000000000, 1.000000000000000444, 1.000000000000000444, 1.000000000000000000, 1.000000000000000222, 1.000000000000000222, 1.000000000000000222, 1.000000000000000444, 1.000000000000000222, 1.000000000000000000, 1.000000000000000222, 1.000000000000000444, 1.000000000000000444, 1.000000000000000222, 1.000000000000000444, 1.000000000000000444, 1.000000000000000000, 1.000000000000000000, 1.000000000000000666, 0.9999999999999997780, 1.000000000000000444, 0.9999999999999997780, 1.000000000000000222, 0.9999999999999997780, 1.000000000000000444, 1.000000000000000000, 1.000000000000000222, 1.000000000000000222, 1.000000000000000444, 1.000000000000000000, 1.000000000000000000, 1.000000000000000444, 1.000000000000000000, 1.000000000000000222, 1.000000000000000222),
 ( 0.3333333333333334259, 0.3333333333333334259, 0.3333333333333334814, 0.3333333333333333703, 0.3333333333333335369, 0.3333333333333335369, 0.3333333333333334259, 0.3333333333333334259, 0.3333333333333334259, 0.3333333333333334814, 0.3333333333333334259, 0.3333333333333334259, 0.3333333333333334259, 0.3333333333333334259, 0.3333333333333333148, 0.3333333333333334259, 0.3333333333333334814, 0.3333333333333333703, 0.3333333333333335369, 0.3333333333333335924, 0.3333333333333334259, 0.3333333333333334814, 0.3333333333333333703, 0.3333333333333334259, 0.3333333333333333703, 0.3333333333333334814, 0.3333333333333333703, 0.3333333333333334259, 0.3333333333333333703, 0.3333333333333333703, 0.3333333333333335369, 0.3333333333333334259, 0.3333333333333333703, 0.3333333333333335924, 0.3333333333333334259, 0.3333333333333334259, 0.3333333333333333703, 0.3333333333333334814, 0.3333333333333333703, 0.3333333333333334814, 0.3333333333333333703, 0.3333333333333335369, 0.3333333333333333148, 0.3333333333333334814, 0.3333333333333333703, 0.3333333333333334814, 0.3333333333333334259, 0.3333333333333333703, 0.3333333333333334259, 0.3333333333333334259, 0.3333333333333334814, 0.3333333333333333703, 0.3333333333333335369, 0.3333333333333334259, 0.3333333333333334259, 0.3333333333333334814, 0.3333333333333334259, 0.3333333333333334259, 0.3333333333333333703, 0.3333333333333333703, 0.3333333333333335924, 0.3333333333333334259, 0.3333333333333335369, 0.3333333333333333703, 0.3333333333333333703, 0.3333333333333333703, 0.3333333333333334814, 0.3333333333333333703, 0.3333333333333335369, 0.3333333333333332593, 0.3333333333333333703, 0.3333333333333334259, 0.3333333333333335369, 0.3333333333333334259, 0.3333333333333333703, 0.3333333333333334814, 0.3333333333333333703, 0.3333333333333335369, 0.3333333333333334259, 0.3333333333333333148, 0.3333333333333334814, 0.3333333333333334814, 0.3333333333333334259, 0.3333333333333333148, 0.3333333333333333703, 0.3333333333333334814, 0.3333333333333333703, 0.3333333333333334814, 0.3333333333333333148, 0.3333333333333334259, 0.3333333333333334814, 0.3333333333333333703, 0.3333333333333335369, 0.3333333333333334814, 0.3333333333333333148, 0.3333333333333335369, 0.3333333333333334814, 0.3333333333333334259, 0.3333333333333334814, 0.3333333333333333703, 0.3333333333333334814, 0.3333333333333334259, 0.3333333333333333703, 0.3333333333333334259, 0.3333333333333335369, 0.3333333333333334259, 0.3333333333333334259, 0.3333333333333334814, 0.3333333333333335369, 0.3333333333333333148, 0.3333333333333334259, 0.3333333333333333148, 0.3333333333333335924, 0.3333333333333334259, 0.3333333333333334814, 0.3333333333333333703, 0.3333333333333334814, 0.3333333333333334259, 0.3333333333333333703, 0.3333333333333335924, 0.3333333333333334259, 0.3333333333333334259, 0.3333333333333333703, 0.3333333333333334259, 0.3333333333333333703, 0.3333333333333333703, 0.3333333333333335369, 0.3333333333333334259, 0.3333333333333333703, 0.3333333333333334814, 0.3333333333333333148, 0.3333333333333335924, 0.3333333333333333148, 0.3333333333333334259, 0.3333333333333333148, 0.3333333333333335924, 0.3333333333333333703, 0.3333333333333335369, 0.3333333333333333148, 0.3333333333333334259, 0.3333333333333334814, 0.3333333333333334259, 0.3333333333333334259, 0.3333333333333334259, 0.3333333333333334259, 0.3333333333333334259, 0.3333333333333334259, 0.3333333333333334814, 0.3333333333333334259, 0.3333333333333333703, 0.3333333333333334814, 0.3333333333333333148, 0.3333333333333334259, 0.3333333333333334814, 0.3333333333333334259, 0.3333333333333333703, 0.3333333333333334259, 0.3333333333333334814, 0.3333333333333333703, 0.3333333333333334259, 0.3333333333333334814, 0.3333333333333333703, 0.3333333333333333703, 0.3333333333333333703, 0.3333333333333335369, 0.3333333333333333703, 0.3333333333333334814, 0.3333333333333334259, 0.3333333333333333703, 0.3333333333333334814, 0.3333333333333333703, 0.3333333333333334259, 0.3333333333333335369, 0.3333333333333333703, 0.3333333333333334259, 0.3333333333333334814, 0.3333333333333334259, 0.3333333333333335924, 0.3333333333333333703, 0.3333333333333334259, 0.3333333333333333148, 0.3333333333333335369, 0.3333333333333334259, 0.3333333333333334259, 0.3333333333333334259, 0.3333333333333333703, 0.3333333333333335369, 0.3333333333333334259, 0.3333333333333333703, 0.3333333333333334259, 0.3333333333333334259, 0.3333333333333333703, 0.3333333333333335369, 0.3333333333333333703, 0.3333333333333335369, 0.3333333333333333703, 0.3333333333333334814, 0.3333333333333334259, 0.3333333333333333703, 0.3333333333333334259, 0.3333333333333333703, 0.3333333333333334814, 0.3333333333333334259, 0.3333333333333333703, 0.3333333333333335369, 0.3333333333333333703, 0.3333333333333333703, 0.3333333333333334814, 0.3333333333333333703, 0.3333333333333333148, 0.3333333333333335924, 0.3333333333333333148, 0.3333333333333335924, 0.3333333333333332593, 0.3333333333333334814, 0.3333333333333334814, 0.3333333333333334259, 0.3333333333333334259, 0.3333333333333334814, 0.3333333333333334259, 0.3333333333333333703, 0.3333333333333335369, 0.3333333333333334259, 0.3333333333333334814, 0.3333333333333333703, 0.3333333333333334259, 0.3333333333333333703, 0.3333333333333334814, 0.3333333333333333703, 0.3333333333333335369, 0.3333333333333333148, 0.3333333333333335924, 0.3333333333333333703, 0.3333333333333334259, 0.3333333333333333703, 0.3333333333333334259, 0.3333333333333333703, 0.3333333333333333703, 0.3333333333333335924, 0.3333333333333334259, 0.3333333333333333148, 0.3333333333333334814, 0.3333333333333335369, 0.3333333333333333703, 0.3333333333333334814, 0.3333333333333333703, 0.3333333333333334259, 0.3333333333333335369, 0.3333333333333333148, 0.3333333333333334814, 0.3333333333333334814, 0.3333333333333333703, 0.3333333333333334259, 0.3333333333333334259, 0.3333333333333335369, 0.3333333333333333148, 0.3333333333333335369, 0.3333333333333333148, 0.3333333333333335369, 0.3333333333333332593, 0.3333333333333335924, 0.3333333333333333148, 0.3333333333333335369, 0.3333333333333335369, 0.3333333333333334814, 0.3333333333333334259, 0.3333333333333334814, 0.3333333333333334814, 0.3333333333333334259, 0.3333333333333334259, 0.3333333333333334259, 0.3333333333333334814, 0.3333333333333334259, 0.3333333333333333703, 0.3333333333333334814, 0.3333333333333333703, 0.3333333333333335369, 0.3333333333333333703, 0.3333333333333334259, 0.3333333333333333148, 0.3333333333333334259, 0.3333333333333334259, 0.3333333333333333703, 0.3333333333333333703, 0.3333333333333335924, 0.3333333333333334259, 0.3333333333333335369, 0.3333333333333333148, 0.3333333333333335369, 0.3333333333333334814, 0.3333333333333334259, 0.3333333333333334814, 0.3333333333333334259, 0.3333333333333333703, 0.3333333333333335369, 0.3333333333333333148, 0.3333333333333335369, 0.3333333333333333703, 0.3333333333333335369, 0.3333333333333333703, 0.3333333333333334814, 0.3333333333333334259, 0.3333333333333333703, 0.3333333333333334259, 0.3333333333333333703, 0.3333333333333335924, 0.3333333333333334259, 0.3333333333333333148, 0.3333333333333334259, 0.3333333333333334259, 0.3333333333333334259, 0.3333333333333335924, 0.3333333333333333703, 0.3333333333333334259, 0.3333333333333334259, 0.3333333333333335369, 0.3333333333333333703, 0.3333333333333334814, 0.3333333333333334814, 0.3333333333333334814, 0.3333333333333333703, 0.3333333333333334814, 0.3333333333333333148, 0.3333333333333335369, 0.3333333333333334259, 0.3333333333333334814, 0.3333333333333333703, 0.3333333333333334259, 0.3333333333333334259, 0.3333333333333334259, 0.3333333333333334259, 0.3333333333333333703, 0.3333333333333333703, 0.3333333333333334814, 0.3333333333333333703, 0.3333333333333334259, 0.3333333333333334814, 0.3333333333333334259, 0.3333333333333334259, 0.3333333333333333703, 0.3333333333333334814, 0.3333333333333333703, 0.3333333333333334259, 0.3333333333333335369, 0.3333333333333333148, 0.3333333333333333703, 0.3333333333333334814, 0.3333333333333333148, 0.3333333333333334259, 0.3333333333333333703, 0.3333333333333333703, 0.3333333333333334814, 0.3333333333333333703, 0.3333333333333334259, 0.3333333333333334814, 0.3333333333333333703, 0.3333333333333334259, 0.3333333333333334259, 0.3333333333333334259, 0.3333333333333335369, 0.3333333333333334259, 0.3333333333333334259, 0.3333333333333333703, 0.3333333333333334259, 0.3333333333333334259, 0.3333333333333334259, 0.3333333333333334814, 0.3333333333333335369, 0.3333333333333333148, 0.3333333333333333703, 0.3333333333333335924, 0.3333333333333333148, 0.3333333333333334259, 0.3333333333333334259, 0.3333333333333333703, 0.3333333333333333148, 0.3333333333333335369, 0.3333333333333334259, 0.3333333333333333703, 0.3333333333333334814, 0.3333333333333334259, 0.3333333333333334259, 0.3333333333333333148, 0.3333333333333335369, 0.3333333333333333703, 0.3333333333333334259, 0.3333333333333334259),
 ( 0.3333333333333334259, 0.3333333333333334259, 0.3333333333333334814, 0.3333333333333333703, 0.3333333333333335369, 0.3333333333333335369, 0.3333333333333334259, 0.3333333333333334259, 0.3333333333333334259, 0.3333333333333334814, 0.3333333333333334259, 0.3333333333333334259, 0.3333333333333334259, 0.3333333333333334259, 0.3333333333333333148, 0.3333333333333334259, 0.3333333333333334814, 0.3333333333333333703, 0.3333333333333335369, 0.3333333333333335924, 0.3333333333333334259, 0.3333333333333334814, 0.3333333333333333703, 0.3333333333333334259, 0.3333333333333333703, 0.3333333333333334814, 0.3333333333333333703, 0.3333333333333334259, 0.3333333333333333703, 0.3333333333333333703, 0.3333333333333335369, 0.3333333333333334259, 0.3333333333333333703, 0.3333333333333335924, 0.3333333333333334259, 0.3333333333333334259, 0.3333333333333333703, 0.3333333333333334814, 0.3333333333333333703, 0.3333333333333334814, 0.3333333333333333703, 0.3333333333333335369, 0.3333333333333333148, 0.3333333333333334814, 0.3333333333333333703, 0.3333333333333334814, 0.3333333333333334259, 0.3333333333333333703, 0.3333333333333334259, 0.3333333333333334259, 0.3333333333333334814, 0.3333333333333333703, 0.3333333333333335369, 0.3333333333333334259, 0.3333333333333334259, 0.3333333333333334814, 0.3333333333333334259, 0.3333333333333334259, 0.3333333333333333703, 0.3333333333333333703, 0.3333333333333335924, 0.3333333333333334259, 0.3333333333333335369, 0.3333333333333333703, 0.3333333333333333703, 0.3333333333333333703, 0.3333333333333334814, 0.3333333333333333703, 0.3333333333333335369, 0.3333333333333332593, 0.3333333333333333703, 0.3333333333333334259, 0.3333333333333335369, 0.3333333333333334259, 0.3333333333333333703, 0.3333333333333334814, 0.3333333333333333703, 0.3333333333333335369, 0.3333333333333334259, 0.3333333333333333148, 0.3333333333333334814, 0.3333333333333334814, 0.3333333333333334259, 0.3333333333333333148, 0.3333333333333333703, 0.3333333333333334814, 0.3333333333333333703, 0.3333333333333334814, 0.3333333333333333148, 0.3333333333333334259, 0.3333333333333334814, 0.3333333333333333703, 0.3333333333333335369, 0.3333333333333334814, 0.3333333333333333148, 0.3333333333333335369, 0.3333333333333334814, 0.3333333333333334259, 0.3333333333333334814, 0.3333333333333333703, 0.3333333333333334814, 0.3333333333333334259, 0.3333333333333333703, 0.3333333333333334259, 0.3333333333333335369, 0.3333333333333334259, 0.3333333333333334259, 0.3333333333333334814, 0.3333333333333335369, 0.3333333333333333148, 0.3333333333333334259, 0.3333333333333333148, 0.3333333333333335924, 0.3333333333333334259, 0.3333333333333334814, 0.3333333333333333703, 0.3333333333333334814, 0.3333333333333334259, 0.3333333333333333703, 0.3333333333333335924, 0.3333333333333334259, 0.3333333333333334259, 0.3333333333333333703, 0.3333333333333334259, 0.3333333333333333703, 0.3333333333333333703, 0.3333333333333335369, 0.3333333333333334259, 0.3333333333333333703, 0.3333333333333334814, 0.3333333333333333148, 0.3333333333333335924, 0.3333333333333333148, 0.3333333333333334259, 0.3333333333333333148, 0.3333333333333335924, 0.3333333333333333703, 0.3333333333333335369, 0.3333333333333333148, 0.3333333333333334259, 0.3333333333333334814, 0.3333333333333334259, 0.3333333333333334259, 0.3333333333333334259, 0.3333333333333334259, 0.3333333333333334259, 0.3333333333333334259, 0.3333333333333334814, 0.3333333333333334259, 0.3333333333333333703, 0.3333333333333334814, 0.3333333333333333148, 0.3333333333333334259, 0.3333333333333334814, 0.3333333333333334259, 0.3333333333333333703, 0.3333333333333334259, 0.3333333333333334814, 0.3333333333333333703, 0.3333333333333334259, 0.3333333333333334814, 0.3333333333333333703, 0.3333333333333333703, 0.3333333333333333703, 0.3333333333333335369, 0.3333333333333333703, 0.3333333333333334814, 0.3333333333333334259, 0.3333333333333333703, 0.3333333333333334814, 0.3333333333333333703, 0.3333333333333334259, 0.3333333333333335369, 0.3333333333333333703, 0.3333333333333334259, 0.3333333333333334814, 0.3333333333333334259, 0.3333333333333335924, 0.3333333333333333703, 0.3333333333333334259, 0.3333333333333333148, 0.3333333333333335369, 0.3333333333333334259, 0.3333333333333334259, 0.3333333333333334259, 0.3333333333333333703, 0.3333333333333335369, 0.3333333333333334259, 0.3333333333333333703, 0.3333333333333334259, 0.3333333333333334259, 0.3333333333333333703, 0.3333333333333335369, 0.3333333333333333703, 0.3333333333333335369, 0.3333333333333333703, 0.3333333333333334814, 0.3333333333333334259, 0.3333333333333333703, 0.3333333333333334259, 0.3333333333333333703, 0.3333333333333334814, 0.3333333333333334259, 0.3333333333333333703, 0.3333333333333335369, 0.3333333333333333703, 0.3333333333333333703, 0.3333333333333334814, 0.3333333333333333703, 0.3333333333333333148, 0.3333333333333335924, 0.3333333333333333148, 0.3333333333333335924, 0.3333333333333332593, 0.3333333333333334814, 0.3333333333333334814, 0.3333333333333334259, 0.3333333333333334259, 0.3333333333333334814, 0.3333333333333334259, 0.3333333333333333703, 0.3333333333333335369, 0.3333333333333334259, 0.3333333333333334814, 0.3333333333333333703, 0.3333333333333334259, 0.3333333333333333703, 0.3333333333333334814, 0.3333333333333333703, 0.3333333333333335369, 0.3333333333333333148, 0.3333333333333335924, 0.3333333333333333703, 0.3333333333333334259, 0.3333333333333333703, 0.3333333333333334259, 0.3333333333333333703, 0.3333333333333333703, 0.3333333333333335924, 0.3333333333333334259, 0.3333333333333333148, 0.3333333333333334814, 0.3333333333333335369, 0.3333333333333333703, 0.3333333333333334814, 0.3333333333333333703, 0.3333333333333334259, 0.3333333333333335369, 0.3333333333333333148, 0.3333333333333334814, 0.3333333333333334814, 0.3333333333333333703, 0.3333333333333334259, 0.3333333333333334259, 0.3333333333333335369, 0.3333333333333333148, 0.3333333333333335369, 0.3333333333333333148, 0.3333333333333335369, 0.3333333333333332593, 0.3333333333333335924, 0.3333333333333333148, 0.3333333333333335369, 0.3333333333333335369, 0.3333333333333334814, 0.3333333333333334259, 0.3333333333333334814, 0.3333333333333334814, 0.3333333333333334259, 0.3333333333333334259, 0.3333333333333334259, 0.3333333333333334814, 0.3333333333333334259, 0.3333333333333333703, 0.3333333333333334814, 0.3333333333333333703, 0.3333333333333335369, 0.3333333333333333703, 0.3333333333333334259, 0.3333333333333333148, 0.3333333333333334259, 0.3333333333333334259, 0.3333333333333333703, 0.3333333333333333703, 0.3333333333333335924, 0.3333333333333334259, 0.3333333333333335369, 0.3333333333333333148, 0.3333333333333335369, 0.3333333333333334814, 0.3333333333333334259, 0.3333333333333334814, 0.3333333333333334259, 0.3333333333333333703, 0.3333333333333335369, 0.3333333333333333148, 0.3333333333333335369, 0.3333333333333333703, 0.3333333333333335369, 0.3333333333333333703, 0.3333333333333334814, 0.3333333333333334259, 0.3333333333333333703, 0.3333333333333334259, 0.3333333333333333703, 0.3333333333333335924, 0.3333333333333334259, 0.3333333333333333148, 0.3333333333333334259, 0.3333333333333334259, 0.3333333333333334259, 0.3333333333333335924, 0.3333333333333333703, 0.3333333333333334259, 0.3333333333333334259, 0.3333333333333335369, 0.3333333333333333703, 0.3333333333333334814, 0.3333333333333334814, 0.3333333333333334814, 0.3333333333333333703, 0.3333333333333334814, 0.3333333333333333148, 0.3333333333333335369, 0.3333333333333334259, 0.3333333333333334814, 0.3333333333333333703, 0.3333333333333334259, 0.3333333333333334259, 0.3333333333333334259, 0.3333333333333334259, 0.3333333333333333703, 0.3333333333333333703, 0.3333333333333334814, 0.3333333333333333703, 0.3333333333333334259, 0.3333333333333334814, 0.3333333333333334259, 0.3333333333333334259, 0.3333333333333333703, 0.3333333333333334814, 0.3333333333333333703, 0.3333333333333334259, 0.3333333333333335369, 0.3333333333333333148, 0.3333333333333333703, 0.3333333333333334814, 0.3333333333333333148, 0.3333333333333334259, 0.3333333333333333703, 0.3333333333333333703, 0.3333333333333334814, 0.3333333333333333703, 0.3333333333333334259, 0.3333333333333334814, 0.3333333333333333703, 0.3333333333333334259, 0.3333333333333334259, 0.3333333333333334259, 0.3333333333333335369, 0.3333333333333334259, 0.3333333333333334259, 0.3333333333333333703, 0.3333333333333334259, 0.3333333333333334259, 0.3333333333333334259, 0.3333333333333334814, 0.3333333333333335369, 0.3333333333333333148, 0.3333333333333333703, 0.3333333333333335924, 0.3333333333333333148, 0.3333333333333334259, 0.3333333333333334259, 0.3333333333333333703, 0.3333333333333333148, 0.3333333333333335369, 0.3333333333333334259, 0.3333333333333333703, 0.3333333333333334814, 0.3333333333333334259, 0.3333333333333334259, 0.3333333333333333148, 0.3333333333333335369, 0.3333333333333333703, 0.3333333333333334259, 0.3333333333333334259),
 ( 1.000000000000000222, 1.000000000000000222, 1.000000000000000222, 1.000000000000000222, 1.000000000000000444, 1.000000000000000444, 1.000000000000000222, 1.000000000000000444, 1.000000000000000222, 1.000000000000000444, 1.000000000000000444, 1.000000000000000000, 1.000000000000000222, 1.000000000000000000, 1.000000000000000222, 1.000000000000000222, 1.000000000000000444, 1.000000000000000000, 1.000000000000000444, 1.000000000000000444, 1.000000000000000222, 1.000000000000000222, 1.000000000000000000, 1.000000000000000222, 1.000000000000000000, 1.000000000000000444, 1.000000000000000000, 1.000000000000000444, 1.000000000000000222, 1.000000000000000000, 1.000000000000000666, 1.000000000000000000, 1.000000000000000222, 1.000000000000000666, 1.000000000000000222, 1.000000000000000444, 1.000000000000000222, 1.000000000000000444, 1.000000000000000000, 1.000000000000000444, 1.000000000000000000, 1.000000000000000444, 1.000000000000000000, 1.000000000000000444, 1.000000000000000000, 1.000000000000000222, 1.000000000000000444, 1.000000000000000000, 1.000000000000000444, 1.000000000000000222, 1.000000000000000222, 1.000000000000000444, 1.000000000000000222, 1.000000000000000444, 1.000000000000000222, 1.000000000000000222, 1.000000000000000444, 1.000000000000000444, 1.000000000000000222, 1.000000000000000222, 1.000000000000000444, 1.000000000000000222, 1.000000000000000444, 1.000000000000000000, 1.000000000000000222, 1.000000000000000222, 1.000000000000000222, 1.000000000000000222, 1.000000000000000444, 1.000000000000000000, 0.9999999999999997780, 1.000000000000000444, 1.000000000000000444, 1.000000000000000222, 1.000000000000000222, 1.000000000000000444, 0.9999999999999997780, 1.000000000000000666, 1.000000000000000000, 1.000000000000000000, 1.000000000000000444, 1.000000000000000222, 1.000000000000000222, 0.9999999999999997780, 1.000000000000000222, 1.000000000000000444, 0.9999999999999997780, 1.000000000000000444, 1.000000000000000000, 1.000000000000000000, 1.000000000000000444, 1.000000000000000000, 1.000000000000000444, 1.000000000000000444, 0.9999999999999997780, 1.000000000000000444, 1.000000000000000444, 1.000000000000000444, 1.000000000000000444, 1.000000000000000000, 1.000000000000000444, 1.000000000000000222, 1.000000000000000000, 1.000000000000000444, 1.000000000000000444, 1.000000000000000222, 1.000000000000000000, 1.000000000000000444, 1.000000000000000444, 1.000000000000000000, 1.000000000000000222, 1.000000000000000000, 1.000000000000000444, 1.000000000000000222, 1.000000000000000444, 1.000000000000000222, 1.000000000000000444, 1.000000000000000444, 1.000000000000000000, 1.000000000000000666, 1.000000000000000222, 1.000000000000000222, 1.000000000000000000, 1.000000000000000222, 1.000000000000000222, 1.000000000000000222, 1.000000000000000444, 1.000000000000000222, 1.000000000000000222, 1.000000000000000444, 0.9999999999999997780, 1.000000000000000666, 0.9999999999999997780, 1.000000000000000222, 1.000000000000000000, 1.000000000000000444, 1.000000000000000000, 1.000000000000000444, 1.000000000000000000, 1.000000000000000222, 1.000000000000000222, 1.000000000000000444, 1.000000000000000444, 1.000000000000000222, 1.000000000000000444, 1.000000000000000444, 1.000000000000000000, 1.000000000000000666, 1.000000000000000222, 1.000000000000000222, 1.000000000000000444, 1.000000000000000000, 1.000000000000000222, 1.000000000000000444, 1.000000000000000000, 1.000000000000000222, 1.000000000000000222, 1.000000000000000444, 1.000000000000000222, 1.000000000000000222, 1.000000000000000444, 1.000000000000000000, 1.000000000000000222, 1.000000000000000000, 1.000000000000000444, 1.000000000000000222, 1.000000000000000444, 1.000000000000000222, 1.000000000000000222, 1.000000000000000444, 1.000000000000000000, 1.000000000000000222, 1.000000000000000444, 1.000000000000000000, 1.000000000000000444, 1.000000000000000222, 1.000000000000000444, 1.000000000000000444, 1.000000000000000222, 1.000000000000000222, 1.000000000000000000, 1.000000000000000444, 1.000000000000000444, 1.000000000000000000, 1.000000000000000444, 1.000000000000000222, 1.000000000000000444, 1.000000000000000444, 1.000000000000000222, 1.000000000000000000, 1.000000000000000444, 1.000000000000000222, 1.000000000000000444, 1.000000000000000000, 1.000000000000000444, 1.000000000000000222, 1.000000000000000222, 1.000000000000000444, 1.000000000000000222, 1.000000000000000222, 1.000000000000000222, 1.000000000000000222, 1.000000000000000444, 1.000000000000000000, 1.000000000000000666, 1.000000000000000000, 1.000000000000000222, 1.000000000000000444, 1.000000000000000000, 1.000000000000000222, 1.000000000000000444, 1.000000000000000000, 1.000000000000000666, 0.9999999999999997780, 1.000000000000000222, 1.000000000000000444, 1.000000000000000000, 1.000000000000000444, 1.000000000000000222, 1.000000000000000444, 1.000000000000000000, 1.000000000000000444, 1.000000000000000222, 1.000000000000000222, 1.000000000000000000, 1.000000000000000444, 1.000000000000000222, 1.000000000000000000, 1.000000000000000222, 1.000000000000000222, 1.000000000000000222, 1.000000000000000444, 1.000000000000000000, 1.000000000000000444, 1.000000000000000222, 1.000000000000000222, 1.000000000000000222, 1.000000000000000000, 1.000000000000000666, 1.000000000000000000, 1.000000000000000000, 1.000000000000000222, 1.000000000000000444, 1.000000000000000222, 1.000000000000000444, 0.9999999999999997780, 1.000000000000000444, 1.000000000000000444, 0.9999999999999997780, 1.000000000000000444, 1.000000000000000444, 1.000000000000000444, 1.000000000000000222, 1.000000000000000444, 1.000000000000000444, 1.000000000000000000, 1.000000000000000444, 0.9999999999999997780, 1.000000000000000444, 0.9999999999999997780, 1.000000000000000444, 1.000000000000000000, 1.000000000000000444, 1.000000000000000444, 1.000000000000000444, 1.000000000000000222, 1.000000000000000444, 1.000000000000000444, 1.000000000000000222, 1.000000000000000222, 1.000000000000000000, 1.000000000000000222, 1.000000000000000444, 0.9999999999999997780, 1.000000000000000666, 0.9999999999999997780, 1.000000000000000444, 1.000000000000000222, 1.000000000000000222, 1.000000000000000000, 1.000000000000000222, 1.000000000000000222, 1.000000000000000000, 1.000000000000000000, 1.000000000000000444, 1.000000000000000222, 1.000000000000000444, 0.9999999999999997780, 1.000000000000000444, 1.000000000000000444, 1.000000000000000222, 1.000000000000000444, 1.000000000000000000, 1.000000000000000444, 1.000000000000000444, 0.9999999999999997780, 1.000000000000000444, 1.000000000000000222, 1.000000000000000444, 1.000000000000000222, 1.000000000000000222, 1.000000000000000444, 1.000000000000000000, 1.000000000000000000, 1.000000000000000444, 1.000000000000000444, 1.000000000000000444, 0.9999999999999997780, 1.000000000000000444, 1.000000000000000222, 1.000000000000000222, 1.000000000000000444, 1.000000000000000000, 1.000000000000000444, 1.000000000000000222, 1.000000000000000444, 1.000000000000000000, 1.000000000000000444, 1.000000000000000444, 1.000000000000000444, 1.000000000000000000, 1.000000000000000444, 1.000000000000000000, 1.000000000000000222, 1.000000000000000444, 1.000000000000000444, 1.000000000000000000, 1.000000000000000444, 1.000000000000000444, 1.000000000000000000, 1.000000000000000444, 1.000000000000000222, 1.000000000000000000, 1.000000000000000444, 1.000000000000000222, 1.000000000000000222, 1.000000000000000444, 1.000000000000000444, 1.000000000000000000, 1.000000000000000000, 1.000000000000000444, 1.000000000000000000, 1.000000000000000222, 1.000000000000000444, 1.000000000000000000, 1.000000000000000222, 1.000000000000000444, 0.9999999999999997780, 1.000000000000000444, 1.000000000000000222, 1.000000000000000000, 1.000000000000000444, 1.000000000000000000, 1.000000000000000444, 1.000000000000000444, 1.000000000000000000, 1.000000000000000222, 1.000000000000000222, 1.000000000000000222, 1.000000000000000444, 1.000000000000000222, 1.000000000000000000, 1.000000000000000222, 1.000000000000000444, 1.000000000000000444, 1.000000000000000222, 1.000000000000000444, 1.000000000000000444, 1.000000000000000000, 1.000000000000000000, 1.000000000000000666, 0.9999999999999997780, 1.000000000000000444, 0.9999999999999997780, 1.000000000000000222, 0.9999999999999997780, 1.000000000000000444, 1.000000000000000000, 1.000000000000000222, 1.000000000000000222, 1.000000000000000444, 1.000000000000000000, 1.000000000000000000, 1.000000000000000444, 1.000000000000000000, 1.000000000000000222, 1.000000000000000222) ) ) 
 REPRESENTATION_ITEM ( '' )  SURFACE ( )  );
#51154 = ORIENTED_EDGE ( 'NONE', *, *, #207587, .T. ) ;
#51155 = CARTESIAN_POINT ( 'NONE',  ( 4.055163089163640322, -1.574157218682000758, 0.8962264629079966793 ) ) ;
#51156 = ORIENTED_EDGE ( 'NONE', *, *, #15800, .T. ) ;
#51157 = CARTESIAN_POINT ( 'NONE',  ( 7.503511670520385479, 7.718794801887437274, 0.7998128361456281477 ) ) ;
#51158 = CARTESIAN_POINT ( 'NONE',  ( -5.403060590669224617, 6.145745408126818354, 1.120749285529927697 ) ) ;
#51159 = CARTESIAN_POINT ( 'NONE',  ( 5.356058406599743194, 0.7285399314688314476, -1.658701577940960847 ) ) ;
#51160 = CARTESIAN_POINT ( 'NONE',  ( 5.682275777458841048, 8.683053269460405232, 1.082531754730547524 ) ) ;
#51161 = DIRECTION ( 'NONE',  ( 0.000000000000000000, 0.000000000000000000, 1.000000000000000000 ) ) ;
#51162 = CARTESIAN_POINT ( 'NONE',  ( 4.872649465673598357, 6.683545894502381124, -1.250567445346082218 ) ) ;
#51163 = ORIENTED_EDGE ( 'NONE', *, *, #101713, .T. ) ;
#51164 = VECTOR ( 'NONE', #16224, 1000.000000000000000 ) ;
#51166 = CARTESIAN_POINT ( 'NONE',  ( 8.028399517586572998, 12.51821653715971472, -0.7998128361456352531 ) ) ;
#51165 = CARTESIAN_POINT ( 'NONE',  ( 6.021894344906984387, 1.833355594513026876, -0.3188260975769128813 ) ) ;
#51167 = CARTESIAN_POINT ( 'NONE',  ( 4.042530882030176187, -1.416877165883747125, 1.289359272694647451 ) ) ;
#51168 = CARTESIAN_POINT ( 'NONE',  ( -11.43645483535884999, 5.654992568747732484, -5.469194708833876817 ) ) ;
#51169 = CARTESIAN_POINT ( 'NONE',  ( 9.499701791763563108, -9.918130724412307586, -0.07530116296179023561 ) ) ;
#51170 = CARTESIAN_POINT ( 'NONE',  ( 1.364683531249986537, -0.8864583329919110133, 0.7879004041258500513 ) ) ;
#51171 = CARTESIAN_POINT ( 'NONE',  ( 6.643132081016125845, 6.852668304048034287, 0.7216878364870317197 ) ) ;
#51172 = CARTESIAN_POINT ( 'NONE',  ( -10.48008955368359629, 11.32911868882677986, 1.040834085586084257E-14 ) ) ;
#51173 = CARTESIAN_POINT ( 'NONE',  ( 0.6905621207787122628, -2.145541755201633372, -0.2633910710312590275 ) ) ;
#51174 = CARTESIAN_POINT ( 'NONE',  ( -5.472651281771599763, 6.413789912602166687, 1.199719254218452935 ) ) ;
#51175 = CARTESIAN_POINT ( 'NONE',  ( 4.532168488718122390, 8.509556680138327778, 0.7998128361456271485 ) ) ;
#51176 = CARTESIAN_POINT ( 'NONE',  ( 0.4108170757193031486, 1.585627777896590151, 0.9046078287104839522 ) ) ;
#51177 = CARTESIAN_POINT ( 'NONE',  ( -4.253507506385335368, 5.985511395581417204, 1.599625672291267398 ) ) ;
#51178 = CARTESIAN_POINT ( 'NONE',  ( 3.153144192703428939, -1.491587519860730460, -1.052284964708279258 ) ) ;
#51179 = CARTESIAN_POINT ( 'NONE',  ( 9.808998241650231265, 12.88675894182173387, 8.003755498086194464 ) ) ;
#51180 = CARTESIAN_POINT ( 'NONE',  ( 1.687617486097678476, 1.829050272730630144, -0.5582976189952293389 ) ) ;
#51181 = VERTEX_POINT ( 'NONE', #202907 ) ;
#51182 = CARTESIAN_POINT ( 'NONE',  ( 2.945709429406599966, 1.390870048597905084, 1.394762357610879855 ) ) ;
#51183 = CARTESIAN_POINT ( 'NONE',  ( 5.161643714676827699, 0.9607356898342777063, 1.687723941809249117 ) ) ;
#51184 = CARTESIAN_POINT ( 'NONE',  ( -6.831329296439251131, 9.063246493969506545, -1.599625672291271394 ) ) ;
#51186 = CARTESIAN_POINT ( 'NONE',  ( 3.674183785563363447, 2.104178206457421485, -0.2630699042918820396 ) ) ;
#51185 = CARTESIAN_POINT ( 'NONE',  ( 6.373214726875630731, 9.593111727067046957, 1.199719254218452047 ) ) ;
#51187 = CARTESIAN_POINT ( 'NONE',  ( -3.853900823548705112, 8.531065964594302997, -2.447540105570083391 ) ) ;
#51188 = CARTESIAN_POINT ( 'NONE',  ( 9.531545685607134999, 11.07889037375188401, 1.199719254218450271 ) ) ;
#51189 = CARTESIAN_POINT ( 'NONE',  ( 5.769745475479523655, 6.237591007168648005, 1.002400605009654111 ) ) ;
#51190 = PLANE ( 'NONE',  #94333 ) ;
#51191 = VERTEX_POINT ( 'NONE', #105465 ) ;
#51193 = CIRCLE ( 'NONE', #172263, 0.04999999999999969746 ) ;
#51192 = CARTESIAN_POINT ( 'NONE',  ( -3.542975373178607779, 14.48034456167257744, 11.47372972533055524 ) ) ;
#51194 = CARTESIAN_POINT ( 'NONE',  ( 4.716257332707354699, 6.595662536282280719, -1.599625672291269396 ) ) ;
#51195 = CARTESIAN_POINT ( 'NONE',  ( 4.416205349749311004, 6.175325546172740765, 1.599625672291267398 ) ) ;
#51196 = CARTESIAN_POINT ( 'NONE',  ( 4.875038752565570732, 7.845239757038595663, -1.199719254218452047 ) ) ;
#51197 = CARTESIAN_POINT ( 'NONE',  ( 11.95359438121989726, 12.49578100291300053, -1.059536798430469107 ) ) ;
#51198 = CARTESIAN_POINT ( 'NONE',  ( 4.512205841073367196, -0.7830535718562798841, -1.649371741558727678 ) ) ;
#51199 = CARTESIAN_POINT ( 'NONE',  ( -4.322138105957580301, 3.567377917394196629, 2.444429911049618820 ) ) ;
#51200 = CARTESIAN_POINT ( 'NONE',  ( -7.510853912290736289, 11.70648729774046792, 0.7216878364870458196 ) ) ;
#51201 = CARTESIAN_POINT ( 'NONE',  ( -6.602617837901656017, 6.766230214585198688, 0.2136612715164920018 ) ) ;
#51202 = DIRECTION ( 'NONE',  ( 0.000000000000000000, 0.000000000000000000, 1.000000000000000000 ) ) ;
#51203 = CARTESIAN_POINT ( 'NONE',  ( 5.541831131927607679, 0.7570117910807551143, -1.710825945835430462 ) ) ;
#51204 = CARTESIAN_POINT ( 'NONE',  ( 5.926885707468349196, 10.06645042535509660, 1.040834085586084257E-14 ) ) ;
#51205 = CARTESIAN_POINT ( 'NONE',  ( -3.601662362724658895, 7.353689856487406473, -0.7998128361456282587 ) ) ;
#51206 = VECTOR ( 'NONE', #21381, 1000.000000000000000 ) ;
#51207 = CARTESIAN_POINT ( 'NONE',  ( 3.897079088924235712, 6.634010472798538949, 1.199719254218462483 ) ) ;
#51208 = CARTESIAN_POINT ( 'NONE',  ( -8.012344526598182026E-15, 9.859375000341399797, -1.575800808251669460 ) ) ;
#51209 = CARTESIAN_POINT ( 'NONE',  ( -5.494078562035765501, 7.432844293840273231, -1.599625672291256295 ) ) ;
#51210 = CARTESIAN_POINT ( 'NONE',  ( 2.900554798319789906, 5.471398800426671372, 1.199719254218452047 ) ) ;
#51211 = CARTESIAN_POINT ( 'NONE',  ( -4.136646265500970365, 5.919449624541475607, -1.443375672974066548 ) ) ;
#51212 = CARTESIAN_POINT ( 'NONE',  ( 0.4618902312403838639, -0.5555351291045197426, 1.994226918997483500 ) ) ;
#51213 = CARTESIAN_POINT ( 'NONE',  ( 0.6677574575255783573, 1.425215384571768551, 1.565850431965072787 ) ) ;
#51214 = CARTESIAN_POINT ( 'NONE',  ( 7.567422294721922960, 11.98040977715095323, 0.7998128361456462443 ) ) ;
#51215 = CARTESIAN_POINT ( 'NONE',  ( 0.1100172516615150753, 7.047065462482141385, 3.945011421259202677 ) ) ;
#51216 = CARTESIAN_POINT ( 'NONE',  ( 5.840704046183605946, -2.018525344099521668, -0.4591754850708437696 ) ) ;
#51218 = CARTESIAN_POINT ( 'NONE',  ( 4.250508905105749413, 7.277302409985156650, -0.9232175757047023090 ) ) ;
#51217 = CARTESIAN_POINT ( 'NONE',  ( 1.944624168438695566, -1.479605912621816621, -1.095697124569312564 ) ) ;
#51219 = CARTESIAN_POINT ( 'NONE',  ( 6.168596704537822717, 6.299043698156668647, 1.040834085586084257E-14 ) ) ;
#51221 = CARTESIAN_POINT ( 'NONE',  ( 0.000000000000000000, 0.000000000000000000, 11.29999999999998828 ) ) ;
#51220 = CARTESIAN_POINT ( 'NONE',  ( 1.737499999999999378, -2.916666666666668295, -3.009438278150925683 ) ) ;
#51222 = CARTESIAN_POINT ( 'NONE',  ( 1.306998621393583138, 2.023524796797530723, 1.076953482639223747 ) ) ;
#51224 = FACE_OUTER_BOUND ( 'NONE', #91690, .T. ) ;
#51223 = CARTESIAN_POINT ( 'NONE',  ( -3.855102659574803248, 8.506872032339188650, 2.500000000000000888 ) ) ;
#51225 = ORIENTED_EDGE ( 'NONE', *, *, #75347, .F. ) ;
#51226 = CARTESIAN_POINT ( 'NONE',  ( 7.199016378732056687, 10.38230762762066384, -1.082531754730537976 ) ) ;
#51227 = CARTESIAN_POINT ( 'NONE',  ( 0.8967405870976161708, -1.965081358092489516, -0.4369277762777488139 ) ) ;
#51228 = CARTESIAN_POINT ( 'NONE',  ( 0.7780835697005837881, -1.044612314895682292, -1.660310580060719188 ) ) ;
#51229 = CARTESIAN_POINT ( 'NONE',  ( 6.503150282362620160, -0.1410805869419759218, 1.984311032119711715 ) ) ;
#51231 = DIRECTION ( 'NONE',  ( -1.000000000000000000, -2.210062264950106756E-32, 1.224646799147353207E-16 ) ) ;
#51230 = CARTESIAN_POINT ( 'NONE',  ( -7.557780564614042795, 10.90482886110335414, -1.199719254218446718 ) ) ;
#51232 = CARTESIAN_POINT ( 'NONE',  ( 0.2999999999999842792, 3.372708439410100567, -0.5000000000000299760 ) ) ;
#51234 = CARTESIAN_POINT ( 'NONE',  ( 1.867668082833298993, 0.9064309091474114233, 1.519949287764200685 ) ) ;
#51233 = CARTESIAN_POINT ( 'NONE',  ( 3.486350522754261494, -0.4081323730865527577, -2.050228346494194831 ) ) ;
#51235 = CARTESIAN_POINT ( 'NONE',  ( 9.579603127937247109, -9.746166700193986898, -0.08720040834114990702 ) ) ;
#51237 = CARTESIAN_POINT ( 'NONE',  ( 4.945436657225622312, 0.7223393070586077158, -2.175551854680431330 ) ) ;
#51236 = CARTESIAN_POINT ( 'NONE',  ( -11.32735429993228138, 6.355809303862883120, 3.965345152087539127 ) ) ;
#51238 = CARTESIAN_POINT ( 'NONE',  ( 3.679424820307465538, -0.8558964687110992564, 1.515225693578539978 ) ) ;
#51239 = CARTESIAN_POINT ( 'NONE',  ( 3.728655938958122196, 4.308852335994623139, -1.199719254218446718 ) ) ;
#51240 = CARTESIAN_POINT ( 'NONE',  ( 4.441177836928239309, 7.339068688795062911, 1.199719254218452047 ) ) ;
#51241 = CARTESIAN_POINT ( 'NONE',  ( 3.497127502780640107, 1.691016411901521854, 0.3820211100199251697 ) ) ;
#51242 = CARTESIAN_POINT ( 'NONE',  ( 3.033805354627703288, 2.062495667156949430, -0.6785788507157832772 ) ) ;
#51243 = CARTESIAN_POINT ( 'NONE',  ( 4.660252114795294887, 6.460046772059735432, -1.599625672291256295 ) ) ;
#51244 = CARTESIAN_POINT ( 'NONE',  ( 4.382046175016578005, -2.016188710442788246, -0.04465648322755921829 ) ) ;
#51245 = CARTESIAN_POINT ( 'NONE',  ( 1.031250000000000888, -0.7852924748300426083, -1.895863743164066584 ) ) ;
#51246 = AXIS2_PLACEMENT_3D ( 'NONE', #163638, #14146, #196134 ) ;
#51247 = CARTESIAN_POINT ( 'NONE',  ( -1.500000000000011324, 4.660416667349484676, -0.8660254037844313801 ) ) ;
#51248 = CARTESIAN_POINT ( 'NONE',  ( 1.905176762840081528, 1.600281962709374062, 1.072135106281972616 ) ) ;
#51249 = CARTESIAN_POINT ( 'NONE',  ( -1.402160292154681736E-14, 8.343750000682796042, 1.732050807568881190 ) ) ;
#51250 = CARTESIAN_POINT ( 'NONE',  ( 5.502238596801645620, -0.9988962762179309784, 1.984187878789472892 ) ) ;
#51251 = ORIENTED_EDGE ( 'NONE', *, *, #21974, .F. ) ;
#51252 = CARTESIAN_POINT ( 'NONE',  ( -0.1108833634136767443, 0.0002062650063822807356, -1.896853557917008271 ) ) ;
#51253 = CARTESIAN_POINT ( 'NONE',  ( 1.499999999999987121, 1.295833333333353377, -0.8660254037844253849 ) ) ;
#51254 = CARTESIAN_POINT ( 'NONE',  ( 7.135668919494039031, 7.219368582364847242, 1.040834085586084257E-14 ) ) ;
#51255 = CARTESIAN_POINT ( 'NONE',  ( 4.487385655998878953, 6.258369236797239665, 1.443375672974062551 ) ) ;
#51256 = CARTESIAN_POINT ( 'NONE',  ( 0.6628206911954310776, -0.9086430318470575251, -3.411154667337676916 ) ) ;
#51257 = ADVANCED_FACE ( 'NONE', ( #170425 ), #4691, .F. ) ;
#51258 = CARTESIAN_POINT ( 'NONE',  ( 1.348599501924132804, 1.090831829848055046, -1.934932191954039427 ) ) ;
#51259 = CARTESIAN_POINT ( 'NONE',  ( 6.848121815800094936, -0.8396676627679277027, 1.771385694100804598 ) ) ;
#51260 = CARTESIAN_POINT ( 'NONE',  ( 8.107412671292031803, 11.44210330227398487, 1.082531754730557072 ) ) ;
#51261 = CARTESIAN_POINT ( 'NONE',  ( 0.3857320732078016179, 2.894052512584738501, 1.963429802559124138 ) ) ;
#51262 = CARTESIAN_POINT ( 'NONE',  ( 6.679017863784723730, -0.1010099541198590523, -2.260277599329813647 ) ) ;
#51263 = CARTESIAN_POINT ( 'NONE',  ( 5.551137550152489553, 5.441024994791534120, 0.7998128361456352531 ) ) ;
#51264 = CIRCLE ( 'NONE', #78911, 0.08000000000000014044 ) ;
#51265 = CARTESIAN_POINT ( 'NONE',  ( -0.1224325501351306023, -0.4448023855274513272, -1.973852191825019364 ) ) ;
#51266 = CARTESIAN_POINT ( 'NONE',  ( 4.334473715658632820, -1.190102281996632261, 1.684540188307581010 ) ) ;
#51267 = CARTESIAN_POINT ( 'NONE',  ( -3.716906668440817185, 7.488141546489591072, 0.7998128361456341429 ) ) ;
#51268 = CARTESIAN_POINT ( 'NONE',  ( 0.7499999999999920064, 4.264583334016150751, 1.299038105676669330 ) ) ;
#51269 = CARTESIAN_POINT ( 'NONE',  ( -1.402160292154681736E-14, -0.1781249996585796136, 1.575800808251672791 ) ) ;
#51270 = CARTESIAN_POINT ( 'NONE',  ( 6.362560269511371658, -1.322780316340057549, 1.322825847358683138 ) ) ;
#51271 = CARTESIAN_POINT ( 'NONE',  ( 4.500456895562253479, -1.699381082468238713, 0.3444616058281315119 ) ) ;
#51272 = CARTESIAN_POINT ( 'NONE',  ( 4.563825558218141509, -1.132311722701891510, 1.321849635945840706 ) ) ;
#51273 = CARTESIAN_POINT ( 'NONE',  ( 2.984766373302843778, 6.633977868828633717, -0.7998128361456291469 ) ) ;
#51274 = CARTESIAN_POINT ( 'NONE',  ( 2.015536172832455897, -2.222481616396556170, 0.5612588729206613447 ) ) ;
#51275 = CARTESIAN_POINT ( 'NONE',  ( 1.364683531249990311, 4.696875000341417916, 1.214306433183764966E-14 ) ) ;
#51276 = CARTESIAN_POINT ( 'NONE',  ( 5.987849877204276083, -2.080749957983673681, -0.2039560948884494573 ) ) ;
#51277 = CARTESIAN_POINT ( 'NONE',  ( 6.386669098100576036, 1.688287130807873293, -0.9594923298414399504 ) ) ;
#51278 = DIRECTION ( 'NONE',  ( -1.000000000000000000, 0.000000000000000000, 0.000000000000000000 ) ) ;
#51279 =( LENGTH_UNIT ( ) NAMED_UNIT ( * ) SI_UNIT ( .MILLI., .METRE. ) );
#51280 = CARTESIAN_POINT ( 'NONE',  ( 1.477185633673218534, -2.006960102380969779, -0.1948397147320118372 ) ) ;
#51281 = CARTESIAN_POINT ( 'NONE',  ( 0.5510472016944796270, -1.853416330350022179, -1.169031858332982177 ) ) ;
#51282 = CARTESIAN_POINT ( 'NONE',  ( 8.253351008435402036, 13.32471229395089907, -8.566933989776503111 ) ) ;
#51283 = CARTESIAN_POINT ( 'NONE',  ( -6.855619230004478482, 11.14997286831390788, -0.7998128361456291469 ) ) ;
#51284 = CARTESIAN_POINT ( 'NONE',  ( 5.494078562035752178, 7.432844293840273231, -1.599625672291262513 ) ) ;
#51285 = CARTESIAN_POINT ( 'NONE',  ( 3.334745777049468618, 1.343786929377327466, -1.640352557257473309 ) ) ;
#51286 = CARTESIAN_POINT ( 'NONE',  ( 0.6823417656249882723, -0.9072916663252494907, 1.181850606188755259 ) ) ;
#51287 = CARTESIAN_POINT ( 'NONE',  ( 5.391160240453525709, 1.608232483172780558, -0.8641324296934371763 ) ) ;
#51288 = ORIENTED_EDGE ( 'NONE', *, *, #186883, .T. ) ;
#51289 = CARTESIAN_POINT ( 'NONE',  ( -5.444481204339554736, 8.509589284108232121, 1.199719254218454489 ) ) ;
#51290 = DIRECTION ( 'NONE',  ( -1.276756478318932585E-15, 1.000000000000000000, -1.665334536937738262E-16 ) ) ;
#51291 = CARTESIAN_POINT ( 'NONE',  ( 7.200788982189461507, 8.533913579710086239, -1.082531754730548412 ) ) ;
#51292 = CARTESIAN_POINT ( 'NONE',  ( -3.474999999999998312, -4.127083332377416980, 2.006292185433951047 ) ) ;
#51293 = CARTESIAN_POINT ( 'NONE',  ( -6.718228810771495141, 7.796687353110217877, 1.199719254218450271 ) ) ;
#51294 = CARTESIAN_POINT ( 'NONE',  ( 2.830336888193147882, -0.9990820879247277464, -1.755331475833141308 ) ) ;
#51295 = CARTESIAN_POINT ( 'NONE',  ( 6.352570083819033542, 0.6862697483850827007, 2.097430819677794656 ) ) ;
#51296 = CARTESIAN_POINT ( 'NONE',  ( 8.516493047678546091, 13.08765898893368629, -0.7998128361456352531 ) ) ;
#51297 = CARTESIAN_POINT ( 'NONE',  ( 3.537814430808595922, 1.177328839734363308, 1.441218929277183536 ) ) ;
#51298 = CARTESIAN_POINT ( 'NONE',  ( 10.38962578677386084, 11.01565159419135043, 0.000000000000000000 ) ) ;
#51299 = FACE_OUTER_BOUND ( 'NONE', #169695, .T. ) ;
#51300 = ORIENTED_EDGE ( 'NONE', *, *, #161121, .F. ) ;
#51301 = CARTESIAN_POINT ( 'NONE',  ( -2.591579918506545344, 6.175260338232929413, 1.040834085586084257E-14 ) ) ;
#51302 = CARTESIAN_POINT ( 'NONE',  ( -7.802881099864745984, 9.062115023719057305, -1.199719254218446718 ) ) ;
#51304 = CARTESIAN_POINT ( 'NONE',  ( -4.418103850092305329, 7.323797853316306394, 1.240345400901581296 ) ) ;
#51303 = CARTESIAN_POINT ( 'NONE',  ( -6.291865805193673111, 9.498204651771386509, -1.199719254218452047 ) ) ;
#51305 = CARTESIAN_POINT ( 'NONE',  ( 1.364683531249986537, -0.3864583329919166199, 0.7879004041258500513 ) ) ;
#51306 = CARTESIAN_POINT ( 'NONE',  ( 1.897353599431324866, 0.1640088499204050976, 1.726041979094733447 ) ) ;
#51307 = CARTESIAN_POINT ( 'NONE',  ( 1.042430265417312985, -1.369658564370433540, -1.073568199598630146 ) ) ;
#51309 = CARTESIAN_POINT ( 'NONE',  ( 7.239690840017413365, 10.42976116578691403, -1.082531754730537976 ) ) ;
#51308 = CARTESIAN_POINT ( 'NONE',  ( 6.656845493208900955, -1.788705722188275837, 1.457663220358196732 ) ) ;
#51310 = CARTESIAN_POINT ( 'NONE',  ( 6.337523607829048444, 6.943994947614124058, 0.8959833429097040502 ) ) ;
#51311 = CARTESIAN_POINT ( 'NONE',  ( 0.9310180319365793933, 0.1487380178207615700, 2.055447871051790720 ) ) ;
#51312 = AXIS2_PLACEMENT_3D ( 'NONE', #33061, #114385, #130639 ) ;
#51313 = CARTESIAN_POINT ( 'NONE',  ( 6.556073970538053075, 2.004588421764907036, -1.124284452974108950 ) ) ;
#51314 = DIRECTION ( 'NONE',  ( -0.7592566023653005702, -0.6507913734559640506, 0.000000000000000000 ) ) ;
#51315 = CARTESIAN_POINT ( 'NONE',  ( -6.473091995881817162, 6.516638514809040217, 0.7998128361456281477 ) ) ;
#51316 = CARTESIAN_POINT ( 'NONE',  ( 6.807498166657679484, -0.4075194142965676836, 1.832415718333743282 ) ) ;
#51318 = CARTESIAN_POINT ( 'NONE',  ( -5.451787166470911217, 9.374519104275787384, 0.7216878364870267237 ) ) ;
#51317 = CARTESIAN_POINT ( 'NONE',  ( 4.675980034926481288, 1.890745994642643479, -0.2862527531290667837 ) ) ;
#51319 = CARTESIAN_POINT ( 'NONE',  ( 6.076841795016812320, -2.094286673724785164, -0.6961510500591641115 ) ) ;
#51320 = CARTESIAN_POINT ( 'NONE',  ( -1.502314598737159228E-15, 1.125000000682793377, 1.414508159514577423 ) ) ;
#51321 = CARTESIAN_POINT ( 'NONE',  ( -6.224601922005509991, 10.27613631906616476, 0.7216878364870267237 ) ) ;
#51322 = CARTESIAN_POINT ( 'NONE',  ( 5.695833931072550094, 5.817763472438987726, 0.000000000000000000 ) ) ;
#51323 = CARTESIAN_POINT ( 'NONE',  ( -4.299344108864961989, 6.109263775132799168, -1.443375672974066548 ) ) ;
#51324 = CARTESIAN_POINT ( 'NONE',  ( 0.4166731193052671256, -0.6827031231213858131, -1.900913249881502232 ) ) ;
#51325 = EDGE_LOOP ( 'NONE', ( #77345, #180769, #62173, #182 ) ) ;
#51326 = CARTESIAN_POINT ( 'NONE',  ( 3.909432592967517550, 1.977442543354444249, 1.189201670975383429 ) ) ;
#51328 = EDGE_CURVE ( 'NONE', #84217, #81797, #173238, .T. ) ;
#51327 = CARTESIAN_POINT ( 'NONE',  ( 5.125427350195786325, 0.1941421753944693185, -1.952251141935714696 ) ) ;
#51329 = CARTESIAN_POINT ( 'NONE',  ( 0.5144084716053355377, 0.7454083195421266073, 1.814826383214888983 ) ) ;
#51330 = CARTESIAN_POINT ( 'NONE',  ( 3.768803514918948938, 4.459654191235965293, -1.082531754730543083 ) ) ;
#51331 = LINE ( 'NONE', #400, #67768 ) ;
#51332 = ORIENTED_EDGE ( 'NONE', *, *, #70875, .T. ) ;
#51333 = CARTESIAN_POINT ( 'NONE',  ( 0.1634790396850393235, 1.973143002845114458, -0.7684359545688070892 ) ) ;
#51334 =( BOUNDED_SURFACE ( )  B_SPLINE_SURFACE ( 1, 2, ( 
 ( #162400, #98456, #95281, #112639, #127855, #13976, #129974, #94212, #32391, #178648, #64876, #145109, #65915, #195961, #197014, #179714, #193805, #48650, #16106, #211115, #15043, #31331, #97408, #161329, #163463, #45454, #49700, #132062, #12913, #198072, #160252, #144051, #1983, #115828, #33447, #69121, #68047, #135242, #50763, #83252, #35570, #149336, #99524, #119030, #52896, #150416, #51846, #167717, #181815, #21433, #916, #185012, #134184, #19320, #183959, #200193, #166656, #201256, #37718, #117965, #18246, #85396, #101650, #36639, #103796, #151482, #3052, #102723, #17177, #199120, #20385, #168780, #86469, #152533, #4118, #66983, #70187, #84330, #136299, #202322, #116893, #133121, #53971, #165583, #120108, #186087, #169846, #87541, #153610, #5181, #100582, #71257, #137370, #203387, #182892, #34509, #55040, #6258, #154673, #59296, #72329, #57172, #123334, #206608, #189298, #39862, #108123, #23585, #91832, #8406, #56107, #187158, #138435, #121189, #88618, #155743, #105971, #7328, #171993, #170913, #140597, #38787, #58237, #174150, #104868, #89692, #190352, #9483, #125455, #42014, #92896, #73405, #22508, #139508, #40938, #107043, #205535, #157891, #141666 ),
 ( #173070, #204453, #24651, #90758, #122264, #156819, #175209, #188222, #74491, #124394, #25723, #75555, #207677, #191417, #43084, #109197, #158941, #26791, #10537, #76610, #142724, #110257, #11606, #27867, #46270, #176266, #210871, #32137, #129725, #143801, #62496, #208733, #128661, #78740, #209798, #161075, #114522, #61433, #45209, #12666, #144864, #93964, #127600, #194627, #146978, #97160, #98218, #112387, #126523, #212996, #178399, #160005, #77680, #193566, #30011, #111323, #96095, #164269, #195709, #177327, #28941, #162150, #13737, #60360, #180517, #95025, #211934, #79810, #145922, #63568, #47344, #113458, #179463, #130772, #31087, #163215, #14797, #80888, #64633, #196767, #48410, #15858, #81945, #192484, #44136, #52640, #117714, #183704, #101389, #167464, #181566, #19060, #198866, #182630, #36381, #82999, #49451, #50513, #65663, #84072, #116635, #202051, #200995, #20123, #51589, #132862, #134984, #37453, #151225, #149075, #2794, #148028, #99277, #33194, #152280, #165326, #150161, #1729, #85138, #67786, #34253, #118769, #100325, #184753, #68865, #652, #131811, #16919, #214038, #66718, #166392, #17983, #133936, #199941, #115570, #102459, #197820, #168525, #86209 ) ),
 .UNSPECIFIED., .F., .F., .T. ) 
 B_SPLINE_SURFACE_WITH_KNOTS ( ( 2, 2 ),
 ( 3, 2, 2, 2, 2, 2, 2, 2, 2, 2, 2, 2, 2, 2, 2, 2, 2, 2, 2, 2, 2, 2, 2, 2, 2, 2, 2, 2, 2, 2, 2, 2, 2, 2, 2, 2, 2, 2, 2, 2, 2, 2, 2, 2, 2, 2, 2, 2, 2, 2, 2, 2, 2, 2, 2, 2, 2, 2, 2, 2, 2, 2, 2, 2, 2, 2, 2, 2, 2, 3 ),
 ( 0.000000000000000000, 1.000000000000000000 ),
 ( 0.000000000000000000, 0.01388888888888888812, 0.02777777777777777624, 0.04166666666666666435, 0.05555555555555555247, 0.06944444444444444753, 0.08333333333333332871, 0.09722222222222222376, 0.1111111111111111049, 0.1250000000000000000, 0.1388888888888888951, 0.1527777777777777901, 0.1666666666666666574, 0.1805555555555555525, 0.1944444444444444475, 0.2083333333333333426, 0.2222222222222222099, 0.2361111111111111049, 0.2500000000000000000, 0.2638888888888888951, 0.2777777777777777901, 0.2916666666666666852, 0.3055555555555555802, 0.3194444444444444198, 0.3333333333333333148, 0.3472222222222222099, 0.3611111111111111049, 0.3750000000000000000, 0.3888888888888888951, 0.4027777777777777901, 0.4166666666666666852, 0.4305555555555555802, 0.4444444444444444198, 0.4583333333333333148, 0.4722222222222222099, 0.4861111111111111049, 0.5000000000000000000, 0.5138888888888888395, 0.5277777777777777901, 0.5416666666666666297, 0.5555555555555555802, 0.5694444444444444198, 0.5833333333333333703, 0.5972222222222222099, 0.6111111111111111605, 0.6250000000000000000, 0.6388888888888888395, 0.6527777777777777901, 0.6666666666666666297, 0.6805555555555555802, 0.6944444444444444198, 0.7083333333333333703, 0.7222222222222222099, 0.7361111111111111605, 0.7500000000000000000, 0.7638888888888888395, 0.7777777777777777901, 0.7916666666666666297, 0.8055555555555555802, 0.8194444444444444198, 0.8333333333333333703, 0.8472222222222222099, 0.8611111111111111605, 0.8750000000000000000, 0.8888888888888888395, 0.9027777777777777901, 0.9166666666666666297, 0.9305555555555555802, 0.9444444444444444198, 0.9523586353390159909 ),
 .UNSPECIFIED. ) 
 GEOMETRIC_REPRESENTATION_ITEM ( )  RATIONAL_B_SPLINE_SURFACE ( (
 ( 1.000000000000000000, 0.8660254037844387076, 1.000000000000000000, 0.8660254037844387076, 1.000000000000000000, 0.8660254037844387076, 1.000000000000000000, 0.8660254037844387076, 1.000000000000000000, 0.8660254037844387076, 1.000000000000000000, 0.8660254037844387076, 1.000000000000000000, 0.8660254037844387076, 1.000000000000000000, 0.8660254037844387076, 1.000000000000000000, 0.8660254037844387076, 1.000000000000000000, 0.8660254037844387076, 1.000000000000000000, 0.8660254037844387076, 1.000000000000000000, 0.8660254037844387076, 1.000000000000000000, 0.8660254037844387076, 1.000000000000000000, 0.8660254037844387076, 1.000000000000000000, 0.8660254037844387076, 1.000000000000000000, 0.8660254037844387076, 1.000000000000000000, 0.8660254037844387076, 1.000000000000000000, 0.8660254037844387076, 1.000000000000000000, 0.8660254037844387076, 1.000000000000000000, 0.8660254037844387076, 1.000000000000000000, 0.8660254037844387076, 1.000000000000000000, 0.8660254037844387076, 1.000000000000000000, 0.8660254037844387076, 1.000000000000000000, 0.8660254037844387076, 1.000000000000000000, 0.8660254037844387076, 1.000000000000000000, 0.8660254037844387076, 1.000000000000000000, 0.8660254037844387076, 1.000000000000000000, 0.8660254037844387076, 1.000000000000000000, 0.8660254037844387076, 1.000000000000000000, 0.8660254037844387076, 1.000000000000000000, 0.8660254037844387076, 1.000000000000000000, 0.8660254037844387076, 1.000000000000000000, 0.8660254037844387076, 1.000000000000000000, 0.8660254037844387076, 1.000000000000000000, 0.8660254037844387076, 1.000000000000000000, 0.8660254037844387076, 1.000000000000000000, 0.8660254037844387076, 1.000000000000000000, 0.8660254037844387076, 1.000000000000000000, 0.8660254037844387076, 1.000000000000000000, 0.8660254037844387076, 1.000000000000000000, 0.8660254037844387076, 1.000000000000000000, 0.8660254037844387076, 1.000000000000000000, 0.8660254037844387076, 1.000000000000000000, 0.8660254037844387076, 1.000000000000000000, 0.8660254037844387076, 1.000000000000000000, 0.8660254037844387076, 1.000000000000000000, 0.8660254037844387076, 1.000000000000000000, 0.8660254037844387076, 1.000000000000000000, 0.8660254037844387076, 1.000000000000000000, 0.8660254037844387076, 1.000000000000000000, 0.8660254037844387076, 1.000000000000000000, 0.8660254037844387076, 1.000000000000000000, 0.8660254037844387076, 1.000000000000000000, 0.8660254037844387076, 1.000000000000000000, 0.8660254037844387076, 1.000000000000000000, 0.8660254037844387076, 1.000000000000000000, 0.8660254037844387076, 1.000000000000000000, 0.8660254037844387076, 1.000000000000000000, 0.8660254037844387076, 1.000000000000000000, 0.8660254037844387076, 1.000000000000000000, 0.8660254037844387076, 1.000000000000000000, 0.8660254037844387076, 1.000000000000000000, 0.8660254037844387076, 1.000000000000000000, 0.8660254037844387076, 1.000000000000000000, 0.8660254037844387076, 1.000000000000000000, 0.8660254037844387076, 1.000000000000000000, 0.8660254037844387076, 1.000000000000000000, 0.8660254037844387076, 1.000000000000000000, 0.9236583618779372618, 0.9343189745674063129),
 ( 1.000000000000000000, 0.8660254037844387076, 1.000000000000000000, 0.8660254037844387076, 1.000000000000000000, 0.8660254037844387076, 1.000000000000000000, 0.8660254037844387076, 1.000000000000000000, 0.8660254037844387076, 1.000000000000000000, 0.8660254037844387076, 1.000000000000000000, 0.8660254037844387076, 1.000000000000000000, 0.8660254037844387076, 1.000000000000000000, 0.8660254037844387076, 1.000000000000000000, 0.8660254037844387076, 1.000000000000000000, 0.8660254037844387076, 1.000000000000000000, 0.8660254037844387076, 1.000000000000000000, 0.8660254037844387076, 1.000000000000000000, 0.8660254037844387076, 1.000000000000000000, 0.8660254037844387076, 1.000000000000000000, 0.8660254037844387076, 1.000000000000000000, 0.8660254037844387076, 1.000000000000000000, 0.8660254037844387076, 1.000000000000000000, 0.8660254037844387076, 1.000000000000000000, 0.8660254037844387076, 1.000000000000000000, 0.8660254037844387076, 1.000000000000000000, 0.8660254037844387076, 1.000000000000000000, 0.8660254037844387076, 1.000000000000000000, 0.8660254037844387076, 1.000000000000000000, 0.8660254037844387076, 1.000000000000000000, 0.8660254037844387076, 1.000000000000000000, 0.8660254037844387076, 1.000000000000000000, 0.8660254037844387076, 1.000000000000000000, 0.8660254037844387076, 1.000000000000000000, 0.8660254037844387076, 1.000000000000000000, 0.8660254037844387076, 1.000000000000000000, 0.8660254037844387076, 1.000000000000000000, 0.8660254037844387076, 1.000000000000000000, 0.8660254037844387076, 1.000000000000000000, 0.8660254037844387076, 1.000000000000000000, 0.8660254037844387076, 1.000000000000000000, 0.8660254037844387076, 1.000000000000000000, 0.8660254037844387076, 1.000000000000000000, 0.8660254037844387076, 1.000000000000000000, 0.8660254037844387076, 1.000000000000000000, 0.8660254037844387076, 1.000000000000000000, 0.8660254037844387076, 1.000000000000000000, 0.8660254037844387076, 1.000000000000000000, 0.8660254037844387076, 1.000000000000000000, 0.8660254037844387076, 1.000000000000000000, 0.8660254037844387076, 1.000000000000000000, 0.8660254037844387076, 1.000000000000000000, 0.8660254037844387076, 1.000000000000000000, 0.8660254037844387076, 1.000000000000000000, 0.8660254037844387076, 1.000000000000000000, 0.8660254037844387076, 1.000000000000000000, 0.8660254037844387076, 1.000000000000000000, 0.8660254037844387076, 1.000000000000000000, 0.8660254037844387076, 1.000000000000000000, 0.8660254037844387076, 1.000000000000000000, 0.8660254037844387076, 1.000000000000000000, 0.8660254037844387076, 1.000000000000000000, 0.8660254037844387076, 1.000000000000000000, 0.8660254037844387076, 1.000000000000000000, 0.8660254037844387076, 1.000000000000000000, 0.8660254037844387076, 1.000000000000000000, 0.8660254037844387076, 1.000000000000000000, 0.8660254037844387076, 1.000000000000000000, 0.8660254037844387076, 1.000000000000000000, 0.8660254037844387076, 1.000000000000000000, 0.8660254037844387076, 1.000000000000000000, 0.8660254037844387076, 1.000000000000000000, 0.8660254037844387076, 1.000000000000000000, 0.9236583618779372618, 0.9343189745674063129) ) ) 
 REPRESENTATION_ITEM ( '' )  SURFACE ( )  );
#51336 = CARTESIAN_POINT ( 'NONE',  ( -7.700141177557535244, 11.07091624287075859, -1.199719254218446718 ) ) ;
#51335 = CARTESIAN_POINT ( 'NONE',  ( -4.436542580169821726, 6.199052314996659874, 1.599625672291267398 ) ) ;
#51337 = DIRECTION ( 'NONE',  ( 0.7592566023653005702, 0.6507913734559639396, 0.000000000000000000 ) ) ;
#51338 = CARTESIAN_POINT ( 'NONE',  ( 3.977515510703835133, -0.1653560672004051324, 2.164858251032927061 ) ) ;
#51339 = CARTESIAN_POINT ( 'NONE',  ( 9.769029508667873785, 11.88457606340896255, -6.891197000744894829 ) ) ;
#51340 = CARTESIAN_POINT ( 'NONE',  ( 1.406653384705614629, -2.110883996484512970, -0.2024971186788473154 ) ) ;
#51341 = CARTESIAN_POINT ( 'NONE',  ( 1.499999999999989120, 2.806250000682818158, 1.214306433183764966E-14 ) ) ;
#51342 = CARTESIAN_POINT ( 'NONE',  ( 10.24048609702354717, 10.84165528948263457, -0.7998128361456281477 ) ) ;
#51343 = CARTESIAN_POINT ( 'NONE',  ( 11.94980361490495469, 13.50332124735856709, -1.099999952232860290 ) ) ;
#51344 = CARTESIAN_POINT ( 'NONE',  ( 6.252685474373055996, 7.003816019006632310, -0.9791501464874209359 ) ) ;
#51345 =( GEOMETRIC_REPRESENTATION_CONTEXT ( 3 ) GLOBAL_UNCERTAINTY_ASSIGNED_CONTEXT ( ( #62453 ) ) GLOBAL_UNIT_ASSIGNED_CONTEXT ( ( #7370, #141709, #10579 ) ) REPRESENTATION_CONTEXT ( 'NONE', 'WORKASPACE' ) );
#51346 = ORIENTED_EDGE ( 'NONE', *, *, #144311, .F. ) ;
#51347 = CARTESIAN_POINT ( 'NONE',  ( 2.565760370094140264, 2.021647365152558606, -0.3987750144259157858 ) ) ;
#51349 = DIRECTION ( 'NONE',  ( 0.000000000000000000, 0.000000000000000000, -1.000000000000000000 ) ) ;
#51348 = CARTESIAN_POINT ( 'NONE',  ( -7.804689982961090955, 12.25722208009664094, 0.7998128361456481317 ) ) ;
#51350 = CARTESIAN_POINT ( 'NONE',  ( 1.364683531249988535, 2.113541667008087099, 0.7879004041258500513 ) ) ;
#51351 = CARTESIAN_POINT ( 'NONE',  ( 0.07775346131143417994, 7.629137130509094256, -2.888902737517151209 ) ) ;
#51352 = EDGE_CURVE ( 'NONE', #131565, #36225, #124971, .T. ) ;
#51353 = CARTESIAN_POINT ( 'NONE',  ( -5.736990052169587351, 5.898621588803449001, 2.499999999999785061 ) ) ;
#51354 = ORIENTED_EDGE ( 'NONE', *, *, #85850, .F. ) ;
#51355 = CARTESIAN_POINT ( 'NONE',  ( 4.916621234345090130, -0.6478637630910142331, -1.799314785492410529 ) ) ;
#51356 = CARTESIAN_POINT ( 'NONE',  ( -11.91826849282518452, 10.89999999999997904, 1.399999999999998579 ) ) ;
#51357 = CARTESIAN_POINT ( 'NONE',  ( 1.388340239569575640, -1.017395381511316810, 2.020837998375684563 ) ) ;
#51358 = CARTESIAN_POINT ( 'NONE',  ( -3.952365473583647315, 4.569846793057691592, 1.199719254218462483 ) ) ;
#51359 = CARTESIAN_POINT ( 'NONE',  ( 1.775370306292364031, 0.3070917902865456517, -1.785173024263370101 ) ) ;
#51360 = CARTESIAN_POINT ( 'NONE',  ( 1.340887447446635017, -1.644988140609974225, -0.9815275998622545739 ) ) ;
#51361 = CIRCLE ( 'NONE', #9909, 2.000000000000000000 ) ;
#51362 = CARTESIAN_POINT ( 'NONE',  ( 1.715371797147913435, -1.774658612622433296, -1.066089629202723765 ) ) ;
#51363 = CARTESIAN_POINT ( 'NONE',  ( 0.6823417656249899377, 1.155208333674752286, 1.181850606188755259 ) ) ;
#51364 = CARTESIAN_POINT ( 'NONE',  ( 0.3562423511419475775, 0.7522458758148011793, 1.822497947957350428 ) ) ;
#51365 = CARTESIAN_POINT ( 'NONE',  ( 6.024042007596412063, -1.072333998858214343, -1.600281699052849893 ) ) ;
#51367 = CARTESIAN_POINT ( 'NONE',  ( 6.357275476766607980, 6.835366726881293431, -0.6123070361637416026 ) ) ;
#51366 = CARTESIAN_POINT ( 'NONE',  ( 6.481111342790009999, -0.1036386110354891726, -2.204582208980155222 ) ) ;
#51368 = CARTESIAN_POINT ( 'NONE',  ( -1.364683531250012516, 2.030208333674750953, 0.7879004041258379498 ) ) ;
#51369 = CARTESIAN_POINT ( 'NONE',  ( 4.756332342268011715, -2.062141065897259207, -0.05393103437261077132 ) ) ;
#51370 = CARTESIAN_POINT ( 'NONE',  ( -5.768104287610143821, 8.816873204598778102, -1.199719254218440723 ) ) ;
#51371 = CARTESIAN_POINT ( 'NONE',  ( 6.913768267964901071, 10.15348118167935709, -1.199719254218441611 ) ) ;
#51372 = CARTESIAN_POINT ( 'NONE',  ( 3.167801447087334132, 6.847518788243869281, -0.7998128361456291469 ) ) ;
#51373 = CARTESIAN_POINT ( 'NONE',  ( 6.006425746053997372, 6.966250444273174303, -1.199719254218445830 ) ) ;
#51375 = CARTESIAN_POINT ( 'NONE',  ( -1.500000000000013101, 3.379166666666691299, -0.8660254037844313801 ) ) ;
#51374 = CARTESIAN_POINT ( 'NONE',  ( 4.788165231579453618, -0.9949995658048852443, 1.856088619770781989 ) ) ;
#51376 = CARTESIAN_POINT ( 'NONE',  ( 0.6257148180217129152, 0.2125798311119214690, -2.160765367999056608 ) ) ;
#51377 = CARTESIAN_POINT ( 'NONE',  ( 1.364683531249988535, 2.676041667008082214, 0.7879004041258500513 ) ) ;
#51378 = CARTESIAN_POINT ( 'NONE',  ( 4.938837616837212785, 0.3641351946921667082, 2.130543054529559832 ) ) ;
#51380 = ADVANCED_FACE ( 'NONE', ( #157403 ), #25242, .T. ) ;
#51379 = CARTESIAN_POINT ( 'NONE',  ( 5.953772690328709594, -1.464304757327790973, -1.391265315224277099 ) ) ;
#51381 = CARTESIAN_POINT ( 'NONE',  ( -1.364683531250000748, -1.240624999658580752, 0.000000000000000000 ) ) ;
#51382 = EDGE_CURVE ( 'NONE', #187611, #177822, #43659, .T. ) ;
#51385 = CARTESIAN_POINT ( 'NONE',  ( 4.338245966692901412, 8.005111361209628740, -0.7216878364870197293 ) ) ;
#51384 = CARTESIAN_POINT ( 'NONE',  ( 1.642778471875001811, -2.092708332855373943, 2.845375778867859751 ) ) ;
#51383 = CARTESIAN_POINT ( 'NONE',  ( 7.014364370223726830, 9.276787413384745662, -1.599625672291269396 ) ) ;
#51386 = CARTESIAN_POINT ( 'NONE',  ( -5.387385936583832802, 7.378645907471495846, -1.599625672291271394 ) ) ;
#51387 = CARTESIAN_POINT ( 'NONE',  ( 3.661342437515973547, 1.897110692972364454, -0.6839366698164971448 ) ) ;
#51388 = CARTESIAN_POINT ( 'NONE',  ( -7.991641480251377772, 11.41099992934688956, 1.199719254218453823 ) ) ;
#51390 = CARTESIAN_POINT ( 'NONE',  ( -0.5773502691896261751, -2.500000000000002220, -0.9999999999999991118 ) ) ;
#51389 = CARTESIAN_POINT ( 'NONE',  ( -2.279742385392243165, 5.811449882932888222, -0.7998128361456281477 ) ) ;
#51392 = CARTESIAN_POINT ( 'NONE',  ( -11.97929049433705551, 12.30000000000000071, -0.7046979865771820783 ) ) ;
#51391 = CARTESIAN_POINT ( 'NONE',  ( 5.190363053866647647, -2.144918610114197488, -0.2683968819863768451 ) ) ;
#51393 = SURFACE_SIDE_STYLE ('',( #98030 ) ) ;
#51394 = CARTESIAN_POINT ( 'NONE',  ( 3.469446951953614189E-15, 3.300000000000018030, 1.214306433183764966E-14 ) ) ;
#51396 = CARTESIAN_POINT ( 'NONE',  ( 5.554314605481814660, -1.277030258849481736, 1.560512323070535112 ) ) ;
#51395 = CARTESIAN_POINT ( 'NONE',  ( -7.985389288324703294, 9.379004260209384825, -1.082531754730543083 ) ) ;
#51397 = CARTESIAN_POINT ( 'NONE',  ( -1.500000000000011324, 5.379166666666692187, -0.8660254037844313801 ) ) ;
#51398 = CARTESIAN_POINT ( 'NONE',  ( 1.084105852307458040, -1.681943224540465964, -0.3816912691657590728 ) ) ;
#51399 = CARTESIAN_POINT ( 'NONE',  ( 5.408776937209000657, 5.274937613024121674, 0.7998128361456352531 ) ) ;
#51401 = CARTESIAN_POINT ( 'NONE',  ( 6.424584688029230328, 8.588711117491191871, 1.599625672291268286 ) ) ;
#51400 = CARTESIAN_POINT ( 'NONE',  ( 6.643132081016105417, 10.69414516125339887, 0.7216878364870438212 ) ) ;
#51402 = DIRECTION ( 'NONE',  ( 0.000000000000000000, -1.000000000000000000, 0.000000000000000000 ) ) ;
#51403 = CARTESIAN_POINT ( 'NONE',  ( 5.712129104542990277, -0.8404194184173617854, -1.671158263034502767 ) ) ;
#51404 = CARTESIAN_POINT ( 'NONE',  ( 5.959245303985257536, -1.698412939339728700, 1.080668751846917797 ) ) ;
#51405 = CARTESIAN_POINT ( 'NONE',  ( -4.252937622776048698, 3.981816863952433838, 0.4689809815191707809 ) ) ;
#51406 = VECTOR ( 'NONE', #161231, 1000.000000000000000 ) ;
#51407 = CARTESIAN_POINT ( 'NONE',  ( -7.417719440008134768, 7.826629899530511025, 0.7216878364870317197 ) ) ;
#51408 = ORIENTED_EDGE ( 'NONE', *, *, #60871, .F. ) ;
#51410 = CARTESIAN_POINT ( 'NONE',  ( 1.792592436991577109, 1.492242793082170227, -1.356315429364700176 ) ) ;
#51409 = CARTESIAN_POINT ( 'NONE',  ( 2.455864667332839257, -1.573010975769023601, -1.422207447652395373 ) ) ;
#51411 = CARTESIAN_POINT ( 'NONE',  ( 1.300706311995255771, -0.2675212335121620599, -1.791602419159578519 ) ) ;
#51412 = CARTESIAN_POINT ( 'NONE',  ( 6.068156270568149324, 9.237210194708310951, 1.199719254218452047 ) ) ;
#51413 = CARTESIAN_POINT ( 'NONE',  ( 5.893488898593548520, 1.633865717575968546, 1.415524914074948404 ) ) ;
#51414 = CARTESIAN_POINT ( 'NONE',  ( 6.425674737872927089, 9.584038729905381970, -1.199719254218440723 ) ) ;
#51416 = CARTESIAN_POINT ( 'NONE',  ( 0.5849901852424718163, 1.567898511244028459, 1.100480585720535087 ) ) ;
#51415 = CARTESIAN_POINT ( 'NONE',  ( -6.403528624356093601, 6.365204904703887223, 1.040834085586084257E-14 ) ) ;
#51417 = VECTOR ( 'NONE', #203218, 1000.000000000000000 ) ;
#51418 = FACE_OUTER_BOUND ( 'NONE', #149181, .T. ) ;
#51419 = DIRECTION ( 'NONE',  ( -4.163336342344327166E-17, -0.5005768354468325132, 0.8656921114426507913 ) ) ;
#51420 = CARTESIAN_POINT ( 'NONE',  ( 4.812781342726855982, 7.598366752281232372, 1.082531754730558626 ) ) ;
#51421 = CARTESIAN_POINT ( 'NONE',  ( 5.536872897005128635, 5.953237723320745189, 0.6961998893310636927 ) ) ;
#51422 = CARTESIAN_POINT ( 'NONE',  ( 4.378920427533921078, 4.211088041652093494, 1.214306433183764966E-14 ) ) ;
#51423 = CARTESIAN_POINT ( 'NONE',  ( -2.300079615812729905, 5.835176651756807331, -0.7998128361456281477 ) ) ;
#51424 = CARTESIAN_POINT ( 'NONE',  ( 4.768767694835816862, -0.2516295123269947642, -2.000731945836851544 ) ) ;
#51425 = CARTESIAN_POINT ( 'NONE',  ( 4.645497774645743760, -1.668943667408796294, -1.373881373981879817 ) ) ;
#51426 = CARTESIAN_POINT ( 'NONE',  ( -7.282137904315833410, 7.668451441222825515, 0.000000000000000000 ) ) ;
#51427 = CARTESIAN_POINT ( 'NONE',  ( 5.072158865288233898, 7.971250205261355859, 1.082531754730549078 ) ) ;
#51428 = CARTESIAN_POINT ( 'NONE',  ( 1.723052270212792836, 1.567896913533245229, -1.427966198690698851 ) ) ;
#51429 = DIRECTION ( 'NONE',  ( 0.000000000000000000, -1.000000000000000000, 0.000000000000000000 ) ) ;
#51430 = CARTESIAN_POINT ( 'NONE',  ( 3.796128654474308028, -1.968949637145664955, -0.1001596523246932047 ) ) ;
#51431 = CARTESIAN_POINT ( 'NONE',  ( 4.412309042748480792, -1.912102599942141268, -0.04143165621695726192 ) ) ;
#51432 = ORIENTED_EDGE ( 'NONE', *, *, #165043, .T. ) ;
#51433 = CARTESIAN_POINT ( 'NONE',  ( 9.483257663144033955, -6.709848117146358426, -0.3912817730722052412 ) ) ;
#51434 = CARTESIAN_POINT ( 'NONE',  ( 5.846149472147661896, -0.8869723270901458401, 1.758618239599341937 ) ) ;
#51435 = CARTESIAN_POINT ( 'NONE',  ( 1.464679669172624488, 0.1433081720705318696, -1.936712990118959032 ) ) ;
#51436 = EDGE_LOOP ( 'NONE', ( #209795, #114593, #13668, #172813 ) ) ;
#51437 = CARTESIAN_POINT ( 'NONE',  ( -4.930325137224961907, 5.781076077297750970, -1.199719254218453823 ) ) ;
#51439 = CARTESIAN_POINT ( 'NONE',  ( 1.879624969287899683, 2.480000000000013305, -2.465175922436416922 ) ) ;
#51438 = CARTESIAN_POINT ( 'NONE',  ( -6.997416678428844072, 8.296645891989347987, 1.082531754730549078 ) ) ;
#51440 = CARTESIAN_POINT ( 'NONE',  ( 5.635385404774530649, 9.726366738878972740, 0.7998128361456462443 ) ) ;
#51442 = CARTESIAN_POINT ( 'NONE',  ( 6.183927461164522299, 6.387205924212962849, 0.000000000000000000 ) ) ;
#51441 = CARTESIAN_POINT ( 'NONE',  ( 7.983053520348166288, 8.207983950027992748, -0.7998128361456281477 ) ) ;
#51444 = ORIENTED_EDGE ( 'NONE', *, *, #134419, .F. ) ;
#51443 = CARTESIAN_POINT ( 'NONE',  ( 6.340485057729076779, 1.096952271789692901, -1.566184530335120950 ) ) ;
#51445 = CARTESIAN_POINT ( 'NONE',  ( 3.246891520140795517, 0.5363302883765566076, 2.140594385818309409 ) ) ;
#51446 = CARTESIAN_POINT ( 'NONE',  ( 2.257103711190447282, -1.706036888594957723, 1.399758388914617013 ) ) ;
#51447 = LINE ( 'NONE', #101245, #58267 ) ;
#51448 = CARTESIAN_POINT ( 'NONE',  ( 0.9438406676962156627, -1.213610516764839664, -1.477797202995428938 ) ) ;
#51449 = CARTESIAN_POINT ( 'NONE',  ( -2.429488990373097845, 5.239623814575174343, 0.8733349908450799282 ) ) ;
#51450 = CARTESIAN_POINT ( 'NONE',  ( -6.576431128232853141, -6.604036961759847557, -7.015831072854298078 ) ) ;
#51451 = CARTESIAN_POINT ( 'NONE',  ( 2.893098739488662030, 0.2508700648995808025, 2.055025655848155886 ) ) ;
#51452 = CARTESIAN_POINT ( 'NONE',  ( -5.494078562035765501, 7.432844293840273231, -1.599625672291256295 ) ) ;
#51453 = CARTESIAN_POINT ( 'NONE',  ( -6.147489916148834332, 6.992309281770507923, 0.9361876800342925353 ) ) ;
#51455 = CARTESIAN_POINT ( 'NONE',  ( 1.815512348505427642, -0.2646426633909418347, 2.145385951886819242 ) ) ;
#51454 = CARTESIAN_POINT ( 'NONE',  ( -2.754277761870538299, 6.365074488824250309, 1.040834085586084257E-14 ) ) ;
#51456 = CARTESIAN_POINT ( 'NONE',  ( 4.089532599075940134, -0.8378280566024614018, 2.025282237563410526 ) ) ;
#51457 = CARTESIAN_POINT ( 'NONE',  ( -0.04117949675282415317, 3.478559061295773525, -1.999678960129391836 ) ) ;
#51458 = CARTESIAN_POINT ( 'NONE',  ( 3.282482588284323821, 6.843663763058119187, 0.7216878364870257245 ) ) ;
#51459 = CARTESIAN_POINT ( 'NONE',  ( -0.3282377607281345422, 1.113835450998177157, 1.224999999999983880 ) ) ;
#51460 = CARTESIAN_POINT ( 'NONE',  ( 1.364683531249997417, 14.54687500034139447, 2.602085213965210642E-15 ) ) ;
#51461 = CARTESIAN_POINT ( 'NONE',  ( -5.655686355556086120, 6.627330832017406692, 1.199719254218452935 ) ) ;
#51462 = CARTESIAN_POINT ( 'NONE',  ( 5.555191991570319843, -1.093772777934084894, 1.345723482730563525 ) ) ;
#51463 = CARTESIAN_POINT ( 'NONE',  ( -3.789667630219657912, 4.380032642466370696, 1.199719254218462483 ) ) ;
#51464 = CARTESIAN_POINT ( 'NONE',  ( 3.942288228968212849, -1.024710522258945655, 1.798826465557185506 ) ) ;
#51465 = CARTESIAN_POINT ( 'NONE',  ( 4.306348207420813701, 1.301105652591315387, -1.670210365991892987 ) ) ;
#51466 = CARTESIAN_POINT ( 'NONE',  ( 4.950698647284403009, 8.927565521807144577, 1.040834085586084257E-14 ) ) ;
#51467 = CARTESIAN_POINT ( 'NONE',  ( 1.364683531249990311, 4.384375000341417028, 1.214306433183764966E-14 ) ) ;
#51468 = CARTESIAN_POINT ( 'NONE',  ( 2.658990959838656742, 1.584636853462956685, -1.169278883008363135 ) ) ;
#51469 = CARTESIAN_POINT ( 'NONE',  ( 1.248149539447914735, 0.9399939672071171426, -1.665319807275446706 ) ) ;
#51470 = CARTESIAN_POINT ( 'NONE',  ( 4.312625044126452423, 2.094834666918590216, 0.9310453638207391025 ) ) ;
#51471 = CARTESIAN_POINT ( 'NONE',  ( 3.070728972534173096, -1.687097908962056803, -0.6982200720766564839 ) ) ;
#51472 = CARTESIAN_POINT ( 'NONE',  ( 3.932747076415766596, 6.745899468197171345, 1.199719254218451159 ) ) ;
#51473 = CARTESIAN_POINT ( 'NONE',  ( 4.650083499362864359, 7.408552601689905259, 1.082531754730558626 ) ) ;
#51474 = CARTESIAN_POINT ( 'NONE',  ( -5.856232286098998152, 8.919689202835742847, 1.199719254218452047 ) ) ;
#51475 = EDGE_CURVE ( 'NONE', #105749, #55379, #159924, .T. ) ;
#51476 = EDGE_LOOP ( 'NONE', ( #32767, #87042, #62091, #44278 ) ) ;
#51477 = VERTEX_POINT ( 'NONE', #177912 ) ;
#51478 = CARTESIAN_POINT ( 'NONE',  ( 3.498294685330126441, -0.9886941555459362041, 1.753605845479579095 ) ) ;
#51479 = CARTESIAN_POINT ( 'NONE',  ( 4.047668389856577065, 1.417901948909123799, 1.355967163993692992 ) ) ;
#51480 = CARTESIAN_POINT ( 'NONE',  ( -7.640183256500752584, 8.872300873127729304, -1.199719254218446718 ) ) ;
#51481 = CARTESIAN_POINT ( 'NONE',  ( -4.388035272317281077, 8.271124917678806199, 0.7998128361456481317 ) ) ;
#51482 = CARTESIAN_POINT ( 'NONE',  ( 0.1751657365761521701, 0.7240325161481726557, -2.128694924679303213 ) ) ;
#51484 = CARTESIAN_POINT ( 'NONE',  ( 5.190226478415982392, -1.756784752911320302, -0.2140884780794347908 ) ) ;
#51483 = CARTESIAN_POINT ( 'NONE',  ( 0.6266517258138035729, 0.1575598857218879489, 2.084883927750030175 ) ) ;
#51485 = CARTESIAN_POINT ( 'NONE',  ( 3.231779075379113131, 6.036511184309971689, 0.9899555337401855226 ) ) ;
#51486 = CARTESIAN_POINT ( 'NONE',  ( 2.256057974219495499, 0.9384471748680022207, 1.980482673072603284 ) ) ;
#51487 = CARTESIAN_POINT ( 'NONE',  ( 0.2920125592734872932, 1.448600077496174476, -0.9643754397266665057 ) ) ;
#51488 = VECTOR ( 'NONE', #168508, 1000.000000000000000 ) ;
#51489 = CARTESIAN_POINT ( 'NONE',  ( 5.926885707468349196, 10.06645042535509660, 1.040834085586084257E-14 ) ) ;
#51490 = CARTESIAN_POINT ( 'NONE',  ( 0.2335667940003021970, 4.085521407782252368, -2.708192491817535075 ) ) ;
#51491 = CARTESIAN_POINT ( 'NONE',  ( 0.1875851866701295223, -0.8181552731707610882, 1.518483014795414032 ) ) ;
#51492 = CARTESIAN_POINT ( 'NONE',  ( 0.6795420635867071013, 1.475991390215245058, 1.620154534501851096 ) ) ;
#51493 = CARTESIAN_POINT ( 'NONE',  ( 2.877765823869771644, 2.095344539500657799, -0.6929138170133213315 ) ) ;
#51494 = CARTESIAN_POINT ( 'NONE',  ( 6.795391773274086944, -1.942485666075419060, 0.9701230550103381312 ) ) ;
#51495 = FACE_OUTER_BOUND ( 'NONE', #176818, .T. ) ;
#51496 = CARTESIAN_POINT ( 'NONE',  ( 2.325544253341553347, -1.572509993196508971, -1.418087145738779808 ) ) ;
#51497 = CARTESIAN_POINT ( 'NONE',  ( 0.000000000000000000, -9.746166700180788567, 9.579665964948883783 ) ) ;
#51498 = CARTESIAN_POINT ( 'NONE',  ( 5.209954918934378121, -1.917094737882633959, 0.1888984193934347133 ) ) ;
#51499 = VERTEX_POINT ( 'NONE', #44724 ) ;
#51500 = CIRCLE ( 'NONE', #6485, 9.616019636405015447 ) ;
#51502 = CARTESIAN_POINT ( 'NONE',  ( -1.499999999999997780, 5.900000000000023448, 1.214306433183764966E-14 ) ) ;
#51501 = CARTESIAN_POINT ( 'NONE',  ( 1.998001414424467104, -2.291734237260790952, 0.06083037064899367297 ) ) ;
#51503 = CARTESIAN_POINT ( 'NONE',  ( 2.822068529938852155, 6.444163718237301275, -0.7998128361456291469 ) ) ;
#51504 = CARTESIAN_POINT ( 'NONE',  ( 6.342516933094585418, 6.294024598232139667, 1.040834085586084257E-14 ) ) ;
#51505 = EDGE_CURVE ( 'NONE', #170318, #105457, #59882, .T. ) ;
#51506 = CARTESIAN_POINT ( 'NONE',  ( 4.336746411289113645, 1.366526421497065824, -1.751164563135388041 ) ) ;
#51507 = CARTESIAN_POINT ( 'NONE',  ( -7.375272376154093479, 9.627570410311676596, -1.443375672974059665 ) ) ;
#51508 = CARTESIAN_POINT ( 'NONE',  ( -5.738313685646318163, 5.917571446856342732, -2.440166996132832722 ) ) ;
#51509 = CARTESIAN_POINT ( 'NONE',  ( 5.341549334104188418, 7.254893527920112994, 1.443375672974062551 ) ) ;
#51510 = CARTESIAN_POINT ( 'NONE',  ( -8.202319746143382773, 9.632089794331152532, 1.082531754730558626 ) ) ;
#51511 = CARTESIAN_POINT ( 'NONE',  ( 5.072158865288233898, 7.971250205261355859, 1.082531754730549078 ) ) ;
#51512 = ORIENTED_EDGE ( 'NONE', *, *, #55286, .F. ) ;
#51513 = CARTESIAN_POINT ( 'NONE',  ( 2.918592439375994552, -1.356299846568160827, -1.492255409411530120 ) ) ;
#51515 = CARTESIAN_POINT ( 'NONE',  ( 0.5146022356567416800, 0.7859572577839054608, 1.907140732884365697 ) ) ;
#51514 = CARTESIAN_POINT ( 'NONE',  ( 6.693975156845185737, 8.832723654451292816, 1.599625672291281386 ) ) ;
#51516 = CARTESIAN_POINT ( 'NONE',  ( -11.87828357749937780, 13.80310252740409283, 1.708055325888793163 ) ) ;
#51517 = CARTESIAN_POINT ( 'NONE',  ( 4.692530563661249765, 8.488719734331187539, 0.000000000000000000 ) ) ;
#51518 =( NAMED_UNIT ( * ) SI_UNIT ( $, .STERADIAN. ) SOLID_ANGLE_UNIT ( ) );
#51519 = CARTESIAN_POINT ( 'NONE',  ( 1.364683531249988535, 3.613541667008086211, 0.7879004041258500513 ) ) ;
#51520 = CARTESIAN_POINT ( 'NONE',  ( 4.277398745584213735, 1.430588233724191083, 1.660156109410643177 ) ) ;
#51521 = CARTESIAN_POINT ( 'NONE',  ( 1.863907939170056149, -0.1017519224979606118, -2.013985838549677609 ) ) ;
#51522 = CARTESIAN_POINT ( 'NONE',  ( 1.206327419354651820, 1.623952629372883427, 0.8676893986077349741 ) ) ;
#51523 = CARTESIAN_POINT ( 'NONE',  ( 4.775077868145559457, 2.139425163340304525, -0.8237163094031977328 ) ) ;
#51524 = CARTESIAN_POINT ( 'NONE',  ( 3.591602706507342369, -1.839109287420921834, -0.08896477992388628075 ) ) ;
#51525 = CARTESIAN_POINT ( 'NONE',  ( 7.587759525142423911, 12.00413654597487501, 0.7998128361456462443 ) ) ;
#51527 = ADVANCED_FACE ( 'NONE', ( #111912 ), #28502, .T. ) ;
#51526 = CARTESIAN_POINT ( 'NONE',  ( 2.375000000000001776, 2.052068128417950277, -1.362642298365709419E-13 ) ) ;
#51528 = CARTESIAN_POINT ( 'NONE',  ( 4.172732250082421324, -1.703408510751417193, -0.6570589383413026896 ) ) ;
#51529 = CARTESIAN_POINT ( 'NONE',  ( 5.432267593368638181, -1.591316862017605471, -1.238322901282742805 ) ) ;
#51530 = CARTESIAN_POINT ( 'NONE',  ( -8.341290820905609138, 10.75459192918846618, 1.599625672291269396 ) ) ;
#51532 = DIRECTION ( 'NONE',  ( 0.000000000000000000, 1.000000000000000000, 0.000000000000000000 ) ) ;
#51531 = CARTESIAN_POINT ( 'NONE',  ( 5.067353023127458833, 0.2270735253321141400, -2.251102950005756220 ) ) ;
#51533 = CARTESIAN_POINT ( 'NONE',  ( 0.1179828827667589730, -2.064941173381201978, 0.4132506003948192563 ) ) ;
#51534 = FACE_OUTER_BOUND ( 'NONE', #29839, .T. ) ;
#51535 = CARTESIAN_POINT ( 'NONE',  ( 3.279797552538410876, -1.996039814156633785, 0.5495672325947635883 ) ) ;
#51536 = CARTESIAN_POINT ( 'NONE',  ( 3.541704441667858472, 5.155074486744371853, -1.599625672291262513 ) ) ;
#51537 = CARTESIAN_POINT ( 'NONE',  ( -1.360316468750007779, 2.171875000341411344, -4.336808689942017736E-14 ) ) ;
#51538 = SHAPE_DEFINITION_REPRESENTATION ( #124996, #63688 ) ;
#51540 = CARTESIAN_POINT ( 'NONE',  ( 1.857912668630396169, 1.921361403365331677, -0.1415498456752254663 ) ) ;
#51539 = CARTESIAN_POINT ( 'NONE',  ( -7.771848369131641121, 10.09024240211882351, -1.599625672291263179 ) ) ;
#51541 = UNCERTAINTY_MEASURE_WITH_UNIT (LENGTH_MEASURE( 1.000000000000000082E-05 ), #144711, 'distance_accuracy_value', 'NONE');
#51542 = CARTESIAN_POINT ( 'NONE',  ( -4.085803189671902480, 5.860132702740892263, -1.599625672291271394 ) ) ;
#51543 = CARTESIAN_POINT ( 'NONE',  ( 0.1683113222354900018, -0.8393015767643360325, -1.780324559216818425 ) ) ;
#51544 = CARTESIAN_POINT ( 'NONE',  ( 5.519577934094864524, 5.612131475965050242, 0.7216878364870328300 ) ) ;
#51545 = CARTESIAN_POINT ( 'NONE',  ( 5.881923755780003482, 5.983360633994940336, 0.1790317558759656202 ) ) ;
#51546 = CARTESIAN_POINT ( 'NONE',  ( -10.03267048443264109, 11.76749898900197877, 1.082531754730558626 ) ) ;
#51548 = CARTESIAN_POINT ( 'NONE',  ( 1.863841412593499003, -1.787636906239049805, -1.318573911375673369 ) ) ;
#51547 = CARTESIAN_POINT ( 'NONE',  ( 0.6156802735862785259, 1.737094954450137285, 1.216079458918501333 ) ) ;
#51549 = CARTESIAN_POINT ( 'NONE',  ( 3.012826026228847098, 1.526343371991075948, -1.451234828553144673 ) ) ;
#51550 = CARTESIAN_POINT ( 'NONE',  ( -7.910256278930404505, 8.193330178365746619, -0.7998128361456362523 ) ) ;
#51551 = CARTESIAN_POINT ( 'NONE',  ( 6.856673000209174695, 9.022537805042615489, 1.599625672291281386 ) ) ;
#51552 = CARTESIAN_POINT ( 'NONE',  ( 0.6427239283240515633, -0.2220358882154548907, -1.847681390136299839 ) ) ;
#51553 = CARTESIAN_POINT ( 'NONE',  ( 5.503720292143644777, 8.508425209887878538, 1.199719254218462483 ) ) ;
#51554 = CARTESIAN_POINT ( 'NONE',  ( -4.275059339850010076, 7.289437269727999436, -0.9335736327708322735 ) ) ;
#51555 = CARTESIAN_POINT ( 'NONE',  ( 5.983225862332436584, 5.874851682342960402, 0.7998128361456341429 ) ) ;
#51556 = CARTESIAN_POINT ( 'NONE',  ( -4.963693636378939011, 8.805076652501815815, 0.7216878364870267237 ) ) ;
#51557 = CARTESIAN_POINT ( 'NONE',  ( -7.158341918335454857, 10.33485409049125003, 1.082531754730549967 ) ) ;
#51559 = CARTESIAN_POINT ( 'NONE',  ( 1.002369745560643510, -0.9483682245385971488, 1.896766750748935415 ) ) ;
#51558 = AXIS2_PLACEMENT_3D ( 'NONE', #171897, #58147, #75464 ) ;
#51560 = CARTESIAN_POINT ( 'NONE',  ( -6.611536185319534908, 7.742488966741438716, 1.199719254218452047 ) ) ;
#51562 = CARTESIAN_POINT ( 'NONE',  ( 4.721123852359588646, -1.751549048416237486, -0.8839179009662299080 ) ) ;
#51561 = CARTESIAN_POINT ( 'NONE',  ( -1.225000000000038058, 0.4791666666666983265, -0.7072540797573158011 ) ) ;
#51563 = CARTESIAN_POINT ( 'NONE',  ( 3.784175263432405956, -1.067420458145739826, 1.879713924940962677 ) ) ;
#51564 = CARTESIAN_POINT ( 'NONE',  ( 2.155570461979210428, 0.7887370375637430264, 1.663910549085621415 ) ) ;
#51565 = CARTESIAN_POINT ( 'NONE',  ( -4.099542569701578820, 7.506983624740954930, -0.5818660602148464367 ) ) ;
#51566 = CARTESIAN_POINT ( 'NONE',  ( 4.184706906298553797, 7.590773377710720915, -0.8858016571234141878 ) ) ;
#51567 = CARTESIAN_POINT ( 'NONE',  ( 4.189205958701418986, -0.6631863921694808317, 1.609220651327713414 ) ) ;
#51568 = CARTESIAN_POINT ( 'NONE',  ( -1.724555757182347993, 14.99999999999692157, -11.68000002332616205 ) ) ;
#51569 = CARTESIAN_POINT ( 'NONE',  ( 5.829642864196168617, 6.863966765392747860, 1.082531754730558626 ) ) ;
#51570 = CARTESIAN_POINT ( 'NONE',  ( -10.52284959769361805, 5.420271152154175986, 5.071911021504272199 ) ) ;
#51571 = CARTESIAN_POINT ( 'NONE',  ( 2.413140945657660907, 1.930630709398067246, 0.9725960170764782475 ) ) ;
#51572 = CARTESIAN_POINT ( 'NONE',  ( 3.075545897833771747, 1.462222457232667416, -1.388272539953112839 ) ) ;
#51573 = CARTESIAN_POINT ( 'NONE',  ( -8.636180661780651135, 13.01936850547871138, -0.7216878364870257245 ) ) ;
#51574 = CIRCLE ( 'NONE', #172641, 0.4800000000000000933 ) ;
#51575 = CARTESIAN_POINT ( 'NONE',  ( 0.9542513359644848592, 2.159166806557303531, -0.1069676271590186134 ) ) ;
#51576 = CARTESIAN_POINT ( 'NONE',  ( 3.362146542844654196, 0.8852860682435258477, 1.761578244261922332 ) ) ;
#51577 = CARTESIAN_POINT ( 'NONE',  ( 6.609000000000038177, 0.002801690667396730672, 2.000160786441218530 ) ) ;
#51578 = CARTESIAN_POINT ( 'NONE',  ( 3.087376005906359744, -0.7846555324184587565, 1.776656735299622980 ) ) ;
#51581 = ORIENTED_EDGE ( 'NONE', *, *, #56226, .T. ) ;
#51580 = CARTESIAN_POINT ( 'NONE',  ( -5.004368097219957789, 5.011053332944274352, 0.000000000000000000 ) ) ;
#51579 = CARTESIAN_POINT ( 'NONE',  ( -8.120970824461345217, 12.41829036193951730, 0.7216878364870458196 ) ) ;
#51582 = CARTESIAN_POINT ( 'NONE',  ( -5.167065940139584868, 6.161236697318522637, 1.082531754730549078 ) ) ;
#51583 = CARTESIAN_POINT ( 'NONE',  ( 3.223806664999388172, 6.983134552466421674, -0.7998128361456362523 ) ) ;
#51584 = CARTESIAN_POINT ( 'NONE',  ( -4.573896719763875574, 6.429575154514868274, -1.599625672291271394 ) ) ;
#51586 = ORIENTED_EDGE ( 'NONE', *, *, #96537, .T. ) ;
#51585 = CARTESIAN_POINT ( 'NONE',  ( -6.577640801285370209, 7.702944352034914566, -1.199719254218452047 ) ) ;
#51587 = CARTESIAN_POINT ( 'NONE',  ( -9.937763408692600109, 10.69640485300394417, -0.7216878364870267237 ) ) ;
#51588 = CARTESIAN_POINT ( 'NONE',  ( 0.3763673390903346516, 1.272619870141003418, 1.802674353332263335 ) ) ;
#51590 = EDGE_CURVE ( 'NONE', #10112, #116404, #173667, .T. ) ;
#51589 = CARTESIAN_POINT ( 'NONE',  ( 1.642778471875001811, -3.142708332855375986, 2.845375778867859751 ) ) ;
#51591 = CARTESIAN_POINT ( 'NONE',  ( 4.821123798404616245, -1.750560105953799184, -0.8856655065374097191 ) ) ;
#51592 = CARTESIAN_POINT ( 'NONE',  ( 1.547500230860882287, -1.423960469535384465, 1.427938386157491246 ) ) ;
#51593 = ORIENTED_EDGE ( 'NONE', *, *, #120271, .F. ) ;
#51594 = CARTESIAN_POINT ( 'NONE',  ( 3.679011075472499392, 1.786488794941149871, -1.136238802782759238 ) ) ;
#51595 = CARTESIAN_POINT ( 'NONE',  ( -1.499999999999997780, 2.931250000682818158, 1.214306433183764966E-14 ) ) ;
#51597 = CARTESIAN_POINT ( 'NONE',  ( -6.579784621333750749, 6.570836901177822931, 0.7998128361456341429 ) ) ;
#51596 = FACE_OUTER_BOUND ( 'NONE', #169447, .T. ) ;
#51598 = CARTESIAN_POINT ( 'NONE',  ( 2.730204174461122069, 0.2256132759956077649, 1.827196471909063202 ) ) ;
#51599 = ORIENTED_EDGE ( 'NONE', *, *, #76523, .F. ) ;
#51600 = CARTESIAN_POINT ( 'NONE',  ( -8.727698198895085469, 11.20540053684285553, -1.599625672291263179 ) ) ;
#51601 = FILL_AREA_STYLE ('',( #169604 ) ) ;
#51602 = CARTESIAN_POINT ( 'NONE',  ( 4.799148092389167175, -0.2621723519393297508, -2.104289960152181393 ) ) ;
#51603 = CARTESIAN_POINT ( 'NONE',  ( -0.7499999999999972244, 4.389583334016150751, -1.299038105676652899 ) ) ;
#51604 = CARTESIAN_POINT ( 'NONE',  ( 7.461064606222022277, 7.598996883547496139, 1.040834085586084257E-14 ) ) ;
#51605 = CARTESIAN_POINT ( 'NONE',  ( 5.079397637315079983, 1.924335792300538861, -0.7379084467255945246 ) ) ;
#51606 = AXIS2_PLACEMENT_3D ( 'NONE', #176277, #27879, #46282 ) ;
#51609 = CARTESIAN_POINT ( 'NONE',  ( 2.735704033801298785, 1.827604811068459956, 0.2230458208379028362 ) ) ;
#51608 = CARTESIAN_POINT ( 'NONE',  ( 0.7482324461028444507, -1.846328264857381996, -0.2332022352751206007 ) ) ;
#51607 = CARTESIAN_POINT ( 'NONE',  ( -1.620863580070949883, 0.5000000000000004441, 1.903365770102947607 ) ) ;
#51610 = CARTESIAN_POINT ( 'NONE',  ( 8.398386088661320414, 11.88553530582519357, -1.199719254218446718 ) ) ;
#51611 =( NAMED_UNIT ( * ) SI_UNIT ( $, .STERADIAN. ) SOLID_ANGLE_UNIT ( ) );
#51612 = FACE_OUTER_BOUND ( 'NONE', #56267, .T. ) ;
#51613 = DIRECTION ( 'NONE',  ( -7.610300982150707428E-15, -1.000000000000000000, 7.722633184682877167E-15 ) ) ;
#51614 = CARTESIAN_POINT ( 'NONE',  ( 2.561379550486083012, -1.920685204893451292, -1.086737900330703166 ) ) ;
#51615 = CARTESIAN_POINT ( 'NONE',  ( 4.341306091576823789, -1.971171287362062818, 1.110239852968941232 ) ) ;
#51616 = CARTESIAN_POINT ( 'NONE',  ( -8.202319746587722449, 8.671720580548228696, 1.040834085586084257E-14 ) ) ;
#51617 = CARTESIAN_POINT ( 'NONE',  ( 4.623216614435611937, 1.579690555364177351, 0.8866180403494609008 ) ) ;
#51618 = CARTESIAN_POINT ( 'NONE',  ( 4.839036869973236676, -1.621808105726432414, -1.019334933273335242 ) ) ;
#51619 = DIRECTION ( 'NONE',  ( -0.000000000000000000, -1.000000000000000000, -0.000000000000000000 ) ) ;
#51620 = CARTESIAN_POINT ( 'NONE',  ( 4.364113771024707766, 0.9285358673545366370, 1.739096546318192882 ) ) ;
#51621 = CARTESIAN_POINT ( 'NONE',  ( 5.313307075269409374, -0.2735208697075517947, 1.850433306854900817 ) ) ;
#51622 = AXIS2_PLACEMENT_3D ( 'NONE', #168315, #53492, #164065 ) ;
#51623 = CARTESIAN_POINT ( 'NONE',  ( 5.353892109531869004, -0.6699537489362316078, 1.736457084658560079 ) ) ;
#51624 = CARTESIAN_POINT ( 'NONE',  ( -7.555533889508359024E-14, -9.900000000000005684, 9.500331257164617682 ) ) ;
#51625 = CARTESIAN_POINT ( 'NONE',  ( 0.5500180045474002410, 0.9981291480291035745, 1.752136972055001518 ) ) ;
#51627 = CARTESIAN_POINT ( 'NONE',  ( 1.313257463657933055, 1.858222661572891621, 0.9912184023134795741 ) ) ;
#51626 = CARTESIAN_POINT ( 'NONE',  ( -2.290964770585000920, 5.616616632417037458, -0.7216878364870257245 ) ) ;
#51628 = CARTESIAN_POINT ( 'NONE',  ( 10.57266086055835075, 11.22919251360659310, 0.000000000000000000 ) ) ;
#51630 = CARTESIAN_POINT ( 'NONE',  ( -10.64045162862669081, 11.30828174301964140, -0.7998128361456221525 ) ) ;
#51629 = DIRECTION ( 'NONE',  ( -3.330669073875479975E-16, 2.334947598634344260E-16, 1.000000000000000000 ) ) ;
#51631 = CARTESIAN_POINT ( 'NONE',  ( 3.357788437482766675, -1.608272433257527556, -1.382313803475518244 ) ) ;
#51632 = CARTESIAN_POINT ( 'NONE',  ( 1.394453263437886604E-15, -2.668749999044085275, 3.474999999999999645 ) ) ;
#51634 = EDGE_CURVE ( 'NONE', #45033, #95692, #190979, .T. ) ;
#51633 = CARTESIAN_POINT ( 'NONE',  ( 2.162373415809074828, 2.019440163517810749, 0.04526320522070524655 ) ) ;
#51635 = CARTESIAN_POINT ( 'NONE',  ( 0.6823417656249899377, 2.092708333674753174, 1.181850606188767472 ) ) ;
#51636 = CARTESIAN_POINT ( 'NONE',  ( 6.720655732516660485, 7.629137130509104914, 2.326260288887294969 ) ) ;
#51637 = CARTESIAN_POINT ( 'NONE',  ( 3.147464216666835402, 6.823792019419957278, -0.7998128361456291469 ) ) ;
#51638 = ORIENTED_EDGE ( 'NONE', *, *, #72896, .T. ) ;
#51639 = CARTESIAN_POINT ( 'NONE',  ( 2.073706595668877384, 2.069181010895416950, -0.6253580070983978390 ) ) ;
#51640 = CARTESIAN_POINT ( 'NONE',  ( 6.609999999999973674, 0.5530568637619069916, 2.330679033986877258 ) ) ;
#51643 = CARTESIAN_POINT ( 'NONE',  ( 4.067082894419602468, 3.847277586352047862, -0.7216878364870188411 ) ) ;
#51642 = CARTESIAN_POINT ( 'NONE',  ( 11.97297122925985313, 9.801250793269113970, -0.8121202983519358876 ) ) ;
#51641 = CARTESIAN_POINT ( 'NONE',  ( 3.573456005653643519, 6.326726552307992080, -1.199719254218453823 ) ) ;
#51644 = LINE ( 'NONE', #117768, #193187 ) ;
#51645 = CARTESIAN_POINT ( 'NONE',  ( -7.749822179018673651, -6.479141885268356660, 7.806953216197599410 ) ) ;
#51646 = CARTESIAN_POINT ( 'NONE',  ( -6.724481002698120768, 9.828683022247721723, -1.082531754730538864 ) ) ;
#51647 = EDGE_CURVE ( 'NONE', #152273, #93282, #29526, .T. ) ;
#51648 = CARTESIAN_POINT ( 'NONE',  ( 0.6268464039562298140, 0.1668571106153530770, 2.185281662807083691 ) ) ;
#51649 = CARTESIAN_POINT ( 'NONE',  ( 0.000000000000000000, 7.849261790823902629, 9.499999999999992895 ) ) ;
#51651 = CARTESIAN_POINT ( 'NONE',  ( 1.364683531249997417, 11.73437500034139802, 2.602085213965210642E-15 ) ) ;
#51650 = CARTESIAN_POINT ( 'NONE',  ( 1.288340396327339432, -1.015645312862264227, 2.021827887327799722 ) ) ;
#51652 = CARTESIAN_POINT ( 'NONE',  ( -7.635213062790267458, 12.05949900656400686, 0.000000000000000000 ) ) ;
#51653 = CARTESIAN_POINT ( 'NONE',  ( -5.395781948114519722, 5.397426482329451325, 0.000000000000000000 ) ) ;
#51655 = AXIS2_PLACEMENT_3D ( 'NONE', #138, #116115, #53190 ) ;
#51654 = CARTESIAN_POINT ( 'NONE',  ( -0.6823417656250003738, 2.280208333674753174, -1.181850606188749264 ) ) ;
#51656 = CARTESIAN_POINT ( 'NONE',  ( 4.661274270878652537, 8.290979908523663511, 0.5017903844357074483 ) ) ;
#51657 = CARTESIAN_POINT ( 'NONE',  ( -1.402160292154681736E-14, 9.312500000000005329, 1.732050807568881190 ) ) ;
#51658 = CARTESIAN_POINT ( 'NONE',  ( 4.459404883141235842, 0.3742951803532655330, -1.683599696842478677 ) ) ;
#51659 = CARTESIAN_POINT ( 'NONE',  ( 3.217027588192558074, 6.975225629525113824, -1.734723475976807094E-15 ) ) ;
#51660 = CARTESIAN_POINT ( 'NONE',  ( 2.038023431533928509, 1.749628755847471018, 0.2652362932685590757 ) ) ;
#51661 = CARTESIAN_POINT ( 'NONE',  ( 4.911249081476436018, 1.917979745144289261, 1.091307337132418454 ) ) ;
#51662 = ORIENTED_EDGE ( 'NONE', *, *, #180142, .F. ) ;
#51664 = CARTESIAN_POINT ( 'NONE',  ( 4.482678814652188315, -1.316266026504675057, 1.532109124154117596 ) ) ;
#51663 = VECTOR ( 'NONE', #209932, 1000.000000000000000 ) ;
#51665 = CARTESIAN_POINT ( 'NONE',  ( -4.911796789900812144, 8.952456364851418158, 0.7998128361456291469 ) ) ;
#51666 = CARTESIAN_POINT ( 'NONE',  ( 5.448842280278080707, -1.824126957265741256, -0.8596167168879662590 ) ) ;
#51667 = ORIENTED_EDGE ( 'NONE', *, *, #103372, .T. ) ;
#51668 = VECTOR ( 'NONE', #18155, 1000.000000000000000 ) ;
#51669 = CARTESIAN_POINT ( 'NONE',  ( 2.184254540302111636, -1.834043650784190405, -0.3674020703766099905 ) ) ;
#51670 = ADVANCED_FACE ( 'NONE', ( #60951 ), #105548, .F. ) ;
#51671 = SPHERICAL_SURFACE ( 'NONE', #117188, 0.08000000000000000167 ) ;
#51672 = CARTESIAN_POINT ( 'NONE',  ( 1.775505761281343631, 0.3235837346332003372, -1.884644527778083001 ) ) ;
#51673 = CARTESIAN_POINT ( 'NONE',  ( -4.662342535738044802, 8.068669011459252971, 0.7682199413396522125 ) ) ;
#51674 = CARTESIAN_POINT ( 'NONE',  ( -11.25372107582773396, 4.972923339538419363, -5.839092030517418763 ) ) ;
#51675 = CARTESIAN_POINT ( 'NONE',  ( -7.004500933659051576, -6.920331743269724889, 7.004500933659075557 ) ) ;
#51676 = CARTESIAN_POINT ( 'NONE',  ( 0.6823417656249899377, 4.488541667008086655, -1.181850606188754593 ) ) ;
#51677 = CARTESIAN_POINT ( 'NONE',  ( 0.2110004604562870645, 1.588762659912812403, -1.064147093309028680 ) ) ;
#51678 = CARTESIAN_POINT ( 'NONE',  ( 6.712695452541852070, 7.004101914153185504, 0.000000000000000000 ) ) ;
#51679 = CARTESIAN_POINT ( 'NONE',  ( 1.381223342121252085, -0.05156877537583307025, 1.961363007973878858 ) ) ;
#51680 = CARTESIAN_POINT ( 'NONE',  ( 0.1399997263886003374, 0.002789056014650820314, -1.999853399661279063 ) ) ;
#51681 = CARTESIAN_POINT ( 'NONE',  ( -5.635349125135588721, 6.603604063193491136, 1.199719254218452935 ) ) ;
#51682 = CARTESIAN_POINT ( 'NONE',  ( 5.344028447597857223, -1.346983732444573256, -1.637812552581649594 ) ) ;
#51684 =( LENGTH_UNIT ( ) NAMED_UNIT ( * ) SI_UNIT ( .MILLI., .METRE. ) );
#51683 = CARTESIAN_POINT ( 'NONE',  ( 7.560643217915098191, 11.97250085420964716, -0.7998128361456291469 ) ) ;
#51685 = CARTESIAN_POINT ( 'NONE',  ( 0.2802489257003986656, -1.812731005579379051, -0.4610361243657657981 ) ) ;
#51686 = CARTESIAN_POINT ( 'NONE',  ( 0.6823417656249882723, 1.926041667008083991, -1.181850606188749264 ) ) ;
#51687 = CARTESIAN_POINT ( 'NONE',  ( 1.740491373288379995, 1.155656410672186496, -1.648304894270665510 ) ) ;
#51688 = ORIENTED_EDGE ( 'NONE', *, *, #161732, .F. ) ;
#51690 = CARTESIAN_POINT ( 'NONE',  ( 1.493934562436026292, -2.100767169153750391, 0.2631679424494152153 ) ) ;
#51689 = CARTESIAN_POINT ( 'NONE',  ( -7.700668062882072284, 10.00719871149432549, -1.443375672974059665 ) ) ;
#51691 = CARTESIAN_POINT ( 'NONE',  ( 11.53430674162873260, 7.314159620192208777, 3.343773152020875106 ) ) ;
#51692 = CARTESIAN_POINT ( 'NONE',  ( 3.139188941651628539, -0.1496422021231707811, -2.064996656166856237 ) ) ;
#51693 = CARTESIAN_POINT ( 'NONE',  ( 4.146814880933355596, 5.931313009212638931, 1.599625672291261402 ) ) ;
#51694 = CARTESIAN_POINT ( 'NONE',  ( 3.088225128862704949, 6.824956093640315302, 0.7998128361456281477 ) ) ;
#51695 = ORIENTED_EDGE ( 'NONE', *, *, #210252, .F. ) ;
#51697 = CARTESIAN_POINT ( 'NONE',  ( 3.408985558832261731, 6.064568021024562938, 1.199719254218462483 ) ) ;
#51696 = CARTESIAN_POINT ( 'NONE',  ( 5.208965158259858619, -0.3072975092734456237, 2.067794563079519143 ) ) ;
#51700 = ORIENTED_EDGE ( 'NONE', *, *, #139653, .T. ) ;
#51699 = CARTESIAN_POINT ( 'NONE',  ( 2.719172733320520674, 1.531317187073286901, 0.9673847807401686483 ) ) ;
#51698 = CARTESIAN_POINT ( 'NONE',  ( 3.241029684393876842, -1.610631872634618933, 0.8593927405577477252 ) ) ;
#51701 = CYLINDRICAL_SURFACE ( 'NONE', #209269, 2.000000000000006661 ) ;
#51702 = CARTESIAN_POINT ( 'NONE',  ( 10.40314139648789471, 12.22719254644319697, 6.661332869700506976 ) ) ;
#51703 = CARTESIAN_POINT ( 'NONE',  ( 5.508869005905306260, 1.674340917344345536, -1.437622030140395912 ) ) ;
#51704 = CARTESIAN_POINT ( 'NONE',  ( -1.364683531250014514, 9.901041667008064096, -0.7879004041258335089 ) ) ;
#51705 = VERTEX_POINT ( 'NONE', #112973 ) ;
#51706 = CARTESIAN_POINT ( 'NONE',  ( 4.090413894173472009, -1.098427525215146749, 1.565146720495188104 ) ) ;
#51707 = B_SPLINE_CURVE_WITH_KNOTS ( 'NONE', 3,
 ( #127772, #177496, #95192, #105097, #88845, #188453, #73641, #189520, #155969, #41167, #174368, #206829, #25947, #9700, #123557, #141885, #139739, #159157, #75778, #154902, #157044, #187383, #57392, #56332, #122491, #39015, #10756, #205763, #6486, #8632, #204681, #40085, #207894, #72562, #140816, #76830, #58463, #107276 ),
 .UNSPECIFIED., .F., .F.,
 ( 4, 2, 2, 2, 2, 2, 2, 2, 2, 2, 2, 2, 2, 2, 2, 2, 2, 2, 4 ),
 ( -5.999999999960951245E-08, 0.001341446902958200009, 0.002682953805916399662, 0.004024460708874599314, 0.005365967611832798967, 0.006707474514790999487, 0.008048981417749198272, 0.009390488320707397057, 0.01006124177218649905, 0.01073199522366559758, 0.01207350212662379636, 0.01341500902958199862, 0.01475651593254019914, 0.01542726938401930113, 0.01609802283549840313, 0.01743952973845660712, 0.01878103664141481111, 0.02012254354437301856, 0.02146405044733121908 ),
 .UNSPECIFIED. ) ;
#51708 = CARTESIAN_POINT ( 'NONE',  ( -4.973143418114339021, 4.696422164088486895, 0.7998128361456341429 ) ) ;
#51709 = CIRCLE ( 'NONE', #103500, 2.500000000000000888 ) ;
#51710 = CARTESIAN_POINT ( 'NONE',  ( 7.958799866421889746, 9.244020251369077457, -1.199719254218441611 ) ) ;
#51711 = B_SPLINE_CURVE_WITH_KNOTS ( 'NONE', 3,
 ( #57882, #173799, #106689, #124044, #125109, #174865, #104512, #41661, #58951, #108839 ),
 .UNSPECIFIED., .F., .F.,
 ( 4, 1, 1, 1, 1, 1, 1, 4 ),
 ( 0.000000000000000000, 0.09373397616858752945, 0.1863105892815605236, 0.2574079725677296260, 0.3612190813870841954, 0.5208938042821120717, 0.7336009914826546741, 1.000000000000000000 ),
 .UNSPECIFIED. ) ;
#51712 = CARTESIAN_POINT ( 'NONE',  ( -5.558564015327488080E-14, 0.4843750003414603600, 1.570758158831762286 ) ) ;
#51713 = CARTESIAN_POINT ( 'NONE',  ( 3.823036128929238942, 7.404033217152015567, 1.040834085586084257E-14 ) ) ;
#51714 = CARTESIAN_POINT ( 'NONE',  ( -11.89942855770814134, 12.30000000000000071, 0.6999999999999992895 ) ) ;
#51715 = DIRECTION ( 'NONE',  ( -5.578564026256490882E-16, -1.000000000000000000, -9.066213480720158442E-32 ) ) ;
#51716 = CARTESIAN_POINT ( 'NONE',  ( -9.484899655072714708, -6.713792789267452932, 0.3525790917593041307 ) ) ;
#51717 = CARTESIAN_POINT ( 'NONE',  ( 5.346851039111033543, 6.199209027673978412, -2.420000000000000373 ) ) ;
#51718 = CARTESIAN_POINT ( 'NONE',  ( 3.479631686803522417, 1.184185218286455621, 1.448006030947253331 ) ) ;
#51719 = CARTESIAN_POINT ( 'NONE',  ( 8.154303043976348420, 8.478051404252736845, 0.7998128361456281477 ) ) ;
#51720 = CARTESIAN_POINT ( 'NONE',  ( -6.236387472606141458, 10.21960978477508952, -0.7216878364870278340 ) ) ;
#51721 = CARTESIAN_POINT ( 'NONE',  ( 5.335297142177534369, 6.183267073083954735, -1.199719254218452047 ) ) ;
#51722 = CARTESIAN_POINT ( 'NONE',  ( 0.3562224712859492493, -1.968894089644295686, -0.05400687454796929826 ) ) ;
#51723 = CARTESIAN_POINT ( 'NONE',  ( 2.829704019156009220, 0.7231233381281775285, -1.882481713119791067 ) ) ;
#51724 = CARTESIAN_POINT ( 'NONE',  ( -7.914208982075130905, 10.25632978388623684, -1.599625672291263179 ) ) ;
#51725 = CARTESIAN_POINT ( 'NONE',  ( 7.015418140428412386, 7.149352350113456822, 0.7998128361456331437 ) ) ;
#51726 = CARTESIAN_POINT ( 'NONE',  ( -6.520158902582635640, 5.290451655907115303, 2.438235897557452514 ) ) ;
#51727 = CARTESIAN_POINT ( 'NONE',  ( 2.308753661914957345, 1.958203289975643191, 0.9839491227633669901 ) ) ;
#51728 = CARTESIAN_POINT ( 'NONE',  ( -2.950870989268691957, 6.594433254122103349, -0.7998128361456281477 ) ) ;
#51729 = CARTESIAN_POINT ( 'NONE',  ( 4.041739190649647817, 6.769093918182960579, -1.082531754730548412 ) ) ;
#51730 = CARTESIAN_POINT ( 'NONE',  ( 9.596473800374404561, 10.09030761005864285, 0.000000000000000000 ) ) ;
#51731 = CARTESIAN_POINT ( 'NONE',  ( 3.704402285031850539, 5.344888637335695414, -1.599625672291262513 ) ) ;
#51732 = CARTESIAN_POINT ( 'NONE',  ( 7.349928672384119288, 8.707909884937221179, 1.082531754730549967 ) ) ;
#51733 = ORIENTED_EDGE ( 'NONE', *, *, #112300, .F. ) ;
#51735 = CARTESIAN_POINT ( 'NONE',  ( 0.5396978354115729015, -1.910900059352708125, 0.6334021227705748380 ) ) ;
#51734 = CARTESIAN_POINT ( 'NONE',  ( 3.544333174469185721, -1.503253232081468216, 1.062929765333266108 ) ) ;
#51736 = CARTESIAN_POINT ( 'NONE',  ( 3.462589497157672724, 1.809959297682335100, 1.416443637550690804 ) ) ;
#51738 = CARTESIAN_POINT ( 'NONE',  ( 1.076741303291447460, 1.716668495539741324, 0.7189669686299257068 ) ) ;
#51737 = CARTESIAN_POINT ( 'NONE',  ( -5.000000000000024869, 0.2350621082554960051, 0.7750000000000117906 ) ) ;
#51739 = CARTESIAN_POINT ( 'NONE',  ( 1.642778471875000035, -4.076041666188710444, -2.845375778867859751 ) ) ;
#51740 = CARTESIAN_POINT ( 'NONE',  ( -4.055860508782465068, 7.883587693554856557, 1.040834085586084257E-14 ) ) ;
#51741 = CARTESIAN_POINT ( 'NONE',  ( 0.000000000000000000, 3.480000000000000426, -2.000000000000000000 ) ) ;
#51742 = CARTESIAN_POINT ( 'NONE',  ( 5.045129621168108258, 0.1466893748028277877, 1.906852434080000824 ) ) ;
#51743 = CARTESIAN_POINT ( 'NONE',  ( -7.811469059767924605, 12.26513100303794168, -0.7998128361456281477 ) ) ;
#51744 = CARTESIAN_POINT ( 'NONE',  ( 6.276967689384127524, 6.888745287521969907, 0.7578909454171089966 ) ) ;
#51745 = CARTESIAN_POINT ( 'NONE',  ( -6.455090533882201775, 8.624301270986276080, -1.443375672974066548 ) ) ;
#51747 = CARTESIAN_POINT ( 'NONE',  ( 2.430351462470367707, 1.813921419787648315, 0.4566771774890953095 ) ) ;
#51746 = CARTESIAN_POINT ( 'NONE',  ( 4.071883345936186060, -1.202257327942996445, 1.710302118368298707 ) ) ;
#51748 = CARTESIAN_POINT ( 'NONE',  ( 5.965224400332808763, 9.903252867122883885, -0.7216878364870267237 ) ) ;
#51749 = CARTESIAN_POINT ( 'NONE',  ( 1.364683531249990311, 5.676041667008088432, 0.7879004041258499402 ) ) ;
#51750 = CARTESIAN_POINT ( 'NONE',  ( 2.841039829263870775, 0.6241981022326682504, -1.624847995071764917 ) ) ;
#51751 = AXIS2_PLACEMENT_3D ( 'NONE', #103842, #137417, #55090 ) ;
#51752 = CARTESIAN_POINT ( 'NONE',  ( 5.671388329218120639, 5.511041227042920099, 1.040834085586084257E-14 ) ) ;
#51754 = CARTESIAN_POINT ( 'NONE',  ( 4.517891501851804215, 6.293959390292322986, -1.599625672291255185 ) ) ;
#51753 = CARTESIAN_POINT ( 'NONE',  ( -0.4019237886467001974, 11.58258545099816494, 1.500000000000001998 ) ) ;
#51755 = CARTESIAN_POINT ( 'NONE',  ( 4.072648179469573471, -1.610461668677556801, -0.6182406629154230115 ) ) ;
#51756 = CARTESIAN_POINT ( 'NONE',  ( -6.015013705957189316, 10.16926642359206134, 0.7998128361456481317 ) ) ;
#51757 =( BOUNDED_SURFACE ( )  B_SPLINE_SURFACE ( 3, 2, ( 
 ( #117943, #66957, #133096 ),
 ( #53949, #120088, #199094 ),
 ( #116866, #85376, #183936 ),
 ( #186063, #35548, #169827 ),
 ( #19294, #119011, #21413 ),
 ( #124373, #157868, #73381 ) ),
 .UNSPECIFIED., .F., .F., .T. ) 
 B_SPLINE_SURFACE_WITH_KNOTS ( ( 4, 2, 4 ),
 ( 3, 3 ),
 ( -4.336808689942017736E-19, 0.0003831416164015013842, 0.0007662832328030032020 ),
 ( 0.000000000000000000, 1.000000000000000000 ),
 .UNSPECIFIED. ) 
 GEOMETRIC_REPRESENTATION_ITEM ( )  RATIONAL_B_SPLINE_SURFACE ( (
 ( 1.000000000000000000, 0.7071067811865475727, 1.000000000000000000),
 ( 1.000000000000000000, 0.6829713513653472567, 1.000000000000000000),
 ( 1.000000000000000000, 0.6534833722372194176, 1.000000000000000000),
 ( 1.000000000000000000, 0.6054027484662655167, 1.000000000000000000),
 ( 1.000000000000000000, 0.5875453974414952540, 1.000000000000000000),
 ( 1.000000000000000000, 0.5879095031487528988, 1.000000000000000000) ) ) 
 REPRESENTATION_ITEM ( '' )  SURFACE ( )  );
#51758 = CARTESIAN_POINT ( 'NONE',  ( 6.111994396789379280, -2.190734547077430872, 0.2660306753756238041 ) ) ;
#51759 =( NAMED_UNIT ( * ) PLANE_ANGLE_UNIT ( ) SI_UNIT ( $, .RADIAN. ) );
#51760 = CARTESIAN_POINT ( 'NONE',  ( -0.3282377607281419252, 0.8638354509981874818, 1.224999999999977440 ) ) ;
#51761 = CARTESIAN_POINT ( 'NONE',  ( 4.065408448962204879, 1.859168595270783042, 1.121007083124803572 ) ) ;
#51762 = CARTESIAN_POINT ( 'NONE',  ( 1.998415063578623085, -0.4859047700337820741, -1.759764234465097221 ) ) ;
#51763 = CARTESIAN_POINT ( 'NONE',  ( 3.834746474454188013E-15, 12.31250000000000178, 1.500000000000001554 ) ) ;
#51764 = CARTESIAN_POINT ( 'NONE',  ( 5.137957784024314911, 2.114781318005181099, -0.1070058694263714694 ) ) ;
#51765 = VERTEX_POINT ( 'NONE', #67309 ) ;
#51767 = CARTESIAN_POINT ( 'NONE',  ( 0.6823417656249882723, 1.988541667008083991, -1.181850606188749264 ) ) ;
#51766 = CARTESIAN_POINT ( 'NONE',  ( 5.390252792638895230, -0.5542908586613685129, -2.224220739628431254 ) ) ;
#51768 = CARTESIAN_POINT ( 'NONE',  ( 9.725276259704228821, 10.24057714594344048, 0.7998128361456462443 ) ) ;
#51769 = EDGE_CURVE ( 'NONE', #5447, #54210, #67494, .T. ) ;
#51770 = CARTESIAN_POINT ( 'NONE',  ( 1.770341816056511863, 2.114587264445011883, -0.1591180397043714667 ) ) ;
#51771 = PRODUCT_DEFINITION ( 'UNKNOWN', '', #163028, #527 ) ;
#51772 = CARTESIAN_POINT ( 'NONE',  ( -5.422898255786203769, 6.389431388914436738, -1.082531754730544860 ) ) ;
#51773 = PRESENTATION_LAYER_ASSIGNMENT (  '', '', ( #203879 ) ) ;
#51774 = CARTESIAN_POINT ( 'NONE',  ( 2.223174002961016082, 5.537527403522402025, -0.7216878364870267237 ) ) ;
#51775 = CARTESIAN_POINT ( 'NONE',  ( -6.249945625775490399, 7.354319987235250267, 1.082531754730549967 ) ) ;
#51776 = CARTESIAN_POINT ( 'NONE',  ( 6.438351068470751670, -1.168633322568404243, 1.829565972870864865 ) ) ;
#51778 = CARTESIAN_POINT ( 'NONE',  ( -1.500000000000001110, 12.55208333401612641, 0.8660254037844419273 ) ) ;
#51777 = CARTESIAN_POINT ( 'NONE',  ( 0.09263662810811511272, -9.999999999999994671, 10.91955560153697746 ) ) ;
#51780 = EDGE_LOOP ( 'NONE', ( #179641, #126856, #72963, #923 ) ) ;
#51779 = CARTESIAN_POINT ( 'NONE',  ( 1.172868535947855673, 0.9048325283492463234, 2.028842389263245227 ) ) ;
#51781 = CARTESIAN_POINT ( 'NONE',  ( 6.363907750917786821, -0.1017471579566435469, -2.013986097687201049 ) ) ;
#51783 = CARTESIAN_POINT ( 'NONE',  ( 4.662968416576672048, 1.597784760895196721, -1.304382716673627707 ) ) ;
#51782 = CARTESIAN_POINT ( 'NONE',  ( 3.876741858503734761, 6.610283703974623393, 1.199719254218462483 ) ) ;
#51785 = CARTESIAN_POINT ( 'NONE',  ( -6.265276382846530545, 6.482112999508623297, 0.000000000000000000 ) ) ;
#51784 = CARTESIAN_POINT ( 'NONE',  ( 6.099189001301251523, 8.209082816308541197, 1.599625672291268286 ) ) ;
#51786 = CARTESIAN_POINT ( 'NONE',  ( 6.688968683495743583, 8.897159112202094988, -1.599625672291283607 ) ) ;
#51787 = CARTESIAN_POINT ( 'NONE',  ( 1.642778471875000035, -1.976041666188709689, -2.845375778867859751 ) ) ;
#51788 = CARTESIAN_POINT ( 'NONE',  ( -7.065207446497166366, 9.336104335703744539, 0.000000000000000000 ) ) ;
#51789 = CARTESIAN_POINT ( 'NONE',  ( 0.1290073198303761104, -1.910558061381230521, 0.8492679875119947264 ) ) ;
#51790 = CARTESIAN_POINT ( 'NONE',  ( 4.852185490356213826, 0.1948433276699329531, -2.006959737079899497 ) ) ;
#51791 = CARTESIAN_POINT ( 'NONE',  ( 4.581507094455529838, -0.8636776874328588871, 1.626104626046148249 ) ) ;
#51792 = CARTESIAN_POINT ( 'NONE',  ( 3.655894977179307226, 7.416961240017848844, -0.7998128361456291469 ) ) ;
#51793 = CARTESIAN_POINT ( 'NONE',  ( 0.6040130627208201153, -0.5744563726430768069, -1.626443300898507305 ) ) ;
#51794 = CARTESIAN_POINT ( 'NONE',  ( 0.3566581422463632189, -1.900417414521380133, -0.6748426577906709856 ) ) ;
#51795 = CARTESIAN_POINT ( 'NONE',  ( 0.4230186368967851496, -1.631317381931682631, -1.619748931356496113 ) ) ;
#51796 = CARTESIAN_POINT ( 'NONE',  ( -4.713430959045263435, 8.650753218861462202, 0.7998128361456481317 ) ) ;
#51797 = CARTESIAN_POINT ( 'NONE',  ( 1.634417699101225585, 1.115656568974830343, -1.968152581808318757 ) ) ;
#51798 = CARTESIAN_POINT ( 'NONE',  ( 3.528042858452341335, -1.254676591636105121, -1.691379958841844111 ) ) ;
#51799 = CARTESIAN_POINT ( 'NONE',  ( -4.773352600463090845, 7.726605912919016106, 1.199719254218452935 ) ) ;
#51800 = CARTESIAN_POINT ( 'NONE',  ( 5.774883364416965037, 8.824782127540085952, -1.199719254218440723 ) ) ;
#51801 = CARTESIAN_POINT ( 'NONE',  ( 6.170369307550815030, 8.292126506933040986, 1.443375672974064550 ) ) ;
#51802 = CARTESIAN_POINT ( 'NONE',  ( 6.562500042754934704, -1.451030237095789266, -1.451031289060847440 ) ) ;
#51803 = CARTESIAN_POINT ( 'NONE',  ( -4.238895582566952314, 8.097128612970093897, 1.040834085586084257E-14 ) ) ;
#51804 = CARTESIAN_POINT ( 'NONE',  ( 5.626270559546810546, 8.547437505237857280, 1.082531754730558626 ) ) ;
#51805 = CARTESIAN_POINT ( 'NONE',  ( -0.7500000000000006661, 2.608333333333358262, -1.299038105676652011 ) ) ;
#51806 = CARTESIAN_POINT ( 'NONE',  ( -5.122283107864663343, 4.870418468797203637, 0.000000000000000000 ) ) ;
#51807 = CARTESIAN_POINT ( 'NONE',  ( 4.869482922584397855, -1.877140712267670430, -1.187567259214457271 ) ) ;
#51808 = CARTESIAN_POINT ( 'NONE',  ( 3.468858241077877214, 0.05382521638562161315, -2.190950023606648145 ) ) ;
#51809 = CARTESIAN_POINT ( 'NONE',  ( -5.870844209917351009, 6.808071985447069707, -1.199719254218446718 ) ) ;
#51810 = CARTESIAN_POINT ( 'NONE',  ( -11.89197816957260478, 9.799999999999998934, 0.8055420615339484725 ) ) ;
#51811 = CARTESIAN_POINT ( 'NONE',  ( 5.353941776413853937, -0.7077614321437855072, 1.829919609802006741 ) ) ;
#51812 = CARTESIAN_POINT ( 'NONE',  ( -1.201851678989727383E-14, 2.696875000341417916, -1.575800808251660134 ) ) ;
#51813 = CARTESIAN_POINT ( 'NONE',  ( -2.279984679289828176, 5.601133616484927025, -0.06592222766762731445 ) ) ;
#51814 = CARTESIAN_POINT ( 'NONE',  ( -6.249945626219832739, 6.393950773452325542, 1.040834085586084257E-14 ) ) ;
#51815 = CARTESIAN_POINT ( 'NONE',  ( 4.447591161967184625, -1.937652164471121763, 0.8620916771790232414 ) ) ;
#51816 = CARTESIAN_POINT ( 'NONE',  ( -6.834718835064852449, 8.106831741398025315, 1.082531754730549078 ) ) ;
#51817 = EDGE_LOOP ( 'NONE', ( #50342, #77428 ) ) ;
#51819 = CARTESIAN_POINT ( 'NONE',  ( 6.825078400183575589, -0.005632053428735600553, 2.144262460745151255 ) ) ;
#51818 = CARTESIAN_POINT ( 'NONE',  ( -4.828112100242279325, 8.646898193675708555, -0.7216878364870338292 ) ) ;
#51820 = CARTESIAN_POINT ( 'NONE',  ( 6.166260936116925606, 6.088392601758203071, 0.7998128361456341429 ) ) ;
#51821 = CARTESIAN_POINT ( 'NONE',  ( 4.581507094455529838, -0.8636776874328588871, 1.626104626046148249 ) ) ;
#51822 =( NAMED_UNIT ( * ) PLANE_ANGLE_UNIT ( ) SI_UNIT ( $, .RADIAN. ) );
#51823 = CARTESIAN_POINT ( 'NONE',  ( -1.364683531250012516, 3.342708333674756727, 0.7879004041258379498 ) ) ;
#51824 = CARTESIAN_POINT ( 'NONE',  ( 0.6963323360776455528, 1.421588922443246084, 1.003805163531448441 ) ) ;
#51825 = CARTESIAN_POINT ( 'NONE',  ( -0.3584499564876342803, 8.158857887134011833, 1.968348077346307790 ) ) ;
#51826 = CARTESIAN_POINT ( 'NONE',  ( 10.56458543818803975, 8.812335408702820061, -5.705356791435097996 ) ) ;
#51827 = CIRCLE ( 'NONE', #44881, 0.08000000000000009881 ) ;
#51828 = CARTESIAN_POINT ( 'NONE',  ( 5.664953204072169513, -1.952404353424816774, -0.9282482345986733385 ) ) ;
#51829 = CARTESIAN_POINT ( 'NONE',  ( -4.959585264500673496, 4.680604318205876524, 1.214306433183764966E-14 ) ) ;
#51830 = CARTESIAN_POINT ( 'NONE',  ( -6.765155463094763455, 8.915767345075790828, 1.443375672974078761 ) ) ;
#51831 = CARTESIAN_POINT ( 'NONE',  ( 4.891577088959510711, 1.599438101461609918, 1.454397306527709155 ) ) ;
#51832 = CARTESIAN_POINT ( 'NONE',  ( 0.6823417656249882723, 2.426041667008084435, -1.181850606188749264 ) ) ;
#51833 = CARTESIAN_POINT ( 'NONE',  ( 6.432890565879505473, 0.1910017811236862373, 1.962057160394870881 ) ) ;
#51834 = CARTESIAN_POINT ( 'NONE',  ( 4.569544190834089470, 1.339882265830975694, -1.100422448201631820 ) ) ;
#51835 = CARTESIAN_POINT ( 'NONE',  ( 1.822082775007987543, 1.258534617508931586, -1.793986466278547853 ) ) ;
#51836 = CARTESIAN_POINT ( 'NONE',  ( 2.731810774274369802, -2.153386645068070759, 0.8298372035008163561 ) ) ;
#51837 = CARTESIAN_POINT ( 'NONE',  ( 5.026665581557772100, 1.970771621317930045, 0.6023086073758465719 ) ) ;
#51838 = CARTESIAN_POINT ( 'NONE',  ( 0.2166051034824221788, -0.09641855276349860226, 1.939669501089319015 ) ) ;
#51839 = CARTESIAN_POINT ( 'NONE',  ( -5.680503174001480637, 9.571078103069643461, 0.7216878364870458196 ) ) ;
#51840 = CARTESIAN_POINT ( 'NONE',  ( -3.817502770699643388, 6.611447778194983194, 1.199719254218452935 ) ) ;
#51841 = FACE_OUTER_BOUND ( 'NONE', #202767, .T. ) ;
#51842 = DIRECTION ( 'NONE',  ( 1.779758311459934189E-16, 0.000000000000000000, -1.000000000000000000 ) ) ;
#51843 = CARTESIAN_POINT ( 'NONE',  ( 1.652970434142877920, 1.038994816082598804, 1.728001345923817267 ) ) ;
#51844 = CARTESIAN_POINT ( 'NONE',  ( -7.334597914868743018, 7.659378443542744996, -0.7216878364870267237 ) ) ;
#51845 = CARTESIAN_POINT ( 'NONE',  ( 3.258999418838660400, -1.672185875938383859, 1.440126295696932068 ) ) ;
#51846 = CARTESIAN_POINT ( 'NONE',  ( -1.642778471874998480, -1.538541666188709245, 2.845375778867863303 ) ) ;
#51847 = CARTESIAN_POINT ( 'NONE',  ( 1.973285428892736171, -0.2338459910692871346, 1.846151439588203935 ) ) ;
#51848 = CARTESIAN_POINT ( 'NONE',  ( 1.056414318722240136E-16, 1.750000000000001554, -1.903066852858540603 ) ) ;
#51849 = CARTESIAN_POINT ( 'NONE',  ( -0.3982008013818653658, -4.205834154663907754, 1.000000000000004663 ) ) ;
#51850 = CARTESIAN_POINT ( 'NONE',  ( -9.554207839743737551, -7.792803924024828355, 0.03436587256740113172 ) ) ;
#51852 = CARTESIAN_POINT ( 'NONE',  ( 6.925078400183582339, 6.034855204486058611, 2.639235227498262670 ) ) ;
#51851 = CARTESIAN_POINT ( 'NONE',  ( -5.114454317065560751, 7.920171510810852133, -1.228010840421199568 ) ) ;
#51853 = CARTESIAN_POINT ( 'NONE',  ( 10.97031310326519282, 12.30000000000000071, -1.695146482106562269 ) ) ;
#51854 = ORIENTED_EDGE ( 'NONE', *, *, #26150, .F. ) ;
#51855 = CARTESIAN_POINT ( 'NONE',  ( 3.502855024581267518, 1.625569291660882598, -1.266701038991333572 ) ) ;
#51856 = CARTESIAN_POINT ( 'NONE',  ( 0.6801582343749796866, 1.723958333674766141, 1.178068619123784355 ) ) ;
#51857 = CARTESIAN_POINT ( 'NONE',  ( -6.566226467720086113, 6.555019055295208119, 1.040834085586084257E-14 ) ) ;
#51858 = CARTESIAN_POINT ( 'NONE',  ( 2.420574729456357765, -0.7750317791199374806, -1.865254733019072297 ) ) ;
#51859 = CARTESIAN_POINT ( 'NONE',  ( 1.499999999999987121, -0.7458333333333122539, 0.8660254037844524744 ) ) ;
#51860 = CARTESIAN_POINT ( 'NONE',  ( 3.009020027229115879, 5.597941567487558778, -1.199719254218446718 ) ) ;
#51861 = CARTESIAN_POINT ( 'NONE',  ( 2.114203836804037007, -0.9703286663178596338, -1.818149309968750016 ) ) ;
#51863 = CARTESIAN_POINT ( 'NONE',  ( 1.364683531249997417, 13.73437500034139980, 2.602085213965210642E-15 ) ) ;
#51862 = CARTESIAN_POINT ( 'NONE',  ( -3.755245360860925086, 6.364574773437617239, -1.082531754730548412 ) ) ;
#51864 = CARTESIAN_POINT ( 'NONE',  ( 4.971035877704902184, 8.951292290631053916, 1.040834085586084257E-14 ) ) ;
#51865 = PRESENTATION_LAYER_ASSIGNMENT (  '', '', ( #58663 ) ) ;
#51866 = CARTESIAN_POINT ( 'NONE',  ( -0.2411972340276282434, 2.878796387150697633, -2.389097370654146513 ) ) ;
#51867 = CARTESIAN_POINT ( 'NONE',  ( 5.162800556355915838, -1.600310254184673431, 1.519886962452212664 ) ) ;
#51868 = CARTESIAN_POINT ( 'NONE',  ( 4.552505719138623341, 8.533283448962240669, 0.7998128361456341429 ) ) ;
#51869 = CARTESIAN_POINT ( 'NONE',  ( 1.194844697948213463, -0.5240009448631496314, -2.097013730318515456 ) ) ;
#51870 = CARTESIAN_POINT ( 'NONE',  ( -3.782361668532609134, 7.356579680022602652, 1.040834085586084257E-14 ) ) ;
#51871 = CARTESIAN_POINT ( 'NONE',  ( 1.692592581891849912, 1.490968054865527304, -1.357870634957742961 ) ) ;
#51872 = CARTESIAN_POINT ( 'NONE',  ( 1.898275044819753621, 0.2256094754716081452, 2.287263704067198145 ) ) ;
#51873 = CARTESIAN_POINT ( 'NONE',  ( -1.040834085586084257E-14, -7.473374494045017968, -9.579665964948867796 ) ) ;
#51874 = LINE ( 'NONE', #83278, #115205 ) ;
#51875 = B_SPLINE_CURVE_WITH_KNOTS ( 'NONE', 3,
 ( #120112, #65916, #151484, #85398, #185015, #33448, #69123, #202324, #201258, #102725, #21436, #132063, #84332, #198074 ),
 .UNSPECIFIED., .F., .F.,
 ( 4, 2, 2, 2, 2, 2, 4 ),
 ( 0.003709280639842194114, 0.003956362438780341648, 0.004203444237718488748, 0.004697607835594784682, 0.004944689634532932650, 0.005191771433471080617, 0.005685935031347376552 ),
 .UNSPECIFIED. ) ;
#51876 = CARTESIAN_POINT ( 'NONE',  ( 1.867826558377215118, 0.9591755677602131769, 1.605880698980370225 ) ) ;
#51877 = CARTESIAN_POINT ( 'NONE',  ( 3.591030000661588062, 1.731995077137841843, 1.032480907900306111 ) ) ;
#51879 = CARTESIAN_POINT ( 'NONE',  ( 11.44779965693276402, 13.49686076798686862, 3.599999932275866676 ) ) ;
#51878 = CARTESIAN_POINT ( 'NONE',  ( 0.6823417656249882723, 2.676041667008084879, -1.181850606188749264 ) ) ;
#51881 = CARTESIAN_POINT ( 'NONE',  ( 4.881522348829672175, 1.965384978258335247, -0.7572991678025364770 ) ) ;
#51880 = CARTESIAN_POINT ( 'NONE',  ( -6.530223543276495235, 10.77034456713125188, -0.7998128361456291469 ) ) ;
#51882 = CARTESIAN_POINT ( 'NONE',  ( 7.820355676984174664, 8.018169799436671852, -0.7998128361456281477 ) ) ;
#51883 = CARTESIAN_POINT ( 'NONE',  ( -5.689618019229208734, 9.789638122409414223, 0.7998128361456481317 ) ) ;
#51884 = CARTESIAN_POINT ( 'NONE',  ( 1.931056844935808314, 3.481093093210268830, -0.4000000000000272227 ) ) ;
#51885 = CARTESIAN_POINT ( 'NONE',  ( 5.379167904621746210, -1.827783419154908273, -0.8597544005511729148 ) ) ;
#51886 = CARTESIAN_POINT ( 'NONE',  ( -1.500000000000001332, -1.318749999317178734, 0.000000000000000000 ) ) ;
#51887 = CARTESIAN_POINT ( 'NONE',  ( 1.059521212928912881, 1.683986000210126788, 1.190688086201870499 ) ) ;
#51888 = CARTESIAN_POINT ( 'NONE',  ( 8.758204044748010730, 9.320252261735261001, 0.7216878364870438212 ) ) ;
#51889 = CARTESIAN_POINT ( 'NONE',  ( 6.866278450678116485, 6.975356045404744521, 0.000000000000000000 ) ) ;
#51890 = CARTESIAN_POINT ( 'NONE',  ( 4.525389411911321602, 8.501647757197021704, -0.7998128361456381397 ) ) ;
#51891 = CARTESIAN_POINT ( 'NONE',  ( 1.364683531249986537, 1.176041667008082658, 0.7879004041258500513 ) ) ;
#51893 = CARTESIAN_POINT ( 'NONE',  ( 6.546325832964379643, 5.229711127717882491, 2.448021111374941938 ) ) ;
#51892 = CARTESIAN_POINT ( 'NONE',  ( 4.692003678781083487, 7.631698837623355658, -1.199719254218450271 ) ) ;
#51894 = CARTESIAN_POINT ( 'NONE',  ( 5.626270559546810546, 8.547437505237857280, 1.082531754730558626 ) ) ;
#51896 = CARTESIAN_POINT ( 'NONE',  ( -5.351242870924207473, 4.712735630379591534, -2.500000000000000444 ) ) ;
#51895 = CARTESIAN_POINT ( 'NONE',  ( 3.525983582677540085, 2.118976886349494659, -0.4726038967238275212 ) ) ;
#51898 = CARTESIAN_POINT ( 'NONE',  ( 2.436835438956724165, -1.365703447793526371, -1.235134912642745775 ) ) ;
#51897 = CARTESIAN_POINT ( 'NONE',  ( -4.989037340148921196, 5.883260320670900434, 1.082531754730560403 ) ) ;
#51899 = EDGE_CURVE ( 'NONE', #76877, #184758, #47934, .T. ) ;
#51900 = CARTESIAN_POINT ( 'NONE',  ( 0.6823417656249899377, 3.176041667008085323, -1.181850606188754593 ) ) ;
#51901 = CARTESIAN_POINT ( 'NONE',  ( 4.001666433686186686, -2.185622478633037602, 0.1623105178310546570 ) ) ;
#51902 = CARTESIAN_POINT ( 'NONE',  ( 8.434540686698982270, 14.01269480687351177, 8.472994457261282975 ) ) ;
#51903 = CARTESIAN_POINT ( 'NONE',  ( 4.944316486460487603, 2.256077187801101669, 0.1715336590100754455 ) ) ;
#51904 = CARTESIAN_POINT ( 'NONE',  ( -5.042743069279040036, 7.970618449879118828, 1.199719254218464037 ) ) ;
#51905 = CARTESIAN_POINT ( 'NONE',  ( 1.364683531249990311, 5.676041667008088432, 0.7879004041258500513 ) ) ;
#51906 = CARTESIAN_POINT ( 'NONE',  ( 5.880365472892705725, 7.167286867907723291, -1.140585135024022811 ) ) ;
#51907 = CARTESIAN_POINT ( 'NONE',  ( -6.590672069574513792, 6.861741300691274859, 0.000000000000000000 ) ) ;
#51908 = CARTESIAN_POINT ( 'NONE',  ( 4.041739190649647817, 6.769093918182960579, -1.082531754730548412 ) ) ;
#51909 = CARTESIAN_POINT ( 'NONE',  ( 6.380137019068807369, -0.9445444496645590826, 1.496399839161892897 ) ) ;
#51910 = CARTESIAN_POINT ( 'NONE',  ( 3.897138702661524956, -0.1997049427340416294, -2.003176435020975088 ) ) ;
#51911 = CARTESIAN_POINT ( 'NONE',  ( 6.123478934866503742, 10.29580919065294431, 0.7998128361456462443 ) ) ;
#51912 = CARTESIAN_POINT ( 'NONE',  ( 3.399542317941701253, 1.658995184361473196, 1.297097526815289115 ) ) ;
#51913 = CARTESIAN_POINT ( 'NONE',  ( 0.6322731411384452382, 0.5572298914768618605, 1.832739050869176101 ) ) ;
#51915 = CARTESIAN_POINT ( 'NONE',  ( -1.201851678989727383E-14, 2.962500000000025224, 1.732050807568877637 ) ) ;
#51914 = CARTESIAN_POINT ( 'NONE',  ( -1.364683531250014514, 12.33854166700806054, -0.7879004041258335089 ) ) ;
#51916 = CARTESIAN_POINT ( 'NONE',  ( 2.119528921591812498, 0.3396393280722594388, -1.939881811770089115 ) ) ;
#51917 = CARTESIAN_POINT ( 'NONE',  ( 4.939715878566554252, -1.916525930768823383, 0.6376727893300809802 ) ) ;
#51918 = CARTESIAN_POINT ( 'NONE',  ( 0.8658264364783776479, 0.9185255527898968930, 1.629538061279064642 ) ) ;
#51919 = CARTESIAN_POINT ( 'NONE',  ( 1.346068015636435522, -0.8851805579040676886, 1.750911360861057142 ) ) ;
#51921 = ORIENTED_EDGE ( 'NONE', *, *, #19236, .T. ) ;
#51920 = CARTESIAN_POINT ( 'NONE',  ( 0.7031954830387620037, 1.685401770928725007, -0.9037484838233383888 ) ) ;
#51922 = CARTESIAN_POINT ( 'NONE',  ( 5.151735183512854199, 8.954182114166247430, -0.7216878364870257245 ) ) ;
#51923 = CARTESIAN_POINT ( 'NONE',  ( -1.364683531250014514, 0.3010416670080866552, -0.7879004041258359514 ) ) ;
#51924 = CARTESIAN_POINT ( 'NONE',  ( 5.401189721097995111, 1.529905263132097071, 1.076157610686766075 ) ) ;
#51925 = CARTESIAN_POINT ( 'NONE',  ( -0.6992639221309246977, 2.800524997876915112, 1.172080594574814727 ) ) ;
#51926 = CARTESIAN_POINT ( 'NONE',  ( 5.225469540725330653, 0.2083811790645866135, -2.059773418507819365 ) ) ;
#51927 = FACE_OUTER_BOUND ( 'NONE', #34372, .T. ) ;
#51928 = EDGE_CURVE ( 'NONE', #192349, #142998, #194128, .T. ) ;
#51929 = CARTESIAN_POINT ( 'NONE',  ( -4.217995187182965289, 6.014356699837137832, 1.443375672974065660 ) ) ;
#51930 = FILL_AREA_STYLE_COLOUR ( '', #74666 ) ;
#51931 = CARTESIAN_POINT ( 'NONE',  ( -0.7500000000000006661, 0.3583333333333563187, -1.299038105676652011 ) ) ;
#51932 = CARTESIAN_POINT ( 'NONE',  ( 6.753933077901968396, 11.03133902419432566, 0.7998128361456462443 ) ) ;
#51933 = CARTESIAN_POINT ( 'NONE',  ( -7.828943636887387925, 11.22118577875556156, 1.199719254218453823 ) ) ;
#51934 = CARTESIAN_POINT ( 'NONE',  ( 5.332099551924443404, 9.442809587212341427, 0.000000000000000000 ) ) ;
#51935 = CARTESIAN_POINT ( 'NONE',  ( 0.6823417656249899377, 1.092708333674752286, 1.181850606188755259 ) ) ;
#51936 = CARTESIAN_POINT ( 'NONE',  ( -1.500000000000011324, 3.170833333333354265, 0.8660254037844403729 ) ) ;
#51938 = CARTESIAN_POINT ( 'NONE',  ( 3.486418057008484617, 7.219238166485217434, 1.040834085586084257E-14 ) ) ;
#51937 = CARTESIAN_POINT ( 'NONE',  ( 5.582460749670235423, 1.169929261559121247, -1.574690175210855747 ) ) ;
#51939 = CARTESIAN_POINT ( 'NONE',  ( 2.671249783466634220, -0.7690017779844946499, -1.863883771055181660 ) ) ;
#51940 = CARTESIAN_POINT ( 'NONE',  ( 1.973720722908858249, -0.8152147109428582450, 1.733722481544483163 ) ) ;
#51941 = CARTESIAN_POINT ( 'NONE',  ( -1.914442667406943910, 3.262253226108043247, -0.4355078757044400506 ) ) ;
#51942 = CARTESIAN_POINT ( 'NONE',  ( -0.1232117409455633916, -0.1621322592461546530, -2.156395338765437764 ) ) ;
#51943 =( BOUNDED_CURVE ( )  B_SPLINE_CURVE ( 2, ( #177549, #12883, #208947 ),
 .UNSPECIFIED., .F., .T. ) 
 B_SPLINE_CURVE_WITH_KNOTS ( ( 3, 3 ),
 ( 0.000000000000000000, 0.005706871658383422079 ),
 .UNSPECIFIED. ) 
 CURVE ( )  GEOMETRIC_REPRESENTATION_ITEM ( )  RATIONAL_B_SPLINE_CURVE ( ( 1.000000000000000000, 0.9082509008696860731, 0.9421658817815319331 ) ) 
 REPRESENTATION_ITEM ( '' )  );
#51944 = CARTESIAN_POINT ( 'NONE',  ( 0.5773502691896124084, -4.295408888568413630, -0.9999999999999991118 ) ) ;
#51945 = CARTESIAN_POINT ( 'NONE',  ( 3.602682612693074660, 1.476495159181415939, -1.148357684351591912 ) ) ;
#51946 = CARTESIAN_POINT ( 'NONE',  ( -1.500000000000015099, -0.5895833326505155458, -0.8660254037844383745 ) ) ;
#51947 = APPLICATION_CONTEXT ( 'automotive_design' ) ;
#51948 = CARTESIAN_POINT ( 'NONE',  ( -8.518600588087975822, 8.832788862391110385, 1.040834085586084257E-14 ) ) ;
#51950 = CARTESIAN_POINT ( 'NONE',  ( 3.989952538763715140, -2.111419002029162328, 0.1578513319024783257 ) ) ;
#51949 = CARTESIAN_POINT ( 'NONE',  ( -3.145128448690310830, 6.613140923539910787, -0.7216878364870267237 ) ) ;
#51951 = CARTESIAN_POINT ( 'NONE',  ( 1.249999999999820588, 10.00000000000000178, -4.154462424328206893 ) ) ;
#51952 = CARTESIAN_POINT ( 'NONE',  ( 5.547352688424546763, 1.827615396715172258, -0.9727077141251788683 ) ) ;
#51954 = CARTESIAN_POINT ( 'NONE',  ( 6.620655732516655512, 0.5568428858156619921, 2.325336003765938742 ) ) ;
#51953 = CARTESIAN_POINT ( 'NONE',  ( 2.806283438348840420, 1.512464495701435929, -1.443730951476623670 ) ) ;
#51956 = ORIENTED_EDGE ( 'NONE', *, *, #181210, .F. ) ;
#51955 = CARTESIAN_POINT ( 'NONE',  ( 0.5336903687956630060, 0.8928529924820073349, -1.475541649381803433 ) ) ;
#51957 = CARTESIAN_POINT ( 'NONE',  ( 5.262536180398716290, 9.291375977107183104, -0.7998128361456291469 ) ) ;
#51958 = DIRECTION ( 'NONE',  ( 0.5773487058764860125, 0.002327115863041261980, 0.8164943700690817652 ) ) ;
#51959 = CARTESIAN_POINT ( 'NONE',  ( 0.000000000000000000, 1000.000000000000000, 0.000000000000000000 ) ) ;
#51960 = CARTESIAN_POINT ( 'NONE',  ( -2.449742653233033085, 3.949999999999988187, 0.4499999999999608757 ) ) ;
#51961 = CARTESIAN_POINT ( 'NONE',  ( 6.765155463094751909, 8.915767345075790828, 1.443375672974076540 ) ) ;
#51962 = CARTESIAN_POINT ( 'NONE',  ( -0.5368768833858145184, 13.37576698399828246, -1.254641125003840507 ) ) ;
#51964 = CARTESIAN_POINT ( 'NONE',  ( 0.5920784091685951100, -1.007499442088593211, 1.505216462368397234 ) ) ;
#51963 = CARTESIAN_POINT ( 'NONE',  ( 5.885121196783658526, 9.023669275293071834, 1.199719254218452047 ) ) ;
#51965 = CARTESIAN_POINT ( 'NONE',  ( -6.723954117373590833, 9.932031339322813679, -1.199719254218440723 ) ) ;
#51966 = CARTESIAN_POINT ( 'NONE',  ( 4.168242161197552420, 6.950367390450747251, -1.199719254218452047 ) ) ;
#51967 = CARTESIAN_POINT ( 'NONE',  ( -5.214720930002679999, 7.727253977155453590, 1.197825571464938399 ) ) ;
#51968 = CARTESIAN_POINT ( 'NONE',  ( 5.826972158823246595, 10.02016096192762085, -0.7998128361456481317 ) ) ;
#51969 = CARTESIAN_POINT ( 'NONE',  ( -9.495347311156809411, -6.857257212219918685, 3.422217897015904270E-15 ) ) ;
#51970 = CARTESIAN_POINT ( 'NONE',  ( 3.995022045461748217, 7.603044914155053569, 0.06581304817247432548 ) ) ;
#51971 = CARTESIAN_POINT ( 'NONE',  ( 9.924205255523292024, 10.68058700763975466, -0.7216878364870257245 ) ) ;
#51972 = ORIENTED_EDGE ( 'NONE', *, *, #66641, .F. ) ;
#51973 = CARTESIAN_POINT ( 'NONE',  ( 6.556263154800559434, -1.238474754573845038, 1.591913907798309991 ) ) ;
#51974 = CARTESIAN_POINT ( 'NONE',  ( 0.6277789859737945566, -0.3070864893036719945, 2.098006834332386994 ) ) ;
#51975 =( NAMED_UNIT ( * ) PLANE_ANGLE_UNIT ( ) SI_UNIT ( $, .RADIAN. ) );
#51976 = CARTESIAN_POINT ( 'NONE',  ( 2.275020158240702361, 5.648663482265439129, 0.5226904017501784461 ) ) ;
#51977 = FACE_BOUND ( 'NONE', #44743, .T. ) ;
#51978 = CARTESIAN_POINT ( 'NONE',  ( -5.450014563013544588, 5.460697866378308341, 0.7216878364870317197 ) ) ;
#51979 = CARTESIAN_POINT ( 'NONE',  ( 8.541273586929342798, 11.94827437051752206, -1.082531754730543083 ) ) ;
#51980 = CARTESIAN_POINT ( 'NONE',  ( 3.397268178914572889, -1.739110600408208196, 0.9241587964883835049 ) ) ;
#51981 = CARTESIAN_POINT ( 'NONE',  ( 1.928540351845555056, -1.002238520345886785, -1.868699319572619366 ) ) ;
#51982 = CARTESIAN_POINT ( 'NONE',  ( -6.501298352952815662, 7.543601818988450169, -1.199719254218446718 ) ) ;
#51983 = CARTESIAN_POINT ( 'NONE',  ( -10.49167311136684511, 5.343773310534622567, 5.730690286876297002 ) ) ;
#51984 = CARTESIAN_POINT ( 'NONE',  ( 6.883263157960374912, 7.629137130509066722, 2.546189081643289942 ) ) ;
#51985 = CARTESIAN_POINT ( 'NONE',  ( 5.876942531769460132, 2.026063101133714461, -0.8356547683932225024 ) ) ;
#51986 = CARTESIAN_POINT ( 'NONE',  ( -1.500000000000035971, 7.750000000000000000, -9.886859966642584041 ) ) ;
#51987 = CARTESIAN_POINT ( 'NONE',  ( 4.383760159432283032, 1.257691660000469058, 1.459273733648867699 ) ) ;
#51988 = CARTESIAN_POINT ( 'NONE',  ( -7.320512876374914768, 10.62801655815766999, 1.199719254218453823 ) ) ;
#51989 = CARTESIAN_POINT ( 'NONE',  ( -0.02968770228137588424, 5.725071598255107475, -2.420367217772397606 ) ) ;
#51990 = CARTESIAN_POINT ( 'NONE',  ( 1.067327838873022516, -1.996528553209110379, -0.9406146916221403975 ) ) ;
#51991 = FACE_OUTER_BOUND ( 'NONE', #26970, .T. ) ;
#51992 = ORIENTED_EDGE ( 'NONE', *, *, #119054, .F. ) ;
#51993 = CARTESIAN_POINT ( 'NONE',  ( 6.104353324094977218, 1.967046249225043342, 0.1001853051637753428 ) ) ;
#51994 = CARTESIAN_POINT ( 'NONE',  ( 0.7494335824394976475, 1.939781244166354002, -0.09678450214786055161 ) ) ;
#51995 = CARTESIAN_POINT ( 'NONE',  ( 6.134147193249257946, 0.1786779444946043904, -2.291516319396588397 ) ) ;
#51997 = CARTESIAN_POINT ( 'NONE',  ( 4.733164070488131259, 0.002922519798398153738, -1.861131630917359336 ) ) ;
#51996 = CARTESIAN_POINT ( 'NONE',  ( -7.130662446144611977, 7.283804040115648526, 0.000000000000000000 ) ) ;
#51998 = CARTESIAN_POINT ( 'NONE',  ( 5.525830126021535449, 8.604496359403894346, -1.199719254218452047 ) ) ;
#51999 = DIRECTION ( 'NONE',  ( -0.000000000000000000, -1.000000000000000000, -0.000000000000000000 ) ) ;
#52000 = PLANE ( 'NONE',  #143976 ) ;
#52001 = CARTESIAN_POINT ( 'NONE',  ( -5.045605722580076780, 9.038290442985410067, -0.7998128361456231517 ) ) ;
#52002 = CARTESIAN_POINT ( 'NONE',  ( -3.384026120672947613, -0.9549381201899959093, 0.2424983683859719685 ) ) ;
#52003 = CARTESIAN_POINT ( 'NONE',  ( 0.06437606466144081552, -1.426665095847098330, 1.663708609037084951 ) ) ;
#52004 = CARTESIAN_POINT ( 'NONE',  ( 3.524756749872944628, 7.056040608253000279, -0.7216878364870267237 ) ) ;
#52005 = VERTEX_POINT ( 'NONE', #98793 ) ;
#52006 = CARTESIAN_POINT ( 'NONE',  ( 0.2999999999999869993, 3.999999999999974243, -0.9782388782689304119 ) ) ;
#52007 = CARTESIAN_POINT ( 'NONE',  ( 3.834746474454188013E-15, 10.56250000000000178, 1.500000000000001554 ) ) ;
#52008 = CARTESIAN_POINT ( 'NONE',  ( 1.066719475142905216, -1.649486405746130258, -0.7827983987617056494 ) ) ;
#52009 = CARTESIAN_POINT ( 'NONE',  ( -5.057354993097396445, 5.859001232490445688, -1.199719254218446718 ) ) ;
#52010 = CARTESIAN_POINT ( 'NONE',  ( 2.021687164805381354, -1.548805232022354650, 0.7802212711869142003 ) ) ;
#52011 = PRESENTATION_STYLE_ASSIGNMENT (( #68227 ) ) ;
#52012 = DIRECTION ( 'NONE',  ( 0.000000000000000000, -1.000000000000000000, 0.000000000000000000 ) ) ;
#52013 = CARTESIAN_POINT ( 'NONE',  ( 0.4465194593917843902, 3.080450244942134486, 0.4155024747329351120 ) ) ;
#52014 = CARTESIAN_POINT ( 'NONE',  ( 6.498675964634617941, -0.4922777150685350156, -1.758009983081544991 ) ) ;
#52015 = CARTESIAN_POINT ( 'NONE',  ( 3.414850490325722632, -1.488543670003230845, 1.277929504599809585 ) ) ;
#52016 = CARTESIAN_POINT ( 'NONE',  ( -1.225000000000047162, -0.1874999993171852508, -2.775557561562891351E-14 ) ) ;
#52017 = CARTESIAN_POINT ( 'NONE',  ( -8.910733272679575379, 11.41894145625809820, -1.599625672291263179 ) ) ;
#52018 = CARTESIAN_POINT ( 'NONE',  ( 6.257251587906815793, 7.258880593101466161, 1.199719254218462483 ) ) ;
#52019 = EDGE_CURVE ( 'NONE', #155820, #97415, #101278, .T. ) ;
#52020 = CARTESIAN_POINT ( 'NONE',  ( 5.074906250706387567, -1.535530725987072298, 1.462626433913247093 ) ) ;
#52021 = CARTESIAN_POINT ( 'NONE',  ( 6.831329296439236032, 9.063246493969506545, -1.599625672291267398 ) ) ;
#52022 = CARTESIAN_POINT ( 'NONE',  ( -8.462260433223891098, 13.02438760540324481, -0.7998128361456281477 ) ) ;
#52023 = CARTESIAN_POINT ( 'NONE',  ( 2.905202624773518316, -1.723727875341171778, 1.146311801414557241 ) ) ;
#52025 = CARTESIAN_POINT ( 'NONE',  ( -0.6823417656250003738, 0.5302083336747518416, -1.181850606188749264 ) ) ;
#52024 = FACE_OUTER_BOUND ( 'NONE', #124803, .T. ) ;
#52027 = ORIENTED_EDGE ( 'NONE', *, *, #10396, .T. ) ;
#52026 = CARTESIAN_POINT ( 'NONE',  ( 5.074942145771424329, -1.609735135204511280, 1.530878986171863687 ) ) ;
#52028 = CARTESIAN_POINT ( 'NONE',  ( 2.743178873131403961, 2.287300171779807378, -0.2288005476599272447 ) ) ;
#52029 = CARTESIAN_POINT ( 'NONE',  ( 6.968527767744088663, 11.07377346243604599, 0.7216878364870438212 ) ) ;
#52031 = CARTESIAN_POINT ( 'NONE',  ( 0.000000000000000000, -1.596874999522041705, -3.793834371823813001 ) ) ;
#52030 = CARTESIAN_POINT ( 'NONE',  ( 2.891631901464575272, 6.595597328342462262, 0.000000000000000000 ) ) ;
#52032 = VERTEX_POINT ( 'NONE', #183221 ) ;
#52034 = EDGE_CURVE ( 'NONE', #74902, #127875, #204886, .T. ) ;
#52033 = CARTESIAN_POINT ( 'NONE',  ( -5.462143695033999435, 6.282726080954706305, -1.018839928044611653 ) ) ;
#52035 = CARTESIAN_POINT ( 'NONE',  ( 3.920094060441734030, -1.906919942518231936, 0.1457910263855527466 ) ) ;
#52036 = DIRECTION ( 'NONE',  ( 0.000000000000000000, 0.000000000000000000, 1.000000000000000000 ) ) ;
#52037 = CARTESIAN_POINT ( 'NONE',  ( 4.137519252912919221, -1.190027120290118257, -1.248710780074323567 ) ) ;
#52038 = CARTESIAN_POINT ( 'NONE',  ( 3.573454097414618946, 1.463926983822515293, 1.387100322000796027 ) ) ;
#52039 = CARTESIAN_POINT ( 'NONE',  ( 4.518391418568163509, -2.101855750862766659, 0.9310765106353561249 ) ) ;
#52040 = CARTESIAN_POINT ( 'NONE',  ( 0.3282377607281163345, 1.136164550367434467, 1.224999999999968114 ) ) ;
#52041 = CARTESIAN_POINT ( 'NONE',  ( 6.270163029207718175, 1.081028068854476665, 1.807315287263556280 ) ) ;
#52042 = CARTESIAN_POINT ( 'NONE',  ( -6.644904684473536882, 6.925012684740138980, 0.7216878364870317197 ) ) ;
#52043 = ORIENTED_EDGE ( 'NONE', *, *, #43445, .T. ) ;
#52044 = CARTESIAN_POINT ( 'NONE',  ( 4.903428802837151324, -0.4723676116331463892, 1.705421244663980263 ) ) ;
#52046 = CARTESIAN_POINT ( 'NONE',  ( 2.273717984289443717, 1.411852697042052185, 1.805783550510152935 ) ) ;
#52045 = CARTESIAN_POINT ( 'NONE',  ( 5.468734858265785093, 7.473552982767158070, 1.599625672291269396 ) ) ;
#52047 = CARTESIAN_POINT ( 'NONE',  ( 0.2513753182956691146, 0.6612109069651134208, 1.610038921780505339 ) ) ;
#52048 = CARTESIAN_POINT ( 'NONE',  ( -5.759181390754928742, 9.941071732514568993, 0.000000000000000000 ) ) ;
#52049 = CARTESIAN_POINT ( 'NONE',  ( -4.787964524281469458, 5.614988695530339413, -1.199719254218453823 ) ) ;
#52050 = CARTESIAN_POINT ( 'NONE',  ( -3.956095110007852622E-14, -0.1406249996585586248, -1.570758158831808249 ) ) ;
#52051 = DIRECTION ( 'NONE',  ( 0.000000000000000000, 0.000000000000000000, 1.000000000000000000 ) ) ;
#52052 = CARTESIAN_POINT ( 'NONE',  ( 0.5554291532160166023, 1.804893407318912901, -1.206520995182088329 ) ) ;
#52053 = CARTESIAN_POINT ( 'NONE',  ( 1.551970632248239612, 1.040795554343958429, 1.727062486439542965 ) ) ;
#52054 = CARTESIAN_POINT ( 'NONE',  ( 0.7499999999999867883, -0.4020833326505157679, -1.299038105676652899 ) ) ;
#52055 = CARTESIAN_POINT ( 'NONE',  ( 4.986905038743431717, -0.2377927182869009337, -1.911709049817163164 ) ) ;
#52056 = CARTESIAN_POINT ( 'NONE',  ( -1.364683531250010295, 11.63020833367472839, 0.7879004041258445001 ) ) ;
#52057 = CARTESIAN_POINT ( 'NONE',  ( 2.145073868429191677, 2.156049884074415779, 0.5345358195362903686 ) ) ;
#52058 = ORIENTED_EDGE ( 'NONE', *, *, #149015, .F. ) ;
#52060 = CARTESIAN_POINT ( 'NONE',  ( 0.006158830626129541130, 7.078243236992583398, -2.121324627965408993 ) ) ;
#52059 = DIRECTION ( 'NONE',  ( -0.6507913734559640506, -0.7592566023653003482, 0.000000000000000000 ) ) ;
#52061 = DIRECTION ( 'NONE',  ( 0.000000000000000000, 0.000000000000000000, 1.000000000000000000 ) ) ;
#52063 = EDGE_CURVE ( 'NONE', #108531, #194102, #106329, .T. ) ;
#52062 = CARTESIAN_POINT ( 'NONE',  ( 10.37606763316019531, 10.99983374830873650, 0.7998128361456462443 ) ) ;
#52064 = FACE_OUTER_BOUND ( 'NONE', #51436, .T. ) ;
#52065 = SPHERICAL_SURFACE ( 'NONE', #80287, 0.08000000000000000167 ) ;
#52066 = CARTESIAN_POINT ( 'NONE',  ( 3.860698480431251411, 0.2083224649859614919, -1.727840645513075923 ) ) ;
#52067 = CARTESIAN_POINT ( 'NONE',  ( 2.137090596337941406, -0.09316805448006217072, -1.959763546484971197 ) ) ;
#52069 = CARTESIAN_POINT ( 'NONE',  ( 1.364683531249988535, 2.426041667008088432, 0.7879004041258500513 ) ) ;
#52068 = CARTESIAN_POINT ( 'NONE',  ( 3.714044015139744914, 6.420469553383295391, 1.199719254218462483 ) ) ;
#52070 = CARTESIAN_POINT ( 'NONE',  ( 4.369805582306193870, 3.992528022312320957, 1.214306433183764966E-14 ) ) ;
#52071 = CARTESIAN_POINT ( 'NONE',  ( 1.047418773927465629, 1.819938098697634343, -0.9707658663142370026 ) ) ;
#52072 = CARTESIAN_POINT ( 'NONE',  ( -7.857113714319432063, 9.125386407249497012, 1.199719254218462483 ) ) ;
#52073 = CARTESIAN_POINT ( 'NONE',  ( -5.111060722227552588, 6.025620933095978238, 1.082531754730546636 ) ) ;
#52074 = CARTESIAN_POINT ( 'NONE',  ( 1.675094374204841419, -2.148779999652763895, -0.7084808733194192243 ) ) ;
#52075 = VERTEX_POINT ( 'NONE', #7077 ) ;
#52077 = ADVANCED_FACE ( 'NONE', ( #8166 ), #154432, .T. ) ;
#52076 = CARTESIAN_POINT ( 'NONE',  ( -1.500000000000013101, -0.2979166659838501929, 0.8660254037844403729 ) ) ;
#52078 = CARTESIAN_POINT ( 'NONE',  ( 2.811613793402362393, -1.850737340378521223, 0.2705540153197931730 ) ) ;
#52079 = CARTESIAN_POINT ( 'NONE',  ( 1.160356219728400307, 1.032376606561947741, 1.393149478428891364 ) ) ;
#52080 = CARTESIAN_POINT ( 'NONE',  ( 4.898067072109578035, -0.7382639882421681010, -2.063579870930781546 ) ) ;
#52081 = CARTESIAN_POINT ( 'NONE',  ( 5.192513718098597408, -2.289403112372697890, -0.2887273360754892826 ) ) ;
#52082 = CARTESIAN_POINT ( 'NONE',  ( 1.393510596882661989, 1.559873972335079184, 1.346953478171313057 ) ) ;
#52083 = CARTESIAN_POINT ( 'NONE',  ( 3.767467431601259076, 1.079656630588815780, 1.613968600252370322 ) ) ;
#52084 = CARTESIAN_POINT ( 'NONE',  ( -4.894130264408873110, 5.772535398974209642, -1.082531754730543971 ) ) ;
#52085 = CARTESIAN_POINT ( 'NONE',  ( 5.923093557443567470, -0.04637014295935314168, 1.870147476527424635 ) ) ;
#52086 = CARTESIAN_POINT ( 'NONE',  ( 1.344440581753393538, 13.33325798258003481, -0.4256415601542729021 ) ) ;
#52087 = CARTESIAN_POINT ( 'NONE',  ( 0.4207071466195873022, 0.6554624660736629860, 1.605403739708724631 ) ) ;
#52088 = CARTESIAN_POINT ( 'NONE',  ( 5.560252395380222090, 5.659585014131299552, 0.7216878364870328300 ) ) ;
#52089 = CARTESIAN_POINT ( 'NONE',  ( -1.953008978358306879E-14, 0.7031250003414775129, 1.570758158831782048 ) ) ;
#52090 = CARTESIAN_POINT ( 'NONE',  ( 4.957657809308734898, -1.899617967926207740, -0.6767155953601932117 ) ) ;
#52091 = CARTESIAN_POINT ( 'NONE',  ( -3.050221372950322252, 5.542046787541873520, 1.082531754730560403 ) ) ;
#52092 = CARTESIAN_POINT ( 'NONE',  ( 8.503988664269582998, 10.94440607977979063, 1.599625672291281386 ) ) ;
#52093 = CARTESIAN_POINT ( 'NONE',  ( 3.770049233051776749, 6.556085317605844232, 1.199719254218451159 ) ) ;
#52095 = CARTESIAN_POINT ( 'NONE',  ( -1.203941962966186052, 3.133481847795091646, 0.7750000000000083489 ) ) ;
#52094 = CARTESIAN_POINT ( 'NONE',  ( 2.508196354075361789, -0.6984789837382252564, -1.686990664346368796 ) ) ;
#52096 = CARTESIAN_POINT ( 'NONE',  ( -5.635349125135588721, 6.603604063193491136, 1.199719254218452935 ) ) ;
#52097 = CARTESIAN_POINT ( 'NONE',  ( 11.37385970535889257, 1.000000000000000888, -3.825613075418463627 ) ) ;
#52098 = CARTESIAN_POINT ( 'NONE',  ( -0.3282377607281426468, 1.863835450998160281, 1.224999999999969003 ) ) ;
#52099 = VERTEX_POINT ( 'NONE', #53725 ) ;
#52100 = CARTESIAN_POINT ( 'NONE',  ( -6.739811759324840779, 7.035737605399991601, -0.7216878364870338292 ) ) ;
#52101 = CARTESIAN_POINT ( 'NONE',  ( -1.423205080756851260, 7.980384757729337863, 10.65537363484302524 ) ) ;
#52102 = CARTESIAN_POINT ( 'NONE',  ( -9.494787648271923786, 9.971673765939062406, 1.040834085586084257E-14 ) ) ;
#52103 = CARTESIAN_POINT ( 'NONE',  ( 5.654946514622759324, 0.3960909877551482827, 1.980269227310478275 ) ) ;
#52105 = ORIENTED_EDGE ( 'NONE', *, *, #199264, .T. ) ;
#52104 = CARTESIAN_POINT ( 'NONE',  ( 6.639320575229294086, -0.003630812595115453199, 2.203388474976493594 ) ) ;
#52106 = CARTESIAN_POINT ( 'NONE',  ( -6.947627372360122955, 7.070263120700404968, 0.000000000000000000 ) ) ;
#52107 = CARTESIAN_POINT ( 'NONE',  ( 6.328958779480917229, 6.278206752349526631, 0.7998128361456341429 ) ) ;
#52108 = STYLED_ITEM ( 'NONE', ( #179339 ), #169204 ) ;
#52110 = CARTESIAN_POINT ( 'NONE',  ( 4.786040499707863383, -0.9732044846940243188, 1.816634495032407814 ) ) ;
#52109 = PRODUCT_DEFINITION ( 'UNKNOWN', '', #79968, #182500 ) ;
#52111 = CARTESIAN_POINT ( 'NONE',  ( 5.660779783930850684, 1.203351582566011047, 1.617819807990819481 ) ) ;
#52112 = EDGE_LOOP ( 'NONE', ( #92291, #84604, #21276, #87130, #78659 ) ) ;
#52113 = ORIENTED_EDGE ( 'NONE', *, *, #78852, .F. ) ;
#52114 = DIRECTION ( 'NONE',  ( 0.000000000000000000, 0.000000000000000000, 1.000000000000000000 ) ) ;
#52115 = CARTESIAN_POINT ( 'NONE',  ( 3.029357257649615054, 5.621668336311468117, -1.199719254218446718 ) ) ;
#52117 = EDGE_LOOP ( 'NONE', ( #164459, #73595, #35737, #193383 ) ) ;
#52116 = CARTESIAN_POINT ( 'NONE',  ( -5.794130544993808307, 7.853181283949808744, 1.599625672291263179 ) ) ;
#52118 = CARTESIAN_POINT ( 'NONE',  ( 4.595652554671352696, 8.489339133230261680, -0.03962354257190832396 ) ) ;
#52119 = CARTESIAN_POINT ( 'NONE',  ( 4.604842190751081255, 0.8645911521153251122, -1.821463593394745395 ) ) ;
#52120 = CARTESIAN_POINT ( 'NONE',  ( 3.995923475689294513, -0.5793754966058572986, -1.747668199984537152 ) ) ;
#52121 = CARTESIAN_POINT ( 'NONE',  ( -0.02319159430947368913, 6.948789054712430691, -2.406029888528108618 ) ) ;
#52122 = CARTESIAN_POINT ( 'NONE',  ( 1.805729983942544026, 1.920404770136320716, 1.279379207282659969 ) ) ;
#52123 = CARTESIAN_POINT ( 'NONE',  ( 7.367930134383754215, 7.560616343061329125, -0.7998128361456341429 ) ) ;
#52124 = CARTESIAN_POINT ( 'NONE',  ( 5.325516461952285674, -2.054413220456321909, 0.6725034809518318779 ) ) ;
#52125 = CARTESIAN_POINT ( 'NONE',  ( 7.235247531187115833, 11.59287255302699648, -0.7998128361456291469 ) ) ;
#52126 = CARTESIAN_POINT ( 'NONE',  ( 0.4505971019186795212, -1.641227270844529018, -1.037965677199135017 ) ) ;
#52127 = CARTESIAN_POINT ( 'NONE',  ( -5.412729640353771465, 7.337937218544611895, 1.599625672291269396 ) ) ;
#52128 = CIRCLE ( 'NONE', #104081, 0.1000000000000000472 ) ;
#52129 = CARTESIAN_POINT ( 'NONE',  ( 2.666414593264813337, 0.4259009368094319181, -0.1247943508829645470 ) ) ;
#52130 = CARTESIAN_POINT ( 'NONE',  ( -6.168033539574333979, 6.160736982450306876, 0.7998128361456281477 ) ) ;
#52131 = CARTESIAN_POINT ( 'NONE',  ( 3.854256360616271415, 0.6726810918341770140, 1.745705178215435582 ) ) ;
#52133 = CARTESIAN_POINT ( 'NONE',  ( -5.692444392891315097, 7.734547439830227411, -1.599625672291271394 ) ) ;
#52132 = CARTESIAN_POINT ( 'NONE',  ( -1.201851678989727383E-14, 5.446875000341422357, -1.575800808251660134 ) ) ;
#52134 = CARTESIAN_POINT ( 'NONE',  ( 1.295869073816724226, 1.673045085319382119, 1.439284050222865652 ) ) ;
#52135 = CARTESIAN_POINT ( 'NONE',  ( 9.586610838029415049, -7.161464053357574855, -0.003376046620562692113 ) ) ;
#52136 = CARTESIAN_POINT ( 'NONE',  ( 3.897079088924235712, 6.634010472798538949, 1.199719254218462483 ) ) ;
#52137 = CARTESIAN_POINT ( 'NONE',  ( -5.298539104842322267, 5.076050465271134016, 0.7998128361456341429 ) ) ;
#52138 = CARTESIAN_POINT ( 'NONE',  ( -7.553300976144787349, 8.945177572657957654, -1.082531754730549967 ) ) ;
#52139 = CARTESIAN_POINT ( 'NONE',  ( 0.2277241186354854174, -1.209499947282626220, -1.557479245376863330 ) ) ;
#52140 = CARTESIAN_POINT ( 'NONE',  ( 6.340458270854060885, 2.281561288062480486, 0.3456012654466412704 ) ) ;
#52141 = CARTESIAN_POINT ( 'NONE',  ( 1.047228354049560828, 1.731870006261830630, -0.9216698261682305660 ) ) ;
#52142 = CARTESIAN_POINT ( 'NONE',  ( 4.100476343641854093, 2.052162271747024924, 0.2072667206600986300 ) ) ;
#52143 = CARTESIAN_POINT ( 'NONE',  ( 5.910991785878156435, 7.919243054989755670, -1.443375672974057666 ) ) ;
#52144 = CARTESIAN_POINT ( 'NONE',  ( 4.844006021832467646, 8.873367135438366304, 0.000000000000000000 ) ) ;
#52145 = ORIENTED_EDGE ( 'NONE', *, *, #156739, .F. ) ;
#52146 = CARTESIAN_POINT ( 'NONE',  ( 8.066738210006679566, 10.43428054980638997, 1.443375672974076540 ) ) ;
#52147 = CARTESIAN_POINT ( 'NONE',  ( -1.201851678989727383E-14, 5.009375000341421469, -1.575800808251660134 ) ) ;
#52148 = DIRECTION ( 'NONE',  ( 2.220446049250312341E-16, -1.000000000000000000, 0.000000000000000000 ) ) ;
#52149 = CARTESIAN_POINT ( 'NONE',  ( 5.002595493318194642, 4.938708951733754127, -0.7216878364870197293 ) ) ;
#52150 = CARTESIAN_POINT ( 'NONE',  ( 6.566846207931698487, 1.613421326539933531, -1.453093050198107861 ) ) ;
#52152 = CARTESIAN_POINT ( 'NONE',  ( 6.128435733830499998, 0.1874100934057248424, 1.831705376836203936 ) ) ;
#52151 = CARTESIAN_POINT ( 'NONE',  ( 0.000000000000000000, 9.719999999999998863, 0.000000000000000000 ) ) ;
#52153 = EDGE_CURVE ( 'NONE', #195274, #191668, #139215, .T. ) ;
#52154 = CARTESIAN_POINT ( 'NONE',  ( -4.758575512226618009, 6.703445193574907535, 1.360375859659995523 ) ) ;
#52155 = CARTESIAN_POINT ( 'NONE',  ( -4.370663978927099791, 5.060324124126027279, 7.500000000000000000 ) ) ;
#52156 = CARTESIAN_POINT ( 'NONE',  ( 0.9131076777311696313, -0.2804849920042574718, 1.849292663789033009 ) ) ;
#52157 = CARTESIAN_POINT ( 'NONE',  ( -5.829309506874599478, 6.192769411583809003, 0.9639237645304669089 ) ) ;
#52158 = FACE_OUTER_BOUND ( 'NONE', #139922, .T. ) ;
#52159 = CARTESIAN_POINT ( 'NONE',  ( 5.991454128980707949, 7.190850779781567503, -1.201235417510186254 ) ) ;
#52160 = CARTESIAN_POINT ( 'NONE',  ( -1.001543065824772872E-14, 5.134375000341421469, 1.575800808251672791 ) ) ;
#52161 = CARTESIAN_POINT ( 'NONE',  ( 0.6098336241119780565, -0.6879379538977903330, 1.784437680087819666 ) ) ;
#52162 = CARTESIAN_POINT ( 'NONE',  ( 3.274023454312132486, -1.055227348164128331, 1.420681018326484413 ) ) ;
#52163 = CARTESIAN_POINT ( 'NONE',  ( 0.3285747216504387724, 1.318609938922534530, -1.385187620709791512 ) ) ;
#52165 = CARTESIAN_POINT ( 'NONE',  ( 4.130425774021486696, 0.5146700378890654015, 1.845081245478853216 ) ) ;
#52164 = CARTESIAN_POINT ( 'NONE',  ( -9.398826802771548472, 11.98838390803207865, -1.599625672291263179 ) ) ;
#52166 =( GEOMETRIC_REPRESENTATION_CONTEXT ( 3 ) GLOBAL_UNCERTAINTY_ASSIGNED_CONTEXT ( ( #90449 ) ) GLOBAL_UNIT_ASSIGNED_CONTEXT ( ( #102775, #52946, #214333 ) ) REPRESENTATION_CONTEXT ( 'NONE', 'WORKASPACE' ) );
#52167 = CARTESIAN_POINT ( 'NONE',  ( 0.000000000000000000, 1.000000000000000888, 0.000000000000000000 ) ) ;
#52168 = CARTESIAN_POINT ( 'NONE',  ( 4.879337363741727884, -0.09859167047137314122, 1.967224067494575346 ) ) ;
#52169 = CARTESIAN_POINT ( 'NONE',  ( 0.4223351350958382544, -2.109807164369668087, 0.2139620856976830743 ) ) ;
#52170 = DIRECTION ( 'NONE',  ( -0.000000000000000000, -1.000000000000000000, -0.000000000000000000 ) ) ;
#52171 = CARTESIAN_POINT ( 'NONE',  ( 3.660894226558962128, -1.649352935060313552, -0.8826137995501317501 ) ) ;
#52173 = ORIENTED_EDGE ( 'NONE', *, *, #5514, .T. ) ;
#52172 = CARTESIAN_POINT ( 'NONE',  ( 0.2932112110246976044, 1.350478442433366677, 1.228755397233910696 ) ) ;
#52175 = FACE_OUTER_BOUND ( 'NONE', #106350, .T. ) ;
#52174 = CARTESIAN_POINT ( 'NONE',  ( 4.002700589841681200, -0.6913439845411989415, -2.095861086919461602 ) ) ;
#52176 = CARTESIAN_POINT ( 'NONE',  ( -1.001543065824772872E-14, 4.634375000341418804, 1.575800808251672791 ) ) ;
#52177 = ADVANCED_FACE ( 'NONE', ( #187978, #20137 ), #3868, .T. ) ;
#52178 = CARTESIAN_POINT ( 'NONE',  ( 0.4497679408741364071, 1.527348849510310247, 1.386460675282843447 ) ) ;
#52179 = CARTESIAN_POINT ( 'NONE',  ( 6.076025397218672630, 10.24044673006381245, -0.7998128361456291469 ) ) ;
#52180 = CARTESIAN_POINT ( 'NONE',  ( -7.831806290188425557, 12.28885777186185990, -0.7998128361456281477 ) ) ;
#52181 = CARTESIAN_POINT ( 'NONE',  ( 11.18654035131437219, 1.000000000000000888, -4.041720556560823852 ) ) ;
#52182 = CARTESIAN_POINT ( 'NONE',  ( -3.425116838706585565, -0.02043104031221949779, -0.4185867116033271107 ) ) ;
#52183 = CARTESIAN_POINT ( 'NONE',  ( -7.778383330260382422, -6.134628647623486586, -7.778383330260335349 ) ) ;
#52184 = ORIENTED_EDGE ( 'NONE', *, *, #55165, .F. ) ;
#52185 = CARTESIAN_POINT ( 'NONE',  ( 3.561042923925850978, 1.633862107263984065, -1.271492733312264090 ) ) ;
#52186 = CARTESIAN_POINT ( 'NONE',  ( -1.201851678989727383E-14, 5.087500000000019007, -1.732050807568863648 ) ) ;
#52187 = CARTESIAN_POINT ( 'NONE',  ( 1.862795570070171713, -1.530026953448139659, 1.527182012981804560 ) ) ;
#52188 = CARTESIAN_POINT ( 'NONE',  ( -6.317530715954224441, 6.956803165068716766, 0.9171252194158643345 ) ) ;
#52189 = CARTESIAN_POINT ( 'NONE',  ( 0.4869804533438352734, -1.902474711392083684, -0.6784070981462678729 ) ) ;
#52190 = DIRECTION ( 'NONE',  ( 0.000000000000000000, 1.000000000000000000, 0.000000000000000000 ) ) ;
#52191 = ORIENTED_EDGE ( 'NONE', *, *, #172200, .F. ) ;
#52193 = CARTESIAN_POINT ( 'NONE',  ( 8.975134502566660899, 10.53370701015836275, -1.082531754730543083 ) ) ;
#52192 = CARTESIAN_POINT ( 'NONE',  ( 0.07499057489264347731, 2.883324855518037300, -2.444194386608829372 ) ) ;
#52194 = FACE_OUTER_BOUND ( 'NONE', #183807, .T. ) ;
#52195 = CARTESIAN_POINT ( 'NONE',  ( 6.421099303836709460, -1.707838190419972424, 0.8681067396549295712 ) ) ;
#52196 = CARTESIAN_POINT ( 'NONE',  ( 6.539320575229247368, 1.232987345766973775, 2.316458022558224972 ) ) ;
#52197 = CARTESIAN_POINT ( 'NONE',  ( 3.808297599986898430, 1.548825491099754315, -1.550762550882843094 ) ) ;
#52198 = CARTESIAN_POINT ( 'NONE',  ( 1.499999999999987121, 2.827083334016148530, -0.8660254037844262731 ) ) ;
#52199 = CARTESIAN_POINT ( 'NONE',  ( 3.023589307540079041, -0.3687504995396119201, 1.876329818327879817 ) ) ;
#52200 = CARTESIAN_POINT ( 'NONE',  ( -4.416205349749324327, 6.175325546172740765, 1.599625672291267398 ) ) ;
#52202 = CARTESIAN_POINT ( 'NONE',  ( 4.243338890952890630, 5.973648010910253880, -1.443375672974051449 ) ) ;
#52201 = CARTESIAN_POINT ( 'NONE',  ( 4.241422899474024177, 0.4370803545316758743, -1.968444674787086512 ) ) ;
#52204 = CARTESIAN_POINT ( 'NONE',  ( 1.177361486786612899, 1.528755565978222819, 1.314981834344926437 ) ) ;
#52203 = CARTESIAN_POINT ( 'NONE',  ( -15.75000000000000000, 11.29999999999999893, -1.800000000000001155 ) ) ;
#52205 = CARTESIAN_POINT ( 'NONE',  ( -1.364683531250000748, 11.42187500034139802, 0.000000000000000000 ) ) ;
#52207 = CARTESIAN_POINT ( 'NONE',  ( -6.493429226302317225, 6.540365283632955773, 0.7998128361456341429 ) ) ;
#52206 = CARTESIAN_POINT ( 'NONE',  ( -0.02329727741511803188, -2.225753042794619496, -0.5483686822410521744 ) ) ;
#52208 = CARTESIAN_POINT ( 'NONE',  ( 4.207791664195513093, -1.720086916870446236, 0.1276756817342617201 ) ) ;
#52209 = CARTESIAN_POINT ( 'NONE',  ( -0.1399997263889663501, 0.2375346743129815030, -2.034463206964792548 ) ) ;
#52210 = CARTESIAN_POINT ( 'NONE',  ( 6.435316467980822353, 10.65961964595298817, 1.040834085586084257E-14 ) ) ;
#52211 = CARTESIAN_POINT ( 'NONE',  ( 5.034155109375821446, 4.767602470560229122, -0.7998128361456221525 ) ) ;
#52212 = CARTESIAN_POINT ( 'NONE',  ( 1.135121963537696566, -0.04462593873827064989, -1.961518378280776354 ) ) ;
#52213 = CARTESIAN_POINT ( 'NONE',  ( 5.005985031943777308, 6.863401842066294556, -1.599625672291256295 ) ) ;
#52214 = CARTESIAN_POINT ( 'NONE',  ( 0.07516593201273635838, 7.629137130509072939, -2.644199648255764590 ) ) ;
#52215 = ORIENTED_EDGE ( 'NONE', *, *, #94831, .T. ) ;
#52216 = SURFACE_STYLE_USAGE ( .BOTH. , #200570 ) ;
#52217 = ORIENTED_EDGE ( 'NONE', *, *, #961, .T. ) ;
#52218 = CARTESIAN_POINT ( 'NONE',  ( 4.178215122889179511, 0.8575144648667647473, 1.595655492163786437 ) ) ;
#52219 = ORIENTED_EDGE ( 'NONE', *, *, #138625, .T. ) ;
#52220 = CARTESIAN_POINT ( 'NONE',  ( 6.505933609711257226, 8.683618192786854095, -1.599625672291281386 ) ) ;
#52221 = CARTESIAN_POINT ( 'NONE',  ( -5.000000000000024869, 3.300000000000025135, 0.7750000000000238920 ) ) ;
#52222 = EDGE_CURVE ( 'NONE', #124966, #168364, #73637, .T. ) ;
#52223 = CARTESIAN_POINT ( 'NONE',  ( 4.811091142047322577, 1.503129720864199381, -1.010622461758519552 ) ) ;
#52224 = CARTESIAN_POINT ( 'NONE',  ( 5.465345319640213972, 8.429967735338637524, -1.082531754730548412 ) ) ;
#52225 = CARTESIAN_POINT ( 'NONE',  ( -11.92619525870750508, 10.07377703206319808, -1.328859154004902621 ) ) ;
#52226 = CARTESIAN_POINT ( 'NONE',  ( 5.575284262857175044, 6.175169341367511500, -0.8878447928483481633 ) ) ;
#52227 = EDGE_CURVE ( 'NONE', #111991, #37457, #186912, .T. ) ;
#52229 = CARTESIAN_POINT ( 'NONE',  ( 8.353795204314554468, 12.89784483834236184, -0.7998128361456352531 ) ) ;
#52228 = CARTESIAN_POINT ( 'NONE',  ( 5.951566935816642534, 1.409582436273165706, 1.215217600354216554 ) ) ;
#52230 = CARTESIAN_POINT ( 'NONE',  ( 3.409697593026795204, -1.143712931967875601, -1.536527803759838662 ) ) ;
#52231 = CARTESIAN_POINT ( 'NONE',  ( 0.000000000000000000, 15.00041888085534758, 0.000000000000000000 ) ) ;
#52232 = CARTESIAN_POINT ( 'NONE',  ( -12.26626736352559455, 6.252815285820443769, 3.851661612215340647 ) ) ;
#52233 = MECHANICAL_DESIGN_GEOMETRIC_PRESENTATION_REPRESENTATION (  '', ( #121419 ), #79883 ) ;
#52234 = CARTESIAN_POINT ( 'NONE',  ( -10.99950989413231106, -9.915617157791128733, 0.1038368378055241209 ) ) ;
#52235 = CARTESIAN_POINT ( 'NONE',  ( 6.805829924380118356, 7.042482454639357847, 0.7216878364870317197 ) ) ;
#52236 = CARTESIAN_POINT ( 'NONE',  ( -9.408995418203979000, 12.00024729270324286, 1.443375672974076540 ) ) ;
#52237 = CARTESIAN_POINT ( 'NONE',  ( 0.3566080023540800781, 0.8287714912002723811, 1.996717379258300840 ) ) ;
#52238 = CARTESIAN_POINT ( 'NONE',  ( -3.962726036944197894, 7.845207153068690431, -0.7998128361456481317 ) ) ;
#52239 = CARTESIAN_POINT ( 'NONE',  ( 4.016958651398847557, 7.908478536599129249, -0.7998128361456362523 ) ) ;
#52240 = CARTESIAN_POINT ( 'NONE',  ( 0.4283665542385572955, 1.745377284433462295, 0.5351633580037706839 ) ) ;
#52241 = CARTESIAN_POINT ( 'NONE',  ( -5.229694566569281555, 7.124396299129368337, 1.599625672291267398 ) ) ;
#52242 = CARTESIAN_POINT ( 'NONE',  ( 3.328933297416610593, 0.04358344136132231289, 1.825221112333124340 ) ) ;
#52243 = CARTESIAN_POINT ( 'NONE',  ( 9.680359324772695118, 13.43752487939448947, 8.167046318416051776 ) ) ;
#52244 = CARTESIAN_POINT ( 'NONE',  ( 1.898553772666348394, -1.876154101037771582, -0.3696338911259658411 ) ) ;
#52245 = CARTESIAN_POINT ( 'NONE',  ( 2.260148812482842828, -1.969196485324760326, 0.04527702327579082725 ) ) ;
#52246 = CARTESIAN_POINT ( 'NONE',  ( 4.194824786304445219, 1.561856751782536135, 1.154042840620983057 ) ) ;
#52247 = ORIENTED_EDGE ( 'NONE', *, *, #9604, .T. ) ;
#52248 = CARTESIAN_POINT ( 'NONE',  ( -8.072954122294394352, 8.383144328957069291, -0.7998128361456362523 ) ) ;
#52250 = CARTESIAN_POINT ( 'NONE',  ( 4.289387122732970958, -0.003046686910593982868, -2.120778211268215419 ) ) ;
#52249 = CARTESIAN_POINT ( 'NONE',  ( 7.343676480457483002, 8.596652644402405841, -1.199719254218452047 ) ) ;
#52251 = CARTESIAN_POINT ( 'NONE',  ( 0.4655551865852050608, -8.176568542494919711, 9.512045263456268884 ) ) ;
#52252 = CARTESIAN_POINT ( 'NONE',  ( 7.747594715205354809, 11.12627870345989756, -1.199719254218446718 ) ) ;
#52253 = CARTESIAN_POINT ( 'NONE',  ( 6.089152713731276201, 6.031799978164165132, 0.2946234760112295126 ) ) ;
#52254 = DIRECTION ( 'NONE',  ( -0.6507913734559640506, -0.7592566023653004592, 0.000000000000000000 ) ) ;
#52255 = ORIENTED_EDGE ( 'NONE', *, *, #190193, .F. ) ;
#52256 = CARTESIAN_POINT ( 'NONE',  ( 3.337278367258157630, 7.045241861776501580, 0.7998128361456341429 ) ) ;
#52257 = VECTOR ( 'NONE', #86295, 999.9999999999998863 ) ;
#52258 = CARTESIAN_POINT ( 'NONE',  ( 5.254667053748194760, 8.288139441751686931, 1.199719254218452047 ) ) ;
#52259 = CARTESIAN_POINT ( 'NONE',  ( 1.458777222063855294, 1.000000000000000888, -1.713029193092652447 ) ) ;
#52260 = CARTESIAN_POINT ( 'NONE',  ( 4.441915170580639227, 0.7783198120194650960, -1.651611053696280695 ) ) ;
#52261 = CARTESIAN_POINT ( 'NONE',  ( 0.1392002015415672034, -0.1474423581745692435, -2.037351525059682977 ) ) ;
#52262 = CARTESIAN_POINT ( 'NONE',  ( -9.829298180227631576, 10.56986208646148384, 1.040834085586084257E-14 ) ) ;
#52263 = CARTESIAN_POINT ( 'NONE',  ( -4.611335679197930304, 8.465601755996580380, 0.3353434889079315862 ) ) ;
#52264 = CARTESIAN_POINT ( 'NONE',  ( 6.764690511086886823E-16, -5.511313137147262786, 11.00000000000000178 ) ) ;
#52265 = CARTESIAN_POINT ( 'NONE',  ( 4.574985519202336981, -0.0001439422951596270033, -1.870836309977530920 ) ) ;
#52266 = CARTESIAN_POINT ( 'NONE',  ( 6.428537391173986038, 10.65171072301167854, 0.7998128361456462443 ) ) ;
#52267 = CARTESIAN_POINT ( 'NONE',  ( 3.580616652426432012, -1.856930023900615456, -0.5128254122194577658 ) ) ;
#52268 = CARTESIAN_POINT ( 'NONE',  ( -4.249591082879585535, 7.045274465746411252, 1.199719254218464037 ) ) ;
#52269 = EDGE_CURVE ( 'NONE', #12495, #164712, #132448, .T. ) ;
#52270 = STYLED_ITEM ( 'NONE', ( #28255 ), #165584 ) ;
#52271 = CARTESIAN_POINT ( 'NONE',  ( 5.190073875932979419, 4.949507698210251938, 0.7998128361456341429 ) ) ;
#52272 = CARTESIAN_POINT ( 'NONE',  ( -0.6823417656250039265, 9.130208333674726617, -1.181850606188755259 ) ) ;
#52273 = CARTESIAN_POINT ( 'NONE',  ( -5.364222332501225488, 9.410009821226765325, 0.7998128361456481317 ) ) ;
#52274 = CARTESIAN_POINT ( 'NONE',  ( 3.334415713957098681, 5.977569868670206787, -1.199719254218446718 ) ) ;
#52275 = CARTESIAN_POINT ( 'NONE',  ( -6.312203035614172286, 9.521931420595302953, -1.199719254218452047 ) ) ;
#52277 = CARTESIAN_POINT ( 'NONE',  ( 1.072038591870585700, -0.9482746200860227015, 1.893052406114493769 ) ) ;
#52276 = B_SPLINE_CURVE_WITH_KNOTS ( 'NONE', 3,
 ( #171719, #107863, #75293, #173889, #73133, #103530, #72063, #170651, #5992, #138173 ),
 .UNSPECIFIED., .F., .F.,
 ( 4, 2, 2, 2, 4 ),
 ( 0.001822879634083279061, 0.002175306537177320535, 0.002527733440271361792, 0.002880160343365403049, 0.003232587246459444306 ),
 .UNSPECIFIED. ) ;
#52278 = CARTESIAN_POINT ( 'NONE',  ( 8.028399517586572998, 12.51821653715971472, -0.7998128361456352531 ) ) ;
#52279 = CARTESIAN_POINT ( 'NONE',  ( -7.005397802120316264, 5.950282834973755541, 2.500000000000000000 ) ) ;
#52280 = CARTESIAN_POINT ( 'NONE',  ( 6.825056245572477032, -1.890314563506745316, -0.8446596084958692963 ) ) ;
#52282 = CARTESIAN_POINT ( 'NONE',  ( 4.149696378627680815, 7.633013953984455036, -0.8115063166676712569 ) ) ;
#52281 = CARTESIAN_POINT ( 'NONE',  ( 1.874305484616908934, -0.09156810461483089192, -1.839108553062768214 ) ) ;
#52283 = CARTESIAN_POINT ( 'NONE',  ( 6.819388077993785657, 7.058300300521964665, 1.040834085586084257E-14 ) ) ;
#52285 = PRESENTATION_STYLE_ASSIGNMENT (( #150866 ) ) ;
#52284 = CARTESIAN_POINT ( 'NONE',  ( 4.258669648468281110, 6.061810238003387141, 1.443375672974058777 ) ) ;
#52286 = CARTESIAN_POINT ( 'NONE',  ( 1.078551950277906402, -2.237456700407819632, -0.4976139165283523513 ) ) ;
#52287 = CARTESIAN_POINT ( 'NONE',  ( -1.233356347899354111, 3.300000000000025135, -0.5988873898902316029 ) ) ;
#52288 = CARTESIAN_POINT ( 'NONE',  ( 6.263619209540105537, 1.000520857970560895, 1.664240579554799648 ) ) ;
#52289 = ORIENTED_EDGE ( 'NONE', *, *, #22632, .T. ) ;
#52291 = ADVANCED_FACE ( 'NONE', ( #24395 ), #158052, .F. ) ;
#52290 = CARTESIAN_POINT ( 'NONE',  ( 7.904040366642684390, 11.20483561351640844, 1.082531754730558626 ) ) ;
#52292 = CARTESIAN_POINT ( 'NONE',  ( 1.002198536899261860, -0.9015652438304004868, 1.800089726458251826 ) ) ;
#52293 = CARTESIAN_POINT ( 'NONE',  ( 6.518203450479811423, 5.167241622962441383, -2.437504649502886256 ) ) ;
#52295 = CARTESIAN_POINT ( 'NONE',  ( 11.04984958223792368, 12.49082486231873546, 1.056557932048283188 ) ) ;
#52294 = CARTESIAN_POINT ( 'NONE',  ( -6.679363233026820446, 10.94434087183997129, 0.000000000000000000 ) ) ;
#52296 = DIRECTION ( 'NONE',  ( 0.000000000000000000, 0.000000000000000000, -1.000000000000000000 ) ) ;
#52298 = CARTESIAN_POINT ( 'NONE',  ( 2.711481306777110412, -1.750889404861367460, 0.2573583090697410536 ) ) ;
#52297 = CARTESIAN_POINT ( 'NONE',  ( 4.066417572287989834, -1.950679019168543471, -0.7525511210752598990 ) ) ;
#52299 = DIRECTION ( 'NONE',  ( 0.000000000000000000, -1.000000000000000000, 0.000000000000000000 ) ) ;
#52301 = CARTESIAN_POINT ( 'NONE',  ( 5.824266732648851530, 2.207754452112113075, 0.6165074292824882507 ) ) ;
#52300 = CARTESIAN_POINT ( 'NONE',  ( -11.51269375458374000, 6.866968676300322372, -3.391140620325245880 ) ) ;
#52302 = CARTESIAN_POINT ( 'NONE',  ( 3.415673062852276232, 1.103011313415346306, -1.346137666936922717 ) ) ;
#52303 = CARTESIAN_POINT ( 'NONE',  ( 9.890836756369282057, 11.49806328964105617, -1.199719254218440723 ) ) ;
#52304 = CARTESIAN_POINT ( 'NONE',  ( 5.143339171537801846, 7.093924681584510061, 1.599625672291269396 ) ) ;
#52305 = CARTESIAN_POINT ( 'NONE',  ( 3.286226705615200139, -1.671546763608670272, 0.4602933761382789202 ) ) ;
#52306 = CARTESIAN_POINT ( 'NONE',  ( 3.947858391199970285, 1.570127341852745273, 1.499791163327832466 ) ) ;
#52307 = CARTESIAN_POINT ( 'NONE',  ( 3.811813743736467419, 7.598866467667865443, 1.040834085586084257E-14 ) ) ;
#52308 = CARTESIAN_POINT ( 'NONE',  ( 4.540250091716044878, 0.7762272601403925609, 1.861345588084816871 ) ) ;
#52309 = CARTESIAN_POINT ( 'NONE',  ( 1.312500000000000888, 1.451031289061174734, 1.451031289061067486 ) ) ;
#52310 = CARTESIAN_POINT ( 'NONE',  ( 1.499999999999989120, 3.785416667349481123, 0.8660254037844524744 ) ) ;
#52311 = CARTESIAN_POINT ( 'NONE',  ( 2.063383741992553144, 0.3316209358346365876, -1.897488084917675843 ) ) ;
#52312 = CARTESIAN_POINT ( 'NONE',  ( -8.012344526598182026E-15, 15.29687500034140157, -1.575800808251669460 ) ) ;
#52313 = CARTESIAN_POINT ( 'NONE',  ( 6.152596803620836496, 2.197069216644991663, 0.3270334163130541594 ) ) ;
#52314 = EDGE_LOOP ( 'NONE', ( #192375, #92719, #194481, #94415 ) ) ;
#52316 = VECTOR ( 'NONE', #147861, 1000.000000000000000 ) ;
#52315 = CARTESIAN_POINT ( 'NONE',  ( -0.2108831679771168421, 7.629137130509075604, -2.497154329497493386 ) ) ;
#52317 = CARTESIAN_POINT ( 'NONE',  ( -1.500000000000013101, 1.420833333333354043, 0.8660254037844403729 ) ) ;
#52318 = CARTESIAN_POINT ( 'NONE',  ( 6.612626235163189925, 8.737816579155630592, -1.599625672291262513 ) ) ;
#52319 = CARTESIAN_POINT ( 'NONE',  ( 3.619663824724254741, 6.206396314611513532, -1.082531754730543971 ) ) ;
#52320 = CARTESIAN_POINT ( 'NONE',  ( 0.000000000000000000, -2.296874999522042327, -3.793834371823813445 ) ) ;
#52321 = CARTESIAN_POINT ( 'NONE',  ( 0.7861345822535183991, 2.139302153856616151, -0.5977261144227277168 ) ) ;
#52322 = CARTESIAN_POINT ( 'NONE',  ( 5.600043156098196917, 0.7966083592686535875, -1.793046234938546979 ) ) ;
#52323 = CARTESIAN_POINT ( 'NONE',  ( 6.968527767744088663, 11.07377346243604599, 0.7216878364870438212 ) ) ;
#52324 = CARTESIAN_POINT ( 'NONE',  ( -0.1286694677790374830, 3.477644553696438656, 1.998596537245283411 ) ) ;
#52325 = CARTESIAN_POINT ( 'NONE',  ( 6.362609103649501385, -1.606607173180201187, 1.593162483179947575 ) ) ;
#52326 = CARTESIAN_POINT ( 'NONE',  ( 3.705121118284530279, 7.544668081299086282, -1.734723475976807094E-15 ) ) ;
#52327 = CARTESIAN_POINT ( 'NONE',  ( -5.478903473698268023, 5.564677938835638216, -0.7216878364870338292 ) ) ;
#52328 = CARTESIAN_POINT ( 'NONE',  ( 4.668458352237446540, -0.8791470107305986437, -1.866060610730088332 ) ) ;
#52329 = CARTESIAN_POINT ( 'NONE',  ( -4.055860508782465068, 7.883587693554856557, 1.040834085586084257E-14 ) ) ;
#52330 =( BOUNDED_CURVE ( )  B_SPLINE_CURVE ( 2, ( #99862, #148615, #165924, #34837, #67318, #83597, #149679 ),
 .UNSPECIFIED., .F., .T. ) 
 B_SPLINE_CURVE_WITH_KNOTS ( ( 3, 2, 2, 3 ),
 ( 0.3250000000000000666, 0.3333333333333333703, 0.3416666666666667851, 0.3500000000000000888 ),
 .UNSPECIFIED. ) 
 CURVE ( )  GEOMETRIC_REPRESENTATION_ITEM ( )  RATIONAL_B_SPLINE_CURVE ( ( 0.9999999999999991118, 0.8660254037844395958, 1.000000000000000000, 0.8660254037844387076, 1.000000000000000000, 0.8660254037844369313, 1.000000000000001776 ) ) 
 REPRESENTATION_ITEM ( '' )  );
#52332 = EDGE_CURVE ( 'NONE', #78570, #93560, #40397, .T. ) ;
#52331 = CARTESIAN_POINT ( 'NONE',  ( 0.7499999999999920064, 4.514583334016150751, 1.299038105676669330 ) ) ;
#52333 = CARTESIAN_POINT ( 'NONE',  ( 1.364683531249990311, 5.196875000341417916, 1.214306433183764966E-14 ) ) ;
#52334 = CARTESIAN_POINT ( 'NONE',  ( 5.800035319642947051, -1.870726058474009079, -0.0005997126256013227737 ) ) ;
#52335 = CARTESIAN_POINT ( 'NONE',  ( 5.115702696222887980, 0.1348363893083539267, 1.728983578677806499 ) ) ;
#52336 = CARTESIAN_POINT ( 'NONE',  ( 3.825523041098664034, 0.9271419989833797892, -1.472723941875812237 ) ) ;
#52337 = CARTESIAN_POINT ( 'NONE',  ( -2.450243370979069635, 1.813773193624685254, 11.74719778151168192 ) ) ;
#52338 = CARTESIAN_POINT ( 'NONE',  ( 2.208868952076637804, 2.049428429192188705, 1.027153634429162743 ) ) ;
#52339 = CARTESIAN_POINT ( 'NONE',  ( 1.364683531249990311, 4.196875000341417028, 1.214306433183764966E-14 ) ) ;
#52340 = CARTESIAN_POINT ( 'NONE',  ( 5.442948297640814559, -1.648798800320664615, -1.285478093666903687 ) ) ;
#52341 = CARTESIAN_POINT ( 'NONE',  ( 6.509718631618705231, -0.9178700960432868428, -1.711342201762585002 ) ) ;
#52342 = EDGE_CURVE ( 'NONE', #17744, #60775, #94393, .T. ) ;
#52343 = LINE ( 'NONE', #117403, #170794 ) ;
#52344 = CARTESIAN_POINT ( 'NONE',  ( 1.512342498431101134, -1.897697209584522815, 0.6819976561535444626 ) ) ;
#52345 = CARTESIAN_POINT ( 'NONE',  ( 0.3928598746986839974, 1.819701785225702473, -1.220828600141062203 ) ) ;
#52346 = CARTESIAN_POINT ( 'NONE',  ( 7.925031528659947533, 13.65663895357722701, -8.702496307462409320 ) ) ;
#52347 = CARTESIAN_POINT ( 'NONE',  ( -7.446452682403657874, 9.710614100936176385, -1.599625672291263179 ) ) ;
#52348 =( BOUNDED_CURVE ( )  B_SPLINE_CURVE ( 2, ( #119346, #185333, #181080, #161, #7641, #21743, #186399, #203702, #124699 ),
 .UNSPECIFIED., .F., .T. ) 
 B_SPLINE_CURVE_WITH_KNOTS ( ( 3, 2, 2, 2, 3 ),
 ( 0.5781250000000001110, 0.5833333333333333703, 0.5937500000000000000, 0.6041666666666666297, 0.6093749999999996669 ),
 .UNSPECIFIED. ) 
 CURVE ( )  GEOMETRIC_REPRESENTATION_ITEM ( )  RATIONAL_B_SPLINE_CURVE ( ( 0.9330127018922192983, 0.9330127018922207416, 1.000000000000000000, 0.8660254037844387076, 1.000000000000000000, 0.8660254037844387076, 1.000000000000000000, 0.9330127018922236282, 0.9330127018922194093 ) ) 
 REPRESENTATION_ITEM ( '' )  );
#52349 = CARTESIAN_POINT ( 'NONE',  ( 4.971035877704902184, 8.951292290631053916, 1.040834085586084257E-14 ) ) ;
#52350 = CARTESIAN_POINT ( 'NONE',  ( 2.086737175084628859, -1.302296122868449535, 1.673399772156684895 ) ) ;
#52351 = CARTESIAN_POINT ( 'NONE',  ( -1.364683531250014514, -1.219791666325248602, 0.7879004041258379498 ) ) ;
#52352 = CARTESIAN_POINT ( 'NONE',  ( 5.760330229460346452, 0.7440287100829169331, 1.667389206893993725 ) ) ;
#52353 = ORIENTED_EDGE ( 'NONE', *, *, #57473, .T. ) ;
#52354 = CARTESIAN_POINT ( 'NONE',  ( -7.306918443122272677, 7.489436036589583345, 0.7998128361456341429 ) ) ;
#52355 = CARTESIAN_POINT ( 'NONE',  ( 2.273349394227877074, 5.683342515206170731, 0.4597581080974435519 ) ) ;
#52356 = CARTESIAN_POINT ( 'NONE',  ( -3.285556943750000070, -0.8968749995220438587, 0.000000000000000000 ) ) ;
#52357 = CARTESIAN_POINT ( 'NONE',  ( -6.880926654135487652, 7.986501503701545879, 1.199719254218450271 ) ) ;
#52358 = CARTESIAN_POINT ( 'NONE',  ( 2.865494903669623117, -1.653614387114977990, -1.159512146270498478 ) ) ;
#52359 = CARTESIAN_POINT ( 'NONE',  ( 6.581111309608331794, -0.1016299978719436697, -2.204559905201553427 ) ) ;
#52360 = CARTESIAN_POINT ( 'NONE',  ( -5.171509248969888617, 4.998125310078441075, 0.7998128361456281477 ) ) ;
#52361 = CARTESIAN_POINT ( 'NONE',  ( 4.311269015108330827, -1.545260327404588852, -1.036625270625696205 ) ) ;
#52362 = CARTESIAN_POINT ( 'NONE',  ( 8.106885785967500979, 11.54545161934907682, 1.199719254218460707 ) ) ;
#52363 =( BOUNDED_SURFACE ( )  B_SPLINE_SURFACE ( 3, 3, ( 
 ( #175735, #205258, #179994, #11068, #27328, #46812, #129202, #28405, #189029, #77147 ),
 ( #14261, #64110, #143268, #127062, #193024, #94499, #80352, #112926, #196243, #44676 ),
 ( #160537, #212466, #31618, #78216, #178939, #194096, #146451, #144339, #210339, #30553 ),
 ( #161621, #61978, #95571, #45745, #111863, #177868, #13214, #145405, #211405, #116104 ),
 ( #48932, #166942, #18535, #182095, #33726, #99804, #51054, #19605, #200475, #84612 ),
 ( #36920, #65144, #165869, #199409, #198346, #135512, #100858, #164801, #117178, #183179 ),
 ( #115050, #53182, #16393, #150701, #1203, #49986, #213521, #34783, #52121, #131300 ) ),
 .UNSPECIFIED., .T., .F., .F. ) 
 B_SPLINE_SURFACE_WITH_KNOTS ( ( 4, 3, 4 ),
 ( 4, 1, 1, 1, 1, 1, 1, 4 ),
 ( 0.000000000000000000, 0.5000000000000000000, 1.000000000000000000 ),
 ( 0.000000000000000000, 0.09884949474608377418, 0.1930937302289311708, 0.2616037862002966730, 0.3630310524065313849, 0.5216543902990324888, 0.7338513509102306820, 0.9999999999999998890 ),
 .UNSPECIFIED. ) 
 GEOMETRIC_REPRESENTATION_ITEM ( )  RATIONAL_B_SPLINE_SURFACE ( (
 ( 1.000000000000000222, 1.000000000000000222, 1.000000000000000000, 1.000000000000000222, 1.000000000000000444, 1.000000000000000222, 1.000000000000000222, 1.000000000000000222, 1.000000000000000222, 1.000000000000000222),
 ( 0.3333333333333334259, 0.3333333333333334259, 0.3333333333333334814, 0.3333333333333333703, 0.3333333333333334814, 0.3333333333333333703, 0.3333333333333334814, 0.3333333333333333703, 0.3333333333333334259, 0.3333333333333334259),
 ( 0.3333333333333334259, 0.3333333333333334259, 0.3333333333333334814, 0.3333333333333333703, 0.3333333333333334814, 0.3333333333333333703, 0.3333333333333334814, 0.3333333333333333703, 0.3333333333333334259, 0.3333333333333334259),
 ( 1.000000000000000222, 1.000000000000000222, 1.000000000000000000, 1.000000000000000222, 1.000000000000000444, 1.000000000000000222, 1.000000000000000222, 1.000000000000000222, 1.000000000000000222, 1.000000000000000222),
 ( 0.3333333333333334259, 0.3333333333333334259, 0.3333333333333334814, 0.3333333333333333703, 0.3333333333333334814, 0.3333333333333333703, 0.3333333333333334814, 0.3333333333333333703, 0.3333333333333334259, 0.3333333333333334259),
 ( 0.3333333333333334259, 0.3333333333333334259, 0.3333333333333334814, 0.3333333333333333703, 0.3333333333333334814, 0.3333333333333333703, 0.3333333333333334814, 0.3333333333333333703, 0.3333333333333334259, 0.3333333333333334259),
 ( 1.000000000000000222, 1.000000000000000222, 1.000000000000000000, 1.000000000000000222, 1.000000000000000444, 1.000000000000000222, 1.000000000000000222, 1.000000000000000222, 1.000000000000000222, 1.000000000000000222) ) ) 
 REPRESENTATION_ITEM ( '' )  SURFACE ( )  );
#52364 = CARTESIAN_POINT ( 'NONE',  ( 3.404766800216717737, 6.348112014766642552, 1.069586989871921467 ) ) ;
#52365 = ORIENTED_EDGE ( 'NONE', *, *, #187963, .T. ) ;
#52366 = CARTESIAN_POINT ( 'NONE',  ( -2.764973262183167968, 5.313220341600567664, 1.199719254218462483 ) ) ;
#52367 = CARTESIAN_POINT ( 'NONE',  ( -7.374745490829552885, 10.69128794168811680, -1.199719254218446718 ) ) ;
#52369 = CARTESIAN_POINT ( 'NONE',  ( -4.127447729399665199, 7.650344214561823009, 0.8192481249636590634 ) ) ;
#52368 = CARTESIAN_POINT ( 'NONE',  ( -6.424584688029276514, 8.588711117491191871, 1.599625672291269396 ) ) ;
#52370 = CARTESIAN_POINT ( 'NONE',  ( 1.364683531249986537, -0.8864583329919110133, 0.7879004041258500513 ) ) ;
#52371 = CARTESIAN_POINT ( 'NONE',  ( 2.020412548985677681, 1.729603159991144556, -0.1218859752038989053 ) ) ;
#52372 = CARTESIAN_POINT ( 'NONE',  ( 1.604977476713872697, -1.727474156022209328, 0.2105546776469246206 ) ) ;
#52374 = CARTESIAN_POINT ( 'NONE',  ( 7.266807147244743526, 11.42176607185347414, -0.7216878364870267237 ) ) ;
#52373 = CARTESIAN_POINT ( 'NONE',  ( 5.408889320884306073, 1.750735854880939746, -1.503546334452151134 ) ) ;
#52375 = CARTESIAN_POINT ( 'NONE',  ( 5.239300017038202917, 5.077214539491492928, 0.000000000000000000 ) ) ;
#52376 = CARTESIAN_POINT ( 'NONE',  ( 1.845067233098520942, -1.742569257963645146, 1.099794920586109725 ) ) ;
#52377 = CARTESIAN_POINT ( 'NONE',  ( 6.166260936116925606, 6.088392601758203071, 0.7998128361456341429 ) ) ;
#52378 = CARTESIAN_POINT ( 'NONE',  ( 0.1399997263886003374, 0.002789056014650820314, -1.999853399661279063 ) ) ;
#52379 = CARTESIAN_POINT ( 'NONE',  ( -6.286140498591554326, 7.362860665558790707, 1.199719254218452047 ) ) ;
#52380 = AXIS2_PLACEMENT_3D ( 'NONE', #84091, #115586, #150178 ) ;
#52381 = CARTESIAN_POINT ( 'NONE',  ( 6.737182200980119440, -1.669782060861616291, 0.8434366901180423426 ) ) ;
#52383 = CARTESIAN_POINT ( 'NONE',  ( -5.939880696562884310, 9.943961556049767836, 0.7216878364870267237 ) ) ;
#52382 = CARTESIAN_POINT ( 'NONE',  ( 4.289254230599209627, -0.005406649120142519548, -1.912571728590661380 ) ) ;
#52384 = CARTESIAN_POINT ( 'NONE',  ( 6.059228469117068805, -1.890744221452178353, -1.137928576693452820 ) ) ;
#52385 = CARTESIAN_POINT ( 'NONE',  ( -7.511572993685796537E-15, 1.750000000682812251, -1.414508159514599628 ) ) ;
#52386 = CARTESIAN_POINT ( 'NONE',  ( 1.499999999999993117, 10.60416666666666607, 0.8660254037844408170 ) ) ;
#52387 = CARTESIAN_POINT ( 'NONE',  ( 5.533136087708556694, 5.627949321847663278, 0.000000000000000000 ) ) ;
#52388 = CARTESIAN_POINT ( 'NONE',  ( -4.380693030546956912, 6.204170850428461392, 1.443375672974065660 ) ) ;
#52389 = CARTESIAN_POINT ( 'NONE',  ( 6.358074577831472673, 0.8120454629646983724, -1.959034198684066697 ) ) ;
#52390 = EDGE_LOOP ( 'NONE', ( #38370, #99596, #141126, #163541 ) ) ;
#52391 = CARTESIAN_POINT ( 'NONE',  ( 3.628207509315328760, -1.372338424813070556, -1.855037849730954091 ) ) ;
#52392 = CARTESIAN_POINT ( 'NONE',  ( 4.914483161888778540, 0.7490505147796695518, 1.813437088826752142 ) ) ;
#52393 = CARTESIAN_POINT ( 'NONE',  ( 0.4265131056294459433, -1.285834093136655643, 1.481649512794058543 ) ) ;
#52394 = DIRECTION ( 'NONE',  ( 0.000000000000000000, 0.000000000000000000, 1.000000000000000000 ) ) ;
#52395 = CYLINDRICAL_SURFACE ( 'NONE', #171548, 0.09999999999999982514 ) ;
#52396 = ORIENTED_EDGE ( 'NONE', *, *, #54844, .F. ) ;
#52397 = CARTESIAN_POINT ( 'NONE',  ( 6.438686429976131720, -1.555646628146038157, 1.282773817382940384 ) ) ;
#52399 = CARTESIAN_POINT ( 'NONE',  ( -8.239604668803112375, 10.63595808506888396, -1.599625672291263179 ) ) ;
#52398 = CARTESIAN_POINT ( 'NONE',  ( -5.331380718671772101, 7.243030143248949670, -1.599625672291256295 ) ) ;
#52400 = DIRECTION ( 'NONE',  ( 0.000000000000000000, 8.546850786086437571E-32, 1.000000000000000000 ) ) ;
#52401 = CARTESIAN_POINT ( 'NONE',  ( 2.817415258179640336, -1.886890863808653007, -1.073800027038468219 ) ) ;
#52402 = CARTESIAN_POINT ( 'NONE',  ( 0.3562973855445230598, 2.786757976255979319, 1.969129866515958005 ) ) ;
#52403 = CARTESIAN_POINT ( 'NONE',  ( 1.160570123509139906, 2.118417766304943495, 0.09849428607798524360 ) ) ;
#52404 = CARTESIAN_POINT ( 'NONE',  ( -1.500000000000013101, 1.452083334016150085, 0.8660254037844403729 ) ) ;
#52405 = CARTESIAN_POINT ( 'NONE',  ( 8.041957671200231417, 12.53403438304231976, 1.040834085586084257E-14 ) ) ;
#52406 = CARTESIAN_POINT ( 'NONE',  ( 11.89942855770814312, 13.79999999999999893, -0.7000000000000009548 ) ) ;
#52407 = CARTESIAN_POINT ( 'NONE',  ( 6.430738266435902517, 6.882057634903050669, 0.7203813067775278745 ) ) ;
#52408 = CARTESIAN_POINT ( 'NONE',  ( 2.249358885376837591, -1.653154358101496246, -1.230164295365917537 ) ) ;
#52409 = MECHANICAL_DESIGN_GEOMETRIC_PRESENTATION_REPRESENTATION (  '', ( #197721 ), #73256 ) ;
#52411 = DIRECTION ( 'NONE',  ( 0.000000000000000000, 0.000000000000000000, -1.000000000000000000 ) ) ;
#52410 = CARTESIAN_POINT ( 'NONE',  ( -8.157201976916404362, 12.66848607304450702, -0.7998128361456281477 ) ) ;
#52412 = CARTESIAN_POINT ( 'NONE',  ( -0.6823417656250212460, 1.801041667008083991, 1.181850606188755259 ) ) ;
#52413 = CARTESIAN_POINT ( 'NONE',  ( 1.499999999999990896, 5.525000000000022560, 1.214306433183764966E-14 ) ) ;
#52414 = CARTESIAN_POINT ( 'NONE',  ( 10.50000000000000355, 11.00718427492793161, 3.599999999999998312 ) ) ;
#52415 = VERTEX_POINT ( 'NONE', #80681 ) ;
#52416 = CARTESIAN_POINT ( 'NONE',  ( 4.231050068913538631, 1.749697241329374098, 0.7720063087622434095 ) ) ;
#52417 =( BOUNDED_CURVE ( )  B_SPLINE_CURVE ( 3, ( #91452, #57858, #138056, #121875 ),
 .UNSPECIFIED., .F., .T. ) 
 B_SPLINE_CURVE_WITH_KNOTS ( ( 4, 4 ),
 ( 4.712388980384560000, 5.557022599642902350 ),
 .UNSPECIFIED. ) 
 CURVE ( )  GEOMETRIC_REPRESENTATION_ITEM ( )  RATIONAL_B_SPLINE_CURVE ( ( 1.000000000000000000, 0.9414278581755095576, 0.9414278581755095576, 1.000000000000000000 ) ) 
 REPRESENTATION_ITEM ( '' )  );
#52418 = CARTESIAN_POINT ( 'NONE',  ( -3.474999999999997868, -1.020833333333332815, 2.006292185433951047 ) ) ;
#52419 = CARTESIAN_POINT ( 'NONE',  ( 1.282923566313122210, -2.207321063319432231, -0.4954982646878171582 ) ) ;
#52420 = CARTESIAN_POINT ( 'NONE',  ( -2.981903720001798597, 5.566305875722335372, -1.199719254218446718 ) ) ;
#52421 = CARTESIAN_POINT ( 'NONE',  ( 1.037045679623523897, -0.04297598538225732429, 1.811226269459820903 ) ) ;
#52422 = CARTESIAN_POINT ( 'NONE',  ( 1.323292448300671165, -1.390094005022534773, -1.318457861805687914 ) ) ;
#52423 = CARTESIAN_POINT ( 'NONE',  ( 1.732962091629593804, -1.965256999408044436, -0.6514315320021792921 ) ) ;
#52424 = CARTESIAN_POINT ( 'NONE',  ( -1.364683531250014514, 0.3427083336747508424, 0.7879004041258379498 ) ) ;
#52425 = AXIS2_PLACEMENT_3D ( 'NONE', #60446, #122355, #190439 ) ;
#52426 = CARTESIAN_POINT ( 'NONE',  ( 0.6550726410136185063, -1.664185259661060234, -1.056694852926373773 ) ) ;
#52427 = CARTESIAN_POINT ( 'NONE',  ( 5.584577364790731302, -1.880054400457907171, -0.4198111936028568469 ) ) ;
#52429 = CARTESIAN_POINT ( 'NONE',  ( 5.997574213172828905, 7.082153300894140635, -1.064076030282636420 ) ) ;
#52428 = CARTESIAN_POINT ( 'NONE',  ( 0.5050340691590156084, -0.7831231796689057667, -2.170891709475693876 ) ) ;
#52430 = CARTESIAN_POINT ( 'NONE',  ( -0.6823417656250212460, 1.051041667008083325, 1.181850606188755259 ) ) ;
#52431 = CARTESIAN_POINT ( 'NONE',  ( 4.562968466866096584, 1.596587869669671145, -1.305994239470360974 ) ) ;
#52432 = CARTESIAN_POINT ( 'NONE',  ( -5.540478329478883524, 9.615641817700700145, 0.000000000000000000 ) ) ;
#52433 = CARTESIAN_POINT ( 'NONE',  ( 8.697719238366680372, 10.10609285197134533, 1.199719254218462483 ) ) ;
#52434 = CARTESIAN_POINT ( 'NONE',  ( 4.704842999142070603, 5.447737239542574272, -1.199719254218452047 ) ) ;
#52435 = CARTESIAN_POINT ( 'NONE',  ( 4.171104814498611368, 8.018039383557042044, 0.7998128361456321445 ) ) ;
#52437 = CARTESIAN_POINT ( 'NONE',  ( -1.500000000000011324, 4.420833333333352044, 0.8660254037844403729 ) ) ;
#52436 = CARTESIAN_POINT ( 'NONE',  ( 5.438542061945497608, 2.074265116652589391, 0.3630613376124564584 ) ) ;
#52438 = CARTESIAN_POINT ( 'NONE',  ( 6.285608408418759119, -1.950803066209889636, 0.6937918898708083093 ) ) ;
#52439 = CARTESIAN_POINT ( 'NONE',  ( -1.402160292154681736E-14, 0.7593750003414168059, -1.575800808251659024 ) ) ;
#52440 = CARTESIAN_POINT ( 'NONE',  ( 4.516967039858135635, 1.974289957696921949, 0.8805908171375662619 ) ) ;
#52441 = CARTESIAN_POINT ( 'NONE',  ( 5.057288377774205479, -1.731171949422895651, 1.040023186547271328 ) ) ;
#52442 = CARTESIAN_POINT ( 'NONE',  ( -0.1399997263889597998, 7.629137130509076492, -2.600276787041354787 ) ) ;
#52445 = CARTESIAN_POINT ( 'NONE',  ( 6.832946231607457399, 7.074118146404578589, -0.7216878364870257245 ) ) ;
#52444 = CARTESIAN_POINT ( 'NONE',  ( 3.285556943749998737, -0.9552083328553737651, -1.896917185911906500 ) ) ;
#52443 = CARTESIAN_POINT ( 'NONE',  ( 6.230854113932139171, 9.427024345299638952, 1.199719254218452047 ) ) ;
#52446 = CARTESIAN_POINT ( 'NONE',  ( -5.444481204339554736, 8.509589284108232121, 1.199719254218454489 ) ) ;
#52447 = CARTESIAN_POINT ( 'NONE',  ( 4.030482632556767975, 0.5424685788828055300, 1.942097399793737633 ) ) ;
#52448 = CARTESIAN_POINT ( 'NONE',  ( -8.666686507633592385, 11.13422023037111330, 1.599625672291269396 ) ) ;
#52449 = CARTESIAN_POINT ( 'NONE',  ( -4.765854690403601879, 5.518917546014321829, 1.199719254218462483 ) ) ;
#52450 = LINE ( 'NONE', #118576, #153418 ) ;
#52451 =( NAMED_UNIT ( * ) PLANE_ANGLE_UNIT ( ) SI_UNIT ( $, .RADIAN. ) );
#52452 = CARTESIAN_POINT ( 'NONE',  ( 6.720655732516622294, 7.629137130509072051, 2.773739711112707340 ) ) ;
#52454 = CARTESIAN_POINT ( 'NONE',  ( 4.798453934790239295, 1.388474963651475269, -1.462457531588717830 ) ) ;
#52453 = CARTESIAN_POINT ( 'NONE',  ( -6.521108698048767138, 10.55178454779148289, -0.7216878364870267237 ) ) ;
#52455 = CARTESIAN_POINT ( 'NONE',  ( 1.499999999999991118, 5.754166666666685970, 0.8660254037844524744 ) ) ;
#52456 = CARTESIAN_POINT ( 'NONE',  ( 1.066563130004109405, -1.557762288434235476, -0.7409518577887274082 ) ) ;
#52457 = CARTESIAN_POINT ( 'NONE',  ( 4.877901405866606588, 8.912911750144889567, 0.7998128361456341429 ) ) ;
#52459 = CARTESIAN_POINT ( 'NONE',  ( 6.061904079085887354, 6.244845311787889486, 0.000000000000000000 ) ) ;
#52458 = CARTESIAN_POINT ( 'NONE',  ( 7.076992996653421741, 10.23994701519558781, -1.082531754730537976 ) ) ;
#52460 = CARTESIAN_POINT ( 'NONE',  ( -11.37585333846683255, 7.825601127584223882, 3.684762987566864378 ) ) ;
#52461 = CARTESIAN_POINT ( 'NONE',  ( 5.202362286721474050, -0.6290170809866748591, -1.761763226176292996 ) ) ;
#52462 = CARTESIAN_POINT ( 'NONE',  ( 6.469000937953021335, -1.553436082622870140, 1.280157488742767136 ) ) ;
#52463 = VECTOR ( 'NONE', #193767, 1000.000000000000227 ) ;
#52464 = CARTESIAN_POINT ( 'NONE',  ( -6.007671464186866928, 8.102312356341712984, 1.443375672974058777 ) ) ;
#52465 = VERTEX_POINT ( 'NONE', #100121 ) ;
#52466 = AXIS2_PLACEMENT_3D ( 'NONE', #122694, #207032, #173507 ) ;
#52467 = CARTESIAN_POINT ( 'NONE',  ( 0.1578276607246929530, 1.163290555716024244, 1.646825313395771762 ) ) ;
#52468 = CARTESIAN_POINT ( 'NONE',  ( 1.494102799026775008, -0.9672467274632718937, 1.531528279607297094 ) ) ;
#52469 = CARTESIAN_POINT ( 'NONE',  ( 4.434925645001613681, 5.307073019657559065, -1.082531754730548412 ) ) ;
#52470 = CARTESIAN_POINT ( 'NONE',  ( 5.911032513020412438, 1.904272706209766630, 1.023102869888978361 ) ) ;
#52471 = EDGE_CURVE ( 'NONE', #122534, #104947, #11323, .T. ) ;
#52472 = CARTESIAN_POINT ( 'NONE',  ( 7.610204295972345712, 7.772993188256215547, 0.7998128361456341429 ) ) ;
#52474 = CARTESIAN_POINT ( 'NONE',  ( 0.7783702408986278298, -0.4687143430282306733, -1.857332652546606733 ) ) ;
#52473 = CARTESIAN_POINT ( 'NONE',  ( -5.752737250900127997, 5.605948302338584099, 0.000000000000000000 ) ) ;
#52475 = DIRECTION ( 'NONE',  ( 1.000000000000000000, -0.000000000000000000, -0.000000000000000000 ) ) ;
#52476 = CARTESIAN_POINT ( 'NONE',  ( 5.138177029454829459, 8.938364267765221527, 0.7216878364870438212 ) ) ;
#52477 = CARTESIAN_POINT ( 'NONE',  ( -1.402160292154681736E-14, -0.4906249996585810846, -1.575800808251665908 ) ) ;
#52478 = CARTESIAN_POINT ( 'NONE',  ( 4.094199201646931741, 4.839282492418613302, -1.082531754730543083 ) ) ;
#52479 = CARTESIAN_POINT ( 'NONE',  ( -2.123823618835070537, 5.629544655282869847, 1.040834085586084257E-14 ) ) ;
#52480 = CARTESIAN_POINT ( 'NONE',  ( 3.766626874709140704, -1.453462046928340579, 1.600284095077113333 ) ) ;
#52481 = CARTESIAN_POINT ( 'NONE',  ( -4.800995793014949165, 8.615262501910491366, 0.7216878364870267237 ) ) ;
#52482 = CARTESIAN_POINT ( 'NONE',  ( 5.668717624289557833, 8.667235424096215723, -1.082531754730548412 ) ) ;
#52483 = CARTESIAN_POINT ( 'NONE',  ( 0.4750491441844888474, -1.531729482103380224, 1.466773057065169139 ) ) ;
#52484 = CARTESIAN_POINT ( 'NONE',  ( -3.621833129746846680, 4.096114899008192367, 2.500000000000011102 ) ) ;
#52485 = CARTESIAN_POINT ( 'NONE',  ( 1.967984887604894206, 1.010138386605848426, 1.692741100060575210 ) ) ;
#52486 = CARTESIAN_POINT ( 'NONE',  ( 4.886922752366290368, -1.802716094696995786, -0.6387714794457154399 ) ) ;
#52487 = ORIENTED_EDGE ( 'NONE', *, *, #103791, .F. ) ;
#52488 = CARTESIAN_POINT ( 'NONE',  ( 9.488968570712872364, -6.747343053191950268, -0.2633404184770131717 ) ) ;
#52489 = CARTESIAN_POINT ( 'NONE',  ( 6.549268392505379843, 1.714383406945050980, -0.9693629108104614422 ) ) ;
#52490 = CARTESIAN_POINT ( 'NONE',  ( 2.079929315299507753, -1.904492180933140322, -0.3787631973139488073 ) ) ;
#52491 = ORIENTED_EDGE ( 'NONE', *, *, #43078, .T. ) ;
#52492 = CARTESIAN_POINT ( 'NONE',  ( -4.285259070371116863, 7.157163461145040095, 1.199719254218452935 ) ) ;
#52494 = CARTESIAN_POINT ( 'NONE',  ( 6.908358566921232402, -6.724344753046858081, -6.684387857553371504 ) ) ;
#52493 = CARTESIAN_POINT ( 'NONE',  ( -3.984117037569407938, 5.741498858621315371, 1.599625672291270506 ) ) ;
#52496 = CARTESIAN_POINT ( 'NONE',  ( 6.061904078641523697, 7.205214525570814210, -1.082531754730548412 ) ) ;
#52495 = CARTESIAN_POINT ( 'NONE',  ( 7.121056995675668411, 9.330985799753529264, -1.599625672291262513 ) ) ;
#52497 = VERTEX_POINT ( 'NONE', #213839 ) ;
#52498 = CARTESIAN_POINT ( 'NONE',  ( 3.457846583235091753, 0.5364296187198510646, -2.140574738106671759 ) ) ;
#52499 = CARTESIAN_POINT ( 'NONE',  ( 2.415298318263587873, 1.970979330149217335, 0.9926799514654093270 ) ) ;
#52500 = CARTESIAN_POINT ( 'NONE',  ( -5.652456368805534481, 5.782309656923097840, 0.2304340072341204693 ) ) ;
#52501 = CARTESIAN_POINT ( 'NONE',  ( 1.014147342612067737, -1.912461472154961539, 0.0006945104691555297090 ) ) ;
#52502 = CARTESIAN_POINT ( 'NONE',  ( -0.02319159430947542733, 0.7471999394491578572, -1.895068635927643630 ) ) ;
#52503 = CARTESIAN_POINT ( 'NONE',  ( 0.3931996164520941694, -9.201308816822022507, -9.491928691057864853 ) ) ;
#52504 = CARTESIAN_POINT ( 'NONE',  ( -6.776370306708066060, -7.161464053357566861, -6.781144757626042185 ) ) ;
#52505 = CARTESIAN_POINT ( 'NONE',  ( 3.244645865714153032, -2.039272935636734285, -0.3565889006169955522 ) ) ;
#52506 = CARTESIAN_POINT ( 'NONE',  ( -3.764360206088648297, 7.543504007078730922, -0.7998128361456281477 ) ) ;
#52507 = CARTESIAN_POINT ( 'NONE',  ( -4.699286343732877569, 8.265425651823845143, 0.5948934201362279239 ) ) ;
#52509 = CARTESIAN_POINT ( 'NONE',  ( 0.9190830904215805397, 1.997680973563022544, 0.8264451868333838602 ) ) ;
#52508 = CARTESIAN_POINT ( 'NONE',  ( -3.846762897975357198, 5.510976019103107859, -1.599625672291256295 ) ) ;
#52510 = CARTESIAN_POINT ( 'NONE',  ( 3.017305944477025825, -2.111434807548946857, 0.5868732223921411251 ) ) ;
#52511 = CARTESIAN_POINT ( 'NONE',  ( -5.764847698752922689, 6.714788497190617989, 1.023463827431342343 ) ) ;
#52512 = CARTESIAN_POINT ( 'NONE',  ( 0.3561222683123154709, -6.532648913094854848, 9.473215147174819606 ) ) ;
#52513 = CARTESIAN_POINT ( 'NONE',  ( 1.364683531249996529, 13.52604166700806587, 0.7879004041258405033 ) ) ;
#52514 = CARTESIAN_POINT ( 'NONE',  ( -5.143339171537843590, 7.093924681584509173, 1.599625672291263179 ) ) ;
#52515 = UNCERTAINTY_MEASURE_WITH_UNIT (LENGTH_MEASURE( 1.000000000000000082E-05 ), #196720, 'distance_accuracy_value', 'NONE');
#52516 = CARTESIAN_POINT ( 'NONE',  ( 6.399014502872731214, -0.8263350558326795214, -1.524632933908439902 ) ) ;
#52517 = AXIS2_PLACEMENT_3D ( 'NONE', #8150, #41751, #91572 ) ;
#52518 = CARTESIAN_POINT ( 'NONE',  ( -8.839552966430002101, 12.29626697993494666, -1.082531754730543971 ) ) ;
#52519 = CARTESIAN_POINT ( 'NONE',  ( 3.643477671580112709, 1.873648065284461817, -0.8808079623299628347 ) ) ;
#52520 = CARTESIAN_POINT ( 'NONE',  ( 4.253586407750776566, 2.053249321966661434, -0.5160394917872836995 ) ) ;
#52521 = CARTESIAN_POINT ( 'NONE',  ( 6.962275575817444384, 8.081408578997208991, -1.199719254218446718 ) ) ;
#52522 = CARTESIAN_POINT ( 'NONE',  ( -0.6823417656250212460, 5.051041667008086655, 1.181850606188767472 ) ) ;
#52523 = CARTESIAN_POINT ( 'NONE',  ( 2.412896334679739851, -1.525488895468416706, 1.245673054583651407 ) ) ;
#52524 = CARTESIAN_POINT ( 'NONE',  ( 0.3340484552533556362, -1.024938778295768849, -1.614363347046356756 ) ) ;
#52525 = CARTESIAN_POINT ( 'NONE',  ( 4.769621702613293657, 1.317199799690757178, 1.875844486027035574 ) ) ;
#52526 = CARTESIAN_POINT ( 'NONE',  ( 3.176193443437186126, -1.086901434622984830, 1.466744820640853320 ) ) ;
#52527 = CARTESIAN_POINT ( 'NONE',  ( 3.878514461961128479, 6.682628084666728085, -1.199719254218448494 ) ) ;
#52529 = EDGE_CURVE ( 'NONE', #109340, #84638, #208451, .T. ) ;
#52528 = CARTESIAN_POINT ( 'NONE',  ( 6.127922243252466039, 6.251590159990418449, 1.040834085586084257E-14 ) ) ;
#52530 = CARTESIAN_POINT ( 'NONE',  ( -7.152089726408780379, 8.302858421353754181, -1.199719254218446718 ) ) ;
#52531 = CARTESIAN_POINT ( 'NONE',  ( 4.306893573823011856, -0.4451576889303583418, -1.963212451998196606 ) ) ;
#52532 = CARTESIAN_POINT ( 'NONE',  ( 4.539869136473917877, 1.278287603951251183, 1.488235606430035274 ) ) ;
#52533 = CARTESIAN_POINT ( 'NONE',  ( -7.477485413136760073, 8.682486722536401302, -1.199719254218446718 ) ) ;
#52534 = CARTESIAN_POINT ( 'NONE',  ( -4.629219384062206011, 7.488174150459498968, -1.199719254218452047 ) ) ;
#52535 = CARTESIAN_POINT ( 'NONE',  ( 0.07556134207193415664, 4.081186479400328082, -2.798928192855642649 ) ) ;
#52537 = CARTESIAN_POINT ( 'NONE',  ( 5.401144703012512593, 1.448466425555764658, 1.016686210146000358 ) ) ;
#52536 = CARTESIAN_POINT ( 'NONE',  ( 0.7145361118556601276, 1.933244891618046024, 0.7966077499205433954 ) ) ;
#52538 = CARTESIAN_POINT ( 'NONE',  ( 3.098963836025306229, 6.178100804120803424, 0.8152952010215334111 ) ) ;
#52539 = CARTESIAN_POINT ( 'NONE',  ( 1.500213180713722450, -0.7911926984936793472, -2.043816727864488314 ) ) ;
#52540 = CARTESIAN_POINT ( 'NONE',  ( 0.3271923042600047848, 0.8970799620377118977, -1.491255180049656071 ) ) ;
#52541 = AXIS2_PLACEMENT_3D ( 'NONE', #60853, #80303, #64057 ) ;
#52542 = CARTESIAN_POINT ( 'NONE',  ( 6.479907352327590964, 9.647310113435821677, 1.199719254218462483 ) ) ;
#52543 = SURFACE_SIDE_STYLE ('',( #126429 ) ) ;
#52544 = CARTESIAN_POINT ( 'NONE',  ( 0.6094340267816320544, -1.717071606940338446, 0.1640370458491739458 ) ) ;
#52545 = CARTESIAN_POINT ( 'NONE',  ( 1.265469760322552206, -2.298542322993640141, 0.001328286606278733300 ) ) ;
#52547 = EDGE_CURVE ( 'NONE', #201145, #181120, #183494, .T. ) ;
#52546 = CARTESIAN_POINT ( 'NONE',  ( 0.3280006606478855224, 1.121390616443746602, -1.882787531365101685 ) ) ;
#52548 = CARTESIAN_POINT ( 'NONE',  ( 6.837244271306878396, -1.062160112102826126, 1.370476690187643731 ) ) ;
#52549 = CARTESIAN_POINT ( 'NONE',  ( 2.455956380646412196, 0.5873987694336445520, -2.127207350628975924 ) ) ;
#52550 = CARTESIAN_POINT ( 'NONE',  ( 0.4444779246538512751, -1.024716592377757696, 1.914062593285012603 ) ) ;
#52551 = DIRECTION ( 'NONE',  ( 0.000000000000000000, 0.000000000000000000, 1.000000000000000000 ) ) ;
#52552 = CARTESIAN_POINT ( 'NONE',  ( 0.7786901736592425349, -0.5205582433389954744, -2.052224243718490992 ) ) ;
#52553 = CARTESIAN_POINT ( 'NONE',  ( 6.620655732516651071, -0.002413161512292844035, 2.173887093218453082 ) ) ;
#52554 = CARTESIAN_POINT ( 'NONE',  ( 5.895520149318425496, 1.459072380863110530, 1.257889585189754023 ) ) ;
#52555 = ORIENTED_EDGE ( 'NONE', *, *, #61890, .T. ) ;
#52557 = CARTESIAN_POINT ( 'NONE',  ( 1.364683531249988757, -0.8031249996585804185, 0.000000000000000000 ) ) ;
#52556 = CARTESIAN_POINT ( 'NONE',  ( 1.910137617552462030, -1.084854587848137708, -2.019442561568355110 ) ) ;
#52558 = CARTESIAN_POINT ( 'NONE',  ( 5.020596955762157698, 4.751784624677624080, 1.040834085586084257E-14 ) ) ;
#52559 = CARTESIAN_POINT ( 'NONE',  ( 6.491656622844908853, 6.468020902940851968, 0.7998128361456341429 ) ) ;
#52560 = CARTESIAN_POINT ( 'NONE',  ( 3.721504678736448302, 1.905620783811642571, 1.141157194635911365 ) ) ;
#52561 = CARTESIAN_POINT ( 'NONE',  ( -6.724481002698120768, 9.828683022247721723, -1.082531754730538864 ) ) ;
#52562 = CARTESIAN_POINT ( 'NONE',  ( 3.469446951953614189E-15, 0.2401923788623722134, 6.938893903907228378E-15 ) ) ;
#52563 = CARTESIAN_POINT ( 'NONE',  ( 5.178851490740196795, 7.065079377328788546, 1.443375672974062551 ) ) ;
#52564 = CARTESIAN_POINT ( 'NONE',  ( -7.985389288324697965, 10.33937347451072775, -1.443375672974058777 ) ) ;
#52565 = CARTESIAN_POINT ( 'NONE',  ( 4.746763178560250651, 7.591621904078704297, 1.082531754730549078 ) ) ;
#52566 = ORIENTED_EDGE ( 'NONE', *, *, #66641, .T. ) ;
#52567 = CARTESIAN_POINT ( 'NONE',  ( 1.758435621656749603, 1.928751379572872571, -0.5880216644931559600 ) ) ;
#52569 = CARTESIAN_POINT ( 'NONE',  ( 1.340767248851399307, -2.011434839998844204, -0.4557168523060088905 ) ) ;
#52568 = CARTESIAN_POINT ( 'NONE',  ( 8.613507663383630941, 8.943513783569379427, -0.7998128361456221525 ) ) ;
#52570 = FACE_OUTER_BOUND ( 'NONE', #103666, .T. ) ;
#52571 = CARTESIAN_POINT ( 'NONE',  ( 5.017926250389229459, 8.868348035513836436, 0.000000000000000000 ) ) ;
#52572 = EDGE_CURVE ( 'NONE', #23747, #166540, #80586, .T. ) ;
#52573 = CARTESIAN_POINT ( 'NONE',  ( -1.201851678989727383E-14, 3.946875000341423689, -1.575800808251660134 ) ) ;
#52574 = CARTESIAN_POINT ( 'NONE',  ( 3.978626637211603700, -0.2140425413966473567, -2.180973779111646138 ) ) ;
#52575 = CARTESIAN_POINT ( 'NONE',  ( 0.7916389524552720491, 1.525042296397002284, -1.319230309296010928 ) ) ;
#52576 = CARTESIAN_POINT ( 'NONE',  ( 0.7492455685023796663, 1.839184785914184994, -0.09005233288367914257 ) ) ;
#52577 = CARTESIAN_POINT ( 'NONE',  ( 5.372717881723642286, -0.05365108595901035143, -2.291914610307096201 ) ) ;
#52578 = CARTESIAN_POINT ( 'NONE',  ( 2.835703941817575569, 1.827261480098177682, 0.2250241719141123087 ) ) ;
#52579 = ADVANCED_FACE ( 'NONE', ( #65457 ), #99067, .T. ) ;
#52580 = CARTESIAN_POINT ( 'NONE',  ( 9.121938423896107651, 9.536683004167278099, -0.7998128361456221525 ) ) ;
#52581 = CARTESIAN_POINT ( 'NONE',  ( 4.612205747861584548, -0.7811881352849485705, -1.650120847746315622 ) ) ;
#52582 = CARTESIAN_POINT ( 'NONE',  ( 4.588517629802620235, -0.5350896943857390564, 1.944070981013111155 ) ) ;
#52583 = CARTESIAN_POINT ( 'NONE',  ( -7.492852449846775897, 11.89341162479659531, 0.000000000000000000 ) ) ;
#52585 = CARTESIAN_POINT ( 'NONE',  ( -5.986807348886189040, 9.142303119412650503, -1.199719254218452047 ) ) ;
#52584 = CARTESIAN_POINT ( 'NONE',  ( 4.223666230214691453, -2.166182250408314580, 0.6532043330096364286 ) ) ;
#52586 = CARTESIAN_POINT ( 'NONE',  ( 6.493207903183886742, 1.834288230482609583, -1.034473908808232201 ) ) ;
#52587 = PRESENTATION_STYLE_ASSIGNMENT (( #135982 ) ) ;
#52588 =( BOUNDED_SURFACE ( )  B_SPLINE_SURFACE ( 1, 2, ( 
 ( #105439, #167214, #35055, #154168, #137923, #184506, #83812, #67539, #70742, #203944, #101126, #18802, #55591, #2538, #51330, #134738, #174705, #25216, #7891, #76108, #206097, #190910, #11093, #205020, #208226, #122830, #89181, #56666, #123888, #73979, #189854, #140073, #138998, #108677, #155233, #26281, #142212, #91320, #110811, #6814, #126010, #191971, #209282, #41499, #141161, #188791, #107612, #8972, #157378, #173643, #59858, #109752, #57731, #43637, #24139, #207169, #75046, #23065, #58793, #124948, #90241, #42574, #143291, #156307, #92395, #158433, #10034, #40426, #175762, #27355, #93457, #159494, #77170, #60929, #106529, #127086, #193049, #172555, #44703, #72892, #14285, #78242, #178964, #154, #97719, #63062, #112953, #62005, #82498, #28431, #148585, #144364, #180021, #129229, #80380, #30579, #46839, #13242, #47915, #98772, #96660, #79315, #146476, #195202, #114025, #164828, #162713, #212495, #31642, #210365, #45772, #81449, #64136, #130280, #196268, #163777, #128161, #15356, #145431, #211431, #65170, #16418, #50010, #147526, #48959, #213547, #131325, #66220, #197318, #115077, #181073, #161647, #32691, #132368, #198370, #177893, #176816, #94524, #111889, #194122, #160562, #12170, #29506, #95599, #33752, #69431, #68363, #135536, #51079, #83564, #35882, #149646, #99829, #119337, #53206, #201560, #54279, #137673, #104099, #21735, #199436, #20682, #182123, #1228, #203695, #120417, #86773, #71566, #185324, #186391, #36948, #100882, #165895, #166969, #152844, #200500, #153915, #103028, #184255, #67290, #169083, #4418, #38028, #19628, #70489, #3361, #34807, #85699, #116134, #18559, #17480, #133429, #118271, #151787, #117204, #183201, #136605, #101957, #202629, #170149, #87844, #84636, #168024, #5485, #150727, #2287, #134497, #52143, #141959, #39094, #9780, #191717, #73717, #138740, #156044, #190650, #76905, #55341, #143029, #105180, #121493, #108426, #74795, #43374, #10831, #8710, #207971, #158188, #93199, #174447, #206906, #92133, #140896, #189599, #124692, #159230, #125754, #139815, #41245, #109495, #122571, #205844, #88925, #107352, #157121, #187465, #175502, #57477, #75852, #172298, #171216, #7632, #59597, #123636, #58537, #42310, #173374, #27092, #26023, #24959, #23886, #56409, #89992, #154978, #22810, #6563, #72644, #204758, #188533, #91060, #40163, #106277, #64920, #79044, #194930, #131069, #61738, #145160, #28168, #46568, #96397, #60661, #197057, #211165, #97454, #111622, #32435, #161383, #163509, #12968, #162447, #80109, #62790, #81184, #47646, #178697, #177634, #210098, #29243, #94264, #82235, #98503, #77980, #160303, #179762, #113757, #95334, #209025, #126824, #14023, #128952, #146214, #144104, #176558, #112687, #11907, #192781, #212231, #63865, #130020, #147262, #16150, #48696, #114810, #127905, #31378, #44439, #193857, #110557, #213294, #15094, #164565, #196011, #180809, #45506, #30311, #198115, #133165, #119075, #18290, #186130, #167763, #2025, #33494, #151525, #3094, #152575, #51888, #102769, #35614, #67028, #118011, #169886, #199165, #21475, #49746, #150464, #184000, #148326, #214325, #69164, #68094, #185056, #19360, #36682, #115873, #134229, #101692, #132107, #202365, #168824, #182937, #20428, #181858, #86511, #70232, #166699, #17219, #34553, #135284, #65957, #99567, #165631, #83295, #149380, #201298, #85440, #136344, #103837, #52939, #4162, #54014, #37765, #120154, #963, #100624, #50811, #84377, #116937, #200238, #173117, #153656, #24699, #206652, #89740, #175252, #5225, #190398, #42055, #59346, #39910, #205582, #55085, #106019, #73453, #7374, #172040, #124440, #174195, #72379, #108169, #88662, #57219, #155790, #87584, #139555, #23633, #154722, #123379, #207722, #6304, #138478, #189344, #40984, #121234, #204500, #58284, #122312, #107095, #90801, #125499, #104916, #188269, #25768, #203431, #170957, #187204, #156865, #38833, #8451, #191463, #74539, #140639, #91880, #22557, #43128, #71299, #109244, #56150, #157935, #9528, #75601, #141712, #137411, #77725, #112431, #163257, #28986, #143848, #78784, #193608, #178444, #14839, #45250, #144906, #30051, #142771, #110302, #145964, #210913, #62540 ),
 ( #209840, #27914, #61479, #126568, #114565, #130818, #176310, #60407, #211974, #79855, #127644, #26838, #158986, #194671, #111368, #46315, #94010, #208776, #161120, #192528, #10582, #96142, #162193, #13780, #179510, #48452, #80929, #63614, #128702, #129769, #195752, #47389, #44182, #113501, #177372, #95072, #31130, #147020, #92941, #97205, #213043, #12708, #64672, #196808, #76656, #160049, #11653, #165370, #167510, #69974, #183751, #181609, #35361, #180557, #131854, #65705, #184801, #197861, #182677, #34298, #117761, #100371, #16963, #19107, #149118, #133981, #168569, #148073, #151269, #49493, #32179, #214079, #66765, #83044, #132906, #701, #81985, #51637, #98255, #101436, #85185, #166441, #53761, #164312, #68910, #135030, #152326, #198911, #84120, #115614, #50557, #18032, #150206, #116678, #2841, #52686, #1778, #201043, #33238, #67835, #199989, #15903, #118816, #36431, #99320, #102507, #86256, #20169, #3904, #136085, #202102, #153394, #186947, #90546, #154469, #171775, #39640, #157676, #137158, #6046, #58024, #21222, #203183, #4965, #23371, #87327, #122048, #9274, #40727, #72118, #55891, #71043, #25517, #185870, #91625, #54829, #123136, #138226, #89480, #188012, #204239, #170703, #205324, #41805, #105748, #22288, #155536, #7115, #56961, #107919, #73188, #139294, #189094, #120979, #38580, #106833, #104655, #169639, #88401, #156610, #172863, #75345, #24435, #8200, #74285, #140379, #206399, #124188, #190151, #173944, #141461, #207468, #119895, #37505, #103581, #149682, #177925, #64170, #97753, #59087, #128195, #65204, #130313, #32724, #81482, #98806, #111925, #196301, #163812, #45804, #116170, #164859, #96701, #148619, #29540, #16452, #198405, #80414, #145466, #162748, #197351, #83600, #194156, #95631, #161681, #13275, #115111, #147559, #50047, #17513, #15388, #187, #82533, #99865, #181108, #213581, #66255, #131356, #47947, #48993, #165928, #132403, #146512, #114062, #182156, #129265, #212529, #79349, #180054, #33786, #211461, #63096, #31676, #195235, #178997, #46873, #14321, #112987, #30612, #169118, #86808, #168060, #87876, #54313, #185359, #118304, #2323, #184291, #100915, #88959, #105211, #84672, #34840, #186425, #120451, #101991, #1263, #133465, #20715, #19662, #152874, #150761, #183236, #135570, #167003, #199469, #4452, #70522, #136638, #153948, #22844, #203726, #121528, #68399, #38064, #67321, #18594, #51111, #5517, #104134, #171248, #202663, #71597, #117236, #3396, #36981, #134527, #200533, #170180, #69465, #21768, #137706, #55374, #52179, #201594, #103064, #35916, #187498, #39128, #85737, #151822, #53242, #119371, #76941, #173414, #23921, #41283, #75888, #176595, #155012, #28206, #204792, #6597, #208010, #174483, #143066, #110592, #108463, #93234, #43409, #192818, #59634, #92173, #191754, #26059, #74832, #9813, #44476, #10867, #24995, #140931, #209060, #7669, #91098, #188567, #206945, #42348, #72678, #60696, #157158, #109533, #57513, #138774, #107392, #175538, #8750, #158224, #141996, #58574, #27128, #125792, #124730, #123671, #156083, #189634, #40199, #56445, #122604, #90027, #106310, #159267, #126861, #190689, #172333, #73754, #139849, #205878, #145197, #210133, #11944, #95369, #78016, #160341, #211204, #62829, #128989, #112724, #80146, #96434, #162485, #61775, #194968, #94300, #127943, #144141, #193896, #45543, #111657, #177669, #29278, #161420, #46604, #79079, #178735, #13003, #30349, #14058, #92859, #141629, #173033, #76575, #142687, #77645, #191380, #27833, #175171, #206573, #43046, #94993, #124359, #161039, #75517, #190316, #125414, #25687, #158906, #61402, #91795, #109159, #208697, #189264, #156786, #192448, #26758, #10502, #60324, #126484, #107009, #44103, #41974, #108085, #176231, #127565, #73367, #110223, #159970, #9446, #174114, #193534, #93929, #11575, #143767, #58200, #209761, #177294, #45176, #74455, #111288, #139472, #24615, #90724, #28908, #8372, #207638, #59256, #205501, #57134, #157852, #123301, #40903, #140559, #3285, #165820, #149570, #104024, #21658, #199357, #20608, #182045, #1153, #137601, #54201, #86696, #71488, #53127, #120341, #135462, #100806, #17403, #166892, #152765 ) ),
 .UNSPECIFIED., .F., .F., .F. ) 
 B_SPLINE_SURFACE_WITH_KNOTS ( ( 2, 2 ),
 ( 3, 2, 2, 2, 2, 2, 2, 2, 2, 2, 2, 2, 2, 2, 2, 2, 2, 2, 2, 2, 2, 2, 2, 2, 2, 2, 2, 2, 2, 2, 2, 2, 2, 2, 2, 2, 2, 2, 2, 2, 2, 2, 2, 2, 2, 2, 2, 2, 2, 2, 2, 2, 2, 2, 2, 2, 2, 2, 2, 2, 2, 2, 2, 2, 2, 2, 2, 2, 2, 2, 2, 2, 2, 2, 2, 2, 2, 2, 2, 2, 2, 2, 2, 2, 2, 2, 2, 2, 2, 2, 2, 2, 2, 2, 2, 2, 2, 2, 2, 2, 2, 2, 2, 2, 2, 2, 2, 2, 2, 2, 2, 2, 2, 2, 2, 2, 2, 2, 2, 2, 2, 2, 2, 2, 2, 2, 2, 2, 2, 2, 2, 2, 2, 2, 2, 2, 2, 2, 2, 2, 2, 2, 2, 2, 2, 2, 2, 2, 2, 2, 2, 2, 2, 2, 2, 2, 2, 2, 2, 2, 2, 2, 2, 2, 2, 2, 2, 2, 2, 2, 2, 2, 2, 2, 2, 2, 2, 2, 2, 2, 2, 2, 2, 2, 2, 2, 2, 2, 2, 2, 2, 2, 2, 2, 2, 2, 2, 2, 2, 2, 2, 2, 2, 2, 2, 2, 2, 2, 2, 2, 2, 2, 2, 2, 2, 2, 2, 2, 2, 2, 2, 2, 2, 2, 2, 2, 2, 2, 2, 2, 2, 2, 2, 2, 2, 2, 2, 2, 2, 2, 3 ),
 ( 0.000000000000000000, 1.000000000000000000 ),
 ( 0.000000000000000000, 0.004166666666666666609, 0.008333333333333333218, 0.01250000000000000069, 0.01666666666666666644, 0.02083333333333333218, 0.02500000000000000139, 0.02916666666666666713, 0.03333333333333333287, 0.03749999999999999861, 0.04166666666666666435, 0.04583333333333333010, 0.05000000000000000278, 0.05416666666666666852, 0.05833333333333333426, 0.06250000000000000000, 0.06666666666666666574, 0.07083333333333333148, 0.07499999999999999722, 0.07916666666666666297, 0.08333333333333332871, 0.08749999999999999445, 0.09166666666666666019, 0.09583333333333333981, 0.1000000000000000056, 0.1041666666666666713, 0.1083333333333333370, 0.1125000000000000028, 0.1166666666666666685, 0.1208333333333333343, 0.1250000000000000000, 0.1291666666666666796, 0.1333333333333333315, 0.1375000000000000111, 0.1416666666666666630, 0.1458333333333333426, 0.1499999999999999944, 0.1541666666666666741, 0.1583333333333333259, 0.1625000000000000056, 0.1666666666666666574, 0.1708333333333333370, 0.1749999999999999889, 0.1791666666666666685, 0.1833333333333333204, 0.1875000000000000000, 0.1916666666666666796, 0.1958333333333333315, 0.2000000000000000111, 0.2041666666666666630, 0.2083333333333333426, 0.2124999999999999944, 0.2166666666666666741, 0.2208333333333333259, 0.2250000000000000056, 0.2291666666666666574, 0.2333333333333333370, 0.2374999999999999889, 0.2416666666666666685, 0.2458333333333333204, 0.2500000000000000000, 0.2541666666666666519, 0.2583333333333333592, 0.2625000000000000111, 0.2666666666666666630, 0.2708333333333333148, 0.2750000000000000222, 0.2791666666666666741, 0.2833333333333333259, 0.2874999999999999778, 0.2916666666666666852, 0.2958333333333333370, 0.2999999999999999889, 0.3041666666666666408, 0.3083333333333333481, 0.3125000000000000000, 0.3166666666666666519, 0.3208333333333333592, 0.3250000000000000111, 0.3291666666666666630, 0.3333333333333333148, 0.3375000000000000222, 0.3416666666666666741, 0.3458333333333333259, 0.3499999999999999778, 0.3541666666666666852, 0.3583333333333333370, 0.3624999999999999889, 0.3666666666666666408, 0.3708333333333333481, 0.3750000000000000000, 0.3791666666666666519, 0.3833333333333333592, 0.3875000000000000111, 0.3916666666666666630, 0.3958333333333333148, 0.4000000000000000222, 0.4041666666666666741, 0.4083333333333333259, 0.4124999999999999778, 0.4166666666666666852, 0.4208333333333333370, 0.4249999999999999889, 0.4291666666666666408, 0.4333333333333333481, 0.4375000000000000000, 0.4416666666666666519, 0.4458333333333333592, 0.4500000000000000111, 0.4541666666666666630, 0.4583333333333333148, 0.4625000000000000222, 0.4666666666666666741, 0.4708333333333333259, 0.4749999999999999778, 0.4791666666666666852, 0.4833333333333333370, 0.4874999999999999889, 0.4916666666666666408, 0.4958333333333333481, 0.5000000000000000000, 0.5041666666666666519, 0.5083333333333333037, 0.5124999999999999556, 0.5166666666666667185, 0.5208333333333333703, 0.5250000000000000222, 0.5291666666666666741, 0.5333333333333333259, 0.5374999999999999778, 0.5416666666666666297, 0.5458333333333332815, 0.5500000000000000444, 0.5541666666666666963, 0.5583333333333333481, 0.5625000000000000000, 0.5666666666666666519, 0.5708333333333333037, 0.5749999999999999556, 0.5791666666666667185, 0.5833333333333333703, 0.5875000000000000222, 0.5916666666666666741, 0.5958333333333333259, 0.5999999999999999778, 0.6041666666666666297, 0.6083333333333332815, 0.6125000000000000444, 0.6166666666666666963, 0.6208333333333333481, 0.6250000000000000000, 0.6291666666666666519, 0.6333333333333333037, 0.6374999999999999556, 0.6416666666666667185, 0.6458333333333333703, 0.6500000000000000222, 0.6541666666666666741, 0.6583333333333333259, 0.6624999999999999778, 0.6666666666666666297, 0.6708333333333332815, 0.6750000000000000444, 0.6791666666666666963, 0.6833333333333333481, 0.6875000000000000000, 0.6916666666666666519, 0.6958333333333333037, 0.6999999999999999556, 0.7041666666666667185, 0.7083333333333333703, 0.7125000000000000222, 0.7166666666666666741, 0.7208333333333333259, 0.7249999999999999778, 0.7291666666666666297, 0.7333333333333332815, 0.7375000000000000444, 0.7416666666666666963, 0.7458333333333333481, 0.7500000000000000000, 0.7541666666666666519, 0.7583333333333333037, 0.7624999999999999556, 0.7666666666666667185, 0.7708333333333333703, 0.7750000000000000222, 0.7791666666666666741, 0.7833333333333333259, 0.7874999999999999778, 0.7916666666666666297, 0.7958333333333332815, 0.8000000000000000444, 0.8041666666666666963, 0.8083333333333333481, 0.8125000000000000000, 0.8166666666666666519, 0.8208333333333333037, 0.8249999999999999556, 0.8291666666666667185, 0.8333333333333333703, 0.8375000000000000222, 0.8416666666666666741, 0.8458333333333333259, 0.8499999999999999778, 0.8541666666666666297, 0.8583333333333332815, 0.8625000000000000444, 0.8666666666666666963, 0.8708333333333333481, 0.8750000000000000000, 0.8791666666666666519, 0.8833333333333333037, 0.8874999999999999556, 0.8916666666666667185, 0.8958333333333333703, 0.9000000000000000222, 0.9041666666666666741, 0.9083333333333333259, 0.9124999999999999778, 0.9166666666666666297, 0.9208333333333332815, 0.9250000000000000444, 0.9291666666666666963, 0.9333333333333333481, 0.9375000000000000000, 0.9416666666666666519, 0.9458333333333333037, 0.9499999999999999556, 0.9541666666666667185, 0.9583333333333333703, 0.9625000000000000222, 0.9666666666666666741, 0.9708333333333333259, 0.9749999999999999778, 0.9791666666666666297, 0.9833333333333332815, 0.9875000000000000444, 0.9916666666666666963, 0.9958333333333333481, 1.000000000000000000 ),
 .UNSPECIFIED. ) 
 GEOMETRIC_REPRESENTATION_ITEM ( )  RATIONAL_B_SPLINE_SURFACE ( (
 ( 1.000000000000000000, 0.8660254037844387076, 1.000000000000000000, 0.8660254037844387076, 1.000000000000000000, 0.8660254037844387076, 1.000000000000000000, 0.8660254037844387076, 1.000000000000000000, 0.8660254037844387076, 1.000000000000000000, 0.8660254037844387076, 1.000000000000000000, 0.8660254037844387076, 1.000000000000000000, 0.8660254037844387076, 1.000000000000000000, 0.8660254037844387076, 1.000000000000000000, 0.8660254037844387076, 1.000000000000000000, 0.8660254037844387076, 1.000000000000000000, 0.8660254037844387076, 1.000000000000000000, 0.8660254037844387076, 1.000000000000000000, 0.8660254037844387076, 1.000000000000000000, 0.8660254037844387076, 1.000000000000000000, 0.8660254037844387076, 1.000000000000000000, 0.8660254037844387076, 1.000000000000000000, 0.8660254037844387076, 1.000000000000000000, 0.8660254037844387076, 1.000000000000000000, 0.8660254037844387076, 1.000000000000000000, 0.8660254037844387076, 1.000000000000000000, 0.8660254037844387076, 1.000000000000000000, 0.8660254037844387076, 1.000000000000000000, 0.8660254037844387076, 1.000000000000000000, 0.8660254037844387076, 1.000000000000000000, 0.8660254037844387076, 1.000000000000000000, 0.8660254037844387076, 1.000000000000000000, 0.8660254037844387076, 1.000000000000000000, 0.8660254037844387076, 1.000000000000000000, 0.8660254037844387076, 1.000000000000000000, 0.8660254037844387076, 1.000000000000000000, 0.8660254037844387076, 1.000000000000000000, 0.8660254037844387076, 1.000000000000000000, 0.8660254037844387076, 1.000000000000000000, 0.8660254037844387076, 1.000000000000000000, 0.8660254037844387076, 1.000000000000000000, 0.8660254037844387076, 1.000000000000000000, 0.8660254037844387076, 1.000000000000000000, 0.8660254037844387076, 1.000000000000000000, 0.8660254037844387076, 1.000000000000000000, 0.8660254037844387076, 1.000000000000000000, 0.8660254037844387076, 1.000000000000000000, 0.8660254037844387076, 1.000000000000000000, 0.8660254037844387076, 1.000000000000000000, 0.8660254037844387076, 1.000000000000000000, 0.8660254037844387076, 1.000000000000000000, 0.8660254037844387076, 1.000000000000000000, 0.8660254037844387076, 1.000000000000000000, 0.8660254037844387076, 1.000000000000000000, 0.8660254037844387076, 1.000000000000000000, 0.8660254037844387076, 1.000000000000000000, 0.8660254037844387076, 1.000000000000000000, 0.8660254037844387076, 1.000000000000000000, 0.8660254037844387076, 1.000000000000000000, 0.8660254037844387076, 1.000000000000000000, 0.8660254037844387076, 1.000000000000000000, 0.8660254037844387076, 1.000000000000000000, 0.8660254037844387076, 1.000000000000000000, 0.8660254037844387076, 1.000000000000000000, 0.8660254037844387076, 1.000000000000000000, 0.8660254037844387076, 1.000000000000000000, 0.8660254037844387076, 1.000000000000000000, 0.8660254037844387076, 1.000000000000000000, 0.8660254037844387076, 1.000000000000000000, 0.8660254037844387076, 1.000000000000000000, 0.8660254037844387076, 1.000000000000000000, 0.8660254037844387076, 1.000000000000000000, 0.8660254037844387076, 1.000000000000000000, 0.8660254037844387076, 1.000000000000000000, 0.8660254037844387076, 1.000000000000000000, 0.8660254037844387076, 1.000000000000000000, 0.8660254037844387076, 1.000000000000000000, 0.8660254037844387076, 1.000000000000000000, 0.8660254037844387076, 1.000000000000000000, 0.8660254037844387076, 1.000000000000000000, 0.8660254037844387076, 1.000000000000000000, 0.8660254037844387076, 1.000000000000000000, 0.8660254037844387076, 1.000000000000000000, 0.8660254037844387076, 1.000000000000000000, 0.8660254037844387076, 1.000000000000000000, 0.8660254037844387076, 1.000000000000000000, 0.8660254037844387076, 1.000000000000000000, 0.8660254037844387076, 1.000000000000000000, 0.8660254037844387076, 1.000000000000000000, 0.8660254037844387076, 1.000000000000000000, 0.8660254037844387076, 1.000000000000000000, 0.8660254037844387076, 1.000000000000000000, 0.8660254037844387076, 1.000000000000000000, 0.8660254037844387076, 1.000000000000000000, 0.8660254037844387076, 1.000000000000000000, 0.8660254037844387076, 1.000000000000000000, 0.8660254037844387076, 1.000000000000000000, 0.8660254037844387076, 1.000000000000000000, 0.8660254037844387076, 1.000000000000000000, 0.8660254037844387076, 1.000000000000000000, 0.8660254037844387076, 1.000000000000000000, 0.8660254037844387076, 1.000000000000000000, 0.8660254037844387076, 1.000000000000000000, 0.8660254037844387076, 1.000000000000000000, 0.8660254037844387076, 1.000000000000000000, 0.8660254037844387076, 1.000000000000000000, 0.8660254037844387076, 1.000000000000000000, 0.8660254037844387076, 1.000000000000000000, 0.8660254037844387076, 1.000000000000000000, 0.8660254037844387076, 1.000000000000000000, 0.8660254037844387076, 1.000000000000000000, 0.8660254037844387076, 1.000000000000000000, 0.8660254037844387076, 1.000000000000000000, 0.8660254037844387076, 1.000000000000000000, 0.8660254037844387076, 1.000000000000000000, 0.8660254037844387076, 1.000000000000000000, 0.8660254037844387076, 1.000000000000000000, 0.8660254037844387076, 1.000000000000000000, 0.8660254037844387076, 1.000000000000000000, 0.8660254037844387076, 1.000000000000000000, 0.8660254037844387076, 1.000000000000000000, 0.8660254037844387076, 1.000000000000000000, 0.8660254037844387076, 1.000000000000000000, 0.8660254037844387076, 1.000000000000000000, 0.8660254037844387076, 1.000000000000000000, 0.8660254037844387076, 1.000000000000000000, 0.8660254037844387076, 1.000000000000000000, 0.8660254037844387076, 1.000000000000000000, 0.8660254037844387076, 1.000000000000000000, 0.8660254037844387076, 1.000000000000000000, 0.8660254037844387076, 1.000000000000000000, 0.8660254037844387076, 1.000000000000000000, 0.8660254037844387076, 1.000000000000000000, 0.8660254037844387076, 1.000000000000000000, 0.8660254037844387076, 1.000000000000000000, 0.8660254037844387076, 1.000000000000000000, 0.8660254037844387076, 1.000000000000000000, 0.8660254037844387076, 1.000000000000000000, 0.8660254037844387076, 1.000000000000000000, 0.8660254037844387076, 1.000000000000000000, 0.8660254037844387076, 1.000000000000000000, 0.8660254037844387076, 1.000000000000000000, 0.8660254037844387076, 1.000000000000000000, 0.8660254037844387076, 1.000000000000000000, 0.8660254037844387076, 1.000000000000000000, 0.8660254037844387076, 1.000000000000000000, 0.8660254037844387076, 1.000000000000000000, 0.8660254037844387076, 1.000000000000000000, 0.8660254037844387076, 1.000000000000000000, 0.8660254037844387076, 1.000000000000000000, 0.8660254037844387076, 1.000000000000000000, 0.8660254037844387076, 1.000000000000000000, 0.8660254037844387076, 1.000000000000000000, 0.8660254037844387076, 1.000000000000000000, 0.8660254037844387076, 1.000000000000000000, 0.8660254037844387076, 1.000000000000000000, 0.8660254037844387076, 1.000000000000000000, 0.8660254037844387076, 1.000000000000000000, 0.8660254037844387076, 1.000000000000000000, 0.8660254037844387076, 1.000000000000000000, 0.8660254037844387076, 1.000000000000000000, 0.8660254037844387076, 1.000000000000000000, 0.8660254037844387076, 1.000000000000000000, 0.8660254037844387076, 1.000000000000000000, 0.8660254037844387076, 1.000000000000000000, 0.8660254037844387076, 1.000000000000000000, 0.8660254037844387076, 1.000000000000000000, 0.8660254037844387076, 1.000000000000000000, 0.8660254037844387076, 1.000000000000000000, 0.8660254037844387076, 1.000000000000000000, 0.8660254037844387076, 1.000000000000000000, 0.8660254037844387076, 1.000000000000000000, 0.8660254037844387076, 1.000000000000000000, 0.8660254037844387076, 1.000000000000000000, 0.8660254037844387076, 1.000000000000000000, 0.8660254037844387076, 1.000000000000000000, 0.8660254037844387076, 1.000000000000000000, 0.8660254037844387076, 1.000000000000000000, 0.8660254037844387076, 1.000000000000000000, 0.8660254037844387076, 1.000000000000000000, 0.8660254037844387076, 1.000000000000000000, 0.8660254037844387076, 1.000000000000000000, 0.8660254037844387076, 1.000000000000000000, 0.8660254037844387076, 1.000000000000000000, 0.8660254037844387076, 1.000000000000000000, 0.8660254037844387076, 1.000000000000000000, 0.8660254037844387076, 1.000000000000000000, 0.8660254037844387076, 1.000000000000000000, 0.8660254037844387076, 1.000000000000000000, 0.8660254037844387076, 1.000000000000000000, 0.8660254037844387076, 1.000000000000000000, 0.8660254037844387076, 1.000000000000000000, 0.8660254037844387076, 1.000000000000000000, 0.8660254037844387076, 1.000000000000000000, 0.8660254037844387076, 1.000000000000000000, 0.8660254037844387076, 1.000000000000000000, 0.8660254037844387076, 1.000000000000000000, 0.8660254037844387076, 1.000000000000000000, 0.8660254037844387076, 1.000000000000000000, 0.8660254037844387076, 1.000000000000000000, 0.8660254037844387076, 1.000000000000000000, 0.8660254037844387076, 1.000000000000000000, 0.8660254037844387076, 1.000000000000000000, 0.8660254037844387076, 1.000000000000000000, 0.8660254037844387076, 1.000000000000000000, 0.8660254037844387076, 1.000000000000000000, 0.8660254037844387076, 1.000000000000000000, 0.8660254037844387076, 1.000000000000000000, 0.8660254037844387076, 1.000000000000000000, 0.8660254037844387076, 1.000000000000000000, 0.8660254037844387076, 1.000000000000000000, 0.8660254037844387076, 1.000000000000000000, 0.8660254037844387076, 1.000000000000000000, 0.8660254037844387076, 1.000000000000000000, 0.8660254037844387076, 1.000000000000000000, 0.8660254037844387076, 1.000000000000000000, 0.8660254037844387076, 1.000000000000000000, 0.8660254037844387076, 1.000000000000000000, 0.8660254037844387076, 1.000000000000000000, 0.8660254037844387076, 1.000000000000000000, 0.8660254037844387076, 1.000000000000000000, 0.8660254037844387076, 1.000000000000000000, 0.8660254037844387076, 1.000000000000000000, 0.8660254037844387076, 1.000000000000000000, 0.8660254037844387076, 1.000000000000000000, 0.8660254037844387076, 1.000000000000000000, 0.8660254037844387076, 1.000000000000000000, 0.8660254037844387076, 1.000000000000000000, 0.8660254037844387076, 1.000000000000000000, 0.8660254037844387076, 1.000000000000000000, 0.8660254037844387076, 1.000000000000000000, 0.8660254037844387076, 1.000000000000000000, 0.8660254037844387076, 1.000000000000000000, 0.8660254037844387076, 1.000000000000000000, 0.8660254037844387076, 1.000000000000000000, 0.8660254037844387076, 1.000000000000000000, 0.8660254037844387076, 1.000000000000000000, 0.8660254037844387076, 1.000000000000000000, 0.8660254037844387076, 1.000000000000000000, 0.8660254037844387076, 1.000000000000000000, 0.8660254037844387076, 1.000000000000000000, 0.8660254037844387076, 1.000000000000000000, 0.8660254037844387076, 1.000000000000000000, 0.8660254037844387076, 1.000000000000000000, 0.8660254037844387076, 1.000000000000000000),
 ( 1.000000000000000000, 0.8660254037844387076, 1.000000000000000000, 0.8660254037844387076, 1.000000000000000000, 0.8660254037844387076, 1.000000000000000000, 0.8660254037844387076, 1.000000000000000000, 0.8660254037844387076, 1.000000000000000000, 0.8660254037844387076, 1.000000000000000000, 0.8660254037844387076, 1.000000000000000000, 0.8660254037844387076, 1.000000000000000000, 0.8660254037844387076, 1.000000000000000000, 0.8660254037844387076, 1.000000000000000000, 0.8660254037844387076, 1.000000000000000000, 0.8660254037844387076, 1.000000000000000000, 0.8660254037844387076, 1.000000000000000000, 0.8660254037844387076, 1.000000000000000000, 0.8660254037844387076, 1.000000000000000000, 0.8660254037844387076, 1.000000000000000000, 0.8660254037844387076, 1.000000000000000000, 0.8660254037844387076, 1.000000000000000000, 0.8660254037844387076, 1.000000000000000000, 0.8660254037844387076, 1.000000000000000000, 0.8660254037844387076, 1.000000000000000000, 0.8660254037844387076, 1.000000000000000000, 0.8660254037844387076, 1.000000000000000000, 0.8660254037844387076, 1.000000000000000000, 0.8660254037844387076, 1.000000000000000000, 0.8660254037844387076, 1.000000000000000000, 0.8660254037844387076, 1.000000000000000000, 0.8660254037844387076, 1.000000000000000000, 0.8660254037844387076, 1.000000000000000000, 0.8660254037844387076, 1.000000000000000000, 0.8660254037844387076, 1.000000000000000000, 0.8660254037844387076, 1.000000000000000000, 0.8660254037844387076, 1.000000000000000000, 0.8660254037844387076, 1.000000000000000000, 0.8660254037844387076, 1.000000000000000000, 0.8660254037844387076, 1.000000000000000000, 0.8660254037844387076, 1.000000000000000000, 0.8660254037844387076, 1.000000000000000000, 0.8660254037844387076, 1.000000000000000000, 0.8660254037844387076, 1.000000000000000000, 0.8660254037844387076, 1.000000000000000000, 0.8660254037844387076, 1.000000000000000000, 0.8660254037844387076, 1.000000000000000000, 0.8660254037844387076, 1.000000000000000000, 0.8660254037844387076, 1.000000000000000000, 0.8660254037844387076, 1.000000000000000000, 0.8660254037844387076, 1.000000000000000000, 0.8660254037844387076, 1.000000000000000000, 0.8660254037844387076, 1.000000000000000000, 0.8660254037844387076, 1.000000000000000000, 0.8660254037844387076, 1.000000000000000000, 0.8660254037844387076, 1.000000000000000000, 0.8660254037844387076, 1.000000000000000000, 0.8660254037844387076, 1.000000000000000000, 0.8660254037844387076, 1.000000000000000000, 0.8660254037844387076, 1.000000000000000000, 0.8660254037844387076, 1.000000000000000000, 0.8660254037844387076, 1.000000000000000000, 0.8660254037844387076, 1.000000000000000000, 0.8660254037844387076, 1.000000000000000000, 0.8660254037844387076, 1.000000000000000000, 0.8660254037844387076, 1.000000000000000000, 0.8660254037844387076, 1.000000000000000000, 0.8660254037844387076, 1.000000000000000000, 0.8660254037844387076, 1.000000000000000000, 0.8660254037844387076, 1.000000000000000000, 0.8660254037844387076, 1.000000000000000000, 0.8660254037844387076, 1.000000000000000000, 0.8660254037844387076, 1.000000000000000000, 0.8660254037844387076, 1.000000000000000000, 0.8660254037844387076, 1.000000000000000000, 0.8660254037844387076, 1.000000000000000000, 0.8660254037844387076, 1.000000000000000000, 0.8660254037844387076, 1.000000000000000000, 0.8660254037844387076, 1.000000000000000000, 0.8660254037844387076, 1.000000000000000000, 0.8660254037844387076, 1.000000000000000000, 0.8660254037844387076, 1.000000000000000000, 0.8660254037844387076, 1.000000000000000000, 0.8660254037844387076, 1.000000000000000000, 0.8660254037844387076, 1.000000000000000000, 0.8660254037844387076, 1.000000000000000000, 0.8660254037844387076, 1.000000000000000000, 0.8660254037844387076, 1.000000000000000000, 0.8660254037844387076, 1.000000000000000000, 0.8660254037844387076, 1.000000000000000000, 0.8660254037844387076, 1.000000000000000000, 0.8660254037844387076, 1.000000000000000000, 0.8660254037844387076, 1.000000000000000000, 0.8660254037844387076, 1.000000000000000000, 0.8660254037844387076, 1.000000000000000000, 0.8660254037844387076, 1.000000000000000000, 0.8660254037844387076, 1.000000000000000000, 0.8660254037844387076, 1.000000000000000000, 0.8660254037844387076, 1.000000000000000000, 0.8660254037844387076, 1.000000000000000000, 0.8660254037844387076, 1.000000000000000000, 0.8660254037844387076, 1.000000000000000000, 0.8660254037844387076, 1.000000000000000000, 0.8660254037844387076, 1.000000000000000000, 0.8660254037844387076, 1.000000000000000000, 0.8660254037844387076, 1.000000000000000000, 0.8660254037844387076, 1.000000000000000000, 0.8660254037844387076, 1.000000000000000000, 0.8660254037844387076, 1.000000000000000000, 0.8660254037844387076, 1.000000000000000000, 0.8660254037844387076, 1.000000000000000000, 0.8660254037844387076, 1.000000000000000000, 0.8660254037844387076, 1.000000000000000000, 0.8660254037844387076, 1.000000000000000000, 0.8660254037844387076, 1.000000000000000000, 0.8660254037844387076, 1.000000000000000000, 0.8660254037844387076, 1.000000000000000000, 0.8660254037844387076, 1.000000000000000000, 0.8660254037844387076, 1.000000000000000000, 0.8660254037844387076, 1.000000000000000000, 0.8660254037844387076, 1.000000000000000000, 0.8660254037844387076, 1.000000000000000000, 0.8660254037844387076, 1.000000000000000000, 0.8660254037844387076, 1.000000000000000000, 0.8660254037844387076, 1.000000000000000000, 0.8660254037844387076, 1.000000000000000000, 0.8660254037844387076, 1.000000000000000000, 0.8660254037844387076, 1.000000000000000000, 0.8660254037844387076, 1.000000000000000000, 0.8660254037844387076, 1.000000000000000000, 0.8660254037844387076, 1.000000000000000000, 0.8660254037844387076, 1.000000000000000000, 0.8660254037844387076, 1.000000000000000000, 0.8660254037844387076, 1.000000000000000000, 0.8660254037844387076, 1.000000000000000000, 0.8660254037844387076, 1.000000000000000000, 0.8660254037844387076, 1.000000000000000000, 0.8660254037844387076, 1.000000000000000000, 0.8660254037844387076, 1.000000000000000000, 0.8660254037844387076, 1.000000000000000000, 0.8660254037844387076, 1.000000000000000000, 0.8660254037844387076, 1.000000000000000000, 0.8660254037844387076, 1.000000000000000000, 0.8660254037844387076, 1.000000000000000000, 0.8660254037844387076, 1.000000000000000000, 0.8660254037844387076, 1.000000000000000000, 0.8660254037844387076, 1.000000000000000000, 0.8660254037844387076, 1.000000000000000000, 0.8660254037844387076, 1.000000000000000000, 0.8660254037844387076, 1.000000000000000000, 0.8660254037844387076, 1.000000000000000000, 0.8660254037844387076, 1.000000000000000000, 0.8660254037844387076, 1.000000000000000000, 0.8660254037844387076, 1.000000000000000000, 0.8660254037844387076, 1.000000000000000000, 0.8660254037844387076, 1.000000000000000000, 0.8660254037844387076, 1.000000000000000000, 0.8660254037844387076, 1.000000000000000000, 0.8660254037844387076, 1.000000000000000000, 0.8660254037844387076, 1.000000000000000000, 0.8660254037844387076, 1.000000000000000000, 0.8660254037844387076, 1.000000000000000000, 0.8660254037844387076, 1.000000000000000000, 0.8660254037844387076, 1.000000000000000000, 0.8660254037844387076, 1.000000000000000000, 0.8660254037844387076, 1.000000000000000000, 0.8660254037844387076, 1.000000000000000000, 0.8660254037844387076, 1.000000000000000000, 0.8660254037844387076, 1.000000000000000000, 0.8660254037844387076, 1.000000000000000000, 0.8660254037844387076, 1.000000000000000000, 0.8660254037844387076, 1.000000000000000000, 0.8660254037844387076, 1.000000000000000000, 0.8660254037844387076, 1.000000000000000000, 0.8660254037844387076, 1.000000000000000000, 0.8660254037844387076, 1.000000000000000000, 0.8660254037844387076, 1.000000000000000000, 0.8660254037844387076, 1.000000000000000000, 0.8660254037844387076, 1.000000000000000000, 0.8660254037844387076, 1.000000000000000000, 0.8660254037844387076, 1.000000000000000000, 0.8660254037844387076, 1.000000000000000000, 0.8660254037844387076, 1.000000000000000000, 0.8660254037844387076, 1.000000000000000000, 0.8660254037844387076, 1.000000000000000000, 0.8660254037844387076, 1.000000000000000000, 0.8660254037844387076, 1.000000000000000000, 0.8660254037844387076, 1.000000000000000000, 0.8660254037844387076, 1.000000000000000000, 0.8660254037844387076, 1.000000000000000000, 0.8660254037844387076, 1.000000000000000000, 0.8660254037844387076, 1.000000000000000000, 0.8660254037844387076, 1.000000000000000000, 0.8660254037844387076, 1.000000000000000000, 0.8660254037844387076, 1.000000000000000000, 0.8660254037844387076, 1.000000000000000000, 0.8660254037844387076, 1.000000000000000000, 0.8660254037844387076, 1.000000000000000000, 0.8660254037844387076, 1.000000000000000000, 0.8660254037844387076, 1.000000000000000000, 0.8660254037844387076, 1.000000000000000000, 0.8660254037844387076, 1.000000000000000000, 0.8660254037844387076, 1.000000000000000000, 0.8660254037844387076, 1.000000000000000000, 0.8660254037844387076, 1.000000000000000000, 0.8660254037844387076, 1.000000000000000000, 0.8660254037844387076, 1.000000000000000000, 0.8660254037844387076, 1.000000000000000000, 0.8660254037844387076, 1.000000000000000000, 0.8660254037844387076, 1.000000000000000000, 0.8660254037844387076, 1.000000000000000000, 0.8660254037844387076, 1.000000000000000000, 0.8660254037844387076, 1.000000000000000000, 0.8660254037844387076, 1.000000000000000000, 0.8660254037844387076, 1.000000000000000000, 0.8660254037844387076, 1.000000000000000000, 0.8660254037844387076, 1.000000000000000000, 0.8660254037844387076, 1.000000000000000000, 0.8660254037844387076, 1.000000000000000000, 0.8660254037844387076, 1.000000000000000000, 0.8660254037844387076, 1.000000000000000000, 0.8660254037844387076, 1.000000000000000000, 0.8660254037844387076, 1.000000000000000000, 0.8660254037844387076, 1.000000000000000000, 0.8660254037844387076, 1.000000000000000000, 0.8660254037844387076, 1.000000000000000000, 0.8660254037844387076, 1.000000000000000000, 0.8660254037844387076, 1.000000000000000000, 0.8660254037844387076, 1.000000000000000000, 0.8660254037844387076, 1.000000000000000000, 0.8660254037844387076, 1.000000000000000000, 0.8660254037844387076, 1.000000000000000000, 0.8660254037844387076, 1.000000000000000000, 0.8660254037844387076, 1.000000000000000000, 0.8660254037844387076, 1.000000000000000000, 0.8660254037844387076, 1.000000000000000000, 0.8660254037844387076, 1.000000000000000000, 0.8660254037844387076, 1.000000000000000000, 0.8660254037844387076, 1.000000000000000000, 0.8660254037844387076, 1.000000000000000000, 0.8660254037844387076, 1.000000000000000000, 0.8660254037844387076, 1.000000000000000000, 0.8660254037844387076, 1.000000000000000000, 0.8660254037844387076, 1.000000000000000000) ) ) 
 REPRESENTATION_ITEM ( '' )  SURFACE ( )  );
#52589 = CARTESIAN_POINT ( 'NONE',  ( 3.666520218671379450, -0.8364210039109070127, -1.894060025281426807 ) ) ;
#52590 = CARTESIAN_POINT ( 'NONE',  ( 4.227444969362701421, 3.826440640544909400, 1.214306433183764966E-14 ) ) ;
#52591 = CARTESIAN_POINT ( 'NONE',  ( -1.360316468750004448, 1.671875000341424666, -8.673617379884035472E-15 ) ) ;
#52592 = APPLICATION_PROTOCOL_DEFINITION ( 'draft international standard', 'automotive_design', 1998, #58896 ) ;
#52594 = CARTESIAN_POINT ( 'NONE',  ( 1.664548039484465614, -1.362698257634049614, 1.362033803609383531 ) ) ;
#52593 = CARTESIAN_POINT ( 'NONE',  ( -7.669108446824431269, 12.09904362127053545, -0.7998128361456291469 ) ) ;
#52595 = CARTESIAN_POINT ( 'NONE',  ( 9.581972888692709134, -7.217909409572547119, 3.990133149647489978E-13 ) ) ;
#52596 = CARTESIAN_POINT ( 'NONE',  ( 0.2386330332824412315, -1.909482672672847992, -0.4822418261516500659 ) ) ;
#52597 = CARTESIAN_POINT ( 'NONE',  ( 5.709392084686216506, 5.833581318321598985, -0.7216878364870458196 ) ) ;
#52598 = CARTESIAN_POINT ( 'NONE',  ( 5.744750223003346257, 6.067414509003485001, 0.6312745094601609486 ) ) ;
#52599 = CARTESIAN_POINT ( 'NONE',  ( -1.500000000000008216, 11.03125000068279427, 3.469446951953614189E-15 ) ) ;
#52600 = CARTESIAN_POINT ( 'NONE',  ( -2.754277761870538299, 6.365074488824250309, 1.040834085586084257E-14 ) ) ;
#52601 = CARTESIAN_POINT ( 'NONE',  ( 2.004415182159818176, -0.9449143528836713157, 2.010537586115124231 ) ) ;
#52602 = CARTESIAN_POINT ( 'NONE',  ( 3.153452123856602896, -1.720715631468725526, -1.213874241417127298 ) ) ;
#52603 = CARTESIAN_POINT ( 'NONE',  ( -5.915100157312088491, 10.12297696016459092, -0.7998128361456362523 ) ) ;
#52604 = CARTESIAN_POINT ( 'NONE',  ( 7.019370843573166319, 9.212351955633947043, 1.599625672291281386 ) ) ;
#52605 = CARTESIAN_POINT ( 'NONE',  ( 0.7130641938532373825, -1.569203791704287809, -1.000260708767531481 ) ) ;
#52606 = CARTESIAN_POINT ( 'NONE',  ( 7.122110765880372618, 7.203550736482235095, 0.7998128361456341429 ) ) ;
#52607 = CARTESIAN_POINT ( 'NONE',  ( 5.443762371086860341, 6.309809840144842141, 1.199719254218462483 ) ) ;
#52608 = CARTESIAN_POINT ( 'NONE',  ( -6.807602527837528505, 7.114826835331461652, 0.7216878364870317197 ) ) ;
#52609 = CARTESIAN_POINT ( 'NONE',  ( -7.944714827928056167, 10.29191993738131927, 1.443375672974090751 ) ) ;
#52610 = CARTESIAN_POINT ( 'NONE',  ( 0.8090202166558431163, -0.5209130535433897924, -2.055487714681260236 ) ) ;
#52611 = CARTESIAN_POINT ( 'NONE',  ( -6.882699257592852504, 8.058845884393651460, -1.199719254218452047 ) ) ;
#52613 = CARTESIAN_POINT ( 'NONE',  ( 4.861744986159981075, -0.5251177144562025889, 1.890194517805739771 ) ) ;
#52612 = CARTESIAN_POINT ( 'NONE',  ( -1.225000000000040279, 0.2500000000000002220, -4.857225732735059864E-14 ) ) ;
#52614 = CARTESIAN_POINT ( 'NONE',  ( 3.379894511112140787, 1.369989894601089775, 1.672159933133889442 ) ) ;
#52615 = CARTESIAN_POINT ( 'NONE',  ( 1.434833617064284805, -1.334073193498284793, -1.269287082821937584 ) ) ;
#52616 = AXIS2_PLACEMENT_3D ( 'NONE', #201616, #120478, #23946 ) ;
#52617 = CARTESIAN_POINT ( 'NONE',  ( -4.124570878694319376, 7.473888947179561981, -0.6522657496016289747 ) ) ;
#52618 = PLANE ( 'NONE',  #54099 ) ;
#52619 = CARTESIAN_POINT ( 'NONE',  ( 4.628681372238307112, -1.589566819310319845, 0.7089629299102307991 ) ) ;
#52620 = CARTESIAN_POINT ( 'NONE',  ( -7.247736482492767252, 15.00000000000521538, -10.57961706324489626 ) ) ;
#52621 = CARTESIAN_POINT ( 'NONE',  ( 4.528060117284229413, 7.266191989264828344, 1.082531754730558626 ) ) ;
#52622 = CARTESIAN_POINT ( 'NONE',  ( -10.47476534206535170, 5.237283261923990629, -5.169982392003922733 ) ) ;
#52623 = CARTESIAN_POINT ( 'NONE',  ( 2.290102563249151402, -0.9248296759884739870, 1.954025333243500917 ) ) ;
#52624 = CARTESIAN_POINT ( 'NONE',  ( 2.934922540206805319, 1.076151813804010926, 1.704677747124828446 ) ) ;
#52625 = LINE ( 'NONE', #36365, #51488 ) ;
#52626 = CARTESIAN_POINT ( 'NONE',  ( 1.235488887756378551, -1.954010380348418119, 0.9248176494114216384 ) ) ;
#52627 = CARTESIAN_POINT ( 'NONE',  ( 2.940257707442377022, 1.956376729411358095, 0.2430245213203632293 ) ) ;
#52628 = CARTESIAN_POINT ( 'NONE',  ( 6.509000000000053632, 6.037921079186737927, 2.494901127718162304 ) ) ;
#52629 = CARTESIAN_POINT ( 'NONE',  ( 3.403789896209925114, -0.7897705758606025084, -1.774406015287466332 ) ) ;
#52632 = ORIENTED_EDGE ( 'NONE', *, *, #88440, .T. ) ;
#52631 = CARTESIAN_POINT ( 'NONE',  ( 4.726684935852882852, 4.891486930089099516, -0.8194250277325197951 ) ) ;
#52630 = CARTESIAN_POINT ( 'NONE',  ( -10.43941509239824228, 11.28166515066052966, 1.040834085586084257E-14 ) ) ;
#52633 = CARTESIAN_POINT ( 'NONE',  ( -4.136646265500958819, 7.840188053144158786, -0.7216878364870458196 ) ) ;
#52634 = CARTESIAN_POINT ( 'NONE',  ( -0.1110810684432777806, 1.403644835841436400, -2.056232460864733103 ) ) ;
#52635 = CARTESIAN_POINT ( 'NONE',  ( 5.306037014901791693, 7.283738832175834510, 1.599625672291269396 ) ) ;
#52636 = CARTESIAN_POINT ( 'NONE',  ( -3.983063267364693960, 7.868933921892603323, -0.7998128361456481317 ) ) ;
#52637 = CARTESIAN_POINT ( 'NONE',  ( -7.144220599758281054, 7.299621885998258897, 0.7998128361456341429 ) ) ;
#52638 = CARTESIAN_POINT ( 'NONE',  ( -8.120970824461345217, 12.41829036193951730, 0.7216878364870458196 ) ) ;
#52639 = CARTESIAN_POINT ( 'NONE',  ( 6.616287922300326585, -1.079552588663035051, -2.039509185488725951 ) ) ;
#52640 = CARTESIAN_POINT ( 'NONE',  ( -3.285556943750000514, -2.588541666188707513, -1.896917185911906500 ) ) ;
#52641 = CARTESIAN_POINT ( 'NONE',  ( 4.311346321947408633, -1.628642355029306987, -1.093319670275281652 ) ) ;
#52642 = CARTESIAN_POINT ( 'NONE',  ( 8.067265095331215718, 9.370563018429956870, 1.199719254218462483 ) ) ;
#52643 = CARTESIAN_POINT ( 'NONE',  ( 1.283827520628720187, 1.646837967535810021, -1.163270716046126196 ) ) ;
#52644 = ORIENTED_EDGE ( 'NONE', *, *, #92114, .T. ) ;
#52645 = CARTESIAN_POINT ( 'NONE',  ( 3.977823109611013930, -0.8067237889231733128, 1.957824063906116407 ) ) ;
#52646 = CARTESIAN_POINT ( 'NONE',  ( 1.499999999999987121, 1.577083334016150751, -0.8660254037844253849 ) ) ;
#52648 = CARTESIAN_POINT ( 'NONE',  ( -5.259673527097670664, 8.223703984000886535, -1.199719254218446718 ) ) ;
#52647 = CARTESIAN_POINT ( 'NONE',  ( 5.021104450059825197, 4.960302734598949215, 0.4581612399162004468 ) ) ;
#52649 = CARTESIAN_POINT ( 'NONE',  ( 2.923586578878138109, 1.022379729796508041, -1.530975008504284141 ) ) ;
#52650 = EDGE_LOOP ( 'NONE', ( #207522, #27860, #186889, #15606 ) ) ;
#52651 = CARTESIAN_POINT ( 'NONE',  ( -8.809047120577080392, 11.30030761213851953, 1.599625672291269396 ) ) ;
#52652 = CARTESIAN_POINT ( 'NONE',  ( 0.005641171162447556654, 8.210923785195014091, 2.038653139403750369 ) ) ;
#52653 = CARTESIAN_POINT ( 'NONE',  ( 4.148766697842418694, 2.080301416381886703, 0.4105806053946169376 ) ) ;
#52654 = CARTESIAN_POINT ( 'NONE',  ( 1.836970198721030181E-16, 13.49999999999999822, 1.500000000000000222 ) ) ;
#52655 = CARTESIAN_POINT ( 'NONE',  ( 6.531277313481192337, 8.642909503859968368, 1.599625672291281386 ) ) ;
#52656 = B_SPLINE_CURVE_WITH_KNOTS ( 'NONE', 3,
 ( #80183, #48765, #214399, #146288, #13037, #98575, #95406, #144177, #114880, #44513 ),
 .UNSPECIFIED., .F., .F.,
 ( 4, 2, 2, 2, 4 ),
 ( 7.099868766331327897E-18, 0.0002236660844579363818, 0.0004473321689158656620, 0.0006709982533737948339, 0.0008946643378317241683 ),
 .UNSPECIFIED. ) ;
#52657 = CARTESIAN_POINT ( 'NONE',  ( 5.114554592455347048, 1.424167462454002608, -1.489711086068323587 ) ) ;
#52658 = AXIS2_PLACEMENT_3D ( 'NONE', #10630, #58338, #174249 ) ;
#52660 = CARTESIAN_POINT ( 'NONE',  ( 2.278628554356322500, 1.682734121078124812, -0.7478279864501293783 ) ) ;
#52659 = CARTESIAN_POINT ( 'NONE',  ( 0.8888279104573212352, 0.1313983060258062385, 1.856467483602406432 ) ) ;
#52661 = CARTESIAN_POINT ( 'NONE',  ( 9.772729797352075920, 10.29593960653257234, -0.7998128361456281477 ) ) ;
#52662 = CARTESIAN_POINT ( 'NONE',  ( 0.6760876847618801921, -1.398214087147084248E-14, 1.193909349079574245 ) ) ;
#52663 = CARTESIAN_POINT ( 'NONE',  ( -7.014364370223741929, 9.276787413384745662, -1.599625672291271394 ) ) ;
#52664 = CARTESIAN_POINT ( 'NONE',  ( 2.455956380646412196, 0.5873987694336445520, -2.127207350628975924 ) ) ;
#52665 = CARTESIAN_POINT ( 'NONE',  ( 5.308033872091713512, -2.252217787711635388, 0.2143866227288723780 ) ) ;
#52666 = CARTESIAN_POINT ( 'NONE',  ( -7.537970219518089543, 8.857015346601659900, -1.082531754730543971 ) ) ;
#52667 = CARTESIAN_POINT ( 'NONE',  ( 4.816585706611137496, -0.6173935602037239345, -1.703258737839604242 ) ) ;
#52668 = CARTESIAN_POINT ( 'NONE',  ( 4.557778266838360182, 1.108094384514320963, 1.562507240529472874 ) ) ;
#52669 = CARTESIAN_POINT ( 'NONE',  ( 0.6823417656249917140, 3.905208333674754950, 1.181850606188765695 ) ) ;
#52670 = CARTESIAN_POINT ( 'NONE',  ( 4.258636414635104117, -1.461677231104720143, 1.323132448414195528 ) ) ;
#52671 = CARTESIAN_POINT ( 'NONE',  ( 4.680451076648031616, -1.814532364864028136, -0.4542276060127621862 ) ) ;
#52672 = CARTESIAN_POINT ( 'NONE',  ( 4.967181581899757781, 1.619035083845013157, 0.9176225028624994673 ) ) ;
#52673 = CARTESIAN_POINT ( 'NONE',  ( 1.364683531249988535, 5.405208333674750953, -0.7879004041258300672 ) ) ;
#52674 = AXIS2_PLACEMENT_3D ( 'NONE', #212604, #98879, #1336 ) ;
#52675 = CARTESIAN_POINT ( 'NONE',  ( 0.1808755166769344669, 1.673851406602990366, -1.124249698880399162 ) ) ;
#52677 = CARTESIAN_POINT ( 'NONE',  ( 1.752698641044206251, 0.6620485714215967876, 1.999371444633216033 ) ) ;
#52676 = CARTESIAN_POINT ( 'NONE',  ( -4.568734577680899633, 4.432537883490215158, -0.7216878364870207285 ) ) ;
#52678 = CARTESIAN_POINT ( 'NONE',  ( 10.72180055030867329, 11.40318881831530540, 0.7998128361456341429 ) ) ;
#52680 = CARTESIAN_POINT ( 'NONE',  ( -10.10098813738111545, 11.74323990082152491, -1.199719254218441611 ) ) ;
#52679 = CARTESIAN_POINT ( 'NONE',  ( -1.432341765625004593, 8.460937500170699010, 8.673617379884035472E-16 ) ) ;
#52681 = CARTESIAN_POINT ( 'NONE',  ( 3.076547362214879566, 0.9570632234598417387, 1.892448740577145738 ) ) ;
#52682 = DIRECTION ( 'NONE',  ( -0.7071067811865462405, 0.000000000000000000, 0.7071067811865489050 ) ) ;
#52683 = CARTESIAN_POINT ( 'NONE',  ( 2.267837486342203057, 0.5347344578308220742, -1.947668537691170876 ) ) ;
#52684 = CARTESIAN_POINT ( 'NONE',  ( -1.364683531250012516, 1.530208333674756505, 0.7879004041258379498 ) ) ;
#52685 = CARTESIAN_POINT ( 'NONE',  ( -2.155383234892699562, 5.458438174109348395, 1.040834085586084257E-14 ) ) ;
#52686 = CARTESIAN_POINT ( 'NONE',  ( 5.495132332240461714, 5.305409230568988832, 0.7998128361456341429 ) ) ;
#52687 = ORIENTED_EDGE ( 'NONE', *, *, #123001, .T. ) ;
#52688 = CARTESIAN_POINT ( 'NONE',  ( 1.845224345143604561, -1.827161268409679407, 1.154667503900350445 ) ) ;
#52689 = CARTESIAN_POINT ( 'NONE',  ( 6.890000000000015667, 0.5768591945385994624, 2.052260346930290247 ) ) ;
#52692 = CARTESIAN_POINT ( 'NONE',  ( 4.586165880992507660, 5.350526861157986147, -7.499999999999997335 ) ) ;
#52691 = CARTESIAN_POINT ( 'NONE',  ( 11.86145017354043674, 10.09514365543876124, -1.100000000000000533 ) ) ;
#52690 = CARTESIAN_POINT ( 'NONE',  ( 4.736594563127852098, 6.619389305106191834, -1.599625672291273171 ) ) ;
#52693 = CARTESIAN_POINT ( 'NONE',  ( 0.1263921867887893569, 7.114106634750518410, 3.985475513000639847 ) ) ;
#52694 = CARTESIAN_POINT ( 'NONE',  ( -8.676855123066030018, 9.225345186439589895, -0.7216878364870267237 ) ) ;
#52695 = CARTESIAN_POINT ( 'NONE',  ( 0.6092356648998223934, -0.3158941238240610128, 2.168550393043596536 ) ) ;
#52696 = DIRECTION ( 'NONE',  ( -2.664535259100375697E-15, 0.000000000000000000, -1.000000000000000000 ) ) ;
#52698 = CARTESIAN_POINT ( 'NONE',  ( 0.6823417656249934904, 12.19270833367473017, 1.181850606188764807 ) ) ;
#52697 = CARTESIAN_POINT ( 'NONE',  ( 1.657462679512666348, -1.941143012291703940, -1.162103002166763988 ) ) ;
#52699 = CARTESIAN_POINT ( 'NONE',  ( -8.779068160048691283, 10.20099992726700933, -1.199719254218446718 ) ) ;
#52700 = CARTESIAN_POINT ( 'NONE',  ( -5.707619481228834779, 5.761236937629489852, -0.7216878364870197293 ) ) ;
#52701 = CARTESIAN_POINT ( 'NONE',  ( -0.6823417656250212460, 2.363541667008084435, 1.181850606188767472 ) ) ;
#52702 = CARTESIAN_POINT ( 'NONE',  ( 4.624009687016504166, 8.337032093926254106, -0.3390773965592456252 ) ) ;
#52703 = ADVANCED_FACE ( 'NONE', ( #167263 ), #17771, .F. ) ;
#52704 = CARTESIAN_POINT ( 'NONE',  ( -6.009258394948636914E-15, 9.937500000000000000, -1.732050807568875195 ) ) ;
#52705 = CARTESIAN_POINT ( 'NONE',  ( 3.580403817701179658, -1.662759015092404535, -0.4584509792747801793 ) ) ;
#52706 = CARTESIAN_POINT ( 'NONE',  ( 4.041212305325117882, 6.872442235258051646, -1.199719254218448494 ) ) ;
#52707 = CARTESIAN_POINT ( 'NONE',  ( 2.231405582217013794, -1.152036887248751862, -1.343533879150171861 ) ) ;
#52708 = CARTESIAN_POINT ( 'NONE',  ( 2.807291710112637340, 1.725400251052783052, -1.036881053028392508 ) ) ;
#52709 = CARTESIAN_POINT ( 'NONE',  ( 8.940712233207955606, 12.51824914112961729, 1.199719254218450271 ) ) ;
#52710 = CARTESIAN_POINT ( 'NONE',  ( 5.684669477433477169, -2.151827843693389308, -0.4886931181809702207 ) ) ;
#52711 = ORIENTED_EDGE ( 'NONE', *, *, #109929, .T. ) ;
#52712 = CARTESIAN_POINT ( 'NONE',  ( 4.271743411778946786, 0.4384756098019436665, -1.971458303354764352 ) ) ;
#52713 = CARTESIAN_POINT ( 'NONE',  ( -6.343235766347277149, 8.493804042195527870, -1.599625672291271394 ) ) ;
#52714 = CARTESIAN_POINT ( 'NONE',  ( 4.025017672583341977, -1.753021876717888006, 0.9963191169995513352 ) ) ;
#52715 = EDGE_LOOP ( 'NONE', ( #54452, #126809, #113120, #110162, #34076, #169516, #157038, #85244 ) ) ;
#52716 = EDGE_CURVE ( 'NONE', #49215, #20719, #133728, .T. ) ;
#52717 = CARTESIAN_POINT ( 'NONE',  ( 3.010468980803046257, 1.356049738124785353, -1.288842618233053683 ) ) ;
#52718 = EDGE_CURVE ( 'NONE', #168104, #55444, #8040, .T. ) ;
#52719 = CARTESIAN_POINT ( 'NONE',  ( 1.494246876672610025, -1.020364814108923213, 1.617233793950809906 ) ) ;
#52720 = LINE ( 'NONE', #102541, #129793 ) ;
#52721 = CARTESIAN_POINT ( 'NONE',  ( -11.76696981052429614, 4.673730779118267620, -4.995440715239801044 ) ) ;
#52722 = FILL_AREA_STYLE ('',( #136127 ) ) ;
#52723 = CARTESIAN_POINT ( 'NONE',  ( 1.364683531249990311, 2.696875000341415696, 1.214306433183764966E-14 ) ) ;
#52724 = CARTESIAN_POINT ( 'NONE',  ( 0.3867804997886997720, -1.801505969789623629, -0.6421655129100201087 ) ) ;
#52725 = CARTESIAN_POINT ( 'NONE',  ( 6.549997609177859559, 6.814287763561861944, 0.000000000000000000 ) ) ;
#52726 = CARTESIAN_POINT ( 'NONE',  ( 1.205434515183744226, -1.544416933936803904, -1.209700862059132964 ) ) ;
#52727 = DIRECTION ( 'NONE',  ( -0.6716942845482062330, -1.762391939599642519E-12, -0.7408284471490506062 ) ) ;
#52728 = CARTESIAN_POINT ( 'NONE',  ( -6.099189001301292379, 8.209082816308541197, 1.599625672291263179 ) ) ;
#52729 = CARTESIAN_POINT ( 'NONE',  ( 5.379186226027963258, -1.918017450862268714, -0.9047448674902383026 ) ) ;
#52731 = CARTESIAN_POINT ( 'NONE',  ( -10.48267169704037727, 5.268073273308885973, 5.153989745587932880 ) ) ;
#52730 = CARTESIAN_POINT ( 'NONE',  ( 7.574201371528760163, 11.98831870009225931, 1.040834085586084257E-14 ) ) ;
#52732 = CARTESIAN_POINT ( 'NONE',  ( 5.940691962724923059, 0.3820465716247494758, 1.933821394355714096 ) ) ;
#52733 = CARTESIAN_POINT ( 'NONE',  ( 1.364683531249986537, 1.113541667008082658, 0.7879004041258500513 ) ) ;
#52734 = CARTESIAN_POINT ( 'NONE',  ( 1.353772324478102584, -1.461116690358499337, -1.385217879419877951 ) ) ;
#52735 = ORIENTED_EDGE ( 'NONE', *, *, #50294, .T. ) ;
#52736 = CARTESIAN_POINT ( 'NONE',  ( 1.072038591870585700, -0.9482746200860227015, 1.893052406114493769 ) ) ;
#52737 = CARTESIAN_POINT ( 'NONE',  ( 11.49074101613450338, 7.329535750694848417, -3.313523036300598967 ) ) ;
#52738 = CARTESIAN_POINT ( 'NONE',  ( 2.875506610227479332, -0.2054619808779626633, 2.060159609288146232 ) ) ;
#52739 = CARTESIAN_POINT ( 'NONE',  ( 5.564695703766185275, 5.456842840674144490, 0.000000000000000000 ) ) ;
#52740 = CARTESIAN_POINT ( 'NONE',  ( 6.170896192875352959, 7.228408975556602556, 1.199719254218453823 ) ) ;
#52741 = ORIENTED_EDGE ( 'NONE', *, *, #142525, .T. ) ;
#52743 = CARTESIAN_POINT ( 'NONE',  ( 2.855963913973019963, 6.483708332943829866, 0.000000000000000000 ) ) ;
#52742 = CARTESIAN_POINT ( 'NONE',  ( 4.435544174077206137, 0.8940267830384877046, -1.889970096008020128 ) ) ;
#52746 = ORIENTED_EDGE ( 'NONE', *, *, #164497, .F. ) ;
#52745 = CARTESIAN_POINT ( 'NONE',  ( 1.154613445820645845, 0.3528100842024176620, 1.776585200675658172 ) ) ;
#52744 = CARTESIAN_POINT ( 'NONE',  ( 3.399243825379614226, 1.438455020490635450, 1.123966471122700650 ) ) ;
#52747 = CARTESIAN_POINT ( 'NONE',  ( 9.499606442108964544, -9.746166700193986898, -0.08647222121513538362 ) ) ;
#52748 = CARTESIAN_POINT ( 'NONE',  ( 4.514586370236258084, 5.411880727520489209, 1.219673154775415824 ) ) ;
#52749 = CARTESIAN_POINT ( 'NONE',  ( 8.810850279130727714, 13.35345686061384640, -7.679452701197651443 ) ) ;
#52750 = CARTESIAN_POINT ( 'NONE',  ( 5.403435775159438847, 1.801252639416499601, 1.274624607731331905 ) ) ;
#52751 = CARTESIAN_POINT ( 'NONE',  ( 1.364683531250000748, 9.567708333674735499, -0.7879004041258355073 ) ) ;
#52752 = ORIENTED_EDGE ( 'NONE', *, *, #89264, .T. ) ;
#52753 = CARTESIAN_POINT ( 'NONE',  ( 4.547458224165379370, -1.746952781796942133, 0.7782266863690868730 ) ) ;
#52754 = CARTESIAN_POINT ( 'NONE',  ( -4.081167932913447594, 4.720116328942494555, -1.199719254218452047 ) ) ;
#52755 = VECTOR ( 'NONE', #202096, 1000.000000000000000 ) ;
#52756 = CARTESIAN_POINT ( 'NONE',  ( 8.121497709785879593, 9.433834401960398353, -1.199719254218445830 ) ) ;
#52757 = CARTESIAN_POINT ( 'NONE',  ( 6.514133371570012265, 2.065101995627930620, -0.1482383472809906122 ) ) ;
#52758 = PRESENTATION_LAYER_ASSIGNMENT (  '', '', ( #187588 ) ) ;
#52759 = CARTESIAN_POINT ( 'NONE',  ( 1.360316468749989571, 0.5677083336747246189, -0.7853790794158941324 ) ) ;
#52760 = CARTESIAN_POINT ( 'NONE',  ( 4.867013957181530515, 5.740899707208986236, -1.082531754730548412 ) ) ;
#52761 = CARTESIAN_POINT ( 'NONE',  ( 6.053423048675670159, 7.145495228771222784, -1.160209803801291795 ) ) ;
#52762 = CARTESIAN_POINT ( 'NONE',  ( -5.991398640336265125, 15.46937860491462757, -10.40685062603460587 ) ) ;
#52763 = CARTESIAN_POINT ( 'NONE',  ( 0.000000000000000000, 4.099999999999999645, 0.000000000000000000 ) ) ;
#52764 = CARTESIAN_POINT ( 'NONE',  ( 3.092876253348992410, 1.606159189733218140, -0.9584765265276545820 ) ) ;
#52765 = CARTESIAN_POINT ( 'NONE',  ( 11.84101807917483740, 11.11021500260877382, -1.444039656437080543 ) ) ;
#52766 = CARTESIAN_POINT ( 'NONE',  ( -2.788906526875773208E-15, 12.46875000068279782, -1.499999999999998446 ) ) ;
#52767 = CARTESIAN_POINT ( 'NONE',  ( -5.558479791922849245, 9.428717490644563881, 0.7216878364870458196 ) ) ;
#52768 = CARTESIAN_POINT ( 'NONE',  ( 5.259637247458703868, 5.100941308315409373, 0.000000000000000000 ) ) ;
#52769 = CARTESIAN_POINT ( 'NONE',  ( 5.311043488251262268, 7.219303374425030562, -1.599625672291256295 ) ) ;
#52770 = CARTESIAN_POINT ( 'NONE',  ( 0.2331713839410576583, 0.005725554726919174046, -1.953566683266183102 ) ) ;
#52771 = CARTESIAN_POINT ( 'NONE',  ( 1.019157904985489305, -1.821734318179563106, 0.8647433871810317196 ) ) ;
#52772 = CARTESIAN_POINT ( 'NONE',  ( -7.635213062790267458, 12.05949900656400686, 0.000000000000000000 ) ) ;
#52773 = CARTESIAN_POINT ( 'NONE',  ( 6.855582950365507244, 8.027210192628430718, -1.199719254218452047 ) ) ;
#52774 = CARTESIAN_POINT ( 'NONE',  ( -4.702146809683744877, 5.356480858934594025, 2.420000000000010587 ) ) ;
#52775 = CARTESIAN_POINT ( 'NONE',  ( 1.781448188194576066, 1.512826363221421833, 1.585725795389548942 ) ) ;
#52776 = CARTESIAN_POINT ( 'NONE',  ( 6.674438497507635404, -1.118711561685633349, 1.443368817030561635 ) ) ;
#52777 = CARTESIAN_POINT ( 'NONE',  ( -2.300079615812729905, 5.835176651756807331, -0.7998128361456281477 ) ) ;
#52778 = CARTESIAN_POINT ( 'NONE',  ( 5.614485009834906393, 6.683225611963085733, -1.082531754730548412 ) ) ;
#52780 = EDGE_CURVE ( 'NONE', #79300, #92493, #115152, .T. ) ;
#52779 = CARTESIAN_POINT ( 'NONE',  ( 9.049177462117294013, 12.64479190819049670, -1.199719254218446718 ) ) ;
#52781 = CARTESIAN_POINT ( 'NONE',  ( 4.715538499454675403, 4.395883092318884522, 1.214306433183764966E-14 ) ) ;
#52782 = CARTESIAN_POINT ( 'NONE',  ( 4.577813143269636065, 5.369812084349879555, -1.199719254218450271 ) ) ;
#52783 = ORIENTED_EDGE ( 'NONE', *, *, #44567, .F. ) ;
#52785 = CARTESIAN_POINT ( 'NONE',  ( 0.8561085696928095734, 0.8139254773164643630, -1.841379974997810143 ) ) ;
#52784 = CARTESIAN_POINT ( 'NONE',  ( 3.772867777003403589, 1.732451475078290448, -0.6238847238279123797 ) ) ;
#52786 = CARTESIAN_POINT ( 'NONE',  ( 1.915759298113205666, 0.7205626639651928622, 2.182595962359680897 ) ) ;
#52788 = CARTESIAN_POINT ( 'NONE',  ( 0.4614603993745093891, -0.5041695895235782654, 1.791261842318598863 ) ) ;
#52787 = CARTESIAN_POINT ( 'NONE',  ( 5.016153647376217606, 4.954526798134778254, 0.7216878364870317197 ) ) ;
#52789 = CARTESIAN_POINT ( 'NONE',  ( 0.000000000000000000, -4.046874999522043659, -3.793834371823813001 ) ) ;
#52790 = CARTESIAN_POINT ( 'NONE',  ( -3.255929445576174697, 6.950334786480840243, -0.7998128361456281477 ) ) ;
#52791 = CARTESIAN_POINT ( 'NONE',  ( -9.497657701571187161, 14.57981886740818922, -7.334628297552537646 ) ) ;
#52792 = CARTESIAN_POINT ( 'NONE',  ( 4.236511230858605259, 1.172298487584079396, -1.510895503047122945 ) ) ;
#52793 = CARTESIAN_POINT ( 'NONE',  ( -9.321394304595349567, 10.83371376257142416, 1.199719254218462483 ) ) ;
#52794 = CARTESIAN_POINT ( 'NONE',  ( 6.151318917739748038, 6.974181327834800825, -0.9227930848511676221 ) ) ;
#52795 = CARTESIAN_POINT ( 'NONE',  ( -7.458393901293492334, 7.874083437696761223, 0.7216878364870317197 ) ) ;
#52797 = CARTESIAN_POINT ( 'NONE',  ( 2.799504582125960095, -0.5885537693137884441, 1.775713401224961574 ) ) ;
#52796 = CARTESIAN_POINT ( 'NONE',  ( 4.194928683902748645, 1.680244682056671879, 1.243991948001839543 ) ) ;
#52798 = CARTESIAN_POINT ( 'NONE',  ( 7.456621297836067086, 10.68284669990868174, 1.082531754730558626 ) ) ;
#52799 = CARTESIAN_POINT ( 'NONE',  ( -0.6823417656249969321, 5.530208333674756283, -1.181850606188749264 ) ) ;
#52800 = CARTESIAN_POINT ( 'NONE',  ( 3.262975863287612466, 1.697222826579761534, -0.3846178214849705901 ) ) ;
#52801 =( GEOMETRIC_REPRESENTATION_CONTEXT ( 3 ) GLOBAL_UNCERTAINTY_ASSIGNED_CONTEXT ( ( #51541 ) ) GLOBAL_UNIT_ASSIGNED_CONTEXT ( ( #144711, #177171, #210723 ) ) REPRESENTATION_CONTEXT ( 'NONE', 'WORKASPACE' ) );
#52802 = CARTESIAN_POINT ( 'NONE',  ( 3.662674053986138656, 7.424870162959149589, 0.7998128361456321445 ) ) ;
#52804 = CARTESIAN_POINT ( 'NONE',  ( 11.89197369110779512, 13.80000000000000249, -0.8056055387119873679 ) ) ;
#52803 = CARTESIAN_POINT ( 'NONE',  ( 0.6124999999999862776, 1.083333333333352799, 1.060881119635887604 ) ) ;
#52805 = CARTESIAN_POINT ( 'NONE',  ( 4.037519343584392573, -1.191552764850771995, -1.247402213628981293 ) ) ;
#52806 = CARTESIAN_POINT ( 'NONE',  ( -6.795661308947694934, 8.951357498570873261, -1.599625672291263179 ) ) ;
#52807 = CARTESIAN_POINT ( 'NONE',  ( 4.335597073515660149, 0.9364531651635084053, -1.981528385891350386 ) ) ;
#52808 = CARTESIAN_POINT ( 'NONE',  ( 6.445939570963194143, 0.8488519614954292969, -2.037301952897092594 ) ) ;
#52809 = CARTESIAN_POINT ( 'NONE',  ( 6.983263157960365675, 7.052158404629149224, 2.651961988451009944 ) ) ;
#52810 = CARTESIAN_POINT ( 'NONE',  ( 3.643588050499571018, 1.964860050422628124, -0.9237357390106512023 ) ) ;
#52811 = CARTESIAN_POINT ( 'NONE',  ( 2.508196354075361789, -0.6984789837382252564, -1.686990664346368796 ) ) ;
#52812 = CARTESIAN_POINT ( 'NONE',  ( -1.500000000000008216, 9.281250000682799595, 3.469446951953614189E-15 ) ) ;
#52813 = CARTESIAN_POINT ( 'NONE',  ( 5.085217855557687905, 1.732777129288827656, 1.216576597717359931 ) ) ;
#52814 = ORIENTED_EDGE ( 'NONE', *, *, #98379, .T. ) ;
#52816 = CARTESIAN_POINT ( 'NONE',  ( -1.201851678989727383E-14, 3.009375000341419248, -1.575800808251660134 ) ) ;
#52815 = CARTESIAN_POINT ( 'NONE',  ( 4.985981925524552771, -2.274816124779193593, -0.2825110863640226122 ) ) ;
#52817 = CARTESIAN_POINT ( 'NONE',  ( 6.720655732516645386, 3.710664525043025019, 2.240930934554703491 ) ) ;
#52818 = CARTESIAN_POINT ( 'NONE',  ( 8.703444544968814256, 12.24143683818393313, -1.199719254218446718 ) ) ;
#52819 = CARTESIAN_POINT ( 'NONE',  ( 1.155114678095255254, 0.4172207117813032662, 2.078868179971034902 ) ) ;
#52820 = CARTESIAN_POINT ( 'NONE',  ( -5.097502569058221411, 6.009803087731781623, -1.082531754730544860 ) ) ;
#52821 = CARTESIAN_POINT ( 'NONE',  ( 4.365362273920252889, 4.195270195769483124, 0.7216878364870317197 ) ) ;
#52822 = VECTOR ( 'NONE', #161306, 1000.000000000000000 ) ;
#52823 = CARTESIAN_POINT ( 'NONE',  ( -4.839897649954225223, 7.630002444046455778, 1.082531754730560403 ) ) ;
#52825 = CARTESIAN_POINT ( 'NONE',  ( 1.499999999999993117, 12.13541666734946212, 0.8660254037844409281 ) ) ;
#52824 = CARTESIAN_POINT ( 'NONE',  ( 6.883263157960364254, 2.431740398616466070, 2.435552827938294751 ) ) ;
#52826 = ORIENTED_EDGE ( 'NONE', *, *, #184968, .T. ) ;
#52827 = CARTESIAN_POINT ( 'NONE',  ( 5.854138739207011888, 0.1455364397412381439, -2.011204036175239018 ) ) ;
#52829 = CARTESIAN_POINT ( 'NONE',  ( 4.909062464502076395, -1.659793021533024548, 1.224303311577365161 ) ) ;
#52828 = CARTESIAN_POINT ( 'NONE',  ( 4.147904930777053245, 6.926640621626830807, -1.199719254218452047 ) ) ;
#52831 = CARTESIAN_POINT ( 'NONE',  ( -1.737500000000000266, -3.558333333333333570, -3.009438278150923907 ) ) ;
#52830 = CARTESIAN_POINT ( 'NONE',  ( 5.397027666691686321, 8.454226823519094935, 1.199719254218451159 ) ) ;
#52832 = CARTESIAN_POINT ( 'NONE',  ( 6.038177310039780643, 8.137902509836795417, -1.599625672291283607 ) ) ;
#52834 = ADVANCED_FACE ( 'NONE', ( #132656 ), #177396, .F. ) ;
#52833 = CARTESIAN_POINT ( 'NONE',  ( 0.000000000000000000, -0.5468749995220422155, -3.793834371823813001 ) ) ;
#52835 = CARTESIAN_POINT ( 'NONE',  ( -3.602337597214539753E-15, 12.81249999999999822, 1.500000000000001554 ) ) ;
#52836 = CARTESIAN_POINT ( 'NONE',  ( 0.6387612955554131666, -1.792149412372344042, 1.076304641864724410 ) ) ;
#52837 = CARTESIAN_POINT ( 'NONE',  ( 4.957657809308734898, -1.899617967926207740, -0.6767155953601932117 ) ) ;
#52838 = CARTESIAN_POINT ( 'NONE',  ( 4.933073973922719624, -1.305863698873997780, -1.298312775753200699 ) ) ;
#52839 = CARTESIAN_POINT ( 'NONE',  ( 6.331821432781979730, 7.345878745455822312, -1.199719254218445830 ) ) ;
#52840 = CARTESIAN_POINT ( 'NONE',  ( 1.219288043345586159, -1.683946549099228029, 0.3722564037182389818 ) ) ;
#52841 = AXIS2_PLACEMENT_3D ( 'NONE', #106769, #89416, #74222 ) ;
#52842 = CARTESIAN_POINT ( 'NONE',  ( 0.4972802279516430057, -0.2910764605805628014, 1.995268990643041640 ) ) ;
#52843 = CARTESIAN_POINT ( 'NONE',  ( 0.8799778958844242105, -0.5652253508772618895, -2.228020342328890901 ) ) ;
#52844 = CARTESIAN_POINT ( 'NONE',  ( -4.876128802409253282, 8.840567369452784874, 0.7998128361456481317 ) ) ;
#52845 = CARTESIAN_POINT ( 'NONE',  ( 0.8786447689848001508, -1.256089115395578659, 1.881495417452299312 ) ) ;
#52846 = CARTESIAN_POINT ( 'NONE',  ( 2.701903229428818776, -0.6601559168808753819, 2.000001591751764618 ) ) ;
#52847 = CARTESIAN_POINT ( 'NONE',  ( -5.123001941117347080, 7.070197912760590064, 1.599625672291263179 ) ) ;
#52849 = EDGE_CURVE ( 'NONE', #70402, #2318, #118684, .T. ) ;
#52848 = CARTESIAN_POINT ( 'NONE',  ( 8.288111976655649471, 8.563885482386732306, -0.7998128361456291469 ) ) ;
#52850 = CARTESIAN_POINT ( 'NONE',  ( 7.336370518326124746, 7.731722824234849689, -0.7216878364870317197 ) ) ;
#52851 = CARTESIAN_POINT ( 'NONE',  ( 5.750000000000004441, 3.273043269275614537E-13, 2.052068128417940951 ) ) ;
#52852 = B_SPLINE_CURVE_WITH_KNOTS ( 'NONE', 3,
 ( #102042, #203777, #72727, #135620, #37026, #103110 ),
 .UNSPECIFIED., .F., .F.,
 ( 4, 2, 4 ),
 ( 0.0004037790303856251119, 0.0007126936173802011359, 0.001021608204374777106 ),
 .UNSPECIFIED. ) ;
#52853 = CARTESIAN_POINT ( 'NONE',  ( -5.708146366553361162, 6.618257834855742594, -1.199719254218446718 ) ) ;
#52854 = CARTESIAN_POINT ( 'NONE',  ( 7.443063143778065438, 7.785921210603627962, -0.7216878364870257245 ) ) ;
#52855 = CARTESIAN_POINT ( 'NONE',  ( 5.008269389056229315, 6.794162766424465261, 1.424127363233711252 ) ) ;
#52856 = CIRCLE ( 'NONE', #32150, 10.99999999999999112 ) ;
#52857 = CARTESIAN_POINT ( 'NONE',  ( -4.460796234096120472, 5.163016013655583158, 1.199719254218462483 ) ) ;
#52858 = CARTESIAN_POINT ( 'NONE',  ( 4.746434557108095476, 1.141014917558682340, -1.905822037654863133 ) ) ;
#52859 = CARTESIAN_POINT ( 'NONE',  ( 1.939652437182255662, 0.8368340126228106524, -2.025574644071465258 ) ) ;
#52860 = CARTESIAN_POINT ( 'NONE',  ( -6.274726165026268454, 6.214935368819085149, 0.7998128361456341429 ) ) ;
#52861 = CARTESIAN_POINT ( 'NONE',  ( -2.823841133396259639, 6.516508098929413961, -0.7998128361456481317 ) ) ;
#52862 = CARTESIAN_POINT ( 'NONE',  ( 5.934033239752055877, 1.167398200610193282, 1.576599764842034457 ) ) ;
#52863 = CARTESIAN_POINT ( 'NONE',  ( 0.6823417656249882723, 1.426041667008083547, -1.181850606188749264 ) ) ;
#52864 = CARTESIAN_POINT ( 'NONE',  ( 6.890000000000014779, 6.038692643467888921, 2.314896014905319266 ) ) ;
#52865 = CARTESIAN_POINT ( 'NONE',  ( -3.768803514918943609, 7.340761834139994058, 0.7216878364870317197 ) ) ;
#52866 = CARTESIAN_POINT ( 'NONE',  ( 5.080389167821143026, 1.047295930500062866, 1.843893106414703054 ) ) ;
#52867 = CARTESIAN_POINT ( 'NONE',  ( -5.790741006812557323, 9.769965251341050205, 0.000000000000000000 ) ) ;
#52868 = ORIENTED_EDGE ( 'NONE', *, *, #205893, .F. ) ;
#52870 = DIRECTION ( 'NONE',  ( -0.000000000000000000, 1.000000000000000000, -0.000000000000000000 ) ) ;
#52869 = CARTESIAN_POINT ( 'NONE',  ( -4.340018570150306232, 8.077455741901736985, -0.7216878364870338292 ) ) ;
#52871 = CARTESIAN_POINT ( 'NONE',  ( 5.120175567455225618, 9.125288595339771547, -0.7998128361456281477 ) ) ;
#52872 = CARTESIAN_POINT ( 'NONE',  ( 5.302248432823610358, 1.390444127666954355, -1.207098008268410183 ) ) ;
#52873 = CARTESIAN_POINT ( 'NONE',  ( 1.364683531249988535, 2.426041667008088432, 0.7879004041258500513 ) ) ;
#52874 = CARTESIAN_POINT ( 'NONE',  ( 1.346757998634398712, 0.5060278187854657661, -1.665264516905233361 ) ) ;
#52875 = CARTESIAN_POINT ( 'NONE',  ( 1.264911064067348656, 3.849999999999994316, 0.5000000000000064393 ) ) ;
#52876 = CARTESIAN_POINT ( 'NONE',  ( -0.6823417656250003738, -0.9697916663252494907, -1.181850606188749264 ) ) ;
#52877 = CARTESIAN_POINT ( 'NONE',  ( 11.09110889797585919, 7.944360173633553401, -4.602131112445142058 ) ) ;
#52878 = CARTESIAN_POINT ( 'NONE',  ( 5.594645800149128156, -0.5210773734287167391, -2.097845705497362712 ) ) ;
#52879 = CARTESIAN_POINT ( 'NONE',  ( -4.973143418114339021, 4.696422164088486895, 0.7998128361456341429 ) ) ;
#52880 = EDGE_CURVE ( 'NONE', #162079, #162324, #124398, .T. ) ;
#52881 = CARTESIAN_POINT ( 'NONE',  ( -8.161645285302366659, 8.624267042381978499, 1.040834085586084257E-14 ) ) ;
#52882 = CARTESIAN_POINT ( 'NONE',  ( 4.733375416736937069, -1.977748744329570263, 0.8730265686548792647 ) ) ;
#52883 = CARTESIAN_POINT ( 'NONE',  ( -1.364683531249997417, 3.509375000341423245, 1.214306433183764966E-14 ) ) ;
#52884 = CARTESIAN_POINT ( 'NONE',  ( 5.132083838642755858, 1.015972595308231474, -1.689280876731833470 ) ) ;
#52885 = CARTESIAN_POINT ( 'NONE',  ( 3.532318661231689916, 1.691930322982236667, -0.3780173437282279281 ) ) ;
#52886 = CARTESIAN_POINT ( 'NONE',  ( 0.5740950506661415265, -1.212703583203307511, 1.825263377225619266 ) ) ;
#52887 = CARTESIAN_POINT ( 'NONE',  ( 2.433052891977859566, 2.238319448195260186, 0.5606502339033142546 ) ) ;
#52888 = CARTESIAN_POINT ( 'NONE',  ( 5.325487547722469905, -1.958136382931666031, 0.6425617224121594750 ) ) ;
#52889 = CARTESIAN_POINT ( 'NONE',  ( -0.01194524340117873729, -0.4266214822964596309, -1.901745140312367521 ) ) ;
#52890 = CARTESIAN_POINT ( 'NONE',  ( -7.388830529323428209, 8.683019041374528513, 1.082531754730549967 ) ) ;
#52891 = CARTESIAN_POINT ( 'NONE',  ( -5.010620288702242853, 8.003418215864698482, -1.199719254218453823 ) ) ;
#52892 =( LENGTH_UNIT ( ) NAMED_UNIT ( * ) SI_UNIT ( .MILLI., .METRE. ) );
#52893 = CARTESIAN_POINT ( 'NONE',  ( 0.9322677863709986079, -1.591319861332978425, -1.238319039483272599 ) ) ;
#52894 = CARTESIAN_POINT ( 'NONE',  ( -6.466876083594135238, 9.528143949959703818, 1.082531754730548412 ) ) ;
#52895 = CARTESIAN_POINT ( 'NONE',  ( 3.206306947805489305, -2.204311952916749640, 0.1065802224688369715 ) ) ;
#52896 = CARTESIAN_POINT ( 'NONE',  ( 1.642778471875001811, -1.480208332855375453, 2.845375778867859751 ) ) ;
#52897 = CARTESIAN_POINT ( 'NONE',  ( 0.6021283177516533192, 1.855420301818105910, 0.1446146731104556993 ) ) ;
#52898 = CARTESIAN_POINT ( 'NONE',  ( -0.1290005225502433017, 0.6921039065478848951, -2.255494067288220439 ) ) ;
#52899 = CARTESIAN_POINT ( 'NONE',  ( 1.499999999999990896, 4.806250000682819490, 1.214306433183765124E-14 ) ) ;
#52900 = CARTESIAN_POINT ( 'NONE',  ( -9.500331257164631893, -7.473374494045002869, 1.019891195965221523E-14 ) ) ;
#52902 = CARTESIAN_POINT ( 'NONE',  ( 6.925078400183577010, 2.950057911518182419, 2.596529392604688180 ) ) ;
#52901 = CARTESIAN_POINT ( 'NONE',  ( -4.584844773125573703, 8.498748274393685520, 0.004977730536110530624 ) ) ;
#52903 = CARTESIAN_POINT ( 'NONE',  ( 6.035073252477260120, -1.336788798515762489, -1.266260169258619284 ) ) ;
#52904 = ORIENTED_EDGE ( 'NONE', *, *, #131239, .T. ) ;
#52906 = CARTESIAN_POINT ( 'NONE',  ( 3.414965445803084254, 1.862500966792278057, 0.8825600945957471355 ) ) ;
#52905 = B_SPLINE_CURVE_WITH_KNOTS ( 'NONE', 3,
 ( #147415, #17370, #144262, #131219 ),
 .UNSPECIFIED., .F., .F.,
 ( 4, 4 ),
 ( 0.002022417813501748915, 0.002304360150591485551 ),
 .UNSPECIFIED. ) ;
#52907 = CARTESIAN_POINT ( 'NONE',  ( -3.555477883677943599E-14, 1.578125000341449535, -1.570758158831814466 ) ) ;
#52908 = CARTESIAN_POINT ( 'NONE',  ( -7.230575994789712801, 7.330093503543126054, 0.7998128361456341429 ) ) ;
#52909 = CARTESIAN_POINT ( 'NONE',  ( 1.770181643375926317, 2.014124636562672155, -0.1506882416659905133 ) ) ;
#52910 = CARTESIAN_POINT ( 'NONE',  ( 0.7499999999999867883, -0.4333333333333133641, -1.299038105676652899 ) ) ;
#52911 = CARTESIAN_POINT ( 'NONE',  ( 3.225950485047770933, 5.851027101609320269, 1.199719254218450271 ) ) ;
#52912 = CARTESIAN_POINT ( 'NONE',  ( 2.483339057139447803, 1.884786786457379737, -0.8339860623947179530 ) ) ;
#52914 = CARTESIAN_POINT ( 'NONE',  ( 1.364683531249997417, 12.73437500034139980, 2.602085213965210642E-15 ) ) ;
#52913 = DIRECTION ( 'NONE',  ( 0.000000000000000000, -1.000000000000000000, 0.000000000000000000 ) ) ;
#52915 = CARTESIAN_POINT ( 'NONE',  ( 6.169123589417988995, 7.156064594864501416, -1.199719254218445830 ) ) ;
#52916 = VECTOR ( 'NONE', #203580, 1000.000000000000000 ) ;
#52917 = CARTESIAN_POINT ( 'NONE',  ( 6.177789192050737732, 5.326704385421541232, 2.500000000000899281 ) ) ;
#52918 = AXIS2_PLACEMENT_3D ( 'NONE', #170193, #105222, #21778 ) ;
#52919 = CARTESIAN_POINT ( 'NONE',  ( 5.092482806099829062, -2.189899077852827780, -0.2726905915074183673 ) ) ;
#52920 = CARTESIAN_POINT ( 'NONE',  ( 1.581558009922879204, 1.997867266642009643, -0.8257073301623578665 ) ) ;
#52921 = CARTESIAN_POINT ( 'NONE',  ( -4.284013352238255301, 6.981470763377843447, -1.082531754730549967 ) ) ;
#52922 = CARTESIAN_POINT ( 'NONE',  ( 0.4093891192313535710, -1.913260280790154866, 0.6371585790938688598 ) ) ;
#52923 = CARTESIAN_POINT ( 'NONE',  ( 2.144337281971959719, -0.1124944508365255252, -2.295720847718041746 ) ) ;
#52924 = PRESENTATION_STYLE_ASSIGNMENT (( #3078 ) ) ;
#52925 = CARTESIAN_POINT ( 'NONE',  ( -2.788906526875773208E-15, 12.21875000068279782, -1.499999999999998446 ) ) ;
#52926 = CARTESIAN_POINT ( 'NONE',  ( 3.109879841324575622, 6.447534329559368338, -0.5062228152068328768 ) ) ;
#52927 = CARTESIAN_POINT ( 'NONE',  ( 2.289737743334671283, -0.8020533187339595749, 1.690132462187944107 ) ) ;
#52928 = CARTESIAN_POINT ( 'NONE',  ( 3.784388871581423786, -0.6371526190629381858, -1.913262240507591416 ) ) ;
#52930 = DIRECTION ( 'NONE',  ( 1.000000000000000000, 0.000000000000000000, 0.000000000000000000 ) ) ;
#52929 = CARTESIAN_POINT ( 'NONE',  ( -1.364683531250014514, 1.738541667008085545, -0.7879004041258289570 ) ) ;
#52932 = CARTESIAN_POINT ( 'NONE',  ( 5.268238656634978589, 1.036954370284940419, 1.833022835974008613 ) ) ;
#52931 = CARTESIAN_POINT ( 'NONE',  ( -7.202405917357668663, 9.425892875049191488, 1.599625672291295375 ) ) ;
#52933 = CARTESIAN_POINT ( 'NONE',  ( 5.960781091502512119, 10.10599504006161986, 0.7998128361456462443 ) ) ;
#52934 = CARTESIAN_POINT ( 'NONE',  ( -6.367525699912501835, 10.58053041653993098, -0.7998128361456291469 ) ) ;
#52935 = CARTESIAN_POINT ( 'NONE',  ( 1.309956906536929200, 3.548345970690609974, 0.4145166106152374796 ) ) ;
#52936 = CARTESIAN_POINT ( 'NONE',  ( 4.957288421310242832, -1.730244549199685400, 1.041802906739682566 ) ) ;
#52937 = CARTESIAN_POINT ( 'NONE',  ( -1.500000000000013101, -0.2979166659838501929, 0.8660254037844403729 ) ) ;
#52938 = CARTESIAN_POINT ( 'NONE',  ( 0.6552251538811122433, 1.716912266053271408, -1.142698840430116602 ) ) ;
#52939 = CARTESIAN_POINT ( 'NONE',  ( 7.429504990608736037, 11.61158022244479682, -0.7216878364870267237 ) ) ;
#52940 = CARTESIAN_POINT ( 'NONE',  ( 4.213551878797002992, 8.137837301896977849, 0.000000000000000000 ) ) ;
#52941 = CARTESIAN_POINT ( 'NONE',  ( -0.6823417656250246877, -0.3864583329919110688, 1.181850606188755259 ) ) ;
#52943 = CARTESIAN_POINT ( 'NONE',  ( 8.743186976631660556, 3.870433085555829766, 7.668514896535032932 ) ) ;
#52942 = CARTESIAN_POINT ( 'NONE',  ( 6.039231080244466199, 6.010467446565510130, 0.7998128361456352531 ) ) ;
#52944 = CARTESIAN_POINT ( 'NONE',  ( 7.470179451005385829, 8.777926116670192513, -1.082531754730537976 ) ) ;
#52946 =( NAMED_UNIT ( * ) PLANE_ANGLE_UNIT ( ) SI_UNIT ( $, .RADIAN. ) );
#52945 = CARTESIAN_POINT ( 'NONE',  ( 3.156845524303863559, -0.6275973837717390147, -2.078511276010074127 ) ) ;
#52948 = CARTESIAN_POINT ( 'NONE',  ( 2.348939331405873077, 0.4892633877765646400, -1.774999737812533063 ) ) ;
#52947 = CARTESIAN_POINT ( 'NONE',  ( -5.748293942514189681, 5.808690475795744490, -0.7216878364870207285 ) ) ;
#52949 = CARTESIAN_POINT ( 'NONE',  ( -1.364683531249997417, 3.509375000341423245, 1.214306433183764966E-14 ) ) ;
#52950 = CARTESIAN_POINT ( 'NONE',  ( 4.405938146338868933, -0.9375679901368579872, -1.981035393479456008 ) ) ;
#52951 = CARTESIAN_POINT ( 'NONE',  ( 6.983263157960365675, -0.006178392973848687020, 2.053544886540019210 ) ) ;
#52952 = CARTESIAN_POINT ( 'NONE',  ( 4.627936124501790260, -1.388401915515205198, -1.786361659577795136 ) ) ;
#52953 = CARTESIAN_POINT ( 'NONE',  ( -4.706651882238427120, 8.642844295920152575, 1.040834085586084257E-14 ) ) ;
#52954 = CARTESIAN_POINT ( 'NONE',  ( 5.647444738788365726, 7.344714329438926548, -1.230740020431456028 ) ) ;
#52955 = CIRCLE ( 'NONE', #135998, 0.08000000000000020983 ) ;
#52956 = CARTESIAN_POINT ( 'NONE',  ( -1.402160292154681736E-14, 13.56250000000000000, 1.732050807568881190 ) ) ;
#52957 = CARTESIAN_POINT ( 'NONE',  ( -5.058600711230246461, 7.955432358860325515, 1.082531754730549967 ) ) ;
#52958 = CARTESIAN_POINT ( 'NONE',  ( 5.736508392357904107, 5.865217010605237924, 0.000000000000000000 ) ) ;
#52959 = CARTESIAN_POINT ( 'NONE',  ( 5.518734381310105519, 1.635532185772445857, 0.6765044976165290880 ) ) ;
#52960 = CARTESIAN_POINT ( 'NONE',  ( 6.446011968293428041, 9.607765498729298415, -1.199719254218440723 ) ) ;
#52961 = CARTESIAN_POINT ( 'NONE',  ( 2.362460971492767570, 0.8994288142968703825, 1.904360703123770149 ) ) ;
#52963 = CARTESIAN_POINT ( 'NONE',  ( 1.499999999999989120, 3.025000000000020783, 1.214306433183764966E-14 ) ) ;
#52962 = CARTESIAN_POINT ( 'NONE',  ( -1.364683531250010295, 12.38020833367473372, 0.7879004041258445001 ) ) ;
#52964 = CARTESIAN_POINT ( 'NONE',  ( 2.383201438719654064, -0.002954665228930426248, 1.969739564733210324 ) ) ;
#52965 = CARTESIAN_POINT ( 'NONE',  ( 0.9009904985227291663, 1.526999960511504772, 1.080287613699250304 ) ) ;
#52966 = CARTESIAN_POINT ( 'NONE',  ( 1.152704166800899932, -0.4732522875653189520, -1.903817266927515961 ) ) ;
#52968 = ORIENTED_EDGE ( 'NONE', *, *, #13749, .T. ) ;
#52967 = CARTESIAN_POINT ( 'NONE',  ( 6.293201719952925544, -0.09848415459409513850, -1.809066888985458199 ) ) ;
#52969 = CARTESIAN_POINT ( 'NONE',  ( 7.158341918335438869, 7.453746447587225710, -0.7216878364870257245 ) ) ;
#52970 = ADVANCED_FACE ( 'NONE', ( #148871 ), #90979, .T. ) ;
#52971 = CARTESIAN_POINT ( 'NONE',  ( 1.364683531249988757, -0.8031249996585804185, 0.000000000000000000 ) ) ;
#52972 = CARTESIAN_POINT ( 'NONE',  ( 5.629731426258720361, -1.187751674602673058, -1.445209747047627946 ) ) ;
#52973 = PLANE ( 'NONE',  #74745 ) ;
#52974 = AXIS2_PLACEMENT_3D ( 'NONE', #164250, #65644, #46252 ) ;
#52975 = CARTESIAN_POINT ( 'NONE',  ( 5.559458666840932928, 1.689222788819956245, 1.196583256836199149 ) ) ;
#52976 = AXIS2_PLACEMENT_3D ( 'NONE', #19243, #118959, #4044 ) ;
#52977 = CARTESIAN_POINT ( 'NONE',  ( -5.358255402162534516E-14, 2.562499999999964473, 1.414508159514571428 ) ) ;
#52978 = CARTESIAN_POINT ( 'NONE',  ( -4.136646265500958819, 7.840188053144158786, -0.7216878364870458196 ) ) ;
#52979 = SURFACE_SIDE_STYLE ('',( #150506 ) ) ;
#52980 = CARTESIAN_POINT ( 'NONE',  ( -1.402160292154681736E-14, 0.8375000000000232259, -1.732050807568863648 ) ) ;
#52981 = CARTESIAN_POINT ( 'NONE',  ( 6.265839547809997079, 10.46189657242035587, 0.7998128361456462443 ) ) ;
#52982 = CARTESIAN_POINT ( 'NONE',  ( -7.330154606482786050, 11.70359747420527619, 0.000000000000000000 ) ) ;
#52983 = CARTESIAN_POINT ( 'NONE',  ( 4.830447868218803897, 8.857549289555754157, -0.7998128361456481317 ) ) ;
#52984 = CARTESIAN_POINT ( 'NONE',  ( -1.364683531250014514, -0.4697916663252449943, 0.7879004041258379498 ) ) ;
#52985 = CARTESIAN_POINT ( 'NONE',  ( -1.500000000000001332, 0.6500000000000255573, 0.000000000000000000 ) ) ;
#52987 = CARTESIAN_POINT ( 'NONE',  ( 4.147904930777053245, 6.926640621626830807, -1.199719254218452047 ) ) ;
#52986 = CARTESIAN_POINT ( 'NONE',  ( 5.441838459065293065, 1.316327937319297758, 1.454900926449454124 ) ) ;
#52988 = CARTESIAN_POINT ( 'NONE',  ( 3.585314394424500062, 1.281165535658060239, -1.556669873624405120 ) ) ;
#52989 = CARTESIAN_POINT ( 'NONE',  ( 2.465921856196826134, -0.9807800477944830231, 1.645437157327357180 ) ) ;
#52990 = CARTESIAN_POINT ( 'NONE',  ( 4.000000000000012434, 5.499999999999998224, -1.214306433183764966E-14 ) ) ;
#52991 = AXIS2_PLACEMENT_3D ( 'NONE', #193766, #212134, #31288 ) ;
#52992 = CARTESIAN_POINT ( 'NONE',  ( 0.7850416839378616674, 1.930235501049954339, -1.037882601892345491 ) ) ;
#52993 = CARTESIAN_POINT ( 'NONE',  ( 0.2331713839410758105, 2.878356536703096324, -2.442089366404568640 ) ) ;
#52994 = CARTESIAN_POINT ( 'NONE',  ( 2.231529376059933956, -1.218349341866202362, -1.419469154777988296 ) ) ;
#52995 = CARTESIAN_POINT ( 'NONE',  ( 1.499999999999987121, -0.7145833326505161009, 0.8660254037844524744 ) ) ;
#52996 = CARTESIAN_POINT ( 'NONE',  ( 4.306893573823011856, -0.4451576889303583418, -1.963212451998196606 ) ) ;
#52997 = CARTESIAN_POINT ( 'NONE',  ( -6.995117189646935962, 10.24838825697502109, 1.199719254218453823 ) ) ;
#52999 = CARTESIAN_POINT ( 'NONE',  ( 4.816069135992575134, 1.087346734782314472, -1.816536155142484121 ) ) ;
#52998 = CARTESIAN_POINT ( 'NONE',  ( -6.100805936469506641, 6.219954468743612352, 0.7216878364870317197 ) ) ;
#53000 = LINE ( 'NONE', #166763, #4230 ) ;
#53001 = CARTESIAN_POINT ( 'NONE',  ( 6.408651866624735405, 0.6456447432892989946, 1.967203394946090977 ) ) ;
#53003 = CARTESIAN_POINT ( 'NONE',  ( 3.992368507422526136, 7.606667543653665042, 0.1043914665942706627 ) ) ;
#53002 = CARTESIAN_POINT ( 'NONE',  ( 0.6793770918060678676, 1.407085465964125204, 1.546551842177671166 ) ) ;
#53005 = ORIENTED_EDGE ( 'NONE', *, *, #96921, .F. ) ;
#53004 = CARTESIAN_POINT ( 'NONE',  ( 6.598675984083053336, -0.4903212918116289787, -1.758449130657411263 ) ) ;
#53006 = CARTESIAN_POINT ( 'NONE',  ( 6.428537391173986038, 10.65171072301167854, 0.7998128361456462443 ) ) ;
#53007 = DIRECTION ( 'NONE',  ( 0.000000000000000000, 0.000000000000000000, -1.000000000000000000 ) ) ;
#53008 = CARTESIAN_POINT ( 'NONE',  ( 0.4799999999999758349, 2.999999999999999112, 2.500000000000000444 ) ) ;
